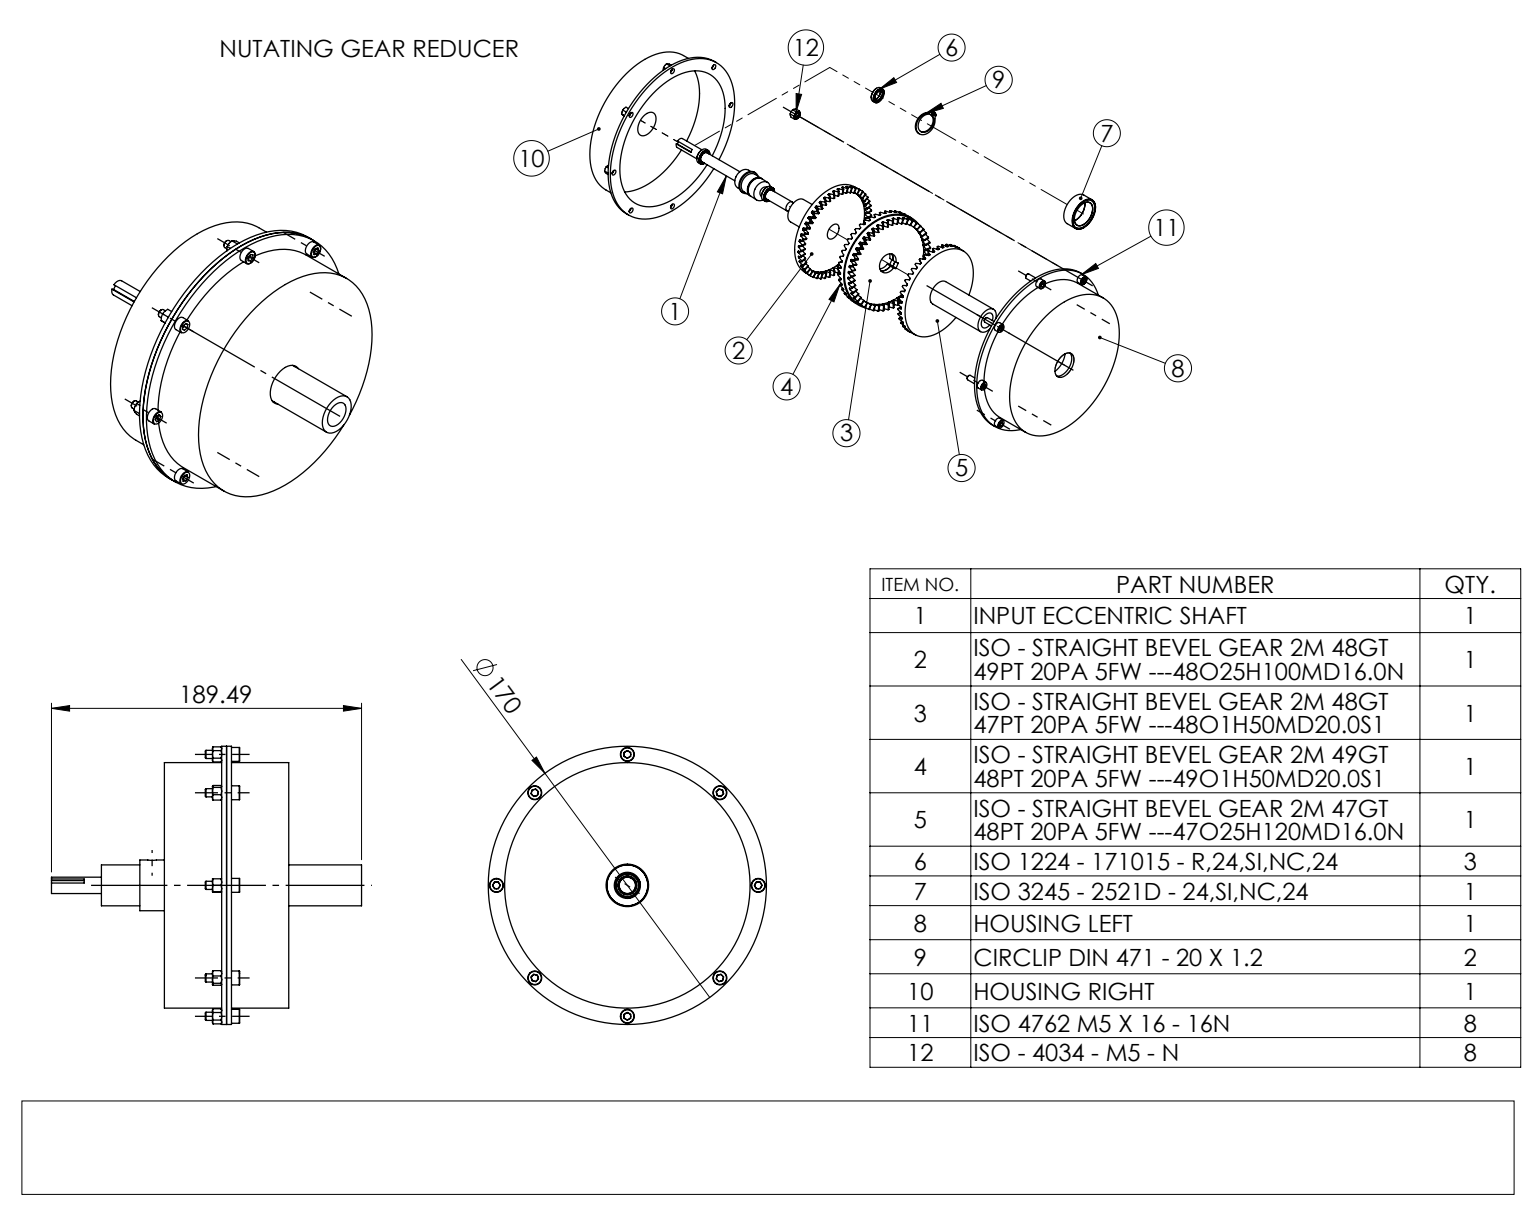
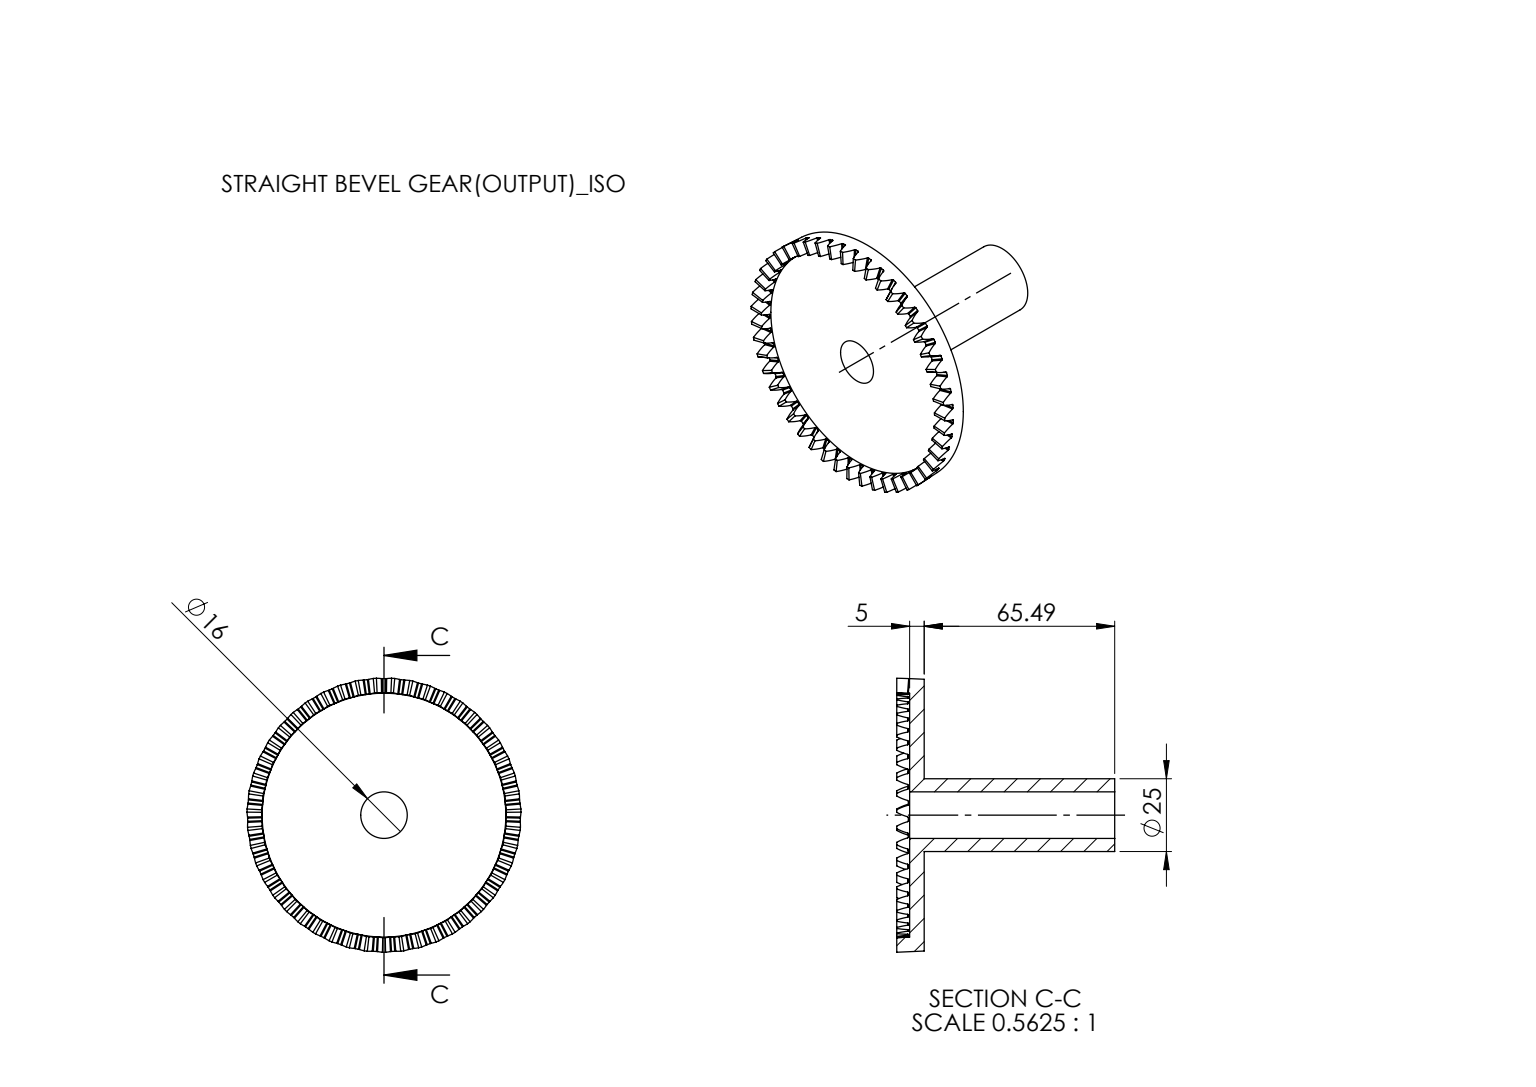
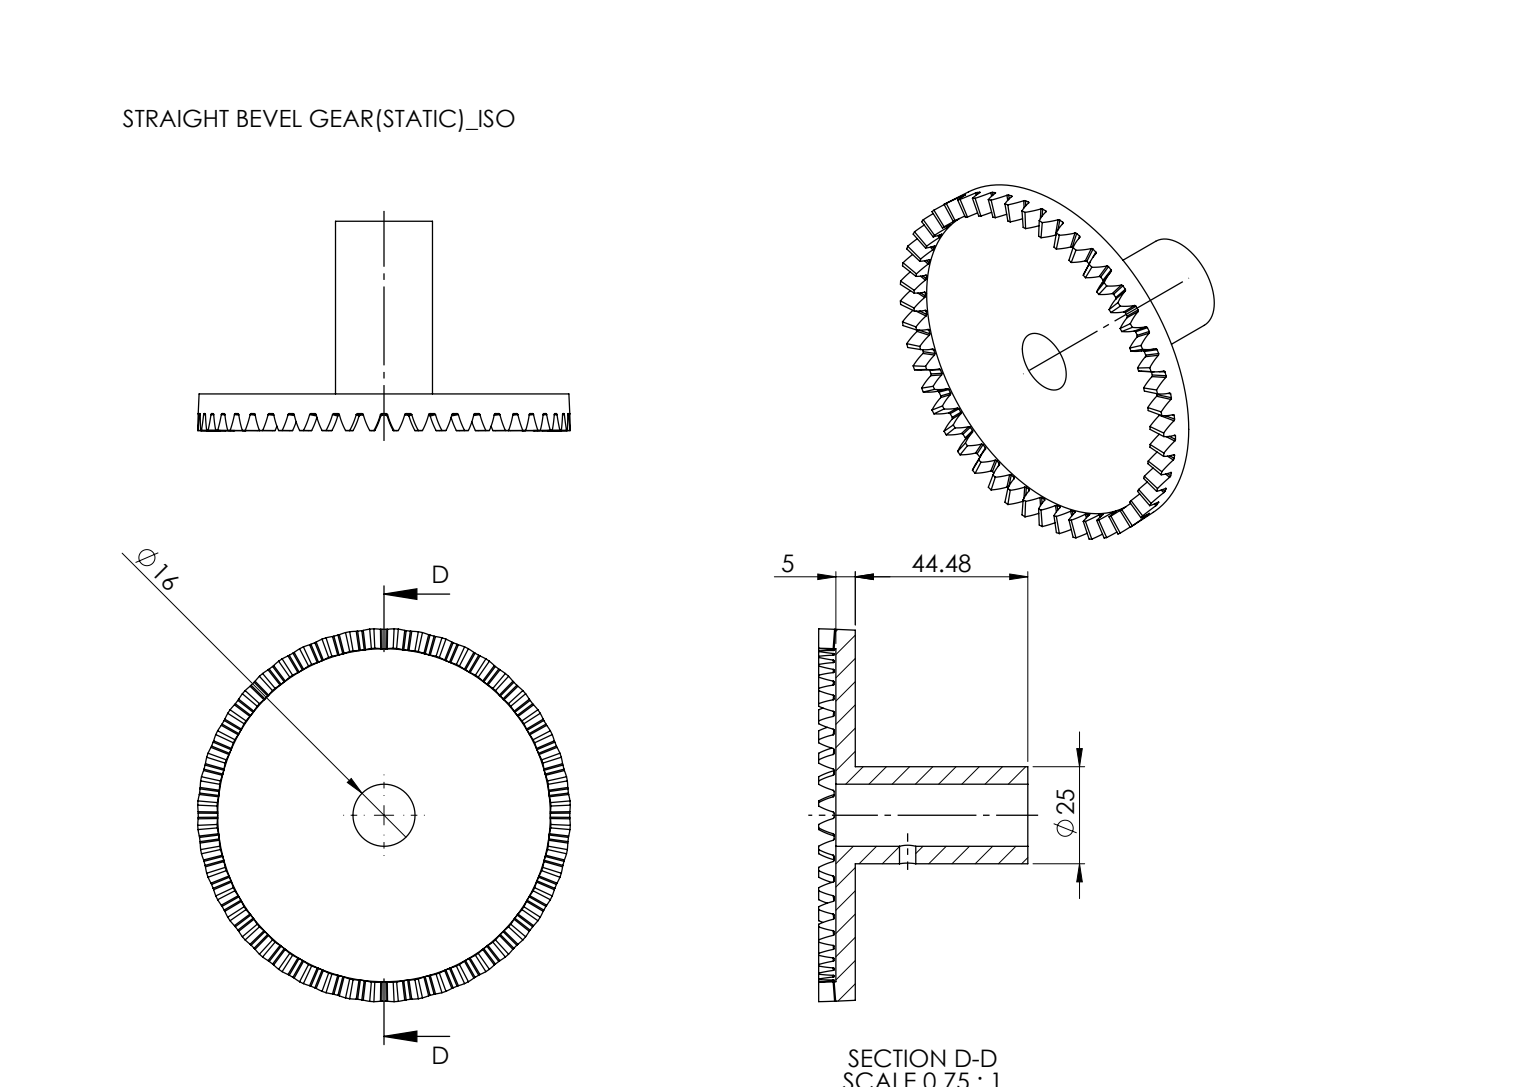
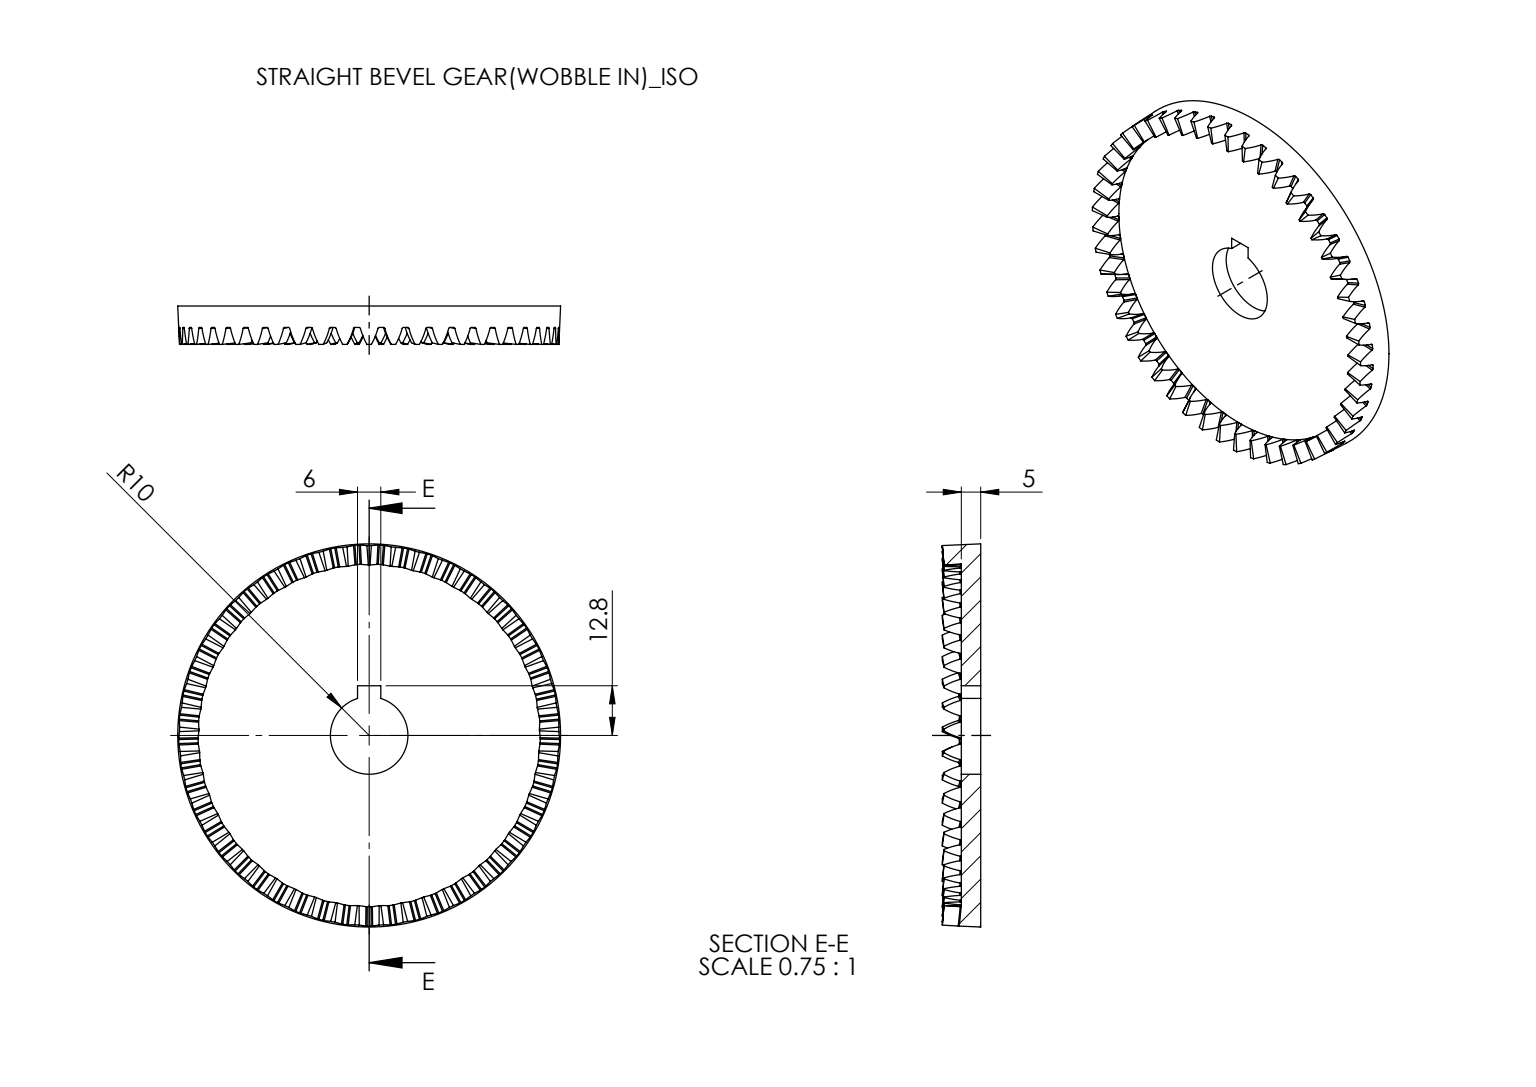
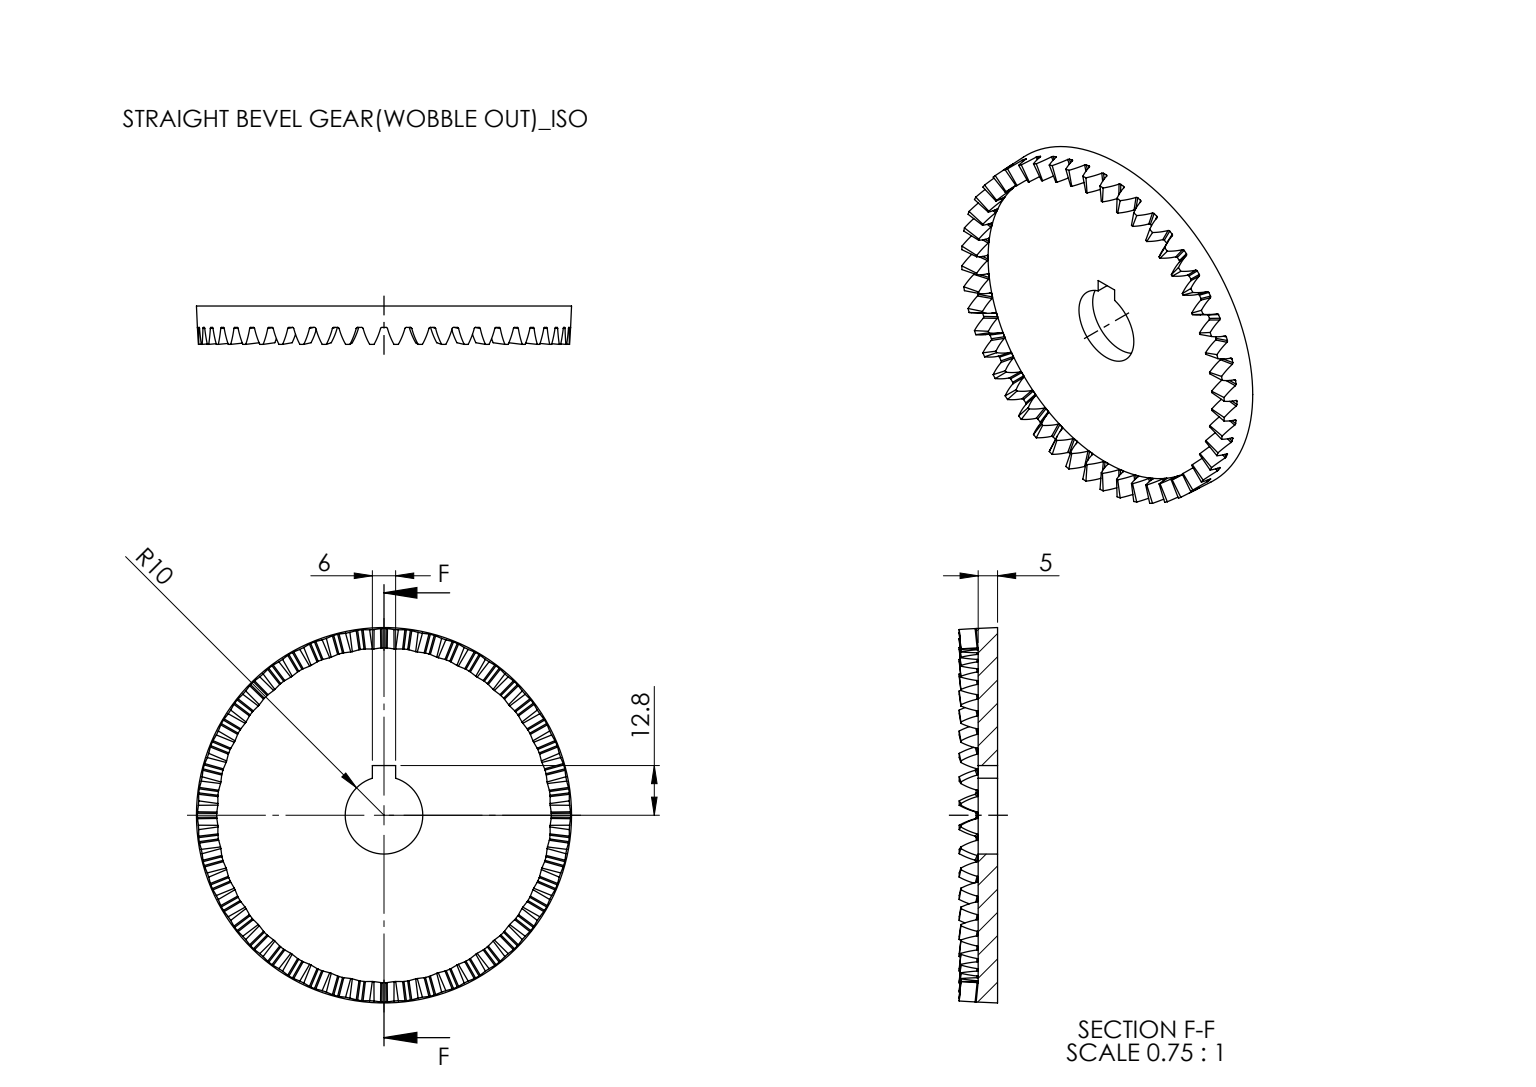
ISO-10303-21;
HEADER;
FILE_DESCRIPTION (('STEP AP214'),
    '1' );
FILE_NAME ('BR-540',
    '2026-10-08T08:02:49',
    ( '' ),
    ( '' ),
    'SwSTEP 2.0',
    'SolidWorks 2026',
    '' );
FILE_SCHEMA (( 'AUTOMOTIVE_DESIGN' ));
ENDSEC;

DATA;
#1 = CARTESIAN_POINT ( 'NONE',  ( 0.6000166863083090663, -45.71468846346234471, -17.94410043432203139 ) ) ;
#2 = ORIENTED_EDGE ( 'NONE', *, *, #40135, .F. ) ;
#3 = CARTESIAN_POINT ( 'NONE',  ( -6.017396004339686577, 14.95000090562881390, 11.47005965438143882 ) ) ;
#4 = VERTEX_POINT ( 'NONE', #15118 ) ;
#5 = FACE_OUTER_BOUND ( 'NONE', #24544, .T. ) ;
#6 = ORIENTED_EDGE ( 'NONE', *, *, #7694, .T. ) ;
#7 = CARTESIAN_POINT ( 'NONE',  ( 0.5848930533535030563, -19.57496322689467760, 42.61565319285014652 ) ) ;
#8 = CARTESIAN_POINT ( 'NONE',  ( -6.077587904424778920, 5.472951620448720078, -18.46192898789718129 ) ) ;
#9 = ORIENTED_EDGE ( 'NONE', *, *, #20619, .T. ) ;
#10 = CARTESIAN_POINT ( 'NONE',  ( 5.910764540655177868, -13.99299321836483045, 14.44636214622763681 ) ) ;
#11 = ORIENTED_EDGE ( 'NONE', *, *, #34105, .F. ) ;
#12 = CARTESIAN_POINT ( 'NONE',  ( 2.624215991343608501, -38.92973006074533515, 28.09277600149204801 ) ) ;
#13 = SHAPE_REPRESENTATION ( 'circlip for shafts normal_din_Circlip DIN 471 - 20 x 1.2', ( #14677 ), #21841 ) ;
#14 = VERTEX_POINT ( 'NONE', #34229 ) ;
#15 = CARTESIAN_POINT ( 'NONE',  ( 0.9752132459055861124, -16.63533515462550127, -39.55248938404434966 ) ) ;
#16 = CARTESIAN_POINT ( 'NONE',  ( 16.60577576646022635, -4.999999999999987566, 6.123233995736738672E-16 ) ) ;
#17 = CARTESIAN_POINT ( 'NONE',  ( 0.1152809850208375564, -22.68421566702489756, -37.84668601161344981 ) ) ;
#18 = ORIENTED_EDGE ( 'NONE', *, *, #60103, .F. ) ;
#19 = CARTESIAN_POINT ( 'NONE',  ( 0.8560838555295158248, -34.16988317699912159, -32.13708010619451727 ) ) ;
#20 = ORIENTED_EDGE ( 'NONE', *, *, #44663, .F. ) ;
#21 = ORIENTED_EDGE ( 'NONE', *, *, #24258, .F. ) ;
#22 = CIRCLE ( 'NONE', #14059, 18.99999999999999645 ) ;
#23 = CARTESIAN_POINT ( 'NONE',  ( 1.092182651088189127, 25.48667707440418440, 33.27447183874333803 ) ) ;
#24 = ADVANCED_FACE ( 'NONE', ( #21978 ), #2362, .F. ) ;
#25 = CARTESIAN_POINT ( 'NONE',  ( 5.960221823109900008, 10.26751639438343311, 17.77295928189558794 ) ) ;
#26 = ORIENTED_EDGE ( 'NONE', *, *, #59034, .F. ) ;
#27 = LINE ( 'NONE', #23853, #11554 ) ;
#28 = CARTESIAN_POINT ( 'NONE',  ( 9.999999999999994671, 54.69470952477936976, 58.44237546506825964 ) ) ;
#29 = CARTESIAN_POINT ( 'NONE',  ( 4.956653778116966613, 0.000000000000000000, 0.000000000000000000 ) ) ;
#30 = CARTESIAN_POINT ( 'NONE',  ( 0.9789233960466694473, -22.43936322751809342, -35.39508023406433068 ) ) ;
#31 = VECTOR ( 'NONE', #37686, 1000.000000000000000 ) ;
#32 = ORIENTED_EDGE ( 'NONE', *, *, #35814, .T. ) ;
#33 = CARTESIAN_POINT ( 'NONE',  ( 0.5806925824938499181, 45.08220210717423271, 12.91578164539256335 ) ) ;
#34 = DIRECTION ( 'NONE',  ( 0.09722883295013594329, -0.9880289017988295175, -0.1197724645039638103 ) ) ;
#35 = CARTESIAN_POINT ( 'NONE',  ( 5.960221823109900008, -10.25807604135609274, -17.77840967225716895 ) ) ;
#36 = DIRECTION ( 'NONE',  ( 0.000000000000000000, 0.000000000000000000, 1.000000000000000000 ) ) ;
#37 = CARTESIAN_POINT ( 'NONE',  ( 0.8560838555295223751, -26.00596412780120303, -39.03924517540328765 ) ) ;
#38 = CARTESIAN_POINT ( 'NONE',  ( 1.827326673878743257, 6.839036141888570342, -42.50320212329573621 ) ) ;
#39 = CARTESIAN_POINT ( 'NONE',  ( 0.5987334308729315158, 46.79309025446952575, 14.89864460301000015 ) ) ;
#40 = CARTESIAN_POINT ( 'NONE',  ( 0.5832655196449135770, 40.46492986189638685, -23.70284021473238667 ) ) ;
#41 = CARTESIAN_POINT ( 'NONE',  ( 0.1313383488274124655, -37.02311703718871883, 22.11173226734828745 ) ) ;
#42 = CARTESIAN_POINT ( 'NONE',  ( 0.6025881611877910160, 48.10699274197334319, 0.2181813582440121635 ) ) ;
#43 = CARTESIAN_POINT ( 'NONE',  ( -1.200000000000006617, 0.000000000000000000, 0.000000000000000000 ) ) ;
#44 = CYLINDRICAL_SURFACE ( 'NONE', #23607, 12.50000000000000000 ) ;
#45 = CARTESIAN_POINT ( 'NONE',  ( 2.528190830796654964, -23.59892530385130627, 34.71807685711083025 ) ) ;
#46 = FACE_OUTER_BOUND ( 'NONE', #12216, .T. ) ;
#47 = EDGE_CURVE ( 'NONE', #13219, #36056, #34301, .T. ) ;
#48 = CARTESIAN_POINT ( 'NONE',  ( 0.5807400328401574052, 47.89582301953903709, 0.5448834511091634747 ) ) ;
#49 = EDGE_CURVE ( 'NONE', #23782, #28115, #2220, .T. ) ;
#50 = FILL_AREA_STYLE_COLOUR ( '', #7249 ) ;
#51 = CARTESIAN_POINT ( 'NONE',  ( -6.015611763856276717, -18.68122482568281839, 2.465697960550983225 ) ) ;
#52 = ORIENTED_EDGE ( 'NONE', *, *, #55367, .T. ) ;
#53 = CARTESIAN_POINT ( 'NONE',  ( 0.5839879327111927587, 29.08515285004941120, -38.05372318152023325 ) ) ;
#54 = CARTESIAN_POINT ( 'NONE',  ( 0.5997462898726536595, 5.235280152387709940, -48.82769165002913070 ) ) ;
#55 = DIRECTION ( 'NONE',  ( -1.000000000000000000, -0.000000000000000000, -0.000000000000000000 ) ) ;
#56 = EDGE_CURVE ( 'NONE', #14922, #2416, #61883, .T. ) ;
#57 = ORIENTED_EDGE ( 'NONE', *, *, #25597, .F. ) ;
#58 = CARTESIAN_POINT ( 'NONE',  ( -6.078726893082806448, 15.42998809551244577, -11.51996131248123234 ) ) ;
#60 = VERTEX_POINT ( 'NONE', #12282 ) ;
#59 = CONICAL_SURFACE ( 'NONE', #54074, 42.92674063221959813, 1.485477209440487556 ) ;
#61 = VERTEX_POINT ( 'NONE', #2846 ) ;
#62 = B_SPLINE_CURVE_WITH_KNOTS ( 'NONE', 3,
 ( #7041, #45606, #7993, #3579, #27403, #31488 ),
 .UNSPECIFIED., .F., .F.,
 ( 4, 2, 4 ),
 ( 1.216335680627485354E-16, 0.0002448718616795927711, 0.0004897437233590629189 ),
 .UNSPECIFIED. ) ;
#63 = CARTESIAN_POINT ( 'NONE',  ( 0.9740398440564311811, -11.50548031350412970, -41.33716823241943672 ) ) ;
#64 = ORIENTED_EDGE ( 'NONE', *, *, #23685, .F. ) ;
#65 = EDGE_CURVE ( 'NONE', #40254, #5752, #47059, .T. ) ;
#66 = EDGE_LOOP ( 'NONE', ( #17110, #3171, #49258, #1993 ) ) ;
#67 = ORIENTED_EDGE ( 'NONE', *, *, #12959, .F. ) ;
#68 = FACE_OUTER_BOUND ( 'NONE', #26695, .T. ) ;
#70 = EDGE_LOOP ( 'NONE', ( #37119, #28268, #15345 ) ) ;
#69 = ADVANCED_FACE ( 'NONE', ( #31062 ), #10020, .T. ) ;
#71 = CARTESIAN_POINT ( 'NONE',  ( 0.9722240741986376555, 11.66659279944034111, -41.29187377038488194 ) ) ;
#72 = DIRECTION ( 'NONE',  ( -1.000000000000000000, 0.000000000000000000, -0.000000000000000000 ) ) ;
#73 = CARTESIAN_POINT ( 'NONE',  ( 0.1073791018717483448, -30.83464511437118816, -30.14884492832378626 ) ) ;
#74 = ORIENTED_EDGE ( 'NONE', *, *, #24741, .T. ) ;
#75 = CARTESIAN_POINT ( 'NONE',  ( 0.2285344041767094769, -7.790448184841448409, -43.42591492847049750 ) ) ;
#76 =( BOUNDED_SURFACE ( )  B_SPLINE_SURFACE ( 3, 1, ( 
 ( #47518, #33740 ),
 ( #24014, #29022 ),
 ( #42835, #9289 ),
 ( #58121, #38143 ) ),
 .UNSPECIFIED., .F., .F., .F. ) 
 B_SPLINE_SURFACE_WITH_KNOTS ( ( 4, 4 ),
 ( 2, 2 ),
 ( 0.000000000000000000, 1.000000000000000000 ),
 ( 0.000000000000000000, 1.000000000000000000 ),
 .UNSPECIFIED. ) 
 GEOMETRIC_REPRESENTATION_ITEM ( )  RATIONAL_B_SPLINE_SURFACE ( (
 ( 1.000000000000000000, 1.000000000000000000),
 ( 0.7211978278499970862, 0.9934217856018976445),
 ( 0.7211978278499970862, 0.9934217856018976445),
 ( 1.000000000000000000, 1.000000000000000000) ) ) 
 REPRESENTATION_ITEM ( '' )  SURFACE ( )  );
#77 = CARTESIAN_POINT ( 'NONE',  ( 0.9740398440564309590, -34.29238484271514409, -25.79088785829017283 ) ) ;
#78 = ORIENTED_EDGE ( 'NONE', *, *, #56716, .F. ) ;
#79 = EDGE_LOOP ( 'NONE', ( #41919, #50694, #26736, #25891 ) ) ;
#80 = DIRECTION ( 'NONE',  ( 0.07906939808003035641, -0.7873210066866034307, 0.6114520935586490458 ) ) ;
#81 = ORIENTED_EDGE ( 'NONE', *, *, #43581, .F. ) ;
#82 = CARTESIAN_POINT ( 'NONE',  ( -6.015611763856276717, 17.40650793417854203, -7.216738110653091454 ) ) ;
#83 = CARTESIAN_POINT ( 'NONE',  ( 0.7044674535452954967, 36.84332507061608908, 32.47109669462702897 ) ) ;
#84 = CARTESIAN_POINT ( 'NONE',  ( 5.981074661064941900, 2.670494474391725159, 20.35019299530689096 ) ) ;
#85 = CARTESIAN_POINT ( 'NONE',  ( 1.227938101723757836, -15.63977281655870222, 39.96870412324331312 ) ) ;
#86 = ORIENTED_EDGE ( 'NONE', *, *, #4568, .F. ) ;
#87 = DIRECTION ( 'NONE',  ( 0.09722883295013592941, 0.4536333312076272772, -0.8858687006891176052 ) ) ;
#88 = CARTESIAN_POINT ( 'NONE',  ( 1.231276596079887264, -16.87422718933211030, 38.37365278131431268 ) ) ;
#89 = CARTESIAN_POINT ( 'NONE',  ( 0.7764146366350301864, -30.95828368181982881, -35.23670167801082442 ) ) ;
#90 = EDGE_CURVE ( 'NONE', #9871, #29097, #13329, .T. ) ;
#91 = ORIENTED_EDGE ( 'NONE', *, *, #56070, .F. ) ;
#92 = CARTESIAN_POINT ( 'NONE',  ( 0.8744876279028306332, 41.62483489565916983, 26.03311679935014666 ) ) ;
#93 = CARTESIAN_POINT ( 'NONE',  ( -6.078075953587585900, 9.986729131371458124, -16.46391252114006321 ) ) ;
#94 = CARTESIAN_POINT ( 'NONE',  ( 0.6008123274975389894, -34.97209513635705491, -34.47473151356003740 ) ) ;
#95 = ORIENTED_EDGE ( 'NONE', *, *, #30971, .T. ) ;
#96 = VERTEX_POINT ( 'NONE', #35469 ) ;
#97 = CARTESIAN_POINT ( 'NONE',  ( 2.526552050251863690, 17.56110221699880825, -39.22765360404633128 ) ) ;
#98 = CARTESIAN_POINT ( 'NONE',  ( 0.1310142868023682072, 37.66054729763593656, -21.00772081177039041 ) ) ;
#99 = CARTESIAN_POINT ( 'NONE',  ( 4.553261556744875094, 35.06776520399859010, 26.45357082552112260 ) ) ;
#100 = CARTESIAN_POINT ( 'NONE',  ( 3.238018933889920792, 11.66219248059495683, 6.587925235854416250 ) ) ;
#101 = B_SPLINE_CURVE_WITH_KNOTS ( 'NONE', 3,
 ( #15435, #38953, #58005, #53923, #53312, #29209 ),
 .UNSPECIFIED., .F., .F.,
 ( 4, 2, 4 ),
 ( 0.000000000000000000, 0.0002291966416970781840, 0.0004583932833941563680 ),
 .UNSPECIFIED. ) ;
#102 = FACE_OUTER_BOUND ( 'NONE', #56108, .T. ) ;
#103 = CARTESIAN_POINT ( 'NONE',  ( 0.9758171775293917882, -42.54062484958058832, 5.606549717954040446 ) ) ;
#104 = AXIS2_PLACEMENT_3D ( 'NONE', #50216, #16097, #21404 ) ;
#105 = LINE ( 'NONE', #9217, #17995 ) ;
#106 = CARTESIAN_POINT ( 'NONE',  ( 3.270143674763207553, -9.870732238228454136, -9.482922169188068295 ) ) ;
#107 = CARTESIAN_POINT ( 'NONE',  ( 0.5782707292762442330, -44.06349990951357398, -16.06687055502457540 ) ) ;
#108 = CARTESIAN_POINT ( 'NONE',  ( 0.9787464366903551038, 41.90826471085239291, 0.1770361985267714100 ) ) ;
#109 = CARTESIAN_POINT ( 'NONE',  ( 5.959547316686252039, -5.315863417546194292, -19.82530672674360517 ) ) ;
#110 = ORIENTED_EDGE ( 'NONE', *, *, #11013, .T. ) ;
#111 = CARTESIAN_POINT ( 'NONE',  ( 0.9730545539215883499, 21.01499094264548972, 37.40983423658480689 ) ) ;
#112 = CARTESIAN_POINT ( 'NONE',  ( 0.6026112563231247332, 41.06109594249098649, 26.93561573281289512 ) ) ;
#113 = CARTESIAN_POINT ( 'NONE',  ( 0.1139756605157203062, -35.12259180221513333, 26.70877692426205030 ) ) ;
#114 = DIRECTION ( 'NONE',  ( 0.000000000000000000, 0.7071067811865540120, -0.7071067811865409114 ) ) ;
#115 = CARTESIAN_POINT ( 'NONE',  ( 4.956653778116975495, 26.26162724282373517, 40.28700667097690769 ) ) ;
#116 = CARTESIAN_POINT ( 'NONE',  ( 0.1102847568649952675, 42.76743495471822598, 5.537466591275816974 ) ) ;
#117 = LINE ( 'NONE', #14570, #16748 ) ;
#118 = CARTESIAN_POINT ( 'NONE',  ( 0.6008122571543326185, 48.11686503207880605, -9.814369564573597771 ) ) ;
#119 = CARTESIAN_POINT ( 'NONE',  ( 0.6016118706126977189, -30.88962476549868796, 38.17567467158400518 ) ) ;
#120 = EDGE_CURVE ( 'NONE', #16502, #9752, #36523, .T. ) ;
#121 = DIRECTION ( 'NONE',  ( 0.000000000000000000, 0.000000000000000000, 1.000000000000000000 ) ) ;
#123 = ORIENTED_EDGE ( 'NONE', *, *, #51983, .T. ) ;
#122 = CARTESIAN_POINT ( 'NONE',  ( 21.00000000000000355, 2.516649172247811061E-16, -2.055000000000000160 ) ) ;
#124 = ORIENTED_EDGE ( 'NONE', *, *, #27240, .T. ) ;
#125 = CARTESIAN_POINT ( 'NONE',  ( 0.1154773475650540671, -6.864599028446649598, 43.58693508638535974 ) ) ;
#126 = DIRECTION ( 'NONE',  ( 0.07906939808003035641, 0.6497517485244377333, -0.7560229464617442829 ) ) ;
#127 = CARTESIAN_POINT ( 'NONE',  ( -5.995132425357893702, -14.95525565067283047, 11.46484027925362170 ) ) ;
#128 = EDGE_CURVE ( 'NONE', #41039, #1919, #35074, .T. ) ;
#129 = VERTEX_POINT ( 'NONE', #54848 ) ;
#130 = DIRECTION ( 'NONE',  ( -1.000000000000000000, -0.000000000000000000, -0.000000000000000000 ) ) ;
#131 = CARTESIAN_POINT ( 'NONE',  ( 0.5987334308729319599, -47.34446294507543485, 13.04088704851432290 ) ) ;
#132 = CARTESIAN_POINT ( 'NONE',  ( 0.5834872094924158370, -41.36515088387901784, -24.14431479207734554 ) ) ;
#133 = B_SPLINE_CURVE_WITH_KNOTS ( 'NONE', 3,
 ( #55260, #2330, #15845, #26459 ),
 .UNSPECIFIED., .F., .F.,
 ( 4, 4 ),
 ( 0.000000000000000000, 0.004446090762761379864 ),
 .UNSPECIFIED. ) ;
#134 = EDGE_CURVE ( 'NONE', #31710, #59272, #52135, .T. ) ;
#135 = ORIENTED_EDGE ( 'NONE', *, *, #59672, .F. ) ;
#136 = ORIENTED_EDGE ( 'NONE', *, *, #11452, .T. ) ;
#137 = B_SPLINE_CURVE_WITH_KNOTS ( 'NONE', 3,
 ( #31189, #25263, #45615, #30260, #59373, #21803, #54354, #49372, #40937, #34673 ),
 .UNSPECIFIED., .F., .F.,
 ( 4, 3, 3, 4 ),
 ( 2.027574016683678720E-17, 0.0002618515315864107518, 0.0003927756766341517500, 0.0005236741812375312905 ),
 .UNSPECIFIED. ) ;
#138 = CARTESIAN_POINT ( 'NONE',  ( -6.015611763856276717, 11.46610900684744472, -14.95313250337417799 ) ) ;
#139 = CARTESIAN_POINT ( 'NONE',  ( 4.956653778116987930, -47.05699031914942054, -9.917440902361647659 ) ) ;
#140 = CARTESIAN_POINT ( 'NONE',  ( 2.648799415243708655, 41.83591888777168322, 25.57876764242928047 ) ) ;
#141 = EDGE_CURVE ( 'NONE', #1542, #34181, #7863, .T. ) ;
#142 = CARTESIAN_POINT ( 'NONE',  ( 4.958415959904820092, 24.01335991616949883, 38.55596580763011616 ) ) ;
#143 = VECTOR ( 'NONE', #45056, 1000.000000000000114 ) ;
#144 = DIRECTION ( 'NONE',  ( 0.1736481776669314969, -0.9848077530122077983, 5.551115123125780853E-17 ) ) ;
#145 = AXIS2_PLACEMENT_3D ( 'NONE', #52152, #34003, #4829 ) ;
#146 = CARTESIAN_POINT ( 'NONE',  ( 0.1152809850208375703, 33.45438703243825529, 28.77063208853051890 ) ) ;
#147 = VERTEX_POINT ( 'NONE', #41411 ) ;
#148 =( BOUNDED_SURFACE ( )  B_SPLINE_SURFACE ( 3, 1, ( 
 ( #20134, #29510 ),
 ( #43334, #14815 ),
 ( #19515, #5067 ),
 ( #19828, #43643 ) ),
 .UNSPECIFIED., .F., .F., .F. ) 
 B_SPLINE_SURFACE_WITH_KNOTS ( ( 4, 4 ),
 ( 2, 2 ),
 ( 0.000000000000000000, 1.000000000000000000 ),
 ( 0.000000000000000000, 1.000000000000000000 ),
 .UNSPECIFIED. ) 
 GEOMETRIC_REPRESENTATION_ITEM ( )  RATIONAL_B_SPLINE_SURFACE ( (
 ( 1.000000000000000000, 1.000000000000000000),
 ( 0.9953390228620291325, 0.8624445117761032620),
 ( 0.9953390228620291325, 0.8624445117761032620),
 ( 1.000000000000000000, 1.000000000000000000) ) ) 
 REPRESENTATION_ITEM ( '' )  SURFACE ( )  );
#149 = CARTESIAN_POINT ( 'NONE',  ( 0.8557997880470697982, -11.51622788066490166, 46.50333260518556244 ) ) ;
#150 = CARTESIAN_POINT ( 'NONE',  ( 2.528190830796656741, -41.94888846746666644, 1.595271919470088395 ) ) ;
#151 = ORIENTED_EDGE ( 'NONE', *, *, #60540, .T. ) ;
#152 = CARTESIAN_POINT ( 'NONE',  ( 1.227938101723756947, 42.65467462194918369, 4.762198645644581951 ) ) ;
#153 = CARTESIAN_POINT ( 'NONE',  ( 0.6064782688330876415, 5.400824873672297244, -46.58503554901177779 ) ) ;
#154 = CARTESIAN_POINT ( 'NONE',  ( 0.7056313189692692278, -13.08832644501797837, 45.03825434923295745 ) ) ;
#155 = CARTESIAN_POINT ( 'NONE',  ( 0.1156867017252034696, -40.85238086880038111, -16.67410521214435093 ) ) ;
#156 = ORIENTED_EDGE ( 'NONE', *, *, #13892, .F. ) ;
#157 = ORIENTED_EDGE ( 'NONE', *, *, #10599, .T. ) ;
#158 = CARTESIAN_POINT ( 'NONE',  ( 0.6001305935487315502, 28.87057754790937381, -38.48510059944018735 ) ) ;
#159 = CARTESIAN_POINT ( 'NONE',  ( 1.500000000000001332, 9.123618653647810742E-16, 7.400000000000022560 ) ) ;
#160 = CARTESIAN_POINT ( 'NONE',  ( 4.956445790444011124, -16.41925925744418180, -44.13554095710700409 ) ) ;
#161 = CARTESIAN_POINT ( 'NONE',  ( 0.9754292589017227177, -37.66327352597247824, -18.37948024844710559 ) ) ;
#162 = EDGE_LOOP ( 'NONE', ( #14150, #34103, #5570, #1627 ) ) ;
#163 = CARTESIAN_POINT ( 'NONE',  ( 0.6001305935487422083, -46.33281397023073112, 12.95698906763730029 ) ) ;
#164 = ORIENTED_EDGE ( 'NONE', *, *, #58852, .T. ) ;
#165 = CARTESIAN_POINT ( 'NONE',  ( 5.880360259849739535, -21.25991003419923331, -43.00389496650606702 ) ) ;
#166 = B_SPLINE_CURVE_WITH_KNOTS ( 'NONE', 3,
 ( #1737, #48445, #29959, #44100, #20871, #49069 ),
 .UNSPECIFIED., .F., .F.,
 ( 4, 2, 4 ),
 ( 1.764953265579307567E-18, 0.0002450742804987333630, 0.0004901485609974648829 ),
 .UNSPECIFIED. ) ;
#167 = ORIENTED_EDGE ( 'NONE', *, *, #37298, .F. ) ;
#168 = CARTESIAN_POINT ( 'NONE',  ( 0.5819845901640497976, -47.42480841519684986, -6.701564444318185210 ) ) ;
#169 = EDGE_CURVE ( 'NONE', #49553, #36850, #1300, .T. ) ;
#170 = CARTESIAN_POINT ( 'NONE',  ( 0.1139756605157203062, -27.19909892944385987, 34.74426912630842423 ) ) ;
#171 = CARTESIAN_POINT ( 'NONE',  ( 0.9749527285493309048, 26.34702925571547993, -33.86694354778329341 ) ) ;
#172 = B_SPLINE_CURVE_WITH_KNOTS ( 'NONE', 3,
 ( #49055, #11162, #20259, #6410, #20862, #40000, #59053, #16169, #54340, #30550, #21165, #49661, #35596, #54656, #11784, #30863, #49979, #45304, #2348 ),
 .UNSPECIFIED., .F., .F.,
 ( 4, 3, 3, 3, 3, 3, 4 ),
 ( 6.939740885162003740E-18, 0.0002732106629380659556, 0.0004098138914053819915, 0.0005464171197651502675, 0.0006830203481512588017, 0.0008196235766963637414, 0.001011968216111144630 ),
 .UNSPECIFIED. ) ;
#174 = ORIENTED_EDGE ( 'NONE', *, *, #46970, .T. ) ;
#173 = EDGE_CURVE ( 'NONE', #14818, #35927, #7295, .T. ) ;
#175 = CARTESIAN_POINT ( 'NONE',  ( 0.5837374860065644988, -18.49670552082923436, -44.18034382476643884 ) ) ;
#176 = CARTESIAN_POINT ( 'NONE',  ( 3.783278058412224976, 41.09146792477083920, -12.79810311738810569 ) ) ;
#177 = CARTESIAN_POINT ( 'NONE',  ( 0.3622758884714730732, 26.89560658783340585, 33.69533458712353280 ) ) ;
#178 = CARTESIAN_POINT ( 'NONE',  ( 0.6009452777970410997, 28.93864923253898169, -38.43042656245044242 ) ) ;
#179 = CARTESIAN_POINT ( 'NONE',  ( 0.1081432562775998252, 16.89351827868222600, -39.67792926340383985 ) ) ;
#180 = ORIENTED_EDGE ( 'NONE', *, *, #28573, .F. ) ;
#181 = EDGE_CURVE ( 'NONE', #8116, #45706, #44738, .T. ) ;
#182 = CARTESIAN_POINT ( 'NONE',  ( -6.015611763856276717, 14.95313250337430055, 11.46610900684727952 ) ) ;
#183 = CARTESIAN_POINT ( 'NONE',  ( 0.5806925824938499181, 28.25565086187788921, -37.42780459384738379 ) ) ;
#184 = ORIENTED_EDGE ( 'NONE', *, *, #61518, .T. ) ;
#185 = CARTESIAN_POINT ( 'NONE',  ( 0.7056555295713297093, 38.50897360867684682, 28.48870155114923008 ) ) ;
#186 = LINE ( 'NONE', #38450, #30341 ) ;
#187 = CARTESIAN_POINT ( 'NONE',  ( 4.975610109902397937, 39.54077024310177535, -28.79195887257430897 ) ) ;
#188 = CARTESIAN_POINT ( 'NONE',  ( 0.6845945791218034371, -45.78817307429869743, -10.19066863517858579 ) ) ;
#189 = FACE_OUTER_BOUND ( 'NONE', #26362, .T. ) ;
#190 = VECTOR ( 'NONE', #29724, 1000.000000000000114 ) ;
#191 = CARTESIAN_POINT ( 'NONE',  ( 52.60669624972128844, 15.41611702489417723, 1.616806307337775861 ) ) ;
#192 = DIRECTION ( 'NONE',  ( -1.000000000000000000, 2.773151286625958102E-17, 5.189784904172182762E-18 ) ) ;
#193 = CARTESIAN_POINT ( 'NONE',  ( 0.7242486021783862693, -29.97000013935198481, -38.89486539404931875 ) ) ;
#194 = AXIS2_PLACEMENT_3D ( 'NONE', #25352, #281, #58847 ) ;
#195 = CARTESIAN_POINT ( 'NONE',  ( 4.975801465491695552, -3.702618843597113685, -47.76942479135485087 ) ) ;
#196 = EDGE_CURVE ( 'NONE', #14140, #9995, #46409, .T. ) ;
#197 = CARTESIAN_POINT ( 'NONE',  ( 0.9772918015221170318, 28.83491956217883967, -30.41190999581177223 ) ) ;
#199 = VERTEX_POINT ( 'NONE', #3761 ) ;
#198 = FACE_OUTER_BOUND ( 'NONE', #52449, .T. ) ;
#200 = ORIENTED_EDGE ( 'NONE', *, *, #48538, .F. ) ;
#201 = CARTESIAN_POINT ( 'NONE',  ( 4.967162193818130511, -32.68434214048149045, -28.07411493385329138 ) ) ;
#202 = EDGE_CURVE ( 'NONE', #46227, #38797, #32610, .T. ) ;
#203 = CARTESIAN_POINT ( 'NONE',  ( -2.678494666091065124, -3.072372537026387018, -0.03421028094655000767 ) ) ;
#204 = CARTESIAN_POINT ( 'NONE',  ( 0.9752570700956801897, 42.57087745267997292, -5.371905812151719140 ) ) ;
#205 = CARTESIAN_POINT ( 'NONE',  ( 3.270143674763207553, 4.983712007628229301, 12.74832469035454352 ) ) ;
#206 = EDGE_CURVE ( 'NONE', #20518, #58874, #57008, .T. ) ;
#207 = ORIENTED_EDGE ( 'NONE', *, *, #11032, .T. ) ;
#208 = CARTESIAN_POINT ( 'NONE',  ( 0.2940133293162999761, -22.17757316225551278, -38.13654150825487932 ) ) ;
#209 = DIRECTION ( 'NONE',  ( -2.280301054154487250E-31, 0.000000000000000000, 1.000000000000000000 ) ) ;
#210 = DIRECTION ( 'NONE',  ( 1.000000000000000000, -0.000000000000000000, -0.000000000000000000 ) ) ;
#211 = ORIENTED_EDGE ( 'NONE', *, *, #8364, .F. ) ;
#212 = EDGE_CURVE ( 'NONE', #15210, #7786, #8757, .T. ) ;
#213 = CARTESIAN_POINT ( 'NONE',  ( 5.910764540655177868, -1.997730036635376738, -20.01275376278557161 ) ) ;
#214 = CARTESIAN_POINT ( 'NONE',  ( 0.5817216825391113844, -25.61650133936588603, -39.28141814315932123 ) ) ;
#215 = ORIENTED_EDGE ( 'NONE', *, *, #7819, .T. ) ;
#216 = CARTESIAN_POINT ( 'NONE',  ( 50.15577769773999961, 12.80000000000000071, 3.000000000000000000 ) ) ;
#217 = VERTEX_POINT ( 'NONE', #13200 ) ;
#218 = CARTESIAN_POINT ( 'NONE',  ( 0.6023143664670691511, 33.83148565876883396, 34.20175727332139815 ) ) ;
#219 = VERTEX_POINT ( 'NONE', #37023 ) ;
#220 = CARTESIAN_POINT ( 'NONE',  ( -5.995132425357893702, -16.32377331145327304, 9.414704407577744405 ) ) ;
#221 = CARTESIAN_POINT ( 'NONE',  ( 4.975610109902397937, -48.11736577406863802, 8.784561349450592971 ) ) ;
#222 = LINE ( 'NONE', #29992, #19722 ) ;
#223 = CARTESIAN_POINT ( 'NONE',  ( 0.8744876279028263033, -43.20725972823498040, 23.31271664041618052 ) ) ;
#224 = B_SPLINE_CURVE_WITH_KNOTS ( 'NONE', 3,
 ( #5732, #1055, #14880, #20192 ),
 .UNSPECIFIED., .F., .F.,
 ( 4, 4 ),
 ( 0.000000000000000000, 0.005013413432710142441 ),
 .UNSPECIFIED. ) ;
#225 = CIRCLE ( 'NONE', #35287, 43.08621763946400307 ) ;
#226 = VERTEX_POINT ( 'NONE', #61691 ) ;
#227 = CARTESIAN_POINT ( 'NONE',  ( 0.6026777506516368677, -8.009456454756694654, -48.44992257926296020 ) ) ;
#228 = ORIENTED_EDGE ( 'NONE', *, *, #20971, .T. ) ;
#229 = DIRECTION ( 'NONE',  ( -1.558861125776144859E-16, 1.000000000000000000, 0.000000000000000000 ) ) ;
#230 = VECTOR ( 'NONE', #33635, 1000.000000000000000 ) ;
#231 = ORIENTED_EDGE ( 'NONE', *, *, #52615, .T. ) ;
#232 = ORIENTED_EDGE ( 'NONE', *, *, #53084, .F. ) ;
#233 = CARTESIAN_POINT ( 'NONE',  ( 4.291220156522059348, -21.76365521422086147, 41.78196152674276931 ) ) ;
#234 = CARTESIAN_POINT ( 'NONE',  ( 0.5807400328401637335, 44.45848844984468684, -17.82553128098359352 ) ) ;
#235 = EDGE_CURVE ( 'NONE', #45826, #24987, #55024, .T. ) ;
#236 = CARTESIAN_POINT ( 'NONE',  ( 0.1095718737110178281, -16.74012863188530531, 39.74279513315646284 ) ) ;
#237 = CARTESIAN_POINT ( 'NONE',  ( 3.894904216938897878, -29.11014567165013744, -32.93514462472435866 ) ) ;
#238 = ORIENTED_EDGE ( 'NONE', *, *, #9253, .F. ) ;
#239 = CARTESIAN_POINT ( 'NONE',  ( 0.7057020205115017708, -46.04437542275037032, -13.20843872046536838 ) ) ;
#240 = ADVANCED_FACE ( 'NONE', ( #18825 ), #57227, .F. ) ;
#241 = CARTESIAN_POINT ( 'NONE',  ( 2.618530812446115519, -21.05599821100534186, -42.02822537933690938 ) ) ;
#242 = CARTESIAN_POINT ( 'NONE',  ( 0.8557997880470690211, -0.9121262075942833114, -47.89938907511595545 ) ) ;
#243 = VERTEX_POINT ( 'NONE', #51378 ) ;
#244 = B_SPLINE_CURVE_WITH_KNOTS ( 'NONE', 3,
 ( #37504, #42512, #47202, #27774, #51255, #61267 ),
 .UNSPECIFIED., .F., .F.,
 ( 4, 2, 4 ),
 ( 8.673617379884035472E-19, 0.0002291966416970798374, 0.0004583932833941588075 ),
 .UNSPECIFIED. ) ;
#245 = ADVANCED_FACE ( 'NONE', ( #8464 ), #1616, .F. ) ;
#246 = B_SPLINE_CURVE_WITH_KNOTS ( 'NONE', 3,
 ( #22467, #55345, #2101, #3338, #21239, #30943 ),
 .UNSPECIFIED., .F., .F.,
 ( 4, 2, 4 ),
 ( 3.496446946337351263E-18, 0.0002450742804987353146, 0.0004901485609974671597 ),
 .UNSPECIFIED. ) ;
#247 =( BOUNDED_SURFACE ( )  B_SPLINE_SURFACE ( 3, 1, ( 
 ( #59221, #21649 ),
 ( #26042, #59538 ),
 ( #16970, #45789 ),
 ( #49843, #50457 ) ),
 .UNSPECIFIED., .F., .F., .F. ) 
 B_SPLINE_SURFACE_WITH_KNOTS ( ( 4, 4 ),
 ( 2, 2 ),
 ( 0.000000000000000000, 1.000000000000000000 ),
 ( 0.000000000000000000, 1.000000000000000000 ),
 .UNSPECIFIED. ) 
 GEOMETRIC_REPRESENTATION_ITEM ( )  RATIONAL_B_SPLINE_SURFACE ( (
 ( 1.000000000000000000, 1.000000000000000000),
 ( 0.7269869731126817891, 0.9931720237060910339),
 ( 0.7269869731126817891, 0.9931720237060910339),
 ( 1.000000000000000000, 1.000000000000000000) ) ) 
 REPRESENTATION_ITEM ( '' )  SURFACE ( )  );
#248 = ORIENTED_EDGE ( 'NONE', *, *, #5501, .F. ) ;
#249 = CARTESIAN_POINT ( 'NONE',  ( 0.9722240741986378776, 16.95645453362518040, -39.41582013185131927 ) ) ;
#250 = FACE_OUTER_BOUND ( 'NONE', #162, .T. ) ;
#251 = B_SPLINE_CURVE_WITH_KNOTS ( 'NONE', 3,
 ( #19332, #43782, #824, #19959 ),
 .UNSPECIFIED., .F., .F.,
 ( 4, 4 ),
 ( 0.000000000000000000, 0.005013413432710153717 ),
 .UNSPECIFIED. ) ;
#252 = CARTESIAN_POINT ( 'NONE',  ( 0.9754292580325143458, 38.80678078702572265, -15.82280733156209784 ) ) ;
#253 = CARTESIAN_POINT ( 'NONE',  ( 0.8751705887134553219, -34.63284514348562482, -33.37254303619542384 ) ) ;
#254 = CARTESIAN_POINT ( 'NONE',  ( 0.9789889208857682767, 38.62063605787587051, 16.27210399817645126 ) ) ;
#255 = ORIENTED_EDGE ( 'NONE', *, *, #39405, .T. ) ;
#256 = EDGE_CURVE ( 'NONE', #600, #12966, #42031, .T. ) ;
#257 = EDGE_CURVE ( 'NONE', #37381, #21977, #57325, .T. ) ;
#258 = ORIENTED_EDGE ( 'NONE', *, *, #20245, .T. ) ;
#259 = CARTESIAN_POINT ( 'NONE',  ( 0.3676999524040323597, -7.853951980432424484, 43.40813312746703190 ) ) ;
#260 = CARTESIAN_POINT ( 'NONE',  ( 0.9769922540276056999, -41.15456160972863131, 7.914140117357955084 ) ) ;
#261 = CARTESIAN_POINT ( 'NONE',  ( -6.077587904424778920, -16.13490349385120481, -10.51003856501195877 ) ) ;
#262 = CARTESIAN_POINT ( 'NONE',  ( 0.9757402383260960210, -21.52772413548508368, 37.11731350497348103 ) ) ;
#263 = CARTESIAN_POINT ( 'NONE',  ( 0.5837157313716003770, 4.784661690600440664, -46.65130304813069273 ) ) ;
#264 =( NAMED_UNIT ( * ) PLANE_ANGLE_UNIT ( ) SI_UNIT ( $, .RADIAN. ) );
#265 = CARTESIAN_POINT ( 'NONE',  ( 4.549368137175248350, 0.000000000000000000, 0.000000000000000000 ) ) ;
#266 =( BOUNDED_SURFACE ( )  B_SPLINE_SURFACE ( 3, 1, ( 
 ( #49830, #53575 ),
 ( #35756, #6889 ),
 ( #40459, #1574 ),
 ( #29792, #1269 ) ),
 .UNSPECIFIED., .F., .F., .F. ) 
 B_SPLINE_SURFACE_WITH_KNOTS ( ( 4, 4 ),
 ( 2, 2 ),
 ( 0.000000000000000000, 1.000000000000000000 ),
 ( 0.000000000000000000, 1.000000000000000000 ),
 .UNSPECIFIED. ) 
 GEOMETRIC_REPRESENTATION_ITEM ( )  RATIONAL_B_SPLINE_SURFACE ( (
 ( 1.000000000000000000, 1.000000000000000000),
 ( 0.7269869731126821222, 0.9931720237060910339),
 ( 0.7269869731126821222, 0.9931720237060910339),
 ( 1.000000000000000000, 1.000000000000000000) ) ) 
 REPRESENTATION_ITEM ( '' )  SURFACE ( )  );
#267 = ORIENTED_EDGE ( 'NONE', *, *, #21360, .T. ) ;
#268 = CARTESIAN_POINT ( 'NONE',  ( -6.077587904424778920, -19.21689618909966413, -1.227567615774088017 ) ) ;
#269 = EDGE_CURVE ( 'NONE', #35355, #39250, #33541, .T. ) ;
#270 = CARTESIAN_POINT ( 'NONE',  ( 3.782542959838391727, 11.41479611462064980, -40.45911866388357936 ) ) ;
#271 = FACE_OUTER_BOUND ( 'NONE', #58195, .T. ) ;
#272 = CARTESIAN_POINT ( 'NONE',  ( 0.5797568599927143129, 40.66629966594037171, -23.35545718137295168 ) ) ;
#273 = FACE_OUTER_BOUND ( 'NONE', #5320, .T. ) ;
#274 = COLOUR_RGB ( '', 0.66274510, 0.83137255, 0.94901961) ;
#275 = CARTESIAN_POINT ( 'NONE',  ( 0.5850706913938534814, -47.50996714391777687, -6.071602062251110432 ) ) ;
#276 = ADVANCED_FACE ( 'NONE', ( #10344 ), #14742, .T. ) ;
#277 = EDGE_LOOP ( 'NONE', ( #3307, #822 ) ) ;
#278 = CARTESIAN_POINT ( 'NONE',  ( 1.227938101723748288, -6.439911493064859549, 42.43379953535183802 ) ) ;
#279 = CARTESIAN_POINT ( 'NONE',  ( 5.895881250540457863, 16.57931246612949394, -11.38657454016544968 ) ) ;
#280 = CARTESIAN_POINT ( 'NONE',  ( -6.077587904424778920, -12.94128980615176872, -14.25899854643104803 ) ) ;
#281 = DIRECTION ( 'NONE',  ( -1.000000000000000000, -0.000000000000000000, -0.000000000000000000 ) ) ;
#282 = DIRECTION ( 'NONE',  ( 1.000000000000000000, 0.000000000000000000, 0.000000000000000000 ) ) ;
#283 = ORIENTED_EDGE ( 'NONE', *, *, #47533, .F. ) ;
#284 = CARTESIAN_POINT ( 'NONE',  ( 4.960386119450151732, 7.741275488564681950, -43.06401187166018474 ) ) ;
#285 = CARTESIAN_POINT ( 'NONE',  ( 5.838029081930957709, 35.04472919977139611, 31.66910187339719940 ) ) ;
#286 = EDGE_CURVE ( 'NONE', #21806, #20018, #34185, .T. ) ;
#287 = CIRCLE ( 'NONE', #35352, 43.08621763946400307 ) ;
#288 = B_SPLINE_CURVE_WITH_KNOTS ( 'NONE', 3,
 ( #44380, #20544, #58724, #11151 ),
 .UNSPECIFIED., .F., .F.,
 ( 4, 4 ),
 ( 5.818439421673296370E-18, 0.004566006591234646368 ),
 .UNSPECIFIED. ) ;
#289 = FACE_OUTER_BOUND ( 'NONE', #54400, .T. ) ;
#290 = ORIENTED_EDGE ( 'NONE', *, *, #8641, .T. ) ;
#291 = DIRECTION ( 'NONE',  ( 0.000000000000000000, 0.000000000000000000, -1.000000000000000000 ) ) ;
#292 = EDGE_CURVE ( 'NONE', #49088, #39212, #16990, .T. ) ;
#293 = B_SPLINE_CURVE_WITH_KNOTS ( 'NONE', 3,
 ( #46059, #55716, #27232, #21301, #12534, #30685 ),
 .UNSPECIFIED., .F., .F.,
 ( 4, 2, 4 ),
 ( 9.842382305685178914E-18, 0.0002450742804987399766, 0.0004901485609974700871 ),
 .UNSPECIFIED. ) ;
#294 = CARTESIAN_POINT ( 'NONE',  ( 3.660176727303412036, -4.399934609596269475, -47.83637937224829528 ) ) ;
#295 = ORIENTED_EDGE ( 'NONE', *, *, #34419, .F. ) ;
#296 = B_SPLINE_CURVE_WITH_KNOTS ( 'NONE', 3,
 ( #42728, #61184, #18606, #18304, #13602, #32708 ),
 .UNSPECIFIED., .F., .F.,
 ( 4, 2, 4 ),
 ( 1.217335034318563839E-16, 0.0002448718616795921206, 0.0004897437233590624852 ),
 .UNSPECIFIED. ) ;
#297 = CARTESIAN_POINT ( 'NONE',  ( -6.078457390727109555, -6.654470124808820941, 18.06965794904637335 ) ) ;
#298 = ORIENTED_EDGE ( 'NONE', *, *, #8490, .F. ) ;
#299 = CARTESIAN_POINT ( 'NONE',  ( 4.956445790443988031, 47.01859095792194410, 2.605792484304518375 ) ) ;
#300 = ORIENTED_EDGE ( 'NONE', *, *, #3443, .F. ) ;
#301 = CARTESIAN_POINT ( 'NONE',  ( 4.962356264823601926, -41.65024625884322518, 6.040909239515423579 ) ) ;
#302 = CARTESIAN_POINT ( 'NONE',  ( -6.078075953587585900, 5.473785299353540523, -18.46165888385214870 ) ) ;
#303 = ORIENTED_EDGE ( 'NONE', *, *, #61917, .T. ) ;
#304 = FACE_OUTER_BOUND ( 'NONE', #29189, .T. ) ;
#305 = PRODUCT_DEFINITION_SHAPE ( 'NONE', 'NONE',  #61992 ) ;
#306 = ORIENTED_EDGE ( 'NONE', *, *, #19497, .F. ) ;
#307 = CARTESIAN_POINT ( 'NONE',  ( 0.2279481005628815338, -43.84759606547602573, 4.887924544401895055 ) ) ;
#308 = CARTESIAN_POINT ( 'NONE',  ( 0.5837157313716025975, 40.30294267679386877, 23.97727831037320456 ) ) ;
#309 = ORIENTED_EDGE ( 'NONE', *, *, #7412, .F. ) ;
#310 = CARTESIAN_POINT ( 'NONE',  ( 0.9730545539215883499, -16.88610103448528221, -39.44597740938079511 ) ) ;
#311 = CARTESIAN_POINT ( 'NONE',  ( 5.974727161628367256, 2.663664384318781941, -20.35137732084673345 ) ) ;
#312 = CARTESIAN_POINT ( 'NONE',  ( 0.5817217712918332229, 16.42911102810642632, 43.92401694784443578 ) ) ;
#313 = ORIENTED_EDGE ( 'NONE', *, *, #32073, .T. ) ;
#314 = ADVANCED_FACE ( 'NONE', ( #10034 ), #32031, .F. ) ;
#315 = CARTESIAN_POINT ( 'NONE',  ( 0.5837374860065646098, 44.31936661703473135, 18.16107481025614945 ) ) ;
#316 = CARTESIAN_POINT ( 'NONE',  ( 1.154321485836934169, -10.30834589251740141, 41.66001465002025128 ) ) ;
#317 = ORIENTED_EDGE ( 'NONE', *, *, #60187, .F. ) ;
#318 = CIRCLE ( 'NONE', #20387, 48.91267123290010943 ) ;
#319 = CARTESIAN_POINT ( 'NONE',  ( 0.5806925824938502512, 46.40146083665138832, -6.791670970259978013 ) ) ;
#320 = ADVANCED_FACE ( 'NONE', ( #53535 ), #44196, .F. ) ;
#321 = ORIENTED_EDGE ( 'NONE', *, *, #58759, .F. ) ;
#322 = CARTESIAN_POINT ( 'NONE',  ( 1.157643937452369043, 25.52398866004628886, 33.24948537160511108 ) ) ;
#323 = DIRECTION ( 'NONE',  ( -1.000000000000000000, -5.380183451256670742E-17, 1.298891185607911324E-16 ) ) ;
#324 = ORIENTED_EDGE ( 'NONE', *, *, #24698, .T. ) ;
#325 = CARTESIAN_POINT ( 'NONE',  ( 0.9788927965476030835, -34.63124975320486953, -23.60112609946664008 ) ) ;
#326 = CARTESIAN_POINT ( 'NONE',  ( 0.1152809850208376258, 25.42529477452768560, -36.06244123902498444 ) ) ;
#327 = CARTESIAN_POINT ( 'NONE',  ( 0.5998501479064708430, 5.759754759340140140, 47.76154736470759588 ) ) ;
#328 = CARTESIAN_POINT ( 'NONE',  ( 0.9790724872846759963, -22.51621571723094561, -35.34621959639500233 ) ) ;
#329 = EDGE_CURVE ( 'NONE', #33849, #9438, #31034, .T. ) ;
#330 = EDGE_CURVE ( 'NONE', #57580, #41543, #34967, .T. ) ;
#331 = VERTEX_POINT ( 'NONE', #19436 ) ;
#332 = CARTESIAN_POINT ( 'NONE',  ( 0.5980894510889448457, 47.60453381548683893, 6.974827154144264796 ) ) ;
#333 = EDGE_CURVE ( 'NONE', #28532, #55039, #19988, .T. ) ;
#334 = CARTESIAN_POINT ( 'NONE',  ( 0.8760168074887090262, 44.09317760313751933, -19.22870327415257563 ) ) ;
#335 = B_SPLINE_CURVE_WITH_KNOTS ( 'NONE', 3,
 ( #7423, #26237, #46002, #7741 ),
 .UNSPECIFIED., .F., .F.,
 ( 4, 4 ),
 ( 6.254634441385501517E-18, 0.004566006591234648103 ),
 .UNSPECIFIED. ) ;
#336 = MECHANICAL_DESIGN_GEOMETRIC_PRESENTATION_REPRESENTATION (  '', ( #58375 ), #3336 ) ;
#337 = CARTESIAN_POINT ( 'NONE',  ( 0.5807400328401637335, 41.75144119563886136, 23.47602859900728944 ) ) ;
#338 = CARTESIAN_POINT ( 'NONE',  ( 2.301430502907644726, 19.56449039932732603, -43.86847929982167216 ) ) ;
#339 = ADVANCED_FACE ( 'NONE', ( #24744 ), #40840, .F. ) ;
#340 = DIRECTION ( 'NONE',  ( 0.09722883295013598492, -0.9860961158916706770, -0.1347627703281412404 ) ) ;
#341 = CARTESIAN_POINT ( 'NONE',  ( 0.6001305935487315502, 6.798494447611584057, 47.62765676940946236 ) ) ;
#342 = CARTESIAN_POINT ( 'NONE',  ( 0.5797568665920704856, 46.55714410835498995, 5.626512336762159450 ) ) ;
#343 = CARTESIAN_POINT ( 'NONE',  ( -69.95594261585600293, 0.000000000000000000, -12.50000000000000000 ) ) ;
#344 = CARTESIAN_POINT ( 'NONE',  ( 0.5998501479064699549, 48.10473956285920138, -0.5236536531309904374 ) ) ;
#345 = CARTESIAN_POINT ( 'NONE',  ( 3.407937589446174087, 11.14158115674384142, -7.970324840161847391 ) ) ;
#346 = CARTESIAN_POINT ( 'NONE',  ( 0.8554163680231738898, 33.26717477998096228, -33.08323677136228724 ) ) ;
#347 = CARTESIAN_POINT ( 'NONE',  ( 0.5834584762367746036, -1.749022159738321536, 46.86338560644049522 ) ) ;
#348 = CARTESIAN_POINT ( 'NONE',  ( 0.5839254288179550612, -23.86932519546702380, -41.52446060675850248 ) ) ;
#349 = CARTESIAN_POINT ( 'NONE',  ( 0.5835871038041865466, 45.26563263149099470, -12.25793438440576821 ) ) ;
#350 = LINE ( 'NONE', #10092, #1144 ) ;
#351 = VERTEX_POINT ( 'NONE', #43564 ) ;
#352 = CARTESIAN_POINT ( 'NONE',  ( 0.5839254288179565044, 29.22920395911566160, -37.94310411505115610 ) ) ;
#353 = CARTESIAN_POINT ( 'NONE',  ( 2.879087469061463178, 18.80129513073439185, -39.78206855092381744 ) ) ;
#354 = CARTESIAN_POINT ( 'NONE',  ( 5.894904586330512508, -20.11291651039286066, -0.001227847351197789826 ) ) ;
#355 = VERTEX_POINT ( 'NONE', #58856 ) ;
#356 = CARTESIAN_POINT ( 'NONE',  ( 0.9757892942422815574, 5.651566539685822121, 42.53466646637865267 ) ) ;
#357 = DIRECTION ( 'NONE',  ( 0.07836865515943411409, 0.8593913859058514015, 0.5052769534812779906 ) ) ;
#358 = AXIS2_PLACEMENT_3D ( 'NONE', #19879, #43697, #29251 ) ;
#359 = UNCERTAINTY_MEASURE_WITH_UNIT (LENGTH_MEASURE( 1.000000000000000082E-05 ), #54349, 'distance_accuracy_value', 'NONE');
#360 = ORIENTED_EDGE ( 'NONE', *, *, #48950, .T. ) ;
#361 = ORIENTED_EDGE ( 'NONE', *, *, #7612, .T. ) ;
#362 = SHAPE_REPRESENTATION ( 'housing right', ( #14677 ), #14881 ) ;
#363 = EDGE_CURVE ( 'NONE', #33629, #19850, #31166, .T. ) ;
#364 = B_SPLINE_CURVE_WITH_KNOTS ( 'NONE', 3,
 ( #15023, #38221, #57268, #19406 ),
 .UNSPECIFIED., .F., .F.,
 ( 4, 4 ),
 ( 2.292215966409847280E-17, 0.004564976165746187711 ),
 .UNSPECIFIED. ) ;
#365 = CARTESIAN_POINT ( 'NONE',  ( 0.5997462898726536595, -31.02483596213057737, 38.06587952047342327 ) ) ;
#366 = ORIENTED_EDGE ( 'NONE', *, *, #38922, .T. ) ;
#367 = CARTESIAN_POINT ( 'NONE',  ( 5.331199999999999939, 0.000000000000000000, 12.55882000000000076 ) ) ;
#368 = ORIENTED_EDGE ( 'NONE', *, *, #18760, .F. ) ;
#369 = ORIENTED_EDGE ( 'NONE', *, *, #45796, .F. ) ;
#370 = CARTESIAN_POINT ( 'NONE',  ( 2.526464513654347765, -41.81190200959792236, -9.948146339971660979 ) ) ;
#371 = VERTEX_POINT ( 'NONE', #31845 ) ;
#372 = CARTESIAN_POINT ( 'NONE',  ( 2.618530812446111078, 9.522253559614041407, 46.03317799527443555 ) ) ;
#373 = CARTESIAN_POINT ( 'NONE',  ( 0.8760168074886960365, -28.57146030081953114, -38.69913431881812471 ) ) ;
#374 = CIRCLE ( 'NONE', #52438, 42.92674063221959813 ) ;
#375 = DIRECTION ( 'NONE',  ( -0.1024043820194934368, 0.2447326578667261276, 0.9641676559171094008 ) ) ;
#376 = VERTEX_POINT ( 'NONE', #3003 ) ;
#377 = CARTESIAN_POINT ( 'NONE',  ( 0.7044674535452954967, 27.40191655692298767, 40.75460332058619883 ) ) ;
#378 = CARTESIAN_POINT ( 'NONE',  ( 0.9783242366443567484, -39.67693573533197338, 13.49352662801158331 ) ) ;
#379 = ORIENTED_EDGE ( 'NONE', *, *, #18746, .F. ) ;
#380 = EDGE_LOOP ( 'NONE', ( #10073, #51406, #39218, #28392 ) ) ;
#381 = CARTESIAN_POINT ( 'NONE',  ( -1.399999999999998579, 9.184850993605175555E-16, 7.500000000000022204 ) ) ;
#382 = EDGE_LOOP ( 'NONE', ( #16913, #17732, #52074, #3845 ) ) ;
#383 = CARTESIAN_POINT ( 'NONE',  ( 2.706805983486680223, 34.55979480539205184, 27.24695756096361166 ) ) ;
#384 = CARTESIAN_POINT ( 'NONE',  ( -6.077587904424778920, 9.987489566522585349, 16.46347695818028001 ) ) ;
#385 = CARTESIAN_POINT ( 'NONE',  ( 4.967162193818130511, 14.26841313271336809, -40.65506779172149976 ) ) ;
#386 = CARTESIAN_POINT ( 'NONE',  ( 4.967162193818130511, 0.000000000000000000, 0.000000000000000000 ) ) ;
#387 = EDGE_CURVE ( 'NONE', #3069, #4945, #35089, .T. ) ;
#388 = ORIENTED_EDGE ( 'NONE', *, *, #42181, .T. ) ;
#389 = CARTESIAN_POINT ( 'NONE',  ( 4.549368137175248350, 0.000000000000000000, 0.000000000000000000 ) ) ;
#390 = CARTESIAN_POINT ( 'NONE',  ( 3.782625744892854414, -16.11616831265073557, 38.82663033297269806 ) ) ;
#391 = ADVANCED_FACE ( 'NONE', ( #36552 ), #45224, .F. ) ;
#392 = CARTESIAN_POINT ( 'NONE',  ( 4.967162193818132288, 19.45289607368876617, -38.44485641567052880 ) ) ;
#393 = DIRECTION ( 'NONE',  ( -1.000000000000000000, 0.000000000000000000, 0.000000000000000000 ) ) ;
#394 = EDGE_LOOP ( 'NONE', ( #29612, #23490, #21931, #13933 ) ) ;
#395 = CARTESIAN_POINT ( 'NONE',  ( 0.08486401232817714080, 0.000000000000000000, 44.12552607296456131 ) ) ;
#396 = CARTESIAN_POINT ( 'NONE',  ( 0.8744876279028306332, 33.66006955981207227, 35.74003032466684004 ) ) ;
#397 = EDGE_CURVE ( 'NONE', #43088, #32860, #59563, .T. ) ;
#398 = CARTESIAN_POINT ( 'NONE',  ( -6.072942160501519027, 11.99473239968586391, 15.06421444845188518 ) ) ;
#399 = CARTESIAN_POINT ( 'NONE',  ( 0.6016117650947691020, -35.51782622858503657, -33.91216705314681690 ) ) ;
#400 = EDGE_CURVE ( 'NONE', #39651, #55243, #39806, .T. ) ;
#401 = ORIENTED_EDGE ( 'NONE', *, *, #17470, .T. ) ;
#402 = ORIENTED_EDGE ( 'NONE', *, *, #26650, .F. ) ;
#403 = DIRECTION ( 'NONE',  ( 0.000000000000000000, 0.000000000000000000, 1.000000000000000000 ) ) ;
#404 = EDGE_CURVE ( 'NONE', #47983, #17365, #23744, .T. ) ;
#405 = CARTESIAN_POINT ( 'NONE',  ( 1.088313998177380837, -20.77783415101598763, -37.54798835078477026 ) ) ;
#406 = LINE ( 'NONE', #42444, #21829 ) ;
#407 = CIRCLE ( 'NONE', #30421, 43.92652462719577500 ) ;
#408 = CARTESIAN_POINT ( 'NONE',  ( 0.8751705887134423323, -13.30665218149394669, 46.21789262997734227 ) ) ;
#409 = CARTESIAN_POINT ( 'NONE',  ( 0.8760168074887090262, 11.58706983520326084, -46.68716261866164530 ) ) ;
#410 = LINE ( 'NONE', #3884, #31382 ) ;
#411 = DIRECTION ( 'NONE',  ( -1.000000000000000000, -0.000000000000000000, -0.000000000000000000 ) ) ;
#412 = DIRECTION ( 'NONE',  ( 0.000000000000000000, 0.000000000000000000, 1.000000000000000000 ) ) ;
#413 = CARTESIAN_POINT ( 'NONE',  ( 0.8753041380234524160, -48.57841546934886168, 7.160717726618433865 ) ) ;
#414 = B_SPLINE_CURVE_WITH_KNOTS ( 'NONE', 3,
 ( #40927, #35601, #2041, #21474, #2662, #7043 ),
 .UNSPECIFIED., .F., .F.,
 ( 4, 2, 4 ),
 ( 3.471140604459641645E-18, 0.0002291459268755710208, 0.0004582918537511385722 ),
 .UNSPECIFIED. ) ;
#415 = CONICAL_SURFACE ( 'NONE', #48459, 42.08604991992415023, 1.569615340895231137 ) ;
#416 = CARTESIAN_POINT ( 'NONE',  ( 0.1103310638050662013, 30.55179781597996680, -30.43528225250908648 ) ) ;
#417 = CARTESIAN_POINT ( 'NONE',  ( 1.000433927950263424, 3.539116715176812367, -41.75994888082603751 ) ) ;
#418 = B_SPLINE_CURVE_WITH_KNOTS ( 'NONE', 3,
 ( #44504, #16914, #36031, #25057, #6222, #26285 ),
 .UNSPECIFIED., .F., .F.,
 ( 4, 2, 4 ),
 ( 1.266823315017301927E-16, 0.0002450741128632354863, 0.0004901482257263442294 ),
 .UNSPECIFIED. ) ;
#420 = ORIENTED_EDGE ( 'NONE', *, *, #21979, .T. ) ;
#419 = EDGE_CURVE ( 'NONE', #16304, #19741, #25964, .T. ) ;
#421 = CARTESIAN_POINT ( 'NONE',  ( 5.960721111146673579, -10.26825948882938278, 17.77250458025974567 ) ) ;
#422 = CARTESIAN_POINT ( 'NONE',  ( 0.1119899015040011631, -35.69472091171160599, 25.93931778647085196 ) ) ;
#424 = EDGE_CURVE ( 'NONE', #19414, #14922, #59166, .T. ) ;
#423 = CARTESIAN_POINT ( 'NONE',  ( 0.1157991065609915299, -35.41034345021505203, 26.32584172017128310 ) ) ;
#425 = CARTESIAN_POINT ( 'NONE',  ( 5.895881250540457863, -15.78174954617507453, -12.46852288244697071 ) ) ;
#426 = VECTOR ( 'NONE', #13703, 1000.000000000000000 ) ;
#427 = CARTESIAN_POINT ( 'NONE',  ( 2.643462169533613793, -17.09809940585690313, 44.89050350746123286 ) ) ;
#428 = CARTESIAN_POINT ( 'NONE',  ( 0.6029442701453591180, 32.95047274681666494, -36.41169552382268648 ) ) ;
#429 = CARTESIAN_POINT ( 'NONE',  ( 0.6254087463353900089, 23.45485308995599993, -42.00124903776048058 ) ) ;
#430 = CONTEXT_DEPENDENT_SHAPE_REPRESENTATION ( #40883, #40299 ) ;
#431 = CARTESIAN_POINT ( 'NONE',  ( 0.1073791018717578927, 21.98088480513665388, -37.10214135362866728 ) ) ;
#432 = CARTESIAN_POINT ( 'NONE',  ( 0.8560838555295158248, -14.76796170096741534, 44.52280473286123907 ) ) ;
#433 = CARTESIAN_POINT ( 'NONE',  ( 4.958415959904820980, -16.79601473596579453, 42.20305489904562535 ) ) ;
#434 = CARTESIAN_POINT ( 'NONE',  ( 4.975610109902397937, -41.30423662854430944, -26.19941685746064053 ) ) ;
#435 = CARTESIAN_POINT ( 'NONE',  ( -6.016761891674564211, 4.880293656734964181, 18.20023637398600869 ) ) ;
#437 = VERTEX_POINT ( 'NONE', #22126 ) ;
#436 = DIRECTION ( 'NONE',  ( -1.000000000000000000, -0.000000000000000000, -0.000000000000000000 ) ) ;
#438 = EDGE_LOOP ( 'NONE', ( #51636, #8049, #36131, #12773 ) ) ;
#439 = DIRECTION ( 'NONE',  ( 0.000000000000000000, 0.000000000000000000, 1.000000000000000000 ) ) ;
#440 = FACE_OUTER_BOUND ( 'NONE', #59744, .T. ) ;
#441 = CARTESIAN_POINT ( 'NONE',  ( 0.8744876279028306332, -48.57046782678520458, 7.159588358747709158 ) ) ;
#442 = ORIENTED_EDGE ( 'NONE', *, *, #38279, .F. ) ;
#443 = CARTESIAN_POINT ( 'NONE',  ( 4.962356264823608143, 39.61238188121388504, 14.21600504921214814 ) ) ;
#444 = CARTESIAN_POINT ( 'NONE',  ( 0.6067099128993267421, 37.56352526808347392, -29.71710940500694065 ) ) ;
#445 = CARTESIAN_POINT ( 'NONE',  ( 5.860006189529234355, -15.52021937683242570, -45.66786516969946064 ) ) ;
#446 =( BOUNDED_SURFACE ( )  B_SPLINE_SURFACE ( 3, 1, ( 
 ( #42165, #8925 ),
 ( #28037, #32125 ),
 ( #2978, #56829 ),
 ( #46231, #61218 ) ),
 .UNSPECIFIED., .F., .F., .F. ) 
 B_SPLINE_SURFACE_WITH_KNOTS ( ( 4, 4 ),
 ( 2, 2 ),
 ( 0.000000000000000000, 1.000000000000000000 ),
 ( 0.000000000000000000, 1.000000000000000000 ),
 .UNSPECIFIED. ) 
 GEOMETRIC_REPRESENTATION_ITEM ( )  RATIONAL_B_SPLINE_SURFACE ( (
 ( 1.000000000000000000, 1.000000000000000000),
 ( 0.9953040768229013402, 0.8617119497784988535),
 ( 0.9953040768229013402, 0.8617119497784988535),
 ( 1.000000000000000000, 1.000000000000000000) ) ) 
 REPRESENTATION_ITEM ( '' )  SURFACE ( )  );
#447 = B_SPLINE_CURVE_WITH_KNOTS ( 'NONE', 3,
 ( #26125, #21427, #16736, #35853, #54922, #31132, #50240, #45560, #2614, #40877, #36165, #59942, #17052, #55539, #31763, #50851 ),
 .UNSPECIFIED., .F., .F.,
 ( 4, 3, 3, 3, 3, 4 ),
 ( 1.095097866269904594E-17, 0.0002724568934985561975, 0.0004086836638483808517, 0.0005449104342063608745, 0.0008173270854453682996, 0.001089761613562689442 ),
 .UNSPECIFIED. ) ;
#448 = VERTEX_POINT ( 'NONE', #17428 ) ;
#449 = AXIS2_PLACEMENT_3D ( 'NONE', #23041, #9232, #46861 ) ;
#450 = VERTEX_POINT ( 'NONE', #35397 ) ;
#451 = EDGE_CURVE ( 'NONE', #48858, #40875, #52468, .T. ) ;
#452 = CARTESIAN_POINT ( 'NONE',  ( 0.8744876279028306332, 32.34273794994798834, -36.93639603806098393 ) ) ;
#453 = CARTESIAN_POINT ( 'NONE',  ( 1.231276596079887264, 33.41651732065550817, 25.31033664684050777 ) ) ;
#454 = CARTESIAN_POINT ( 'NONE',  ( -2.569797478183790229, 14.55946937464483959, -1.464172661884012960 ) ) ;
#455 = CARTESIAN_POINT ( 'NONE',  ( 0.5824936645240066380, 17.19419371894991500, -43.63024044622647324 ) ) ;
#456 = CARTESIAN_POINT ( 'NONE',  ( 0.6254087463353900089, -17.77193046492983441, 44.70339519268186024 ) ) ;
#457 = B_SPLINE_CURVE_WITH_KNOTS ( 'NONE', 3,
 ( #61646, #61952, #57249, #33493, #52569, #5253, #28771, #46982, #61341, #18456, #47895, #37582, #56652, #54096, #25009, #25303, #35038, #58486, #25614 ),
 .UNSPECIFIED., .F., .F.,
 ( 4, 3, 3, 3, 3, 3, 4 ),
 ( 0.000000000000000000, 0.0002724573126191725029, 0.0004086839781548403999, 0.0005449106435901787757, 0.0006811373090491486390, 0.0008459866663933673144, 0.001010840725717216185 ),
 .UNSPECIFIED. ) ;
#458 = FACE_OUTER_BOUND ( 'NONE', #15532, .T. ) ;
#459 = COLOUR_RGB ( '', 0.66274510, 0.83137255, 0.94901961) ;
#460 = CARTESIAN_POINT ( 'NONE',  ( 5.960221823109900008, 2.673723662181063165, 20.35070456576735509 ) ) ;
#461 = VERTEX_POINT ( 'NONE', #18671 ) ;
#462 = VERTEX_POINT ( 'NONE', #56553 ) ;
#463 = DIRECTION ( 'NONE',  ( -1.000000000000000000, -0.000000000000000000, -0.000000000000000000 ) ) ;
#464 = CARTESIAN_POINT ( 'NONE',  ( 0.9268187852002115479, 44.04984738791743126, 1.834469408251422351 ) ) ;
#465 = VECTOR ( 'NONE', #30114, 999.9999999999998863 ) ;
#466 = ORIENTED_EDGE ( 'NONE', *, *, #12676, .F. ) ;
#467 = CARTESIAN_POINT ( 'NONE',  ( 4.975801465491695552, 15.94009207552985252, 45.18341283946464415 ) ) ;
#468 = FACE_OUTER_BOUND ( 'NONE', #1447, .T. ) ;
#469 = CARTESIAN_POINT ( 'NONE',  ( 0.6030672727741701600, 46.44558360016994669, 12.53539249098730757 ) ) ;
#470 = CARTESIAN_POINT ( 'NONE',  ( 4.549368137175248350, 0.000000000000000000, 0.000000000000000000 ) ) ;
#471 = VECTOR ( 'NONE', #9116, 1000.000000000000114 ) ;
#472 = VERTEX_POINT ( 'NONE', #13670 ) ;
#473 = VERTEX_POINT ( 'NONE', #43416 ) ;
#474 = DIRECTION ( 'NONE',  ( -1.000000000000000000, 0.000000000000000000, 0.000000000000000000 ) ) ;
#475 = CARTESIAN_POINT ( 'NONE',  ( 0.9754642270333672149, -42.51806607596984833, -5.774842730422477644 ) ) ;
#476 = CARTESIAN_POINT ( 'NONE',  ( 0.1073791018717483448, -37.58707531572191840, -21.14095454447545919 ) ) ;
#477 = CARTESIAN_POINT ( 'NONE',  ( 0.8554163680231708922, 28.56078411578483056, -37.22213163970263139 ) ) ;
#478 = VERTEX_POINT ( 'NONE', #23060 ) ;
#479 = CARTESIAN_POINT ( 'NONE',  ( 0.6027444965799114707, 4.845435411165755824, -48.86778357531332517 ) ) ;
#480 = EDGE_CURVE ( 'NONE', #24850, #5676, #46177, .T. ) ;
#481 = ORIENTED_EDGE ( 'NONE', *, *, #49627, .F. ) ;
#482 = CARTESIAN_POINT ( 'NONE',  ( 4.962356264823602814, 39.61238188121407688, -14.21600504921160812 ) ) ;
#483 = CARTESIAN_POINT ( 'NONE',  ( 0.1129192098497447394, 10.29049805561828101, 42.90754522869457332 ) ) ;
#484 = ORIENTED_EDGE ( 'NONE', *, *, #31844, .F. ) ;
#485 = CARTESIAN_POINT ( 'NONE',  ( -6.017396004339687465, -4.878103249821196030, 18.20079405513548565 ) ) ;
#486 = EDGE_CURVE ( 'NONE', #49719, #55841, #52030, .T. ) ;
#487 = CARTESIAN_POINT ( 'NONE',  ( 0.6009453534118440743, -47.75104957283902962, 5.846398087358569029 ) ) ;
#488 = CARTESIAN_POINT ( 'NONE',  ( 4.691466044806103852, -25.04870410140763326, -36.88741755356061702 ) ) ;
#489 = B_SPLINE_CURVE_WITH_KNOTS ( 'NONE', 3,
 ( #45173, #59532, #34830, #7209, #21337, #54832 ),
 .UNSPECIFIED., .F., .F.,
 ( 4, 2, 4 ),
 ( 0.000000000000000000, 0.0002291966416970804880, 0.0004583932833941609759 ),
 .UNSPECIFIED. ) ;
#490 = ORIENTED_EDGE ( 'NONE', *, *, #26338, .F. ) ;
#491 = CARTESIAN_POINT ( 'NONE',  ( 0.8753041380234524160, 49.05142151719380195, 2.257515230415333196 ) ) ;
#492 = CARTESIAN_POINT ( 'NONE',  ( 4.956445790443998689, -17.42806872899825521, 43.74700527484080936 ) ) ;
#493 = CARTESIAN_POINT ( 'NONE',  ( 0.9754292589017224957, -40.94879475388736267, 8.917604784878262691 ) ) ;
#494 = AXIS2_PLACEMENT_3D ( 'NONE', #841, #54061, #35924 ) ;
#495 = CARTESIAN_POINT ( 'NONE',  ( 0.6031357023905875581, 29.32055886552322477, -38.13964912630303417 ) ) ;
#496 = CARTESIAN_POINT ( 'NONE',  ( 0.1129192098497455998, -38.68182264534154058, 21.22895156665764915 ) ) ;
#497 = VERTEX_POINT ( 'NONE', #19290 ) ;
#498 = CARTESIAN_POINT ( 'NONE',  ( 0.5809828226811565299, -23.47450554821739743, 41.74875432577639600 ) ) ;
#499 = CARTESIAN_POINT ( 'NONE',  ( 0.9789233960466690032, 41.51700863864244440, 5.716180589452370064 ) ) ;
#500 = CARTESIAN_POINT ( 'NONE',  ( 5.894904586330512508, -15.78536547177706773, 12.46401416013601171 ) ) ;
#501 = ORIENTED_EDGE ( 'NONE', *, *, #49290, .F. ) ;
#502 = CARTESIAN_POINT ( 'NONE',  ( 5.895881250540457863, 10.82621851909522803, 16.95053610317680892 ) ) ;
#503 = LINE ( 'NONE', #38764, #11349 ) ;
#505 = EDGE_CURVE ( 'NONE', #5333, #39487, #51048, .T. ) ;
#504 = CARTESIAN_POINT ( 'NONE',  ( 4.956445790444004018, -47.08764048036452721, -0.5405220916603282744 ) ) ;
#506 = CARTESIAN_POINT ( 'NONE',  ( 5.895881250540457863, 19.71075194021738852, 4.001742065590625508 ) ) ;
#507 = CARTESIAN_POINT ( 'NONE',  ( 0.8557997880470690211, -28.43566216844996930, 38.55640757422429488 ) ) ;
#508 = LINE ( 'NONE', #20561, #47490 ) ;
#509 = SURFACE_STYLE_USAGE ( .BOTH. , #19650 ) ;
#510 = CARTESIAN_POINT ( 'NONE',  ( 4.956445790443991584, 39.12691469763999663, 26.20348443209871903 ) ) ;
#511 = DIRECTION ( 'NONE',  ( -0.07906939808003034253, -0.7447223275783662055, -0.6626738904570801392 ) ) ;
#512 = AXIS2_PLACEMENT_3D ( 'NONE', #37885, #12518, #51011 ) ;
#513 = CARTESIAN_POINT ( 'NONE',  ( 0.2885697896453121580, -26.88157175352913342, 33.71073718007492914 ) ) ;
#515 = ORIENTED_EDGE ( 'NONE', *, *, #31367, .T. ) ;
#514 = CARTESIAN_POINT ( 'NONE',  ( 5.880360259849739535, 21.17507050419515480, -43.04573319267424125 ) ) ;
#516 = VERTEX_POINT ( 'NONE', #28669 ) ;
#517 = CARTESIAN_POINT ( 'NONE',  ( 0.5980271706414711508, -47.67913160907373538, 11.77920421107846316 ) ) ;
#518 = CIRCLE ( 'NONE', #13553, 5.612499999999999822 ) ;
#519 = DIRECTION ( 'NONE',  ( -1.000000000000000000, -0.000000000000000000, -0.000000000000000000 ) ) ;
#520 = CARTESIAN_POINT ( 'NONE',  ( 0.5786265663353153954, 47.89572889566446179, -0.7221568112308096588 ) ) ;
#521 = AXIS2_PLACEMENT_3D ( 'NONE', #61352, #4959, #18467 ) ;
#522 = FACE_OUTER_BOUND ( 'NONE', #7239, .T. ) ;
#523 = CARTESIAN_POINT ( 'NONE',  ( 0.5819845901640490204, -47.54333976522121219, 5.801229454883783276 ) ) ;
#524 = CARTESIAN_POINT ( 'NONE',  ( 0.1157991065609915993, 9.897904771235362276, -42.99969589052061281 ) ) ;
#525 = ORIENTED_EDGE ( 'NONE', *, *, #29778, .F. ) ;
#526 = EDGE_CURVE ( 'NONE', #5254, #21667, #31964, .T. ) ;
#527 = CARTESIAN_POINT ( 'NONE',  ( 0.2279481005628749279, -22.21835642701406144, -38.11624489315645548 ) ) ;
#528 =( BOUNDED_SURFACE ( )  B_SPLINE_SURFACE ( 3, 1, ( 
 ( #7956, #17065 ),
 ( #3239, #18301 ),
 ( #36177, #22999 ),
 ( #13289, #2627 ) ),
 .UNSPECIFIED., .F., .F., .F. ) 
 B_SPLINE_SURFACE_WITH_KNOTS ( ( 4, 4 ),
 ( 2, 2 ),
 ( 0.000000000000000000, 1.000000000000000000 ),
 ( 0.000000000000000000, 1.000000000000000000 ),
 .UNSPECIFIED. ) 
 GEOMETRIC_REPRESENTATION_ITEM ( )  RATIONAL_B_SPLINE_SURFACE ( (
 ( 1.000000000000000000, 1.000000000000000000),
 ( 0.9953485035131437453, 0.8621029689291515030),
 ( 0.9953485035131437453, 0.8621029689291515030),
 ( 1.000000000000000000, 1.000000000000000000) ) ) 
 REPRESENTATION_ITEM ( '' )  SURFACE ( )  );
#529 = CARTESIAN_POINT ( 'NONE',  ( -6.078457390727109555, -11.01309887717693670, 15.79576412077085656 ) ) ;
#530 = CARTESIAN_POINT ( 'NONE',  ( 4.975801465491695552, 0.000000000000000000, 0.000000000000000000 ) ) ;
#531 = ORIENTED_EDGE ( 'NONE', *, *, #50574, .F. ) ;
#532 = B_SPLINE_CURVE_WITH_KNOTS ( 'NONE', 3,
 ( #47179, #28362, #4227, #47482 ),
 .UNSPECIFIED., .F., .F.,
 ( 4, 4 ),
 ( 0.000000000000000000, 0.005004948556313794893 ),
 .UNSPECIFIED. ) ;
#533 = ADVANCED_FACE ( 'NONE', ( #9251 ), #17209, .F. ) ;
#534 = DIRECTION ( 'NONE',  ( -1.000000000000000000, -0.000000000000000000, -0.000000000000000000 ) ) ;
#535 = CARTESIAN_POINT ( 'NONE',  ( 4.962356264823598373, -19.84272732133986139, 37.11471096901200895 ) ) ;
#536 = VERTEX_POINT ( 'NONE', #46883 ) ;
#537 = EDGE_CURVE ( 'NONE', #3024, #29827, #532, .T. ) ;
#538 = CARTESIAN_POINT ( 'NONE',  ( 4.549368137175248350, 40.58005590356670211, 13.99871866169379508 ) ) ;
#539 = VERTEX_POINT ( 'NONE', #4530 ) ;
#540 = CARTESIAN_POINT ( 'NONE',  ( 52.25260954720639006, 15.37154784856826772, -1.995153943981983202 ) ) ;
#541 = CARTESIAN_POINT ( 'NONE',  ( 0.3676999524040323597, -2.238562284876542741, 44.05609404179593724 ) ) ;
#542 = ORIENTED_EDGE ( 'NONE', *, *, #53181, .F. ) ;
#543 = FACE_OUTER_BOUND ( 'NONE', #2482, .T. ) ;
#544 = CARTESIAN_POINT ( 'NONE',  ( 5.895596859100789899, -4.659086063546006073, 19.56581458219818259 ) ) ;
#545 = CARTESIAN_POINT ( 'NONE',  ( 0.5997462898726536595, 22.24958391914503153, 43.77793560195857481 ) ) ;
#546 = CARTESIAN_POINT ( 'NONE',  ( 7.147292112312093160, -11.82536368408644911, -2.999999999999993339 ) ) ;
#547 = ORIENTED_EDGE ( 'NONE', *, *, #20916, .F. ) ;
#548 = CARTESIAN_POINT ( 'NONE',  ( 4.975610109902397937, 48.90928568712960356, 0.5754830253899292369 ) ) ;
#549 = ORIENTED_EDGE ( 'NONE', *, *, #18643, .T. ) ;
#550 = CARTESIAN_POINT ( 'NONE',  ( 1.000110580585049425, 40.58939401150527004, -10.43640630440781258 ) ) ;
#551 = CONICAL_SURFACE ( 'NONE', #54554, 43.08621763946400307, 1.568696531533066763 ) ;
#552 = ORIENTED_EDGE ( 'NONE', *, *, #15034, .T. ) ;
#553 = ADVANCED_FACE ( 'NONE', ( #4842 ), #51575, .F. ) ;
#554 = ORIENTED_EDGE ( 'NONE', *, *, #59411, .T. ) ;
#555 = CARTESIAN_POINT ( 'NONE',  ( 5.910764540655177868, 0.6875337509668891789, -20.10046108452351987 ) ) ;
#556 = CARTESIAN_POINT ( 'NONE',  ( 0.9772918015221170318, 35.84507786591080958, -21.71329658383247363 ) ) ;
#557 = AXIS2_PLACEMENT_3D ( 'NONE', #18443, #31926, #56946 ) ;
#558 = CARTESIAN_POINT ( 'NONE',  ( -2.739355103387248747, 13.33354922980911361, -6.712974891005759837 ) ) ;
#559 = EDGE_LOOP ( 'NONE', ( #5677, #4763, #51928, #14978 ) ) ;
#560 = FACE_OUTER_BOUND ( 'NONE', #30769, .T. ) ;
#561 = EDGE_CURVE ( 'NONE', #53916, #49170, #12131, .T. ) ;
#562 = CARTESIAN_POINT ( 'NONE',  ( 0.7057020205115049905, 11.58334423512235922, 46.47981817772228652 ) ) ;
#563 = CARTESIAN_POINT ( 'NONE',  ( -6.063463321072278589, 19.25669258467947387, 0.01559418547018328639 ) ) ;
#564 = AXIS2_PLACEMENT_3D ( 'NONE', #56138, #46464, #17637 ) ;
#565 = ORIENTED_EDGE ( 'NONE', *, *, #41540, .F. ) ;
#566 = B_SPLINE_CURVE_WITH_KNOTS ( 'NONE', 3,
 ( #25141, #5401, #33641, #24529, #7175, #53940, #58323, #5699, #11936, #43670, #15144, #53329, #10440, #48640, #24846, #43986, #39270, #15449, #31012 ),
 .UNSPECIFIED., .F., .F.,
 ( 4, 3, 3, 3, 3, 3, 4 ),
 ( 1.517943542627326963E-18, 0.0002612768053151706790, 0.0003919133833142909797, 0.0005225499612322605366, 0.0006531865391693358501, 0.0008112755173415187732, 0.0009693688056799720310 ),
 .UNSPECIFIED. ) ;
#567 = ADVANCED_FACE ( 'NONE', ( #52778 ), #57973, .F. ) ;
#568 = ORIENTED_EDGE ( 'NONE', *, *, #7137, .F. ) ;
#569 = CARTESIAN_POINT ( 'NONE',  ( 4.962356264823608143, 0.000000000000000000, 0.000000000000000000 ) ) ;
#570 = B_SPLINE_CURVE_WITH_KNOTS ( 'NONE', 3,
 ( #8385, #3987, #23127, #3374, #22510, #41628, #56005, #13125, #32224, #27508, #46636, #3679, #41946, #61013, #18121, #37242, #42257, #56310, #18429, #13424, #32531, #43726, #20817, #5753, #16120 ),
 .UNSPECIFIED., .F., .F.,
 ( 4, 3, 3, 3, 3, 3, 3, 3, 4 ),
 ( 5.553824967135426632E-18, 0.0005656085177311408327, 0.001131215744874501140, 0.001696821861372767651, 0.002262427090022497284, 0.002828031679238745058, 0.003393635864401604862, 0.003977030878808131623, 0.004561030005651157265 ),
 .UNSPECIFIED. ) ;
#571 = CARTESIAN_POINT ( 'NONE',  ( -6.078075953587585900, -18.90195907099241879, 3.675747206441630333 ) ) ;
#572 = CARTESIAN_POINT ( 'NONE',  ( 5.000000000000007994, -58.44237546506767700, -54.69470952477997372 ) ) ;
#573 = CARTESIAN_POINT ( 'NONE',  ( 0.9790850452238877288, -27.09605925476339294, -31.97093841484085885 ) ) ;
#574 = CARTESIAN_POINT ( 'NONE',  ( 0.5806925824938499181, 5.237374507879953178, -46.60249210726582447 ) ) ;
#575 = ORIENTED_EDGE ( 'NONE', *, *, #20466, .T. ) ;
#576 = ORIENTED_EDGE ( 'NONE', *, *, #47910, .T. ) ;
#577 = CARTESIAN_POINT ( 'NONE',  ( 0.6017667736363749853, 12.11362382130071502, 46.55748817282779584 ) ) ;
#579 = EDGE_CURVE ( 'NONE', #58789, #16193, #41322, .T. ) ;
#578 = CARTESIAN_POINT ( 'NONE',  ( 0.5997462898726536595, -20.35457962188166192, -44.69052157405179315 ) ) ;
#580 = CARTESIAN_POINT ( 'NONE',  ( 0.1129192098497447394, -42.55567333040724520, 11.66046547873710537 ) ) ;
#581 = CARTESIAN_POINT ( 'NONE',  ( 0.9754402186311948997, -21.29160191075025210, 37.25324696807224001 ) ) ;
#582 = CARTESIAN_POINT ( 'NONE',  ( 3.680882792899938138, 43.58303137875407174, -20.05474345988764284 ) ) ;
#583 = FILL_AREA_STYLE_COLOUR ( '', #10848 ) ;
#584 = CARTESIAN_POINT ( 'NONE',  ( 5.965394784446458765, 18.95742317323944803, -7.868087674480759297 ) ) ;
#585 = EDGE_LOOP ( 'NONE', ( #45645, #16766, #10272, #13377 ) ) ;
#586 = CARTESIAN_POINT ( 'NONE',  ( 0.6016117650947689910, 37.16599190767838223, -32.09735346976265191 ) ) ;
#587 = CARTESIAN_POINT ( 'NONE',  ( 5.901764892641288895, -22.68842833057508912, -43.39615982236257707 ) ) ;
#588 = CARTESIAN_POINT ( 'NONE',  ( 0.1129192098497447394, 30.02178898772887550, 32.33641869102754640 ) ) ;
#589 = FACE_OUTER_BOUND ( 'NONE', #57216, .T. ) ;
#590 = DIRECTION ( 'NONE',  ( -0.1011922191286467598, 0.6101824289146680069, 0.7857719377985040721 ) ) ;
#591 = CARTESIAN_POINT ( 'NONE',  ( 0.9787464366903563251, -34.65110827157835161, 23.57190464179372569 ) ) ;
#592 = CARTESIAN_POINT ( 'NONE',  ( 0.5807400328401574052, -47.55718917606839824, -5.711437504336464244 ) ) ;
#593 = VERTEX_POINT ( 'NONE', #44049 ) ;
#594 = CARTESIAN_POINT ( 'NONE',  ( 1.600000000000000089, -11.64055411052240352, -1.199999999999999956 ) ) ;
#595 = CARTESIAN_POINT ( 'NONE',  ( 0.5804410086790514622, -38.97211966759181934, 26.09010809617888427 ) ) ;
#596 = AXIS2_PLACEMENT_3D ( 'NONE', #6152, #30291, #11204 ) ;
#597 = CARTESIAN_POINT ( 'NONE',  ( 0.9268187852002115479, 24.40384675953001192, -36.71793289723704135 ) ) ;
#598 = CARTESIAN_POINT ( 'NONE',  ( 2.706805983486680223, 40.34082766586489299, 17.58959171080285699 ) ) ;
#599 = DIRECTION ( 'NONE',  ( 0.1024043820194936449, 0.01315135725335150538, 0.9946559125373961585 ) ) ;
#600 = VERTEX_POINT ( 'NONE', #1078 ) ;
#601 = EDGE_CURVE ( 'NONE', #54484, #21442, #16427, .T. ) ;
#602 = CARTESIAN_POINT ( 'NONE',  ( 0.3622758884714730732, -15.73321244754880688, 40.13994584881756111 ) ) ;
#603 = CARTESIAN_POINT ( 'NONE',  ( 0.8554163680231738898, 36.24698750680799009, 29.78861141095913112 ) ) ;
#604 = B_SPLINE_CURVE_WITH_KNOTS ( 'NONE', 3,
 ( #30557, #55279, #7044, #58741, #45007, #54663, #54345, #16471, #25555, #54046, #20559, #59060, #26479, #49364, #2663, #36214, #40928, #59992, #49668 ),
 .UNSPECIFIED., .F., .F.,
 ( 4, 3, 3, 3, 3, 3, 4 ),
 ( 1.301113191146877164E-18, 0.0002612768053151710043, 0.0003919133833142908713, 0.0005225499612322609703, 0.0006531865391693360669, 0.0008112755173415192068, 0.0009693688056799722478 ),
 .UNSPECIFIED. ) ;
#605 = EDGE_CURVE ( 'NONE', #26948, #16981, #11334, .T. ) ;
#606 = CARTESIAN_POINT ( 'NONE',  ( 4.956653778116975495, 9.917440902361160937, 47.05699031914952712 ) ) ;
#607 = ORIENTED_EDGE ( 'NONE', *, *, #39326, .T. ) ;
#608 = CARTESIAN_POINT ( 'NONE',  ( 0.7954196712028469562, -44.76287685048099263, 17.60078400783944019 ) ) ;
#609 = EDGE_CURVE ( 'NONE', #39397, #32445, #6080, .T. ) ;
#610 = CARTESIAN_POINT ( 'NONE',  ( 0.1129192098497447394, -0.9297496242502409913, 44.11448008785053077 ) ) ;
#611 = ORIENTED_EDGE ( 'NONE', *, *, #25395, .F. ) ;
#613 = AXIS2_PLACEMENT_3D ( 'NONE', #47675, #58583, #43615 ) ;
#612 = B_SPLINE_CURVE_WITH_KNOTS ( 'NONE', 3,
 ( #46317, #36930, #27494, #13113, #46024, #8082 ),
 .UNSPECIFIED., .F., .F.,
 ( 4, 2, 4 ),
 ( 8.570390151981194323E-17, 0.0002293366620881429790, 0.0004586733241762002517 ),
 .UNSPECIFIED. ) ;
#614 = CARTESIAN_POINT ( 'NONE',  ( 0.2940133293163011974, 41.60821255532008678, 14.66278273484767780 ) ) ;
#615 = EDGE_LOOP ( 'NONE', ( #60615, #22132, #37483, #15249 ) ) ;
#616 = CARTESIAN_POINT ( 'NONE',  ( 4.975610109902397937, -37.61482235126175766, 31.26618855282478648 ) ) ;
#617 = ORIENTED_EDGE ( 'NONE', *, *, #13578, .F. ) ;
#618 = DIRECTION ( 'NONE',  ( 0.000000000000000000, 0.000000000000000000, 1.000000000000000000 ) ) ;
#619 = CARTESIAN_POINT ( 'NONE',  ( 0.5807400328401574052, 41.20655774452968956, 24.41979442053183647 ) ) ;
#620 = ORIENTED_EDGE ( 'NONE', *, *, #5146, .T. ) ;
#621 = CARTESIAN_POINT ( 'NONE',  ( 0.6001305935487315502, -12.95698906763778524, -46.33281397023059611 ) ) ;
#622 = ORIENTED_EDGE ( 'NONE', *, *, #59993, .F. ) ;
#623 = CARTESIAN_POINT ( 'NONE',  ( 0.5819845079324652559, 0.4540594263153105992, 47.89381220525411464 ) ) ;
#624 =( BOUNDED_SURFACE ( )  B_SPLINE_SURFACE ( 3, 1, ( 
 ( #9004, #37856 ),
 ( #26963, #2518 ),
 ( #41390, #56916 ),
 ( #21644, #47233 ) ),
 .UNSPECIFIED., .F., .F., .F. ) 
 B_SPLINE_SURFACE_WITH_KNOTS ( ( 4, 4 ),
 ( 2, 2 ),
 ( 0.000000000000000000, 1.000000000000000000 ),
 ( 0.000000000000000000, 1.000000000000000000 ),
 .UNSPECIFIED. ) 
 GEOMETRIC_REPRESENTATION_ITEM ( )  RATIONAL_B_SPLINE_SURFACE ( (
 ( 1.000000000000000000, 1.000000000000000000),
 ( 0.9952954269826590483, 0.8620686068821307169),
 ( 0.9952954269826590483, 0.8620686068821307169),
 ( 1.000000000000000000, 1.000000000000000000) ) ) 
 REPRESENTATION_ITEM ( '' )  SURFACE ( )  );
#625 = CARTESIAN_POINT ( 'NONE',  ( 1.088313998177384834, 22.12859469727390760, -36.76812638579207260 ) ) ;
#626 = DIRECTION ( 'NONE',  ( 1.000000000000000000, 0.000000000000000000, 0.000000000000000000 ) ) ;
#627 = EDGE_CURVE ( 'NONE', #10594, #18602, #5314, .T. ) ;
#628 = EDGE_LOOP ( 'NONE', ( #53914, #15394, #25567, #1434 ) ) ;
#629 = CARTESIAN_POINT ( 'NONE',  ( 4.322998006666179727, -8.359821156456151314, -47.25487450103533860 ) ) ;
#630 = CARTESIAN_POINT ( 'NONE',  ( 0.5809828226811617480, 34.25055090842200656, -33.48000389720580472 ) ) ;
#631 = CARTESIAN_POINT ( 'NONE',  ( 0.5786265663353153954, 18.99608782658033590, 43.97352617418621890 ) ) ;
#632 = CARTESIAN_POINT ( 'NONE',  ( 0.8744876279028306332, 27.35388303025845147, -40.76904626731451486 ) ) ;
#633 = ORIENTED_EDGE ( 'NONE', *, *, #26342, .T. ) ;
#634 = EDGE_CURVE ( 'NONE', #39212, #54056, #37548, .T. ) ;
#635 = CARTESIAN_POINT ( 'NONE',  ( 0.5839254288179547281, -33.80331890503245518, -33.93171296845874707 ) ) ;
#636 = CARTESIAN_POINT ( 'NONE',  ( 3.238741278300275805, -38.98370040185414354, -18.12697907494881377 ) ) ;
#637 = ORIENTED_EDGE ( 'NONE', *, *, #3991, .T. ) ;
#638 = CARTESIAN_POINT ( 'NONE',  ( 0.8551540677456715978, -19.17641535420884580, 43.91216198251532887 ) ) ;
#639 = EDGE_CURVE ( 'NONE', #7531, #35778, #49498, .T. ) ;
#640 = ORIENTED_EDGE ( 'NONE', *, *, #39428, .T. ) ;
#641 =( BOUNDED_SURFACE ( )  B_SPLINE_SURFACE ( 3, 1, ( 
 ( #9444, #9142 ),
 ( #28248, #47991 ),
 ( #4720, #28864 ),
 ( #23866, #14478 ) ),
 .UNSPECIFIED., .F., .F., .F. ) 
 B_SPLINE_SURFACE_WITH_KNOTS ( ( 4, 4 ),
 ( 2, 2 ),
 ( 0.000000000000000000, 1.000000000000000000 ),
 ( 0.000000000000000000, 1.000000000000000000 ),
 .UNSPECIFIED. ) 
 GEOMETRIC_REPRESENTATION_ITEM ( )  RATIONAL_B_SPLINE_SURFACE ( (
 ( 1.000000000000000000, 1.000000000000000000),
 ( 0.9732289882329797637, 0.9999525324661233672),
 ( 0.9732289882329797637, 0.9999525324661233672),
 ( 1.000000000000000000, 1.000000000000000000) ) ) 
 REPRESENTATION_ITEM ( '' )  SURFACE ( )  );
#642 = CARTESIAN_POINT ( 'NONE',  ( 0.9745511491811738036, 25.84997388131858997, 34.24777528633291723 ) ) ;
#643 = CARTESIAN_POINT ( 'NONE',  ( 0.1135584504625007929, 24.88873145264492592, 36.43491592982444871 ) ) ;
#644 = ORIENTED_EDGE ( 'NONE', *, *, #34344, .F. ) ;
#645 = CARTESIAN_POINT ( 'NONE',  ( 3.270143674763207553, 9.482922169188102046, -9.870732238228422162 ) ) ;
#646 = CARTESIAN_POINT ( 'NONE',  ( 0.08486401232817714080, 0.000000000000000000, 3.000000000000000000 ) ) ;
#647 = CARTESIAN_POINT ( 'NONE',  ( 0.1129192098497447394, -22.45785791439742241, 37.98152716363431125 ) ) ;
#648 = CARTESIAN_POINT ( 'NONE',  ( 0.1073791018717578927, -40.02496097243069784, 16.05399293000745686 ) ) ;
#649 = VECTOR ( 'NONE', #57815, 1000.000000000000114 ) ;
#650 = AXIS2_PLACEMENT_3D ( 'NONE', #4623, #9354, #47896 ) ;
#651 = ORIENTED_EDGE ( 'NONE', *, *, #50283, .F. ) ;
#652 = CARTESIAN_POINT ( 'NONE',  ( 0.1135584504625008623, -41.05968028581452955, 16.15718747065669447 ) ) ;
#653 = CIRCLE ( 'NONE', #23655, 43.92652462719577500 ) ;
#654 = CARTESIAN_POINT ( 'NONE',  ( 5.917102823773431552, 5.950457534745815735, 19.21150106521946910 ) ) ;
#656 = EDGE_CURVE ( 'NONE', #2290, #7571, #45749, .T. ) ;
#655 = CARTESIAN_POINT ( 'NONE',  ( 5.860006189529234355, 26.78264244998154098, -40.11385274514653787 ) ) ;
#657 = CARTESIAN_POINT ( 'NONE',  ( 5.960221823109900008, -7.859839668735337348, 18.96108896995701798 ) ) ;
#658 = CARTESIAN_POINT ( 'NONE',  ( 0.7048096507298635682, 41.23648859290927504, -24.78213711671556396 ) ) ;
#659 = EDGE_CURVE ( 'NONE', #34606, #4050, #44974, .T. ) ;
#660 = CARTESIAN_POINT ( 'NONE',  ( 4.549368137175248350, 8.166781970325731166, -42.14271863032826104 ) ) ;
#661 = CIRCLE ( 'NONE', #21651, 48.09070567114147110 ) ;
#662 = CARTESIAN_POINT ( 'NONE',  ( -2.700785417809989042, -13.56184546075576769, -3.000000000000003997 ) ) ;
#663 = LINE ( 'NONE', #19802, #9200 ) ;
#664 = CARTESIAN_POINT ( 'NONE',  ( 0.8751705887134423323, -42.09020928323391075, 23.27176129838352736 ) ) ;
#665 = FACE_OUTER_BOUND ( 'NONE', #5662, .T. ) ;
#666 = DIRECTION ( 'NONE',  ( 1.000000000000000000, 0.000000000000000000, 0.000000000000000000 ) ) ;
#667 = CARTESIAN_POINT ( 'NONE',  ( 0.1129192098497455998, 39.54191224844618802, 19.58032082273768637 ) ) ;
#668 = CARTESIAN_POINT ( 'NONE',  ( -6.015611763856276717, 4.882992715191300626, 18.19956619163659894 ) ) ;
#669 = B_SPLINE_CURVE_WITH_KNOTS ( 'NONE', 3,
 ( #10160, #48987, #747, #24568, #6036, #20188, #4813, #39301, #58355, #34590, #53655, #52751, #10786, #33669, #29872, #25174 ),
 .UNSPECIFIED., .F., .F.,
 ( 4, 3, 3, 3, 3, 4 ),
 ( 2.221635811791082109E-17, 0.0002618515315864366642, 0.0003927756766341980997, 0.0005236998216950544205, 0.0007855159896329859956, 0.001047349442285927003 ),
 .UNSPECIFIED. ) ;
#670 = CARTESIAN_POINT ( 'NONE',  ( 0.5809828226811553087, 34.25055090842153760, 33.48000389720628789 ) ) ;
#671 = CARTESIAN_POINT ( 'NONE',  ( 0.6000166863083106206, -48.77118664543515791, 5.761495891223091803 ) ) ;
#672 = ORIENTED_EDGE ( 'NONE', *, *, #404, .F. ) ;
#673 = CARTESIAN_POINT ( 'NONE',  ( 8.000000000000007105, -56.56854249492331377, -56.56854249492430142 ) ) ;
#674 = CARTESIAN_POINT ( 'NONE',  ( 0.9790850452238870627, -1.349767895839444121, 41.88693658995079261 ) ) ;
#675 = CARTESIAN_POINT ( 'NONE',  ( -6.016761891674564211, -9.418621820384613486, 16.32039929810254009 ) ) ;
#676 = ORIENTED_EDGE ( 'NONE', *, *, #35823, .T. ) ;
#677 = EDGE_CURVE ( 'NONE', #34340, #5939, #5995, .T. ) ;
#678 = CARTESIAN_POINT ( 'NONE',  ( 0.6846871229502899947, 47.37786444808403274, -7.109010606686910982 ) ) ;
#679 = CARTESIAN_POINT ( 'NONE',  ( 5.999999999999998224, 6.934333478519240412E-15, 0.000000000000000000 ) ) ;
#680 = EDGE_CURVE ( 'NONE', #47950, #8264, #32312, .T. ) ;
#681 = ORIENTED_EDGE ( 'NONE', *, *, #11907, .F. ) ;
#682 = ORIENTED_EDGE ( 'NONE', *, *, #17053, .F. ) ;
#683 = CARTESIAN_POINT ( 'NONE',  ( 0.6846871229502932144, -13.23224427737861930, 46.04462816497483146 ) ) ;
#684 = CIRCLE ( 'NONE', #45757, 9.499999999999996447 ) ;
#685 = EDGE_CURVE ( 'NONE', #32705, #13041, #48717, .T. ) ;
#686 = ORIENTED_EDGE ( 'NONE', *, *, #27933, .T. ) ;
#687 = EDGE_CURVE ( 'NONE', #54494, #4004, #28518, .T. ) ;
#688 = CARTESIAN_POINT ( 'NONE',  ( 0.9730545539215892381, 25.71816799638828499, -34.34678117142529175 ) ) ;
#689 = AXIS2_PLACEMENT_3D ( 'NONE', #15589, #28433, #47560 ) ;
#690 = ADVANCED_FACE ( 'NONE', ( #22057 ), #36431, .F. ) ;
#691 = ORIENTED_EDGE ( 'NONE', *, *, #39031, .F. ) ;
#692 = ORIENTED_EDGE ( 'NONE', *, *, #16762, .T. ) ;
#693 = CARTESIAN_POINT ( 'NONE',  ( 0.3622758884714730732, -42.84426538328728640, -4.808133778521729518 ) ) ;
#694 = VERTEX_POINT ( 'NONE', #41182 ) ;
#695 = DIRECTION ( 'NONE',  ( -1.000000000000000000, -0.000000000000000000, -0.000000000000000000 ) ) ;
#696 = DIRECTION ( 'NONE',  ( -1.000000000000000000, -1.836909530733580185E-16, 1.836909530733574022E-16 ) ) ;
#697 = CARTESIAN_POINT ( 'NONE',  ( 0.5997462898726536595, 48.29911994996575686, -8.873930482211887849 ) ) ;
#698 = EDGE_LOOP ( 'NONE', ( #12368, #22476, #25732, #52712 ) ) ;
#699 = LINE ( 'NONE', #38957, #41739 ) ;
#700 = EDGE_CURVE ( 'NONE', #45191, #45197, #17329, .T. ) ;
#701 = CARTESIAN_POINT ( 'NONE',  ( 5.910764540655178756, -9.651974367318080894, 17.64484710281723068 ) ) ;
#702 = EDGE_LOOP ( 'NONE', ( #10491, #19240, #32643, #32157 ) ) ;
#703 = CIRCLE ( 'NONE', #14728, 15.38217999999999996 ) ;
#704 = ORIENTED_EDGE ( 'NONE', *, *, #30101, .T. ) ;
#705 = CARTESIAN_POINT ( 'NONE',  ( -6.079354080745853928, -16.13884862108074003, -10.50383360654586795 ) ) ;
#706 = CARTESIAN_POINT ( 'NONE',  ( 4.956445790444022670, -4.175462451061590308, -46.90526157542895191 ) ) ;
#707 = DIRECTION ( 'NONE',  ( 0.000000000000000000, 0.000000000000000000, 1.000000000000000000 ) ) ;
#708 = CARTESIAN_POINT ( 'NONE',  ( 4.963659409799330291, 14.83726297270336580, -42.22332985082294243 ) ) ;
#709 = CARTESIAN_POINT ( 'NONE',  ( 4.691466044806102076, 19.42108863068321511, 40.13652286047901185 ) ) ;
#710 = EDGE_LOOP ( 'NONE', ( #19478, #17460, #53566, #59552 ) ) ;
#711 = CARTESIAN_POINT ( 'NONE',  ( 0.6025881611877911270, -12.66175293297434656, 46.41131722377287616 ) ) ;
#712 = CARTESIAN_POINT ( 'NONE',  ( 2.643462169533600914, 1.382267876918459315, -48.01657676222235693 ) ) ;
#713 = CARTESIAN_POINT ( 'NONE',  ( 5.838029081930957709, -22.71741985886527715, -41.41236401256216482 ) ) ;
#714 = CARTESIAN_POINT ( 'NONE',  ( -6.078726893082806448, 9.985094725776210822, 16.46486940689163703 ) ) ;
#715 = VERTEX_POINT ( 'NONE', #55863 ) ;
#716 = CARTESIAN_POINT ( 'NONE',  ( 0.7762783648524382851, -38.54028518467400488, -28.45155609988369250 ) ) ;
#717 = CARTESIAN_POINT ( 'NONE',  ( 0.1152809850208375564, 37.10017609937931127, -23.88560687704625352 ) ) ;
#718 = LINE ( 'NONE', #58032, #49664 ) ;
#719 = CARTESIAN_POINT ( 'NONE',  ( 1.834102595619085507, -5.740732742422371082, 43.67197880148968636 ) ) ;
#720 = AXIS2_PLACEMENT_3D ( 'NONE', #46539, #27411, #3586 ) ;
#721 = ORIENTED_EDGE ( 'NONE', *, *, #32659, .F. ) ;
#722 = VERTEX_POINT ( 'NONE', #26431 ) ;
#723 = DIRECTION ( 'NONE',  ( 1.000000000000000000, 0.000000000000000000, 0.000000000000000000 ) ) ;
#724 = CARTESIAN_POINT ( 'NONE',  ( -2.569797478183783568, 2.353985772484557426, 14.44232325624827595 ) ) ;
#725 = CARTESIAN_POINT ( 'NONE',  ( 1.830465331921977024, -42.27910384509804231, -12.36339087523346336 ) ) ;
#727 = ADVANCED_FACE ( 'NONE', ( #41490 ), #47217, .F. ) ;
#726 = CARTESIAN_POINT ( 'NONE',  ( 4.834790513006555379, -47.12142688710419947, 3.487186408506746105 ) ) ;
#728 = B_SPLINE_CURVE_WITH_KNOTS ( 'NONE', 3,
 ( #16941, #36055, #21315, #30385 ),
 .UNSPECIFIED., .F., .F.,
 ( 4, 4 ),
 ( 0.000000000000000000, 0.005014147105413705591 ),
 .UNSPECIFIED. ) ;
#729 = CARTESIAN_POINT ( 'NONE',  ( 4.975801465491695552, -14.85979367497206205, 45.55012473237727733 ) ) ;
#730 = DIRECTION ( 'NONE',  ( 0.000000000000000000, 0.000000000000000000, 1.000000000000000000 ) ) ;
#731 = CARTESIAN_POINT ( 'NONE',  ( 0.5800708057587392608, 0.6275304576137059609, -47.89175345272231255 ) ) ;
#732 = EDGE_CURVE ( 'NONE', #32675, #50174, #22, .T. ) ;
#733 = CARTESIAN_POINT ( 'NONE',  ( 3.238741278300276694, 31.66556122967958231, -29.07934833201334968 ) ) ;
#734 = CARTESIAN_POINT ( 'NONE',  ( 5.894904586330512508, 12.98639672351314189, 15.35848013968732140 ) ) ;
#735 = CIRCLE ( 'NONE', #51752, 2.649999999999997691 ) ;
#736 = CARTESIAN_POINT ( 'NONE',  ( -6.015611763856276717, -13.32857883366842700, 13.31979030221794424 ) ) ;
#737 = B_SPLINE_CURVE_WITH_KNOTS ( 'NONE', 3,
 ( #57303, #14440, #48863, #33549 ),
 .UNSPECIFIED., .F., .F.,
 ( 4, 4 ),
 ( 0.000000000000000000, 0.005013413432710154584 ),
 .UNSPECIFIED. ) ;
#738 = CARTESIAN_POINT ( 'NONE',  ( 0.1119898979215350476, 39.99500470998355439, 18.63762073066790492 ) ) ;
#739 = EDGE_LOOP ( 'NONE', ( #30578, #30226 ) ) ;
#740 = AXIS2_PLACEMENT_3D ( 'NONE', #47734, #42736, #43357 ) ;
#741 = AXIS2_PLACEMENT_3D ( 'NONE', #15685, #34479, #34171 ) ;
#742 = CARTESIAN_POINT ( 'NONE',  ( 3.238741278300273585, -19.89284324544667015, -38.11287256318055228 ) ) ;
#743 = CARTESIAN_POINT ( 'NONE',  ( 0.1102144999581333162, -34.13606714958032740, -26.35238362727828232 ) ) ;
#744 = PRODUCT_DEFINITION ( 'UNKNOWN', '', #56876, #15421 ) ;
#745 = FACE_OUTER_BOUND ( 'NONE', #14666, .T. ) ;
#746 = CARTESIAN_POINT ( 'NONE',  ( 0.1129192098497455998, -27.13044910148877165, -34.79785222304216319 ) ) ;
#747 = CARTESIAN_POINT ( 'NONE',  ( 0.6017667736363749853, -24.35549005323445471, 41.48674115080360281 ) ) ;
#748 = CARTESIAN_POINT ( 'NONE',  ( 0.6016117650947691020, 32.75634116857341382, -36.58651619780874853 ) ) ;
#749 = CARTESIAN_POINT ( 'NONE',  ( -31.74999999999995737, 0.000000000000000000, 0.000000000000000000 ) ) ;
#750 = CONTEXT_DEPENDENT_SHAPE_REPRESENTATION ( #29569, #305 ) ;
#751 = FACE_OUTER_BOUND ( 'NONE', #41449, .T. ) ;
#752 = CARTESIAN_POINT ( 'NONE',  ( 0.6029443449137434907, 22.75264314188179782, -43.51846467927736484 ) ) ;
#753 =( REPRESENTATION_RELATIONSHIP ('NONE','NONE', #44881, #19619 ) REPRESENTATION_RELATIONSHIP_WITH_TRANSFORMATION ( #37456 )SHAPE_REPRESENTATION_RELATIONSHIP( ) );
#754 =( BOUNDED_SURFACE ( )  B_SPLINE_SURFACE ( 3, 1, ( 
 ( #48930, #29199 ),
 ( #58298, #43641 ),
 ( #5979, #683 ),
 ( #20739, #25738 ) ),
 .UNSPECIFIED., .F., .F., .F. ) 
 B_SPLINE_SURFACE_WITH_KNOTS ( ( 4, 4 ),
 ( 2, 2 ),
 ( 0.000000000000000000, 1.000000000000000000 ),
 ( 0.000000000000000000, 1.000000000000000000 ),
 .UNSPECIFIED. ) 
 GEOMETRIC_REPRESENTATION_ITEM ( )  RATIONAL_B_SPLINE_SURFACE ( (
 ( 1.000000000000000000, 1.000000000000000000),
 ( 0.9953390228620291325, 0.8624445117761032620),
 ( 0.9953390228620291325, 0.8624445117761032620),
 ( 1.000000000000000000, 1.000000000000000000) ) ) 
 REPRESENTATION_ITEM ( '' )  SURFACE ( )  );
#755 = CARTESIAN_POINT ( 'NONE',  ( 0.9730545539215892381, -11.59290486963536360, 41.31259007387227911 ) ) ;
#756 = CARTESIAN_POINT ( 'NONE',  ( 3.238931869106853600, -23.06038324659541772, -36.28407486357512823 ) ) ;
#757 = CARTESIAN_POINT ( 'NONE',  ( 0.8753041380234465318, -8.714053517584193997, 48.32394436680080219 ) ) ;
#759 = VERTEX_POINT ( 'NONE', #26750 ) ;
#758 = CARTESIAN_POINT ( 'NONE',  ( 0.8751705887134423323, -23.27176129838396790, -42.09020928323367627 ) ) ;
#760 = ORIENTED_EDGE ( 'NONE', *, *, #60258, .F. ) ;
#761 = DIRECTION ( 'NONE',  ( -1.000000000000000000, -0.000000000000000000, -0.000000000000000000 ) ) ;
#762 = CARTESIAN_POINT ( 'NONE',  ( 2.359973842542475886, 43.81130819181431946, -4.324947300761510682 ) ) ;
#763 = CARTESIAN_POINT ( 'NONE',  ( 0.3622758884714600280, 15.73321244754796666, 40.13994584881788086 ) ) ;
#764 = ORIENTED_EDGE ( 'NONE', *, *, #45036, .T. ) ;
#765 = CARTESIAN_POINT ( 'NONE',  ( 1.227938101723748288, 39.96870412324358313, -15.63977281655798812 ) ) ;
#766 = CARTESIAN_POINT ( 'NONE',  ( 0.5824935313925968527, -45.88237815356815474, 9.697708596715390428 ) ) ;
#767 = CARTESIAN_POINT ( 'NONE',  ( 0.5839879327111929808, -41.52454255611490197, -23.86931774877339762 ) ) ;
#768 = B_SPLINE_CURVE_WITH_KNOTS ( 'NONE', 3,
 ( #39427, #58479, #39121, #52877, #25605, #20305 ),
 .UNSPECIFIED., .F., .F.,
 ( 4, 2, 4 ),
 ( 8.652891131202922673E-17, 0.0002293366620881455539, 0.0004586733241762045886 ),
 .UNSPECIFIED. ) ;
#769 = VECTOR ( 'NONE', #19028, 1000.000000000000114 ) ;
#770 = EDGE_CURVE ( 'NONE', #27059, #18903, #60242, .T. ) ;
#771 = ORIENTED_EDGE ( 'NONE', *, *, #4210, .F. ) ;
#772 = ORIENTED_EDGE ( 'NONE', *, *, #60310, .T. ) ;
#773 = CARTESIAN_POINT ( 'NONE',  ( 5.901764892641288895, 47.37867283933450580, 12.37953260115202525 ) ) ;
#774 = EDGE_CURVE ( 'NONE', #35221, #43756, #59136, .T. ) ;
#775 = CIRCLE ( 'NONE', #19798, 5.612499999999999822 ) ;
#776 = ADVANCED_FACE ( 'NONE', ( #3231 ), #27365, .T. ) ;
#777 = CARTESIAN_POINT ( 'NONE',  ( -4.000000000000000000, -0.3902508023145539462, 2.371692252312039717E-17 ) ) ;
#778 = CARTESIAN_POINT ( 'NONE',  ( -6.079354080745853928, -12.94667982361303160, 14.25399722158711846 ) ) ;
#779 = CARTESIAN_POINT ( 'NONE',  ( 0.5806925824938499181, 46.89268439822727430, -0.5463627657667492477 ) ) ;
#780 = ADVANCED_FACE ( 'NONE', ( #41804 ), #54611, .F. ) ;
#781 = CARTESIAN_POINT ( 'NONE',  ( 0.9762797500689124330, -40.96497924994810091, -8.842808390835211085 ) ) ;
#782 = CARTESIAN_POINT ( 'NONE',  ( 0.8751705887134423323, -17.57879340691512837, -44.76769609654229498 ) ) ;
#783 = CARTESIAN_POINT ( 'NONE',  ( 0.8551540677456715978, -7.157691013574052796, -47.37911285756627677 ) ) ;
#784 = ORIENTED_EDGE ( 'NONE', *, *, #20649, .F. ) ;
#785 = ORIENTED_EDGE ( 'NONE', *, *, #4685, .F. ) ;
#786 = CARTESIAN_POINT ( 'NONE',  ( 0.1365634738349390531, 43.42681589074051374, -7.808603025828129596 ) ) ;
#787 = CARTESIAN_POINT ( 'NONE',  ( 1.227938101723748288, 42.43379953535185933, 6.439911493064710335 ) ) ;
#788 = VECTOR ( 'NONE', #13466, 1000.000000000000114 ) ;
#789 = VERTEX_POINT ( 'NONE', #46810 ) ;
#790 = LINE ( 'NONE', #58093, #17538 ) ;
#791 = CARTESIAN_POINT ( 'NONE',  ( 0.5797568665920712627, -0.9380854118316781509, 46.88651516547137987 ) ) ;
#792 = CARTESIAN_POINT ( 'NONE',  ( 5.283180000000047727, 0.000000000000000000, 15.43999999999999240 ) ) ;
#793 = CARTESIAN_POINT ( 'NONE',  ( 0.3676999524040366896, 40.09552319080398775, 18.39292264373822405 ) ) ;
#794 = B_SPLINE_CURVE_WITH_KNOTS ( 'NONE', 3,
 ( #8782, #27896, #8163, #37018, #46401, #3447 ),
 .UNSPECIFIED., .F., .F.,
 ( 4, 2, 4 ),
 ( 1.051843754078492886E-17, 0.0002448709889506574819, 0.0004897419779013044471 ),
 .UNSPECIFIED. ) ;
#795 = ORIENTED_EDGE ( 'NONE', *, *, #6044, .T. ) ;
#796 = FACE_OUTER_BOUND ( 'NONE', #9055, .T. ) ;
#797 = CARTESIAN_POINT ( 'NONE',  ( -6.016761891674564211, 17.41015286184802946, 7.207804629151374876 ) ) ;
#798 = CARTESIAN_POINT ( 'NONE',  ( 1.231276596079881047, 40.19859528295886975, 11.88905834349143653 ) ) ;
#799 = B_SPLINE_CURVE_WITH_KNOTS ( 'NONE', 3,
 ( #60694, #8701, #46635, #55683, #55382, #31593, #46951, #46327, #41627, #56004, #3986, #7773, #50681, #27507, #3073, #22200, #59050, #36206, #45602, #2653, #59358, #21785, #6716, #30545, #45301 ),
 .UNSPECIFIED., .F., .F.,
 ( 4, 3, 3, 3, 3, 3, 3, 3, 4 ),
 ( 3.469446951953613804E-18, 0.0005656085177311393148, 0.001131215744874498972, 0.001696821861372763965, 0.002262427090022496850, 0.002828031679238744624, 0.003393635864401604429, 0.003977030878808129888, 0.004561030005651157265 ),
 .UNSPECIFIED. ) ;
#800 = CARTESIAN_POINT ( 'NONE',  ( 0.5827359174754832560, 28.86822142608449226, 38.21848266111678782 ) ) ;
#801 = ORIENTED_EDGE ( 'NONE', *, *, #43455, .F. ) ;
#802 = CARTESIAN_POINT ( 'NONE',  ( 0.6021448801613057400, 4.975419407533241412, -48.85474736753931069 ) ) ;
#803 = ORIENTED_EDGE ( 'NONE', *, *, #32383, .T. ) ;
#804 = DIRECTION ( 'NONE',  ( -1.000000000000000000, 0.000000000000000000, -0.000000000000000000 ) ) ;
#805 = CARTESIAN_POINT ( 'NONE',  ( 2.624215991343608501, -43.79392271049056262, -19.66774719433024998 ) ) ;
#806 = TOROIDAL_SURFACE ( 'NONE', #38851, 7.400000000000022560, 0.09999999999999961697 ) ;
#807 = ORIENTED_EDGE ( 'NONE', *, *, #18327, .F. ) ;
#808 = CARTESIAN_POINT ( 'NONE',  ( 0.3622758884714730732, -25.58609868863794290, 34.70015533914785522 ) ) ;
#809 = CARTESIAN_POINT ( 'NONE',  ( 0.9757402383260950218, 26.18833306844200237, -33.98983788393794470 ) ) ;
#810 = FACE_OUTER_BOUND ( 'NONE', #7730, .T. ) ;
#811 = CARTESIAN_POINT ( 'NONE',  ( 0.1155031312995260795, 33.70714732405365766, -28.47402064700997926 ) ) ;
#813 = DIRECTION ( 'NONE',  ( 0.000000000000000000, 0.000000000000000000, -1.000000000000000000 ) ) ;
#812 =( GEOMETRIC_REPRESENTATION_CONTEXT ( 3 ) GLOBAL_UNCERTAINTY_ASSIGNED_CONTEXT ( ( #24190 ) ) GLOBAL_UNIT_ASSIGNED_CONTEXT ( ( #51284, #41927, #36297 ) ) REPRESENTATION_CONTEXT ( 'NONE', 'WORKASPACE' ) );
#814 = CARTESIAN_POINT ( 'NONE',  ( 0.6031356755773454870, 29.28593560184431510, -38.16621646312178484 ) ) ;
#815 = EDGE_CURVE ( 'NONE', #12977, #53425, #47107, .T. ) ;
#816 = DIRECTION ( 'NONE',  ( 0.000000000000000000, 0.7071067811865527908, -0.7071067811865421326 ) ) ;
#817 = VERTEX_POINT ( 'NONE', #56170 ) ;
#818 = CARTESIAN_POINT ( 'NONE',  ( 0.5819845901640506858, -24.34012668949516112, 41.25023214430193264 ) ) ;
#819 = MECHANICAL_DESIGN_GEOMETRIC_PRESENTATION_REPRESENTATION (  '', ( #60818 ), #10854 ) ;
#820 = CARTESIAN_POINT ( 'NONE',  ( 4.553261556744875094, 0.000000000000000000, 0.000000000000000000 ) ) ;
#821 = CARTESIAN_POINT ( 'NONE',  ( 4.553261556744875094, -15.38244134641827898, 41.14510984366961566 ) ) ;
#822 = ORIENTED_EDGE ( 'NONE', *, *, #2768, .T. ) ;
#823 = CARTESIAN_POINT ( 'NONE',  ( 0.5998501479064708430, -0.5236536531318284338, 48.10473956285918717 ) ) ;
#824 = CARTESIAN_POINT ( 'NONE',  ( 4.834790513006555379, 41.39428925248022040, 22.78381351324621917 ) ) ;
#825 = DIRECTION ( 'NONE',  ( -1.655270492344282294E-16, 1.000000000000000000, 0.000000000000000000 ) ) ;
#826 = CARTESIAN_POINT ( 'NONE',  ( 5.981074661064941900, 2.687517936919725958, 20.34795181394749619 ) ) ;
#827 = CARTESIAN_POINT ( 'NONE',  ( 0.9762797500689124330, -26.66896101499549587, -32.32787193067855469 ) ) ;
#828 = CARTESIAN_POINT ( 'NONE',  ( 0.1073791018717483448, -0.4849339620930353534, -43.12183934961191056 ) ) ;
#829 = DIRECTION ( 'NONE',  ( 7.166653630759624877E-15, -1.000000000000000000, -1.047444401652939849E-14 ) ) ;
#830 = CARTESIAN_POINT ( 'NONE',  ( 4.833616638992208614, -30.83411269743540473, -34.47248434257901550 ) ) ;
#831 =( BOUNDED_SURFACE ( )  B_SPLINE_SURFACE ( 3, 1, ( 
 ( #41675, #17861 ),
 ( #21625, #46373 ),
 ( #50730, #27252 ),
 ( #60738, #2807 ) ),
 .UNSPECIFIED., .F., .F., .F. ) 
 B_SPLINE_SURFACE_WITH_KNOTS ( ( 4, 4 ),
 ( 2, 2 ),
 ( 0.000000000000000000, 1.000000000000000000 ),
 ( 0.000000000000000000, 1.000000000000000000 ),
 .UNSPECIFIED. ) 
 GEOMETRIC_REPRESENTATION_ITEM ( )  RATIONAL_B_SPLINE_SURFACE ( (
 ( 1.000000000000000000, 1.000000000000000000),
 ( 0.9729067724841187204, 0.9999501103223794596),
 ( 0.9729067724841187204, 0.9999501103223794596),
 ( 1.000000000000000000, 1.000000000000000000) ) ) 
 REPRESENTATION_ITEM ( '' )  SURFACE ( )  );
#832 = CARTESIAN_POINT ( 'NONE',  ( 0.9789889208857702751, -6.875788487547667138, 41.34075991944121142 ) ) ;
#833 = AXIS2_PLACEMENT_3D ( 'NONE', #52167, #23673, #42803 ) ;
#834 = CARTESIAN_POINT ( 'NONE',  ( 0.9762797500689124330, 28.76866969768027715, -30.47438972336406238 ) ) ;
#836 = ORIENTED_EDGE ( 'NONE', *, *, #601, .T. ) ;
#835 = CARTESIAN_POINT ( 'NONE',  ( 4.958415959904818315, -35.95869674887519807, -27.75204644607441296 ) ) ;
#837 = ORIENTED_EDGE ( 'NONE', *, *, #10998, .T. ) ;
#838 = FACE_OUTER_BOUND ( 'NONE', #41555, .T. ) ;
#839 = VECTOR ( 'NONE', #31657, 1000.000000000000227 ) ;
#840 = FACE_OUTER_BOUND ( 'NONE', #26080, .T. ) ;
#841 = CARTESIAN_POINT ( 'NONE',  ( 0.08486401232817714080, 0.000000000000000000, 0.000000000000000000 ) ) ;
#842 = CARTESIAN_POINT ( 'NONE',  ( 4.691466044806102076, 25.04870410140789261, -36.88741755356043228 ) ) ;
#843 = CARTESIAN_POINT ( 'NONE',  ( 1.088313998177379949, 30.89087247895970734, -29.78798111128795512 ) ) ;
#844 = EDGE_CURVE ( 'NONE', #61266, #41784, #57084, .T. ) ;
#845 = ORIENTED_EDGE ( 'NONE', *, *, #3724, .T. ) ;
#846 = EDGE_CURVE ( 'NONE', #28462, #53243, #29302, .T. ) ;
#847 = CARTESIAN_POINT ( 'NONE',  ( 0.5797568665920715958, -38.30338252035704016, 27.05690662476175490 ) ) ;
#848 = CARTESIAN_POINT ( 'NONE',  ( -20.00652009675311405, -7.982586356554360663, 0.5445903824078870414 ) ) ;
#849 = CARTESIAN_POINT ( 'NONE',  ( 3.345653888883671545, -2.687187980154741140, -5.460849780464844372 ) ) ;
#850 = EDGE_LOOP ( 'NONE', ( #20238, #49927, #25803, #15835 ) ) ;
#851 = EDGE_CURVE ( 'NONE', #38431, #10608, #42121, .T. ) ;
#852 = B_SPLINE_CURVE_WITH_KNOTS ( 'NONE', 3,
 ( #40262, #11737, #26126, #30819 ),
 .UNSPECIFIED., .F., .F.,
 ( 4, 4 ),
 ( 2.204559228842524708E-17, 0.004444306975806115896 ),
 .UNSPECIFIED. ) ;
#853 = CARTESIAN_POINT ( 'NONE',  ( 0.8551540677456834771, 29.88829867897813841, 37.45266983663506721 ) ) ;
#854 = CARTESIAN_POINT ( 'NONE',  ( 0.5827359174754830340, 47.53228759166454864, -5.891371786504479680 ) ) ;
#855 = VERTEX_POINT ( 'NONE', #32699 ) ;
#856 = AXIS2_PLACEMENT_3D ( 'NONE', #6728, #16176, #30560 ) ;
#857 = CARTESIAN_POINT ( 'NONE',  ( 0.8557997880470599172, -44.60232077416698360, 17.48760788519201981 ) ) ;
#858 = ORIENTED_EDGE ( 'NONE', *, *, #44639, .F. ) ;
#859 = DIRECTION ( 'NONE',  ( -0.1024043820194934368, -0.2701391291102854253, 0.9573600124648732335 ) ) ;
#860 = EDGE_CURVE ( 'NONE', #44643, #7607, #39105, .T. ) ;
#861 = CARTESIAN_POINT ( 'NONE',  ( 0.5980894510889457338, -46.65000524237077428, -11.77356634613301445 ) ) ;
#862 = ORIENTED_EDGE ( 'NONE', *, *, #14237, .T. ) ;
#863 = CARTESIAN_POINT ( 'NONE',  ( 5.917102823773431552, 19.00193826451960888, 6.589086449814391955 ) ) ;
#864 = CARTESIAN_POINT ( 'NONE',  ( 5.894904586330512508, -4.661384928609073164, 19.56529842882492076 ) ) ;
#865 = DIRECTION ( 'NONE',  ( 0.07836865515943411409, -0.5052769534812810992, 0.8593913859058496252 ) ) ;
#866 = LINE ( 'NONE', #10586, #42418 ) ;
#867 = EDGE_CURVE ( 'NONE', #47641, #16356, #52484, .T. ) ;
#868 = VERTEX_POINT ( 'NONE', #13911 ) ;
#869 = CARTESIAN_POINT ( 'NONE',  ( 5.896782393890504181, 14.91246379622012874, 13.49609241241464375 ) ) ;
#870 = CARTESIAN_POINT ( 'NONE',  ( 0.6031356219577719280, -0.08729769678277263245, -48.10744328000515679 ) ) ;
#871 = ORIENTED_EDGE ( 'NONE', *, *, #55780, .T. ) ;
#872 = CARTESIAN_POINT ( 'NONE',  ( 3.238018933889920792, -13.17791601574921145, 2.397920317590518824 ) ) ;
#873 = VERTEX_POINT ( 'NONE', #13279 ) ;
#874 = FACE_OUTER_BOUND ( 'NONE', #59056, .T. ) ;
#875 = ORIENTED_EDGE ( 'NONE', *, *, #14039, .T. ) ;
#876 = CARTESIAN_POINT ( 'NONE',  ( 0.8560838555295223751, -46.85553835019177882, -2.220666565569921591 ) ) ;
#877 = CARTESIAN_POINT ( 'NONE',  ( 4.975610109902397937, 39.54077024310134902, 28.79195887257488451 ) ) ;
#878 = AXIS2_PLACEMENT_3D ( 'NONE', #55529, #46473, #8857 ) ;
#879 = VECTOR ( 'NONE', #23921, 1000.000000000000227 ) ;
#880 = DIRECTION ( 'NONE',  ( -0.1011922191286467598, 0.7056551247449875941, 0.7012923639317314439 ) ) ;
#881 = ORIENTED_EDGE ( 'NONE', *, *, #47421, .F. ) ;
#882 = CARTESIAN_POINT ( 'NONE',  ( 0.5836750258453345941, 6.071582023534265460, 47.50958153310754284 ) ) ;
#883 = CARTESIAN_POINT ( 'NONE',  ( 0.5838002273316434954, -6.386683873060837513, 47.46823345111867809 ) ) ;
#884 = VERTEX_POINT ( 'NONE', #47714 ) ;
#885 = VERTEX_POINT ( 'NONE', #22990 ) ;
#886 = FACE_OUTER_BOUND ( 'NONE', #43567, .T. ) ;
#887 = CARTESIAN_POINT ( 'NONE',  ( -6.078726893082806448, 7.797636468844645563, 17.60655862934219584 ) ) ;
#888 = DIRECTION ( 'NONE',  ( -1.000000000000000000, -0.000000000000000000, -0.000000000000000000 ) ) ;
#889 = EDGE_CURVE ( 'NONE', #22076, #50810, #31522, .T. ) ;
#890 = CARTESIAN_POINT ( 'NONE',  ( 0.7948878604505672518, -13.13616273002648072, 47.30898303735433075 ) ) ;
#891 = CARTESIAN_POINT ( 'NONE',  ( 0.8744876279028263033, -45.83369275826233036, 17.59609782084381280 ) ) ;
#892 = ORIENTED_EDGE ( 'NONE', *, *, #60788, .T. ) ;
#893 = CARTESIAN_POINT ( 'NONE',  ( 0.9762797500689124330, -40.96497924994810091, -8.842808390835211085 ) ) ;
#894 = CIRCLE ( 'NONE', #35930, 43.08621763946400307 ) ;
#895 = ORIENTED_EDGE ( 'NONE', *, *, #36444, .F. ) ;
#896 = CARTESIAN_POINT ( 'NONE',  ( 0.6030672727741701600, 12.36682345648116410, 46.49075153683476458 ) ) ;
#897 = DIRECTION ( 'NONE',  ( 0.000000000000000000, 0.000000000000000000, 1.000000000000000000 ) ) ;
#898 = CARTESIAN_POINT ( 'NONE',  ( 2.643462169533600914, 43.83256147628706145, 19.65219740572204543 ) ) ;
#899 = CARTESIAN_POINT ( 'NONE',  ( 5.960721111146673579, -2.685391721746187343, 20.34914600876570390 ) ) ;
#900 = CARTESIAN_POINT ( 'NONE',  ( 0.5980271706414711508, -48.61493274831085643, -6.974063142736467213 ) ) ;
#901 = CARTESIAN_POINT ( 'NONE',  ( 2.624215991343608501, 46.71702075422666667, -11.05657803850996856 ) ) ;
#902 = ORIENTED_EDGE ( 'NONE', *, *, #5659, .F. ) ;
#903 = CARTESIAN_POINT ( 'NONE',  ( 4.549368137175248350, -42.84816078363928682, 2.596185425821780246 ) ) ;
#904 = CARTESIAN_POINT ( 'NONE',  ( 3.238931869106854489, 23.06038324659516903, 36.28407486357528455 ) ) ;
#905 =( BOUNDED_SURFACE ( )  B_SPLINE_SURFACE ( 3, 1, ( 
 ( #19570, #11393 ),
 ( #26404, #54580 ),
 ( #11093, #22031 ),
 ( #30476, #49590 ) ),
 .UNSPECIFIED., .F., .F., .F. ) 
 B_SPLINE_SURFACE_WITH_KNOTS ( ( 4, 4 ),
 ( 2, 2 ),
 ( 0.000000000000000000, 1.000000000000000000 ),
 ( 0.000000000000000000, 1.000000000000000000 ),
 .UNSPECIFIED. ) 
 GEOMETRIC_REPRESENTATION_ITEM ( )  RATIONAL_B_SPLINE_SURFACE ( (
 ( 1.000000000000000000, 1.000000000000000000),
 ( 0.9953390228620291325, 0.8624445117760984880),
 ( 0.9953390228620291325, 0.8624445117760984880),
 ( 1.000000000000000000, 1.000000000000000000) ) ) 
 REPRESENTATION_ITEM ( '' )  SURFACE ( )  );
#906 = CARTESIAN_POINT ( 'NONE',  ( 0.8753041380234471980, -6.957149426673730375, -48.60798699522449340 ) ) ;
#907 = CARTESIAN_POINT ( 'NONE',  ( -6.016104459813374383, -18.20253432612970457, 4.871830707672994087 ) ) ;
#908 = CARTESIAN_POINT ( 'NONE',  ( 1.000110580585051201, -41.76694666412394241, -3.455379737181916600 ) ) ;
#909 = CARTESIAN_POINT ( 'NONE',  ( 3.407937589446174087, -5.663729899985161076, 12.47329436636627165 ) ) ;
#910 = LINE ( 'NONE', #10019, #48650 ) ;
#911 = B_SPLINE_CURVE_WITH_KNOTS ( 'NONE', 3,
 ( #35772, #40794, #49848, #40176, #59541, #54839 ),
 .UNSPECIFIED., .F., .F.,
 ( 4, 2, 4 ),
 ( 2.818925648462311528E-18, 0.0002447193893791703044, 0.0004894387787583377898 ),
 .UNSPECIFIED. ) ;
#912 = ORIENTED_EDGE ( 'NONE', *, *, #39913, .F. ) ;
#913 = ADVANCED_FACE ( 'NONE', ( #18291 ), #53578, .F. ) ;
#914 =( BOUNDED_SURFACE ( )  B_SPLINE_SURFACE ( 3, 1, ( 
 ( #11593, #53245 ),
 ( #5309, #59175 ),
 ( #30365, #48259 ),
 ( #34166, #619 ) ),
 .UNSPECIFIED., .F., .F., .F. ) 
 B_SPLINE_SURFACE_WITH_KNOTS ( ( 4, 4 ),
 ( 2, 2 ),
 ( 0.000000000000000000, 1.000000000000000000 ),
 ( 0.000000000000000000, 1.000000000000000000 ),
 .UNSPECIFIED. ) 
 GEOMETRIC_REPRESENTATION_ITEM ( )  RATIONAL_B_SPLINE_SURFACE ( (
 ( 1.000000000000000000, 1.000000000000000000),
 ( 0.9732289882329797637, 0.9999525324661233672),
 ( 0.9732289882329797637, 0.9999525324661233672),
 ( 1.000000000000000000, 1.000000000000000000) ) ) 
 REPRESENTATION_ITEM ( '' )  SURFACE ( )  );
#915 = AXIS2_PLACEMENT_3D ( 'NONE', #38595, #48285, #43928 ) ;
#916 = CARTESIAN_POINT ( 'NONE',  ( 1.830465331921977468, -40.35099765304325814, -17.66841940532562560 ) ) ;
#917 = CARTESIAN_POINT ( 'NONE',  ( 0.6026777506516367566, -47.54531535096658246, -12.28777354993009396 ) ) ;
#918 = DIRECTION ( 'NONE',  ( 0.000000000000000000, 0.000000000000000000, 1.000000000000000000 ) ) ;
#919 = FACE_OUTER_BOUND ( 'NONE', #8044, .T. ) ;
#920 = ORIENTED_EDGE ( 'NONE', *, *, #19893, .T. ) ;
#921 = ADVANCED_FACE ( 'NONE', ( #33014, #18595 ), #48023, .F. ) ;
#922 =( BOUNDED_SURFACE ( )  B_SPLINE_SURFACE ( 3, 1, ( 
 ( #61204, #61807 ),
 ( #57111, #27707 ),
 ( #4791, #22697 ),
 ( #32725, #8581 ) ),
 .UNSPECIFIED., .F., .F., .F. ) 
 B_SPLINE_SURFACE_WITH_KNOTS ( ( 4, 4 ),
 ( 2, 2 ),
 ( 0.000000000000000000, 1.000000000000000000 ),
 ( 0.000000000000000000, 1.000000000000000000 ),
 .UNSPECIFIED. ) 
 GEOMETRIC_REPRESENTATION_ITEM ( )  RATIONAL_B_SPLINE_SURFACE ( (
 ( 1.000000000000000000, 1.000000000000000000),
 ( 0.9953390228620291325, 0.8624445117761032620),
 ( 0.9953390228620291325, 0.8624445117761032620),
 ( 1.000000000000000000, 1.000000000000000000) ) ) 
 REPRESENTATION_ITEM ( '' )  SURFACE ( )  );
#923 = CARTESIAN_POINT ( 'NONE',  ( 0.5997462898726536595, 32.62638226927682439, 36.70246327105753892 ) ) ;
#924 = DIRECTION ( 'NONE',  ( -1.000000000000000000, -0.000000000000000000, -0.000000000000000000 ) ) ;
#925 = B_SPLINE_CURVE_WITH_KNOTS ( 'NONE', 3,
 ( #18539, #13233, #27317, #46445, #18240, #32336 ),
 .UNSPECIFIED., .F., .F.,
 ( 4, 2, 4 ),
 ( 3.529906531158615134E-18, 0.0002445244328975386492, 0.0004890488657950738290 ),
 .UNSPECIFIED. ) ;
#926 = ADVANCED_FACE ( 'NONE', ( #57380 ), #4353, .F. ) ;
#927 = B_SPLINE_CURVE_WITH_KNOTS ( 'NONE', 3,
 ( #45392, #7755, #22796, #26879, #21564, #16557, #54745, #41611, #26252, #36605, #11883, #30962, #40699, #59768, #12486, #35995, #31270, #7436, #26567 ),
 .UNSPECIFIED., .F., .F.,
 ( 4, 3, 3, 3, 3, 3, 4 ),
 ( 0.000000000000000000, 0.0002612768053151720343, 0.0003919133833142897328, 0.0005225499612322591272, 0.0006531865391693329227, 0.0008112755173415183395, 0.0009693688056799717057 ),
 .UNSPECIFIED. ) ;
#928 = CARTESIAN_POINT ( 'NONE',  ( 1.000110580585050091, 38.32249311736364916, 16.96478717937593572 ) ) ;
#929 = VERTEX_POINT ( 'NONE', #23904 ) ;
#930 = CARTESIAN_POINT ( 'NONE',  ( 4.834790513006555379, -32.10612123254703221, -34.66678987626880826 ) ) ;
#931 = CARTESIAN_POINT ( 'NONE',  ( 4.553261556744873317, 7.233533384970671776, 43.32684572631789166 ) ) ;
#932 = ORIENTED_EDGE ( 'NONE', *, *, #47477, .F. ) ;
#933 = CARTESIAN_POINT ( 'NONE',  ( 1.088908134280554885, -6.374115321932803724, -42.43751564162690926 ) ) ;
#934 = VECTOR ( 'NONE', #9923, 999.9999999999998863 ) ;
#935 = EDGE_LOOP ( 'NONE', ( #31985, #2475, #19862, #53772 ) ) ;
#936 = CARTESIAN_POINT ( 'NONE',  ( 4.999999999999997335, 9.184547653667864935E-16, -9.629649721936170507E-32 ) ) ;
#937 = ORIENTED_EDGE ( 'NONE', *, *, #19804, .F. ) ;
#938 = CARTESIAN_POINT ( 'NONE',  ( 0.3676999524040366896, -13.34038000160327364, -42.04741186726791113 ) ) ;
#939 = CARTESIAN_POINT ( 'NONE',  ( -2.569797478183790229, 10.65947181927839615, -10.02484965418630303 ) ) ;
#940 = VERTEX_POINT ( 'NONE', #43035 ) ;
#941 = DIRECTION ( 'NONE',  ( -1.000000000000000000, -0.000000000000000000, -0.000000000000000000 ) ) ;
#942 = EDGE_CURVE ( 'NONE', #12367, #49832, #46520, .T. ) ;
#943 = ORIENTED_EDGE ( 'NONE', *, *, #26032, .F. ) ;
#944 = CARTESIAN_POINT ( 'NONE',  ( 4.975801465491695552, 0.000000000000000000, 0.000000000000000000 ) ) ;
#945 = CARTESIAN_POINT ( 'NONE',  ( 0.9968887458511664912, 22.02152923727802403, -36.82760690604603582 ) ) ;
#946 = CARTESIAN_POINT ( 'NONE',  ( 0.5837800005270550319, 40.34941272192465078, 23.89895712447661680 ) ) ;
#947 = EDGE_LOOP ( 'NONE', ( #43971, #42340, #37157, #45668 ) ) ;
#948 = CARTESIAN_POINT ( 'NONE',  ( 0.9268187852002115479, -35.91688603071045094, -25.56817613295056191 ) ) ;
#949 = CARTESIAN_POINT ( 'NONE',  ( 0.5806925824938502512, 32.20670061096268455, -34.08739940358283604 ) ) ;
#950 = CARTESIAN_POINT ( 'NONE',  ( 0.8753041380234530822, -45.17330286263802464, 19.24866323549142066 ) ) ;
#951 = ORIENTED_EDGE ( 'NONE', *, *, #57190, .F. ) ;
#952 = CARTESIAN_POINT ( 'NONE',  ( -6.017396004339687465, 18.20079405513549631, 4.878103249821131193 ) ) ;
#953 = FACE_OUTER_BOUND ( 'NONE', #61682, .T. ) ;
#954 = ORIENTED_EDGE ( 'NONE', *, *, #11455, .T. ) ;
#955 = CARTESIAN_POINT ( 'NONE',  ( 4.962356264823609031, -20.60668162140307658, 36.69605251817252878 ) ) ;
#956 = ORIENTED_EDGE ( 'NONE', *, *, #27151, .T. ) ;
#957 = CARTESIAN_POINT ( 'NONE',  ( -5.995132425357893702, 13.33084941932907519, 13.31880955509731734 ) ) ;
#958 = DIRECTION ( 'NONE',  ( 0.000000000000000000, -0.7071067811865487940, 0.7071067811865461294 ) ) ;
#959 = ORIENTED_EDGE ( 'NONE', *, *, #22632, .F. ) ;
#960 = CARTESIAN_POINT ( 'NONE',  ( 0.9780303403264759554, -12.72545693111817400, -39.92996818542863480 ) ) ;
#961 = CARTESIAN_POINT ( 'NONE',  ( -2.601141883200665639, 8.168301201416211299, 12.49296934088654076 ) ) ;
#962 = CARTESIAN_POINT ( 'NONE',  ( 4.956653778116975495, -27.17045123668499684, 39.67974989265029961 ) ) ;
#963 = CARTESIAN_POINT ( 'NONE',  ( 0.7056759521544929692, -39.13842014767732280, 25.84439779644466384 ) ) ;
#964 = CIRCLE ( 'NONE', #42008, 7.400000000000021672 ) ;
#965 = ORIENTED_EDGE ( 'NONE', *, *, #16950, .F. ) ;
#966 = EDGE_CURVE ( 'NONE', #10647, #6988, #36109, .T. ) ;
#967 = DIRECTION ( 'NONE',  ( 1.000000000000000000, 1.836909530733573776E-16, 0.000000000000000000 ) ) ;
#968 = B_SPLINE_CURVE_WITH_KNOTS ( 'NONE', 3,
 ( #26241, #55049, #43610, #44768 ),
 .UNSPECIFIED., .F., .F.,
 ( 4, 4 ),
 ( 0.000000000000000000, 0.004445488388166993383 ),
 .UNSPECIFIED. ) ;
#969 = EDGE_CURVE ( 'NONE', #49966, #55475, #35315, .T. ) ;
#970 = FACE_BOUND ( 'NONE', #13663, .T. ) ;
#971 = CARTESIAN_POINT ( 'NONE',  ( 0.5800708057587357080, 46.09746469244102229, 13.00144577271058388 ) ) ;
#972 = CARTESIAN_POINT ( 'NONE',  ( -6.010958268070873523, 14.94067681728549779, 11.48268200989202192 ) ) ;
#973 = EDGE_CURVE ( 'NONE', #44200, #49037, #20751, .T. ) ;
#974 = CARTESIAN_POINT ( 'NONE',  ( 4.956653778116990594, -3.690426056929668075, -47.94889704119055551 ) ) ;
#975 = VECTOR ( 'NONE', #8436, 1000.000000000000227 ) ;
#976 = CARTESIAN_POINT ( 'NONE',  ( 0.8744876279028306332, 17.78802839418675674, 45.75954650373076049 ) ) ;
#977 = CARTESIAN_POINT ( 'NONE',  ( 0.8751705887134423323, -17.57879340691512837, -44.76769609654229498 ) ) ;
#978 = CARTESIAN_POINT ( 'NONE',  ( 0.09136607875274982415, 0.000000000000000000, 0.000000000000000000 ) ) ;
#979 = CARTESIAN_POINT ( 'NONE',  ( 7.000000000000016875, -56.56854249492410958, 56.56854249492351983 ) ) ;
#980 = CARTESIAN_POINT ( 'NONE',  ( 0.1145239942831223490, 39.61174555950172760, 19.43849516896738905 ) ) ;
#981 = CARTESIAN_POINT ( 'NONE',  ( 0.5806925824938494740, -1.020860314013172454, 46.88475452172951918 ) ) ;
#982 = EDGE_CURVE ( 'NONE', #10729, #25288, #1299, .T. ) ;
#983 = DIRECTION ( 'NONE',  ( -0.1011922191286467598, -0.9919158664526095404, -0.07657054699679781418 ) ) ;
#984 = ORIENTED_EDGE ( 'NONE', *, *, #31684, .F. ) ;
#985 = CARTESIAN_POINT ( 'NONE',  ( 0.5809828226811626362, 29.58751527316234231, -37.66417181417519799 ) ) ;
#986 = CARTESIAN_POINT ( 'NONE',  ( 0.5997462898726536595, -7.321308210775749004, 48.55872811583040516 ) ) ;
#987 = CARTESIAN_POINT ( 'NONE',  ( 0.3622758884714600280, 39.50828911766974016, 17.25816669465007891 ) ) ;
#988 = VERTEX_POINT ( 'NONE', #20435 ) ;
#989 = CARTESIAN_POINT ( 'NONE',  ( 0.9758171775293910111, 5.606549717954186995, 42.54062484958058121 ) ) ;
#990 = CARTESIAN_POINT ( 'NONE',  ( 3.894904216938898323, 26.94017379411146607, 34.73256927466309918 ) ) ;
#991 = EDGE_CURVE ( 'NONE', #3830, #45554, #39257, .T. ) ;
#992 =( BOUNDED_SURFACE ( )  B_SPLINE_SURFACE ( 3, 1, ( 
 ( #421, #14258 ),
 ( #33364, #13635 ),
 ( #19566, #28636 ),
 ( #23948, #56213 ) ),
 .UNSPECIFIED., .F., .F., .F. ) 
 B_SPLINE_SURFACE_WITH_KNOTS ( ( 4, 4 ),
 ( 2, 2 ),
 ( 0.000000000000000000, 1.000000000000000000 ),
 ( 0.000000000000000000, 1.000000000000000000 ),
 .UNSPECIFIED. ) 
 GEOMETRIC_REPRESENTATION_ITEM ( )  RATIONAL_B_SPLINE_SURFACE ( (
 ( 1.000000000000000000, 1.000000000000000000),
 ( 0.9953390228620291325, 0.8624445117760984880),
 ( 0.9953390228620291325, 0.8624445117760984880),
 ( 1.000000000000000000, 1.000000000000000000) ) ) 
 REPRESENTATION_ITEM ( '' )  SURFACE ( )  );
#993 = B_SPLINE_CURVE_WITH_KNOTS ( 'NONE', 3,
 ( #7007, #34629, #29915, #16436 ),
 .UNSPECIFIED., .F., .F.,
 ( 4, 4 ),
 ( 0.000000000000000000, 0.004447772540403792038 ),
 .UNSPECIFIED. ) ;
#994 = ORIENTED_EDGE ( 'NONE', *, *, #2396, .T. ) ;
#995 = VERTEX_POINT ( 'NONE', #15749 ) ;
#996 = CARTESIAN_POINT ( 'NONE',  ( 0.7044674535453004927, 21.96536420256020250, -43.92408790469978896 ) ) ;
#997 = ORIENTED_EDGE ( 'NONE', *, *, #53649, .T. ) ;
#998 =( BOUNDED_SURFACE ( )  B_SPLINE_SURFACE ( 3, 1, ( 
 ( #15677, #54781 ),
 ( #21290, #34781 ),
 ( #20676, #49790 ),
 ( #15982, #53845 ) ),
 .UNSPECIFIED., .F., .F., .F. ) 
 B_SPLINE_SURFACE_WITH_KNOTS ( ( 4, 4 ),
 ( 2, 2 ),
 ( 0.000000000000000000, 1.000000000000000000 ),
 ( 0.000000000000000000, 1.000000000000000000 ),
 .UNSPECIFIED. ) 
 GEOMETRIC_REPRESENTATION_ITEM ( )  RATIONAL_B_SPLINE_SURFACE ( (
 ( 1.000000000000000000, 1.000000000000000000),
 ( 0.7269869731126821222, 0.9931720237060910339),
 ( 0.7269869731126821222, 0.9931720237060910339),
 ( 1.000000000000000000, 1.000000000000000000) ) ) 
 REPRESENTATION_ITEM ( '' )  SURFACE ( )  );
#999 = CARTESIAN_POINT ( 'NONE',  ( 4.956445790444027111, 8.365049606152357597, -46.34181691762039179 ) ) ;
#1000 = ORIENTED_EDGE ( 'NONE', *, *, #47037, .T. ) ;
#1001 = VERTEX_POINT ( 'NONE', #34238 ) ;
#1002 = CARTESIAN_POINT ( 'NONE',  ( 0.5980271706414734822, -20.51809962909598184, -44.62125984832962899 ) ) ;
#1003 = EDGE_LOOP ( 'NONE', ( #55950, #35313, #30459, #44447 ) ) ;
#1004 = DIRECTION ( 'NONE',  ( 0.000000000000000000, 0.7071067811865500152, -0.7071067811865449082 ) ) ;
#1005 = CARTESIAN_POINT ( 'NONE',  ( 4.975801465491695552, 47.76942479135485797, -3.702618843596948039 ) ) ;
#1006 = EDGE_CURVE ( 'NONE', #14410, #28664, #11050, .T. ) ;
#1007 = CARTESIAN_POINT ( 'NONE',  ( 0.6041374136657476912, -41.74951251761557813, -23.90252055111306717 ) ) ;
#1008 = ORIENTED_EDGE ( 'NONE', *, *, #22055, .F. ) ;
#1009 = CARTESIAN_POINT ( 'NONE',  ( 4.963659409799330291, -43.79875484948454556, 9.199077662858760718 ) ) ;
#1010 = LINE ( 'NONE', #39571, #13026 ) ;
#1011 = ORIENTED_EDGE ( 'NONE', *, *, #3651, .F. ) ;
#1012 = ORIENTED_EDGE ( 'NONE', *, *, #32338, .T. ) ;
#1013 = CARTESIAN_POINT ( 'NONE',  ( 50.50000000000000000, 0.000000000000000000, -2.649999999999992806 ) ) ;
#1014 = VECTOR ( 'NONE', #19095, 1000.000000000000000 ) ;
#1015 = CARTESIAN_POINT ( 'NONE',  ( 5.895596859100789899, -7.232071727009982354, -18.76766692340500242 ) ) ;
#1016 = CARTESIAN_POINT ( 'NONE',  ( 5.958863334805807099, -14.51296551801813095, 14.51469124124454702 ) ) ;
#1017 = CARTESIAN_POINT ( 'NONE',  ( 0.1064266418746774995, 0.5615180042400674809, -43.12102053154802661 ) ) ;
#1019 = ORIENTED_EDGE ( 'NONE', *, *, #22432, .T. ) ;
#1018 = B_SPLINE_CURVE_WITH_KNOTS ( 'NONE', 3,
 ( #48990, #34593, #49286, #53658, #15796, #29258 ),
 .UNSPECIFIED., .F., .F.,
 ( 4, 2, 4 ),
 ( 8.848046324741092137E-18, 0.0002291978881530155638, 0.0004583957763060222913 ),
 .UNSPECIFIED. ) ;
#1020 = CARTESIAN_POINT ( 'NONE',  ( 0.6017667736363748743, -12.78803812527920591, 46.37677940471275662 ) ) ;
#1021 = CARTESIAN_POINT ( 'NONE',  ( -5.995132425357893702, 0.008513469642806619636, 18.84415457712583475 ) ) ;
#1022 = CARTESIAN_POINT ( 'NONE',  ( 2.282803330402978670, 45.63374208672272658, -11.13815472237010695 ) ) ;
#1023 = CARTESIAN_POINT ( 'NONE',  ( 0.6041374136657475802, 6.452348380035901165, -47.67304777898693402 ) ) ;
#1024 = ORIENTED_EDGE ( 'NONE', *, *, #19184, .T. ) ;
#1025 = CARTESIAN_POINT ( 'NONE',  ( 2.359973842542475886, -42.94220026048606087, -9.700687162299988842 ) ) ;
#1026 = CARTESIAN_POINT ( 'NONE',  ( 4.975610109902397937, 0.000000000000000000, 0.000000000000000000 ) ) ;
#1027 = CARTESIAN_POINT ( 'NONE',  ( 5.901764892641307547, -32.89013534638866787, -36.27989063291003191 ) ) ;
#1028 = DIRECTION ( 'NONE',  ( -1.000000000000000000, -0.000000000000000000, -0.000000000000000000 ) ) ;
#1029 = VERTEX_POINT ( 'NONE', #34856 ) ;
#1030 = ORIENTED_EDGE ( 'NONE', *, *, #26800, .F. ) ;
#1031 = DIRECTION ( 'NONE',  ( 0.09835009131224564660, 0.2650256080583759943, -0.9592125346408693076 ) ) ;
#1032 = DIRECTION ( 'NONE',  ( 0.07836865515943411409, -0.2503967164834464132, -0.9649662368512228472 ) ) ;
#1033 = ADVANCED_FACE ( 'NONE', ( #49241 ), #29825, .F. ) ;
#1034 = CARTESIAN_POINT ( 'NONE',  ( 3.240649175237396484, -42.05244175136726170, -12.91731629037221474 ) ) ;
#1035 = CARTESIAN_POINT ( 'NONE',  ( 3.782625744892853081, -19.24499441524892518, -37.37470125702732560 ) ) ;
#1036 = CARTESIAN_POINT ( 'NONE',  ( 0.1119898979215350893, 15.76451811348070997, 41.21214962728306119 ) ) ;
#1037 = EDGE_CURVE ( 'NONE', #437, #47724, #101, .T. ) ;
#1038 = DIRECTION ( 'NONE',  ( 0.000000000000000000, 0.000000000000000000, 1.000000000000000000 ) ) ;
#1039 = B_SPLINE_CURVE_WITH_KNOTS ( 'NONE', 3,
 ( #22633, #61430, #38919, #57348 ),
 .UNSPECIFIED., .F., .F.,
 ( 4, 4 ),
 ( 1.226634733346699349E-18, 0.004042984057420973693 ),
 .UNSPECIFIED. ) ;
#1040 = CARTESIAN_POINT ( 'NONE',  ( 5.965394784446460541, -20.35165389555760029, 2.664747781315769615 ) ) ;
#1041 = CARTESIAN_POINT ( 'NONE',  ( -6.078457390727109555, -6.654470124808557152, -18.06965794904646216 ) ) ;
#1042 = EDGE_CURVE ( 'NONE', #26356, #28755, #19522, .T. ) ;
#1043 = DIRECTION ( 'NONE',  ( 1.000000000000000000, 0.000000000000000000, 0.000000000000000000 ) ) ;
#1044 = AXIS2_PLACEMENT_3D ( 'NONE', #15501, #38707, #9874 ) ;
#1045 = EDGE_CURVE ( 'NONE', #44352, #37554, #11099, .T. ) ;
#1046 = CARTESIAN_POINT ( 'NONE',  ( 4.549368137175248350, 0.000000000000000000, 0.000000000000000000 ) ) ;
#1047 = ORIENTED_EDGE ( 'NONE', *, *, #27171, .T. ) ;
#1048 = EDGE_CURVE ( 'NONE', #8147, #48887, #3112, .T. ) ;
#1049 = CARTESIAN_POINT ( 'NONE',  ( 0.3622758884714600280, -20.83792692158946025, -37.74294673546579304 ) ) ;
#1050 = CARTESIAN_POINT ( 'NONE',  ( 4.962356264823601926, 34.44911810793277596, -24.17630781256817940 ) ) ;
#1051 = CARTESIAN_POINT ( 'NONE',  ( 0.5980894510889448457, 38.59343625445447401, -28.72954109785563404 ) ) ;
#1052 = CARTESIAN_POINT ( 'NONE',  ( 0.5998501479064708430, -47.62484632993683675, -6.798102206413969562 ) ) ;
#1053 = CARTESIAN_POINT ( 'NONE',  ( 0.5834872094924179464, -41.59216540884680313, 23.75111410077694174 ) ) ;
#1054 = CARTESIAN_POINT ( 'NONE',  ( 0.7056759521544955227, 45.45046072100352319, -11.57602908451353585 ) ) ;
#1055 = CARTESIAN_POINT ( 'NONE',  ( 4.834790513006553603, -16.75039937818133140, 44.18159641293876660 ) ) ;
#1056 = AXIS2_PLACEMENT_3D ( 'NONE', #46617, #46933, #37219 ) ;
#1057 = EDGE_CURVE ( 'NONE', #15504, #24440, #40539, .T. ) ;
#1058 = CARTESIAN_POINT ( 'NONE',  ( 4.549368137175248350, 0.000000000000000000, 0.000000000000000000 ) ) ;
#1059 = ADVANCED_FACE ( 'NONE', ( #44575 ), #1610, .T. ) ;
#1060 = CARTESIAN_POINT ( 'NONE',  ( 4.960156602257177916, 30.99165383632763238, 34.56254177294278662 ) ) ;
#1061 = CARTESIAN_POINT ( 'NONE',  ( 0.6029443199889047422, 48.20183188216083892, 9.387281025851251570 ) ) ;
#1063 = ORIENTED_EDGE ( 'NONE', *, *, #30338, .F. ) ;
#1062 = CARTESIAN_POINT ( 'NONE',  ( 0.000000000000000000, 0.000000000000000000, -5.599999999999999645 ) ) ;
#1064 = ORIENTED_EDGE ( 'NONE', *, *, #141, .F. ) ;
#1065 = CARTESIAN_POINT ( 'NONE',  ( 1.091591847532191073, 36.45402868198649315, -20.68484430226018489 ) ) ;
#1066 = CARTESIAN_POINT ( 'NONE',  ( 0.1368894036331276820, -43.83795633916983547, -5.009482002001066192 ) ) ;
#1067 = CARTESIAN_POINT ( 'NONE',  ( 0.1135584504625008068, 41.73827531235328081, 14.31322556538019164 ) ) ;
#1068 = ORIENTED_EDGE ( 'NONE', *, *, #6587, .F. ) ;
#1069 = CARTESIAN_POINT ( 'NONE',  ( 1.227938101723747621, 22.18841447410770940, -36.73927144310489012 ) ) ;
#1070 = CARTESIAN_POINT ( 'NONE',  ( 3.238931869106854933, -14.74782013370872846, 40.38337734129178358 ) ) ;
#1071 = CARTESIAN_POINT ( 'NONE',  ( 2.624215991343608501, -17.05978231157370928, -44.87417713512106587 ) ) ;
#1072 = ORIENTED_EDGE ( 'NONE', *, *, #37861, .F. ) ;
#1073 = ORIENTED_EDGE ( 'NONE', *, *, #49902, .F. ) ;
#1074 = CARTESIAN_POINT ( 'NONE',  ( 1.000433927950263646, 33.29480191618684159, 25.45338568864124795 ) ) ;
#1075 = CARTESIAN_POINT ( 'NONE',  ( 0.9730545539215883499, -39.44597740938048958, -16.88610103448599986 ) ) ;
#1076 = CARTESIAN_POINT ( 'NONE',  ( 1.227938101723748288, -25.45152231597034387, -34.55893248994532030 ) ) ;
#1077 = CARTESIAN_POINT ( 'NONE',  ( 4.962356264823608143, 0.000000000000000000, 0.000000000000000000 ) ) ;
#1078 = CARTESIAN_POINT ( 'NONE',  ( -79.49999999999975842, 4.769696007084731626, 1.500000000000002220 ) ) ;
#1079 = EDGE_CURVE ( 'NONE', #57986, #43044, #10426, .T. ) ;
#1080 = CARTESIAN_POINT ( 'NONE',  ( 0.8560838555295223751, -34.16988317699956923, 32.13708010619405542 ) ) ;
#1081 = ADVANCED_FACE ( 'NONE', ( #35168 ), #6041, .F. ) ;
#1082 = CARTESIAN_POINT ( 'NONE',  ( 0.9757402383260936896, 42.53022961222603726, 5.684842778069367775 ) ) ;
#1083 = EDGE_LOOP ( 'NONE', ( #44728, #30417, #16495, #59746 ) ) ;
#1084 = EDGE_LOOP ( 'NONE', ( #1474, #55394, #45983, #47094 ) ) ;
#1085 = CARTESIAN_POINT ( 'NONE',  ( 0.9754292589017198312, -30.68784786461271352, 28.54090854078868844 ) ) ;
#1086 = CARTESIAN_POINT ( 'NONE',  ( 0.9968887458511644928, -0.6574002966411479632, 42.90440775986216693 ) ) ;
#1087 = EDGE_LOOP ( 'NONE', ( #1602, #31859, #25371, #6168 ) ) ;
#1088 = CARTESIAN_POINT ( 'NONE',  ( 4.691466044806103852, 20.01963481131604183, 39.84135254923144487 ) ) ;
#1089 = CARTESIAN_POINT ( 'NONE',  ( 3.661933894777877896, -12.12681416997633121, -45.44855930652273912 ) ) ;
#1090 = CARTESIAN_POINT ( 'NONE',  ( 5.896782393890504181, -13.97772289704270676, -14.46199673252280249 ) ) ;
#1091 = CARTESIAN_POINT ( 'NONE',  ( 4.691466044806103852, 33.74235639413287657, 29.14742760351121831 ) ) ;
#1092 = ORIENTED_EDGE ( 'NONE', *, *, #34956, .T. ) ;
#1093 = CARTESIAN_POINT ( 'NONE',  ( 5.981074661064941900, 19.82752479807519919, 5.303881226583745168 ) ) ;
#1094 = FACE_OUTER_BOUND ( 'NONE', #30509, .T. ) ;
#1095 = CARTESIAN_POINT ( 'NONE',  ( 0.5987334363312691865, 28.58958334901124587, -39.92741702642453561 ) ) ;
#1096 = VECTOR ( 'NONE', #56830, 1000.000000000000227 ) ;
#1097 = CARTESIAN_POINT ( 'NONE',  ( 5.965394784446460541, -17.78272165951808148, 10.25014670152084229 ) ) ;
#1098 = ORIENTED_EDGE ( 'NONE', *, *, #1896, .F. ) ;
#1099 = LINE ( 'NONE', #49642, #12543 ) ;
#1100 = ORIENTED_EDGE ( 'NONE', *, *, #30334, .T. ) ;
#1101 = CARTESIAN_POINT ( 'NONE',  ( 4.322998006666165516, -22.13465289016597382, -42.57894920390120319 ) ) ;
#1102 = CARTESIAN_POINT ( 'NONE',  ( 0.5832367798473389042, 24.18350431151220192, -41.34221369670658675 ) ) ;
#1103 = ORIENTED_EDGE ( 'NONE', *, *, #51969, .F. ) ;
#1104 = CARTESIAN_POINT ( 'NONE',  ( 0.6001305935487422083, 11.94532529598378012, -46.60388846085711378 ) ) ;
#1105 = CARTESIAN_POINT ( 'NONE',  ( -6.010958268070873523, 16.32616437357112105, 9.409153349053642756 ) ) ;
#1106 = CARTESIAN_POINT ( 'NONE',  ( 4.967162193818130511, 32.10009971360111791, -28.74031574029977776 ) ) ;
#1107 = EDGE_CURVE ( 'NONE', #42042, #20290, #49545, .T. ) ;
#1108 = CARTESIAN_POINT ( 'NONE',  ( 0.1129192098497447394, -18.30288010335054949, -40.14917642626718930 ) ) ;
#1109 = CARTESIAN_POINT ( 'NONE',  ( 4.291220156522059348, 18.92432707711549256, -43.14230918696924277 ) ) ;
#1110 = CARTESIAN_POINT ( 'NONE',  ( 0.7764146366350254125, 45.46540463260674159, 11.52985061752779394 ) ) ;
#1111 = CARTESIAN_POINT ( 'NONE',  ( 0.1064266379913943877, -21.07422113734189750, 37.62465837278038094 ) ) ;
#1112 =( BOUNDED_SURFACE ( )  B_SPLINE_SURFACE ( 3, 1, ( 
 ( #25198, #24903 ),
 ( #39632, #58382 ),
 ( #35235, #54296 ),
 ( #15505, #44342 ) ),
 .UNSPECIFIED., .F., .F., .F. ) 
 B_SPLINE_SURFACE_WITH_KNOTS ( ( 4, 4 ),
 ( 2, 2 ),
 ( 0.000000000000000000, 1.000000000000000000 ),
 ( 0.000000000000000000, 1.000000000000000000 ),
 .UNSPECIFIED. ) 
 GEOMETRIC_REPRESENTATION_ITEM ( )  RATIONAL_B_SPLINE_SURFACE ( (
 ( 1.000000000000000000, 1.000000000000000000),
 ( 0.9751682680413298332, 0.9999560080971552356),
 ( 0.9751682680413298332, 0.9999560080971552356),
 ( 1.000000000000000000, 1.000000000000000000) ) ) 
 REPRESENTATION_ITEM ( '' )  SURFACE ( )  );
#1113 = FACE_OUTER_BOUND ( 'NONE', #4513, .T. ) ;
#1114 = ORIENTED_EDGE ( 'NONE', *, *, #16102, .T. ) ;
#1115 = FACE_OUTER_BOUND ( 'NONE', #7002, .T. ) ;
#1116 = EDGE_CURVE ( 'NONE', #39908, #48550, #49093, .T. ) ;
#1117 = CARTESIAN_POINT ( 'NONE',  ( 4.956653778117001252, 47.27023054223765541, -8.845409907520457082 ) ) ;
#1118 = ADVANCED_FACE ( 'NONE', ( #59873 ), #21225, .F. ) ;
#1119 = CARTESIAN_POINT ( 'NONE',  ( 3.240649175237395596, 16.89562953456788819, -40.61776237101557285 ) ) ;
#1120 = VERTEX_POINT ( 'NONE', #49868 ) ;
#1121 = EDGE_CURVE ( 'NONE', #11901, #16132, #11993, .T. ) ;
#1122 = CARTESIAN_POINT ( 'NONE',  ( 0.7056313189692690058, 16.06732225071473508, -44.06347466609102526 ) ) ;
#1123 = DIRECTION ( 'NONE',  ( 0.09835009131224550782, -0.9223318362920762681, -0.3736726418952285855 ) ) ;
#1124 = CARTESIAN_POINT ( 'NONE',  ( 0.6024113833632039894, 22.52083809065578990, 43.63890146183028662 ) ) ;
#1125 = CARTESIAN_POINT ( 'NONE',  ( 0.5804410086790514622, -45.84731009780851707, -9.876437042313495951 ) ) ;
#1126 = B_SPLINE_CURVE_WITH_KNOTS ( 'NONE', 3,
 ( #53200, #18468, #47908, #47595, #4636, #57262 ),
 .UNSPECIFIED., .F., .F.,
 ( 4, 2, 4 ),
 ( 4.878909776184769953E-19, 0.0002293801035737091010, 0.0004587602071474177140 ),
 .UNSPECIFIED. ) ;
#1127 = CARTESIAN_POINT ( 'NONE',  ( 0.6024113833632039894, -20.07675414434353200, 44.81591025660922156 ) ) ;
#1128 = CARTESIAN_POINT ( 'NONE',  ( 0.6031356219577718170, 38.11305734842063941, -29.35521383643418503 ) ) ;
#1129 = CARTESIAN_POINT ( 'NONE',  ( -1.599999999999950795, 8.286069005957492380E-13, -80.00000000000001421 ) ) ;
#1130 = CARTESIAN_POINT ( 'NONE',  ( 4.291220156522060236, -47.09990378333908723, -0.9940125280393553586 ) ) ;
#1131 = ADVANCED_FACE ( 'NONE', ( #41422 ), #10810, .F. ) ;
#1132 = CARTESIAN_POINT ( 'NONE',  ( -1.200000000000006617, 6.873330160214519262E-16, 5.612499999999999822 ) ) ;
#1133 = CARTESIAN_POINT ( 'NONE',  ( 4.956445790444002242, -36.61936279692601204, 29.60676136436992678 ) ) ;
#1135 = ORIENTED_EDGE ( 'NONE', *, *, #2307, .F. ) ;
#1134 = LINE ( 'NONE', #20271, #18358 ) ;
#1136 = ORIENTED_EDGE ( 'NONE', *, *, #51297, .F. ) ;
#1137 = FACE_OUTER_BOUND ( 'NONE', #50337, .T. ) ;
#1138 = B_SPLINE_CURVE_WITH_KNOTS ( 'NONE', 3,
 ( #1297, #39882, #370, #33930 ),
 .UNSPECIFIED., .F., .F.,
 ( 4, 4 ),
 ( 4.670885906470169154E-18, 0.004050076154993003351 ),
 .UNSPECIFIED. ) ;
#1139 = CARTESIAN_POINT ( 'NONE',  ( 0.5997462898726536595, -8.352924653000716404, 48.39194436975645175 ) ) ;
#1140 = CARTESIAN_POINT ( 'NONE',  ( 4.549368137175248350, -28.46244473166650479, -32.13400537129916046 ) ) ;
#1141 = CARTESIAN_POINT ( 'NONE',  ( 4.960386119450139297, 41.48529788082155534, 13.90706742673822838 ) ) ;
#1142 = CARTESIAN_POINT ( 'NONE',  ( 1.157644175074338921, -41.23316702885658458, 7.538448928632200285 ) ) ;
#1143 = CARTESIAN_POINT ( 'NONE',  ( 0.1158516988532803799, 9.770552602771916284, -43.02880965898619081 ) ) ;
#1144 = VECTOR ( 'NONE', #29188, 1000.000000000000000 ) ;
#1145 = ORIENTED_EDGE ( 'NONE', *, *, #12252, .T. ) ;
#1146 = VERTEX_POINT ( 'NONE', #30749 ) ;
#1147 = CARTESIAN_POINT ( 'NONE',  ( 4.549368137175248350, -28.14399996863474129, -32.41327393324131378 ) ) ;
#1148 = DIRECTION ( 'NONE',  ( 0.07906939808003035641, 0.2876259487683096583, 0.9544733332484420796 ) ) ;
#1149 = CARTESIAN_POINT ( 'NONE',  ( 0.6024113833632039894, 37.25118206351266537, 31.99830157948853326 ) ) ;
#1150 = ORIENTED_EDGE ( 'NONE', *, *, #24042, .T. ) ;
#1151 = B_SPLINE_CURVE_WITH_KNOTS ( 'NONE', 3,
 ( #11366, #25144, #44290, #30451 ),
 .UNSPECIFIED., .F., .F.,
 ( 4, 4 ),
 ( 2.100108283942811974E-17, 0.004444306975806115029 ),
 .UNSPECIFIED. ) ;
#1152 = CARTESIAN_POINT ( 'NONE',  ( 0.1103744047535531458, -0.03874731383761919473, 43.12441516302519773 ) ) ;
#1153 = CARTESIAN_POINT ( 'NONE',  ( 0.2500000000000002220, 0.000000000000000000, 0.000000000000000000 ) ) ;
#1154 = ORIENTED_EDGE ( 'NONE', *, *, #29107, .T. ) ;
#1155 = ADVANCED_FACE ( 'NONE', ( #26675 ), #57594, .F. ) ;
#1156 = CARTESIAN_POINT ( 'NONE',  ( 0.1073791018717483448, -21.14095454447585709, 37.58707531572169813 ) ) ;
#1157 = VERTEX_POINT ( 'NONE', #7237 ) ;
#1158 = CARTESIAN_POINT ( 'NONE',  ( 0.5835226383429259478, -34.65813563702828759, 31.59202603049256908 ) ) ;
#1159 = CARTESIAN_POINT ( 'NONE',  ( 0.6028618097248863439, 34.14037999462324535, 33.89350006451839192 ) ) ;
#1160 = EDGE_LOOP ( 'NONE', ( #10693, #60226, #61947, #6287 ) ) ;
#1161 = CARTESIAN_POINT ( 'NONE',  ( 2.648799415243708655, 26.90653288552096711, -40.99458441513923646 ) ) ;
#1162 = CARTESIAN_POINT ( 'NONE',  ( 0.8554163680231720024, -44.61245466728215092, -14.52357950615188642 ) ) ;
#1163 = CARTESIAN_POINT ( 'NONE',  ( 0.9769922540276050338, 40.30057869606137899, 11.49760461351358209 ) ) ;
#1164 = DIRECTION ( 'NONE',  ( 0.000000000000000000, 0.000000000000000000, -1.000000000000000000 ) ) ;
#1165 = ORIENTED_EDGE ( 'NONE', *, *, #39795, .T. ) ;
#1166 = CARTESIAN_POINT ( 'NONE',  ( -6.016761891674564211, -17.40752468084787452, 7.214149619366299504 ) ) ;
#1167 = CARTESIAN_POINT ( 'NONE',  ( 0.8551540677456739292, 44.61036085020975150, -17.49081417858739229 ) ) ;
#1169 = ORIENTED_EDGE ( 'NONE', *, *, #4409, .T. ) ;
#1168 =( BOUNDED_SURFACE ( )  B_SPLINE_SURFACE ( 3, 1, ( 
 ( #4101, #45834 ),
 ( #3800, #56425 ),
 ( #23241, #50502 ),
 ( #17312, #31716 ) ),
 .UNSPECIFIED., .F., .F., .F. ) 
 B_SPLINE_SURFACE_WITH_KNOTS ( ( 4, 4 ),
 ( 2, 2 ),
 ( 0.000000000000000000, 1.000000000000000000 ),
 ( 0.000000000000000000, 1.000000000000000000 ),
 .UNSPECIFIED. ) 
 GEOMETRIC_REPRESENTATION_ITEM ( )  RATIONAL_B_SPLINE_SURFACE ( (
 ( 1.000000000000000000, 1.000000000000000000),
 ( 0.7269869731126821222, 0.9931720237060910339),
 ( 0.7269869731126821222, 0.9931720237060910339),
 ( 1.000000000000000000, 1.000000000000000000) ) ) 
 REPRESENTATION_ITEM ( '' )  SURFACE ( )  );
#1170 = CARTESIAN_POINT ( 'NONE',  ( 4.960386119450136633, 7.741275488564100193, 43.06401187166027711 ) ) ;
#1171 = ORIENTED_EDGE ( 'NONE', *, *, #26743, .F. ) ;
#1172 = CARTESIAN_POINT ( 'NONE',  ( 0.5819845079324662551, -17.90867223323918367, 44.42187385013357925 ) ) ;
#1173 = ORIENTED_EDGE ( 'NONE', *, *, #12970, .F. ) ;
#1174 = CARTESIAN_POINT ( 'NONE',  ( 0.1064266418746779297, 41.50637583369805128, 11.70292610004339195 ) ) ;
#1175 = FACE_BOUND ( 'NONE', #17045, .T. ) ;
#1176 = CARTESIAN_POINT ( 'NONE',  ( 0.1129192098497447394, 33.91039995638862337, 28.23183597612653983 ) ) ;
#1177 = VERTEX_POINT ( 'NONE', #2229 ) ;
#1178 = CARTESIAN_POINT ( 'NONE',  ( 0.5809828226811553087, 6.791453954330313181, 47.41188724015881917 ) ) ;
#1179 = CARTESIAN_POINT ( 'NONE',  ( 3.407937589446174087, 9.356405769959053487, 10.00592723328964162 ) ) ;
#1180 = EDGE_CURVE ( 'NONE', #50113, #497, #50927, .T. ) ;
#1181 = DIRECTION ( 'NONE',  ( 1.000000000000000000, 0.000000000000000000, 0.000000000000000000 ) ) ;
#1182 = ORIENTED_EDGE ( 'NONE', *, *, #29135, .F. ) ;
#1183 = VECTOR ( 'NONE', #23803, 1000.000000000000000 ) ;
#1184 = ADVANCED_FACE ( 'NONE', ( #46119 ), #59, .F. ) ;
#1185 = ORIENTED_EDGE ( 'NONE', *, *, #43378, .T. ) ;
#1186 =( BOUNDED_SURFACE ( )  B_SPLINE_SURFACE ( 3, 1, ( 
 ( #56448, #37376 ),
 ( #13562, #37076 ),
 ( #51750, #61444 ),
 ( #18567, #16256 ) ),
 .UNSPECIFIED., .F., .F., .F. ) 
 B_SPLINE_SURFACE_WITH_KNOTS ( ( 4, 4 ),
 ( 2, 2 ),
 ( 0.000000000000000000, 1.000000000000000000 ),
 ( 0.000000000000000000, 1.000000000000000000 ),
 .UNSPECIFIED. ) 
 GEOMETRIC_REPRESENTATION_ITEM ( )  RATIONAL_B_SPLINE_SURFACE ( (
 ( 1.000000000000000000, 1.000000000000000000),
 ( 0.9953390228620291325, 0.8624445117760984880),
 ( 0.9953390228620291325, 0.8624445117760984880),
 ( 1.000000000000000000, 1.000000000000000000) ) ) 
 REPRESENTATION_ITEM ( '' )  SURFACE ( )  );
#1187 = CARTESIAN_POINT ( 'NONE',  ( 0.9784957157296363395, -31.23728338876063049, -27.93859666272861375 ) ) ;
#1188 = CARTESIAN_POINT ( 'NONE',  ( 5.960221823109900008, 19.82478916873574448, -5.317678907195231730 ) ) ;
#1189 = CARTESIAN_POINT ( 'NONE',  ( 0.7044674535452954967, -19.10600803152149751, -45.24116687167055773 ) ) ;
#1190 = DIRECTION ( 'NONE',  ( 0.09722883295013597105, -0.9646010353641062407, 0.2451354658503108463 ) ) ;
#1191 = CARTESIAN_POINT ( 'NONE',  ( 0.9787464366903556590, -26.92194882595154226, -32.11763790043268330 ) ) ;
#1192 = CARTESIAN_POINT ( 'NONE',  ( 0.8751705887134423323, -28.56654290188627243, -38.69254731947824411 ) ) ;
#1193 = ORIENTED_EDGE ( 'NONE', *, *, #12418, .F. ) ;
#1194 = EDGE_CURVE ( 'NONE', #21289, #10372, #9768, .T. ) ;
#1195 = CARTESIAN_POINT ( 'NONE',  ( 0.6845945791218023269, 28.51769667890508586, 37.24442907125723679 ) ) ;
#1196 = ADVANCED_FACE ( 'NONE', ( #40814 ), #27628, .F. ) ;
#1197 = ORIENTED_EDGE ( 'NONE', *, *, #37868, .F. ) ;
#1198 = ADVANCED_FACE ( 'NONE', ( #22914 ), #35941, .F. ) ;
#1199 = CARTESIAN_POINT ( 'NONE',  ( 0.5998501479064699549, 12.95623334615437550, 46.33007877220744319 ) ) ;
#1200 = CARTESIAN_POINT ( 'NONE',  ( 1.227938101723748288, 42.91134962331487657, 0.8460948827226649760 ) ) ;
#1201 = DIRECTION ( 'NONE',  ( 1.000000000000000000, 0.000000000000000000, 0.000000000000000000 ) ) ;
#1202 = DIRECTION ( 'NONE',  ( 0.07836865515943412797, 0.7956898808744514717, -0.6006129930017356511 ) ) ;
#1203 = CARTESIAN_POINT ( 'NONE',  ( 2.879087469061463178, 11.47169626938654474, 42.47942868596894073 ) ) ;
#1204 =( LENGTH_UNIT ( ) NAMED_UNIT ( * ) SI_UNIT ( .MILLI., .METRE. ) );
#1205 = CARTESIAN_POINT ( 'NONE',  ( 4.960386119450149955, -10.60034705332619431, 42.45078452774905742 ) ) ;
#1206 = CARTESIAN_POINT ( 'NONE',  ( -6.077587904424778920, 9.987489566522585349, 16.46347695818028001 ) ) ;
#1207 = CARTESIAN_POINT ( 'NONE',  ( 0.7948884756798509921, -47.70571120116157005, 11.61308586860173797 ) ) ;
#1209 = EDGE_CURVE ( 'NONE', #37522, #55939, #6365, .T. ) ;
#1208 = DIRECTION ( 'NONE',  ( -0.07906939808003035641, 0.8535645278111612111, -0.5149520629629237289 ) ) ;
#1210 = CARTESIAN_POINT ( 'NONE',  ( 0.3622758884714730732, 34.70015533914794759, 25.58609868863780434 ) ) ;
#1211 = ADVANCED_FACE ( 'NONE', ( #23215 ), #34056, .F. ) ;
#1212 = CARTESIAN_POINT ( 'NONE',  ( -6.016761891674564211, -18.68153697670643609, 2.462934516563739518 ) ) ;
#1213 = DIRECTION ( 'NONE',  ( 0.07836865515943411409, 0.7860872967108141207, 0.6131273243286309294 ) ) ;
#1214 = ORIENTED_EDGE ( 'NONE', *, *, #58418, .T. ) ;
#1215 = CARTESIAN_POINT ( 'NONE',  ( 3.238018933889920792, -8.435922058907767251, -10.40397574889937182 ) ) ;
#1216 = CARTESIAN_POINT ( 'NONE',  ( 5.959547316686252039, -12.49238070347965035, -16.28624005235095495 ) ) ;
#1217 = CARTESIAN_POINT ( 'NONE',  ( 0.5839879882012682932, 18.32896541547133040, -44.25011577017253472 ) ) ;
#1218 = CARTESIAN_POINT ( 'NONE',  ( 5.896782393890504181, 12.98055409426303441, 15.36331026452057813 ) ) ;
#1219 = DIRECTION ( 'NONE',  ( 0.000000000000000000, 0.000000000000000000, 1.000000000000000000 ) ) ;
#1220 = EDGE_LOOP ( 'NONE', ( #16192, #58248 ) ) ;
#1221 = CARTESIAN_POINT ( 'NONE',  ( 0.9736507210033059634, -37.38294557109051652, 21.06291100879426992 ) ) ;
#1222 = CARTESIAN_POINT ( 'NONE',  ( 0.8551540677456739292, -23.16399837394517292, -41.94570365541225954 ) ) ;
#1223 =( REPRESENTATION_RELATIONSHIP ('NONE','NONE', #44881, #53251 ) REPRESENTATION_RELATIONSHIP_WITH_TRANSFORMATION ( #59297 )SHAPE_REPRESENTATION_RELATIONSHIP( ) );
#1224 = CARTESIAN_POINT ( 'NONE',  ( -99.49999999999975842, -9.382821356248120971E-15, -1.500000000000001554 ) ) ;
#1225 = AXIS2_PLACEMENT_3D ( 'NONE', #21925, #31315, #55107 ) ;
#1226 = ORIENTED_EDGE ( 'NONE', *, *, #1888, .F. ) ;
#1227 = CARTESIAN_POINT ( 'NONE',  ( 0.1313383488274139088, -30.94058105930541558, -30.03864748494533643 ) ) ;
#1228 = EDGE_CURVE ( 'NONE', #21594, #10282, #26979, .T. ) ;
#1229 = DIRECTION ( 'NONE',  ( 0.000000000000000000, 0.000000000000000000, -1.000000000000000000 ) ) ;
#1230 = ORIENTED_EDGE ( 'NONE', *, *, #16681, .T. ) ;
#1231 = CARTESIAN_POINT ( 'NONE',  ( 4.962356264823598373, -24.61258717641114657, 34.13877780978559429 ) ) ;
#1232 = ORIENTED_EDGE ( 'NONE', *, *, #35856, .F. ) ;
#1233 = CARTESIAN_POINT ( 'NONE',  ( -6.000000000000001776, 4.730042041638951881E-15, 0.000000000000000000 ) ) ;
#1234 = ORIENTED_EDGE ( 'NONE', *, *, #11984, .F. ) ;
#1235 = CARTESIAN_POINT ( 'NONE',  ( 0.1155031312995260795, 29.78923516837971874, -32.55062365938290014 ) ) ;
#1236 = CARTESIAN_POINT ( 'NONE',  ( 0.1152339509894530906, 20.60693138425672544, 39.01662555090813811 ) ) ;
#1237 = ORIENTED_EDGE ( 'NONE', *, *, #46578, .T. ) ;
#1238 = FACE_OUTER_BOUND ( 'NONE', #25127, .T. ) ;
#1239 = ORIENTED_EDGE ( 'NONE', *, *, #35443, .F. ) ;
#1240 = CARTESIAN_POINT ( 'NONE',  ( 0.1313383488274124655, -41.48452234694106266, 11.77600546273697724 ) ) ;
#1241 = CARTESIAN_POINT ( 'NONE',  ( 0.1152339509894530906, -1.190938228105830055, 44.10809853748038023 ) ) ;
#1242 = ORIENTED_EDGE ( 'NONE', *, *, #56798, .F. ) ;
#1243 = CARTESIAN_POINT ( 'NONE',  ( -2.569797478183790229, -12.44213550320647954, -7.701637110048636714 ) ) ;
#1244 = CARTESIAN_POINT ( 'NONE',  ( 2.359973842542475886, -36.16349720208508955, -25.10652036319019587 ) ) ;
#1245 = LINE ( 'NONE', #5931, #30257 ) ;
#1246 = CARTESIAN_POINT ( 'NONE',  ( 0.5980271706414734822, -45.25597162979979515, 19.07737599053966449 ) ) ;
#1247 = VERTEX_POINT ( 'NONE', #28214 ) ;
#1248 = CARTESIAN_POINT ( 'NONE',  ( -6.016761891674564211, 18.20201388312095503, 4.873659902332430960 ) ) ;
#1249 = CARTESIAN_POINT ( 'NONE',  ( 0.8557997880470697982, -41.02602466100796619, 24.73961900479237386 ) ) ;
#1250 = ORIENTED_EDGE ( 'NONE', *, *, #39355, .F. ) ;
#1251 = CARTESIAN_POINT ( 'NONE',  ( 4.960386119450149955, -43.42409617054094895, 5.365103581847332492 ) ) ;
#1252 = ORIENTED_EDGE ( 'NONE', *, *, #33947, .F. ) ;
#1253 = CARTESIAN_POINT ( 'NONE',  ( 0.000000000000000000, 0.000000000000000000, 0.000000000000000000 ) ) ;
#1254 = CARTESIAN_POINT ( 'NONE',  ( 4.960156602257181468, 30.22163187094385961, 35.23783291257178263 ) ) ;
#1255 = EDGE_LOOP ( 'NONE', ( #52868, #40210, #7155, #49299 ) ) ;
#1256 = DIRECTION ( 'NONE',  ( -0.07836865515943411409, 0.6993330359244963601, -0.7104869166656966328 ) ) ;
#1257 = CARTESIAN_POINT ( 'NONE',  ( 4.834790513006555379, -35.67803047646649617, 30.97850032271910692 ) ) ;
#1258 = CARTESIAN_POINT ( 'NONE',  ( 43.00000000000000000, -15.49999999999999645, -2.995852231480067093E-16 ) ) ;
#1259 = CARTESIAN_POINT ( 'NONE',  ( 0.8753041380234524160, -38.81339214172321306, 30.07754840949971609 ) ) ;
#1260 = EDGE_CURVE ( 'NONE', #26356, #29096, #28406, .T. ) ;
#1261 =( BOUNDED_SURFACE ( )  B_SPLINE_SURFACE ( 3, 1, ( 
 ( #23943, #43376 ),
 ( #19562, #4803 ),
 ( #734, #10776 ),
 ( #15169, #29554 ) ),
 .UNSPECIFIED., .F., .F., .F. ) 
 B_SPLINE_SURFACE_WITH_KNOTS ( ( 4, 4 ),
 ( 2, 2 ),
 ( 0.000000000000000000, 1.000000000000000000 ),
 ( 0.000000000000000000, 1.000000000000000000 ),
 .UNSPECIFIED. ) 
 GEOMETRIC_REPRESENTATION_ITEM ( )  RATIONAL_B_SPLINE_SURFACE ( (
 ( 1.000000000000000000, 1.000000000000000000),
 ( 0.9729067724841187204, 0.9999501103223794596),
 ( 0.9729067724841187204, 0.9999501103223794596),
 ( 1.000000000000000000, 1.000000000000000000) ) ) 
 REPRESENTATION_ITEM ( '' )  SURFACE ( )  );
#1262 = ORIENTED_EDGE ( 'NONE', *, *, #48309, .T. ) ;
#1263 = DIRECTION ( 'NONE',  ( -1.000000000000000000, -0.000000000000000000, -0.000000000000000000 ) ) ;
#1264 = EDGE_CURVE ( 'NONE', #57237, #10490, #61347, .T. ) ;
#1265 = CARTESIAN_POINT ( 'NONE',  ( 0.000000000000000000, 2.357898499370431722, -2.818925648462311528E-15 ) ) ;
#1266 = B_SPLINE_CURVE_WITH_KNOTS ( 'NONE', 3,
 ( #16711, #25173, #12033, #48986, #21096, #40536 ),
 .UNSPECIFIED., .F., .F.,
 ( 4, 2, 4 ),
 ( 3.576224061345498009E-18, 0.0002445244328975361555, 0.0004890488657950687332 ),
 .UNSPECIFIED. ) ;
#1267 = AXIS2_PLACEMENT_3D ( 'NONE', #56128, #32657, #60824 ) ;
#1268 = CARTESIAN_POINT ( 'NONE',  ( 4.549368137175248350, 0.000000000000000000, 0.000000000000000000 ) ) ;
#1269 = CARTESIAN_POINT ( 'NONE',  ( 5.860006189529234355, 15.52021937683276498, 45.66786516969934695 ) ) ;
#1270 = CARTESIAN_POINT ( 'NONE',  ( 2.643462169533613793, -38.93558293168521089, -28.13401304854706808 ) ) ;
#1271 = CARTESIAN_POINT ( 'NONE',  ( 0.6846871229502932144, 41.91507847151831356, -23.20185915381512842 ) ) ;
#1272 =( BOUNDED_SURFACE ( )  B_SPLINE_SURFACE ( 3, 1, ( 
 ( #30931, #2410 ),
 ( #60340, #17453 ),
 ( #36891, #60048 ),
 ( #40361, #21532 ) ),
 .UNSPECIFIED., .F., .F., .F. ) 
 B_SPLINE_SURFACE_WITH_KNOTS ( ( 4, 4 ),
 ( 2, 2 ),
 ( 0.000000000000000000, 1.000000000000000000 ),
 ( 0.000000000000000000, 1.000000000000000000 ),
 .UNSPECIFIED. ) 
 GEOMETRIC_REPRESENTATION_ITEM ( )  RATIONAL_B_SPLINE_SURFACE ( (
 ( 1.000000000000000000, 1.000000000000000000),
 ( 0.9953040768229005630, 0.8617119497784937465),
 ( 0.9953040768229005630, 0.8617119497784937465),
 ( 1.000000000000000000, 1.000000000000000000) ) ) 
 REPRESENTATION_ITEM ( '' )  SURFACE ( )  );
#1273 = CARTESIAN_POINT ( 'NONE',  ( 0.7764146366350237471, 46.59651770594938114, 5.367030030502223603 ) ) ;
#1274 = DIRECTION ( 'NONE',  ( -1.000000000000000000, -1.836909530733573776E-16, 1.925929944387235853E-32 ) ) ;
#1275 =( BOUNDED_SURFACE ( )  B_SPLINE_SURFACE ( 3, 1, ( 
 ( #32106, #12699 ),
 ( #40598, #7649 ),
 ( #17385, #59976 ),
 ( #31475, #44989 ) ),
 .UNSPECIFIED., .F., .F., .F. ) 
 B_SPLINE_SURFACE_WITH_KNOTS ( ( 4, 4 ),
 ( 2, 2 ),
 ( 0.000000000000000000, 1.000000000000000000 ),
 ( 0.000000000000000000, 1.000000000000000000 ),
 .UNSPECIFIED. ) 
 GEOMETRIC_REPRESENTATION_ITEM ( )  RATIONAL_B_SPLINE_SURFACE ( (
 ( 1.000000000000000000, 1.000000000000000000),
 ( 0.7211978278499970862, 0.9934217856018976445),
 ( 0.7211978278499970862, 0.9934217856018976445),
 ( 1.000000000000000000, 1.000000000000000000) ) ) 
 REPRESENTATION_ITEM ( '' )  SURFACE ( )  );
#1276 = CARTESIAN_POINT ( 'NONE',  ( 4.833616638992205949, -41.67905425467720448, 20.04871863793733056 ) ) ;
#1277 = ADVANCED_FACE ( 'NONE', ( #47039 ), #22875, .F. ) ;
#1278 = DIRECTION ( 'NONE',  ( -1.000000000000000000, -0.000000000000000000, -0.000000000000000000 ) ) ;
#1279 = CARTESIAN_POINT ( 'NONE',  ( 4.962356264823609919, 39.89814050050791394, -13.39305724859256763 ) ) ;
#1280 = CARTESIAN_POINT ( 'NONE',  ( 0.5809828226811556418, 44.45562576850601744, 17.82437196699697424 ) ) ;
#1281 = VECTOR ( 'NONE', #39244, 1000.000000000000114 ) ;
#1282 = CARTESIAN_POINT ( 'NONE',  ( 4.553261556744875094, -9.994631851593741345, 42.77437199977043036 ) ) ;
#1283 = CARTESIAN_POINT ( 'NONE',  ( -2.708315649062910779, 3.532515819624157505, 14.20182604343561295 ) ) ;
#1284 = ORIENTED_EDGE ( 'NONE', *, *, #49360, .T. ) ;
#1285 = CARTESIAN_POINT ( 'NONE',  ( -4.915099999999999802, 0.000000000000000000, 3.000000000000000000 ) ) ;
#1286 = CARTESIAN_POINT ( 'NONE',  ( 3.894904216938898323, 18.33300990194901559, -39.95028260740141945 ) ) ;
#1287 = DIRECTION ( 'NONE',  ( -1.000000000000000000, -0.000000000000000000, -0.000000000000000000 ) ) ;
#1288 = ORIENTED_EDGE ( 'NONE', *, *, #26094, .T. ) ;
#1289 = CARTESIAN_POINT ( 'NONE',  ( 0.5987334363312689645, -14.55165115253731756, 46.90215725536444324 ) ) ;
#1290 = CARTESIAN_POINT ( 'NONE',  ( 0.1139756605157203340, 4.632526725434476411, 43.88046166385626634 ) ) ;
#1291 = ORIENTED_EDGE ( 'NONE', *, *, #54153, .T. ) ;
#1292 = ORIENTED_EDGE ( 'NONE', *, *, #1379, .F. ) ;
#1293 = VERTEX_POINT ( 'NONE', #57019 ) ;
#1294 = CARTESIAN_POINT ( 'NONE',  ( 0.5997462898726536595, 10.41743419021273631, 47.98988117339838055 ) ) ;
#1295 = ORIENTED_EDGE ( 'NONE', *, *, #60687, .F. ) ;
#1296 = ORIENTED_EDGE ( 'NONE', *, *, #57741, .T. ) ;
#1297 = CARTESIAN_POINT ( 'NONE',  ( 4.967162193818130511, -42.16965968614187688, -8.839793687085657936 ) ) ;
#1298 = VERTEX_POINT ( 'NONE', #17914 ) ;
#1299 = LINE ( 'NONE', #19836, #50083 ) ;
#1300 = B_SPLINE_CURVE_WITH_KNOTS ( 'NONE', 3,
 ( #26354, #60468, #2540, #21662, #30425, #40803 ),
 .UNSPECIFIED., .F., .F.,
 ( 4, 2, 4 ),
 ( 1.519276763058329222E-16, 0.0002445252820015159914, 0.0004890505640028799776 ),
 .UNSPECIFIED. ) ;
#1301 = VECTOR ( 'NONE', #57417, 1000.000000000000114 ) ;
#1302 = ADVANCED_FACE ( 'NONE', ( #22602 ), #50133, .F. ) ;
#1303 = FACE_OUTER_BOUND ( 'NONE', #57037, .T. ) ;
#1304 = EDGE_LOOP ( 'NONE', ( #45179, #2061, #25588, #25077 ) ) ;
#1305 = CARTESIAN_POINT ( 'NONE',  ( 4.967162193818130511, -42.16965968614200477, 8.839793687085075291 ) ) ;
#1306 = CARTESIAN_POINT ( 'NONE',  ( 3.238931869106854489, 41.01619136531527232, -12.88361013339121008 ) ) ;
#1307 = ORIENTED_EDGE ( 'NONE', *, *, #52182, .F. ) ;
#1308 = ADVANCED_FACE ( 'NONE', ( #34786, #1238 ), #48554, .F. ) ;
#1309 = VERTEX_POINT ( 'NONE', #38568 ) ;
#1310 = CARTESIAN_POINT ( 'NONE',  ( 0.3676999524040323597, -17.09834788623527047, -40.66444494744902727 ) ) ;
#1311 = CARTESIAN_POINT ( 'NONE',  ( 4.956445790444022670, -4.175462451061590308, -46.90526157542895191 ) ) ;
#1312 = CARTESIAN_POINT ( 'NONE',  ( 0.5806925824938499181, -14.41498975133639426, 44.62544602368059543 ) ) ;
#1313 = CARTESIAN_POINT ( 'NONE',  ( 0.5998501479064699549, 12.95623334615437550, 46.33007877220744319 ) ) ;
#1314 = CIRCLE ( 'NONE', #36387, 0.02570000000000176310 ) ;
#1315 = VERTEX_POINT ( 'NONE', #5004 ) ;
#1316 = CARTESIAN_POINT ( 'NONE',  ( 0.6017666602106489515, -12.11361215600212304, 46.55749120190025536 ) ) ;
#1317 = CARTESIAN_POINT ( 'NONE',  ( 1.227938101723756947, 41.23019537246726429, -11.92353943227906399 ) ) ;
#1318 = CARTESIAN_POINT ( 'NONE',  ( 4.956445790444041322, 46.03642002599030292, -9.908889005849065512 ) ) ;
#1319 = CARTESIAN_POINT ( 'NONE',  ( 4.834790513006553603, 7.085748555637120916, 46.71596631057383320 ) ) ;
#1320 = VERTEX_POINT ( 'NONE', #5610 ) ;
#1321 = CARTESIAN_POINT ( 'NONE',  ( 5.960221823109900008, 14.50993159119790654, 14.51763960716783508 ) ) ;
#1322 = LINE ( 'NONE', #16078, #26277 ) ;
#1323 = CARTESIAN_POINT ( 'NONE',  ( 2.185380717157383135, 8.390375351159853778, -43.22524036409571124 ) ) ;
#1324 = CARTESIAN_POINT ( 'NONE',  ( 2.299652685299201860, -29.55407244308045023, -39.12593164241979338 ) ) ;
#1325 = EDGE_CURVE ( 'NONE', #18038, #2711, #15080, .T. ) ;
#1326 = ORIENTED_EDGE ( 'NONE', *, *, #58268, .T. ) ;
#1327 = ORIENTED_EDGE ( 'NONE', *, *, #14501, .F. ) ;
#1328 = CARTESIAN_POINT ( 'NONE',  ( 0.9787284016396621267, -39.65084253017462146, -13.57006579114940870 ) ) ;
#1329 = CARTESIAN_POINT ( 'NONE',  ( -2.708315649062916552, 11.76894112707800844, 8.698422600177160291 ) ) ;
#1330 = EDGE_CURVE ( 'NONE', #4316, #49088, #60568, .T. ) ;
#1331 = CARTESIAN_POINT ( 'NONE',  ( 0.9780106845699487739, 15.35453589240238870, -38.99448004505720178 ) ) ;
#1332 = CARTESIAN_POINT ( 'NONE',  ( 1.088908134280556439, -33.56490895818185294, 26.73890361625902301 ) ) ;
#1333 = CARTESIAN_POINT ( 'NONE',  ( 0.1081432562775997974, 34.46918062033751085, -25.91533557232854790 ) ) ;
#1334 = EDGE_CURVE ( 'NONE', #1876, #16670, #3758, .T. ) ;
#1335 = CARTESIAN_POINT ( 'NONE',  ( 0.1064266418746775689, -43.12102053154801951, -0.5615180042399171567 ) ) ;
#1336 = CARTESIAN_POINT ( 'NONE',  ( 0.9788927965476035276, 9.577372930391250705, -40.79963897369664494 ) ) ;
#1337 = CARTESIAN_POINT ( 'NONE',  ( 4.967162193818130511, 32.68434214048205888, -28.07411493385260925 ) ) ;
#1338 = CARTESIAN_POINT ( 'NONE',  ( 0.5980894510889457338, 37.73932204245519273, -29.84264441023739067 ) ) ;
#1339 = CARTESIAN_POINT ( 'NONE',  ( 0.6031357023905875581, -18.36962560204189288, -44.46217339385164280 ) ) ;
#1340 = CARTESIAN_POINT ( 'NONE',  ( 5.959547316686252039, -14.51128755440531393, -14.51632612601523853 ) ) ;
#1341 = CARTESIAN_POINT ( 'NONE',  ( 0.1145239942831223490, -6.719625162407512953, -43.60954159792800056 ) ) ;
#1342 = LINE ( 'NONE', #2271, #20424 ) ;
#1343 = FACE_OUTER_BOUND ( 'NONE', #51667, .T. ) ;
#1344 = EDGE_CURVE ( 'NONE', #29077, #21542, #47180, .T. ) ;
#1345 = B_SPLINE_CURVE_WITH_KNOTS ( 'NONE', 3,
 ( #57704, #14835, #53023, #10123, #29219, #5397 ),
 .UNSPECIFIED., .F., .F.,
 ( 4, 2, 4 ),
 ( 0.000000000000000000, 0.0002291966416970784280, 0.0004583932833941568559 ),
 .UNSPECIFIED. ) ;
#1346 = CARTESIAN_POINT ( 'NONE',  ( 0.8557997880470606944, -17.48760788519184217, -44.60232077416704755 ) ) ;
#1347 = AXIS2_PLACEMENT_3D ( 'NONE', #12331, #7917, #59917 ) ;
#1348 = CARTESIAN_POINT ( 'NONE',  ( 4.967162193818130511, 35.57684288742009215, -24.30453456948074376 ) ) ;
#1349 = CARTESIAN_POINT ( 'NONE',  ( -4.915099999999998914, 9.539392014169456147, -3.000000000000000000 ) ) ;
#1350 = CARTESIAN_POINT ( 'NONE',  ( 0.2285344041767098378, 44.07067438182842523, 2.068049763982732880 ) ) ;
#1351 =( BOUNDED_SURFACE ( )  B_SPLINE_SURFACE ( 3, 1, ( 
 ( #7117, #26244 ),
 ( #58274, #10697 ),
 ( #48589, #24163 ),
 ( #38918, #337 ) ),
 .UNSPECIFIED., .F., .F., .F. ) 
 B_SPLINE_SURFACE_WITH_KNOTS ( ( 4, 4 ),
 ( 2, 2 ),
 ( 0.000000000000000000, 1.000000000000000000 ),
 ( 0.000000000000000000, 1.000000000000000000 ),
 .UNSPECIFIED. ) 
 GEOMETRIC_REPRESENTATION_ITEM ( )  RATIONAL_B_SPLINE_SURFACE ( (
 ( 1.000000000000000000, 1.000000000000000000),
 ( 0.9953390228620291325, 0.8624445117760984880),
 ( 0.9953390228620291325, 0.8624445117760984880),
 ( 1.000000000000000000, 1.000000000000000000) ) ) 
 REPRESENTATION_ITEM ( '' )  SURFACE ( )  );
#1352 = CARTESIAN_POINT ( 'NONE',  ( 0.9752570700956798566, -11.32817567195941777, 41.38610171411356475 ) ) ;
#1353 = CARTESIAN_POINT ( 'NONE',  ( 0.5988103622719989083, -47.61318311633120004, -6.880137819454693826 ) ) ;
#1354 = CARTESIAN_POINT ( 'NONE',  ( 1.157644175074339365, -27.68781125088666428, 31.47042077275824568 ) ) ;
#1356 = ORIENTED_EDGE ( 'NONE', *, *, #44945, .F. ) ;
#1355 = CARTESIAN_POINT ( 'NONE',  ( 0.09136607875274982415, 0.000000000000000000, -3.000000000000000000 ) ) ;
#1357 = VERTEX_POINT ( 'NONE', #29143 ) ;
#1358 = FACE_OUTER_BOUND ( 'NONE', #43017, .T. ) ;
#1359 = CARTESIAN_POINT ( 'NONE',  ( 1.296416391601052265, 43.89588502411658766, -3.931749232300615571 ) ) ;
#1360 = CARTESIAN_POINT ( 'NONE',  ( 0.1139756605157203201, 42.00001770421683744, 13.52603905585425714 ) ) ;
#1361 = VERTEX_POINT ( 'NONE', #29753 ) ;
#1362 = EDGE_LOOP ( 'NONE', ( #20699, #3409, #36647, #9267 ) ) ;
#1363 = LINE ( 'NONE', #40872, #18313 ) ;
#1364 = CARTESIAN_POINT ( 'NONE',  ( 4.549368137175248350, -13.99871866169391765, 40.58005590356665948 ) ) ;
#1365 = CARTESIAN_POINT ( 'NONE',  ( 2.648799415243708655, 48.37728179772441450, 8.009748382637324582 ) ) ;
#1366 = VERTEX_POINT ( 'NONE', #39498 ) ;
#1367 = ORIENTED_EDGE ( 'NONE', *, *, #20893, .F. ) ;
#1368 = FACE_OUTER_BOUND ( 'NONE', #44704, .T. ) ;
#1369 = EDGE_CURVE ( 'NONE', #23520, #22992, #25078, .T. ) ;
#1370 = CARTESIAN_POINT ( 'NONE',  ( 1.227938101723747621, 6.439911493065174852, -42.43379953535178828 ) ) ;
#1371 = CARTESIAN_POINT ( 'NONE',  ( -6.079354080745853928, -12.94495173828262047, 14.25556662296156496 ) ) ;
#1372 = CARTESIAN_POINT ( 'NONE',  ( 1.227938101723748288, 41.23019537246709376, 11.92353943227963597 ) ) ;
#1373 = EDGE_CURVE ( 'NONE', #30313, #7742, #20985, .T. ) ;
#1374 = CARTESIAN_POINT ( 'NONE',  ( 0.7954190325252775695, 19.20649988843056732, 44.09776758977478295 ) ) ;
#1375 = ADVANCED_FACE ( 'NONE', ( #304 ), #29263, .F. ) ;
#1376 = CARTESIAN_POINT ( 'NONE',  ( 0.5980271706414711508, -13.30134363210393644, -47.27709276618382006 ) ) ;
#1377 = CARTESIAN_POINT ( 'NONE',  ( -6.016104459813371719, -7.206059014950207064, 17.41090761020834066 ) ) ;
#1378 = EDGE_LOOP ( 'NONE', ( #17663, #16734, #24499, #56689 ) ) ;
#1379 = EDGE_CURVE ( 'NONE', #46207, #45900, #10564, .T. ) ;
#1380 = B_SPLINE_CURVE_WITH_KNOTS ( 'NONE', 3,
 ( #57058, #23875, #33291, #47371, #13877, #28257 ),
 .UNSPECIFIED., .F., .F.,
 ( 4, 2, 4 ),
 ( 0.000000000000000000, 0.0002291966416970781298, 0.0004583932833941562596 ),
 .UNSPECIFIED. ) ;
#1381 = EDGE_LOOP ( 'NONE', ( #46301, #55090, #25849, #33963 ) ) ;
#1382 = CARTESIAN_POINT ( 'NONE',  ( 4.962356264823603702, 37.36413190407388640, -19.36897635181878030 ) ) ;
#1383 = CARTESIAN_POINT ( 'NONE',  ( -5.995132425357893702, -9.414704407577689338, -16.32377331145330501 ) ) ;
#1384 = ORIENTED_EDGE ( 'NONE', *, *, #50407, .F. ) ;
#1385 = CARTESIAN_POINT ( 'NONE',  ( 4.960156602257185909, -30.99165383632742277, -34.56254177294303531 ) ) ;
#1386 = CARTESIAN_POINT ( 'NONE',  ( 0.6008123274975393224, -8.267100005214324199, 48.40671036811161088 ) ) ;
#1387 = DIRECTION ( 'NONE',  ( 0.000000000000000000, 0.000000000000000000, 1.000000000000000000 ) ) ;
#1388 = CARTESIAN_POINT ( 'NONE',  ( 0.6845945791218023269, -8.654967045697796735, -46.10312425586610630 ) ) ;
#1389 = VECTOR ( 'NONE', #52131, 1000.000000000000114 ) ;
#1390 = ORIENTED_EDGE ( 'NONE', *, *, #12134, .F. ) ;
#1391 = CARTESIAN_POINT ( 'NONE',  ( 0.5817217712918331118, -14.32834839058178389, 44.65348123502227651 ) ) ;
#1392 = DIRECTION ( 'NONE',  ( 0.000000000000000000, 0.000000000000000000, 1.000000000000000000 ) ) ;
#1393 = CARTESIAN_POINT ( 'NONE',  ( 4.958415959904820092, 43.07243048339554292, -14.42115411732696195 ) ) ;
#1394 = CARTESIAN_POINT ( 'NONE',  ( 4.963659409799330291, 13.93274247732021287, 42.53037318521000287 ) ) ;
#1395 = VERTEX_POINT ( 'NONE', #57936 ) ;
#1396 = DIRECTION ( 'NONE',  ( 1.000000000000000000, 1.836909530733573776E-16, 0.000000000000000000 ) ) ;
#1397 = CARTESIAN_POINT ( 'NONE',  ( 5.896782393890504181, 10.81700609697900894, -16.95636948099241792 ) ) ;
#1398 = VERTEX_POINT ( 'NONE', #34168 ) ;
#1399 = FACE_BOUND ( 'NONE', #17286, .T. ) ;
#1400 = CARTESIAN_POINT ( 'NONE',  ( 0.1154773475650540393, 9.993826709811125752, 42.97751805002688741 ) ) ;
#1401 = EDGE_CURVE ( 'NONE', #59975, #52610, #57565, .T. ) ;
#1402 = ORIENTED_EDGE ( 'NONE', *, *, #22563, .F. ) ;
#1403 = CARTESIAN_POINT ( 'NONE',  ( 1.231276596079887264, -13.22565419921979313, -39.77887431816952102 ) ) ;
#1404 = EDGE_CURVE ( 'NONE', #41574, #37380, #46122, .T. ) ;
#1405 = CARTESIAN_POINT ( 'NONE',  ( 0.6027935024548037868, -47.71838037711337677, 6.106197519200678769 ) ) ;
#1406 = CARTESIAN_POINT ( 'NONE',  ( 0.1129192098497455998, -42.55567333040708888, -11.66046547873770756 ) ) ;
#1407 = MECHANICAL_DESIGN_GEOMETRIC_PRESENTATION_REPRESENTATION (  '', ( #54392 ), #17442 ) ;
#1408 = EDGE_CURVE ( 'NONE', #2552, #57258, #32199, .T. ) ;
#1409 = CARTESIAN_POINT ( 'NONE',  ( -6.072942160501519027, -19.21577577016805094, -1.248248308487848401 ) ) ;
#1410 = CARTESIAN_POINT ( 'NONE',  ( 4.956653778116966613, 0.000000000000000000, 0.000000000000000000 ) ) ;
#1411 = CARTESIAN_POINT ( 'NONE',  ( 1.296416391601052265, 21.36356421792644511, 38.54744476593347002 ) ) ;
#1412 = CARTESIAN_POINT ( 'NONE',  ( 0.5809828226811553087, 46.11980934799357357, -12.92184523170154620 ) ) ;
#1413 = CARTESIAN_POINT ( 'NONE',  ( 3.238741278300274917, -9.350673766180513269, -41.96285461600078293 ) ) ;
#1414 = VERTEX_POINT ( 'NONE', #55901 ) ;
#1415 = CARTESIAN_POINT ( 'NONE',  ( 0.9754642270333692133, 39.70914670678655511, -16.25787253057890425 ) ) ;
#1416 = CARTESIAN_POINT ( 'NONE',  ( 0.9775691876210979014, 41.48266884170315194, 5.960024728101428693 ) ) ;
#1417 = CARTESIAN_POINT ( 'NONE',  ( 0.7948884756798506590, 33.64624544102139225, -35.75791957486759998 ) ) ;
#1418 = EDGE_LOOP ( 'NONE', ( #55748, #32684, #10445, #30814 ) ) ;
#1419 = CARTESIAN_POINT ( 'NONE',  ( 0.8551540677456739292, 34.52115452272974494, -33.23105123575864894 ) ) ;
#1420 = CARTESIAN_POINT ( 'NONE',  ( 0.6000166863083106206, 37.05402083933981316, -32.23077754796219807 ) ) ;
#1421 = CARTESIAN_POINT ( 'NONE',  ( 0.5987334308729317378, 48.96426922180645391, -3.750099484572206432 ) ) ;
#1422 = CARTESIAN_POINT ( 'NONE',  ( 0.5980271706414734822, 5.412294693954527780, 48.81348490926923489 ) ) ;
#1423 = EDGE_CURVE ( 'NONE', #16132, #8543, #39641, .T. ) ;
#1424 = LINE ( 'NONE', #15869, #46163 ) ;
#1425 = CARTESIAN_POINT ( 'NONE',  ( 0.9730545539215883499, 41.31259007387247095, -11.59290486963463351 ) ) ;
#1426 = CARTESIAN_POINT ( 'NONE',  ( 0.000000000000000000, 0.000000000000000000, 0.000000000000000000 ) ) ;
#1427 = CARTESIAN_POINT ( 'NONE',  ( 4.691466044806103852, -29.64918311951105778, -33.30232861642423359 ) ) ;
#1428 = ADVANCED_FACE ( 'NONE', ( #13320 ), #35699, .F. ) ;
#1429 = VECTOR ( 'NONE', #5050, 1000.000000000000114 ) ;
#1430 = DIRECTION ( 'NONE',  ( 0.000000000000000000, 0.000000000000000000, -1.000000000000000000 ) ) ;
#1431 = CARTESIAN_POINT ( 'NONE',  ( 0.1064266418746773746, -6.185136754498649303, 42.67882141624135528 ) ) ;
#1433 = EDGE_LOOP ( 'NONE', ( #37109, #26749, #12228, #28663 ) ) ;
#1432 = CARTESIAN_POINT ( 'NONE',  ( 0.8560838555295223751, -29.58154842764516701, 36.40473632241573654 ) ) ;
#1434 = ORIENTED_EDGE ( 'NONE', *, *, #19326, .F. ) ;
#1435 = CARTESIAN_POINT ( 'NONE',  ( 4.694002226626921015, -4.034398983147713835, 45.40934261020424856 ) ) ;
#1436 = CARTESIAN_POINT ( 'NONE',  ( 5.959547316686252039, -16.28624005235090877, -12.49238070347970364 ) ) ;
#1437 = B_SPLINE_CURVE_WITH_KNOTS ( 'NONE', 3,
 ( #47295, #47008, #4042, #17876 ),
 .UNSPECIFIED., .F., .F.,
 ( 4, 4 ),
 ( 0.000000000000000000, 0.005013413432710148512 ),
 .UNSPECIFIED. ) ;
#1438 = CARTESIAN_POINT ( 'NONE',  ( 4.956445790443988919, 44.65954324082213134, 14.93530206124989945 ) ) ;
#1439 = CARTESIAN_POINT ( 'NONE',  ( 2.526464513654346433, -42.43615126908562729, 6.809833384818880120 ) ) ;
#1440 = CARTESIAN_POINT ( 'NONE',  ( 0.8557997880470606944, -11.51622788066425684, -46.50333260518571876 ) ) ;
#1441 = EDGE_LOOP ( 'NONE', ( #60485, #13982, #14945, #61799 ) ) ;
#1442 = ORIENTED_EDGE ( 'NONE', *, *, #24398, .F. ) ;
#1443 = CARTESIAN_POINT ( 'NONE',  ( 3.782625744892851749, 30.43998245888566245, 28.99388852840778341 ) ) ;
#1445 = CARTESIAN_POINT ( 'NONE',  ( -2.500000000000000444, 3.061616997868384127E-16, 3.469446951953614189E-15 ) ) ;
#1444 = AXIS2_PLACEMENT_3D ( 'NONE', #21886, #41315, #26887 ) ;
#1446 = CARTESIAN_POINT ( 'NONE',  ( 0.5997462898726536595, 37.72933316221968170, 31.43324751403423534 ) ) ;
#1447 = EDGE_LOOP ( 'NONE', ( #2708, #42694, #34709, #41037 ) ) ;
#1448 = EDGE_CURVE ( 'NONE', #42568, #34245, #40424, .T. ) ;
#1449 = AXIS2_PLACEMENT_3D ( 'NONE', #48895, #15398, #34502 ) ;
#1450 = EDGE_CURVE ( 'NONE', #1988, #10608, #40149, .T. ) ;
#1451 = B_SPLINE_CURVE_WITH_KNOTS ( 'NONE', 3,
 ( #29436, #58233, #61695, #38560, #48254, #29136 ),
 .UNSPECIFIED., .F., .F.,
 ( 4, 2, 4 ),
 ( 1.870559545977334001E-17, 0.0002293319059085109570, 0.0004586638118170032114 ),
 .UNSPECIFIED. ) ;
#1452 = CARTESIAN_POINT ( 'NONE',  ( 0.1073791018717483448, 37.10214135362888754, -21.98088480513627729 ) ) ;
#1453 = CARTESIAN_POINT ( 'NONE',  ( 4.303969348037258058, 48.06163817123226067, -2.158280495710381608 ) ) ;
#1454 = EDGE_LOOP ( 'NONE', ( #41993, #42412, #46073, #34853 ) ) ;
#1455 = CARTESIAN_POINT ( 'NONE',  ( 0.5809828226811548646, -46.40184912890831015, -11.86925843957216742 ) ) ;
#1456 = ORIENTED_EDGE ( 'NONE', *, *, #1817, .F. ) ;
#1457 = EDGE_CURVE ( 'NONE', #27177, #27976, #6745, .T. ) ;
#1458 = EDGE_CURVE ( 'NONE', #22677, #21051, #43417, .T. ) ;
#1459 = CARTESIAN_POINT ( 'NONE',  ( 0.9762797500689124330, 4.697980241569248427, -41.64437257103928403 ) ) ;
#1460 = DIRECTION ( 'NONE',  ( -0.1736481776669314137, 0.9848077530122079093, -5.551115123125779004E-17 ) ) ;
#1461 = EDGE_LOOP ( 'NONE', ( #5875, #47255, #11594, #58640 ) ) ;
#1462 = CARTESIAN_POINT ( 'NONE',  ( 0.8554163680231816613, 40.82560365045065254, 23.11872746688558067 ) ) ;
#1463 = ADVANCED_FACE ( 'NONE', ( #56515 ), #12099, .F. ) ;
#1464 = CARTESIAN_POINT ( 'NONE',  ( 4.303969348037258058, -27.54579249306236832, 39.44373910178601506 ) ) ;
#1465 = CARTESIAN_POINT ( 'NONE',  ( -2.678494666091065124, -3.072372537026387018, -5.565789719053451101 ) ) ;
#1466 = VERTEX_POINT ( 'NONE', #41840 ) ;
#1467 = DIRECTION ( 'NONE',  ( -0.1024043820194934507, -0.01315135725336535714, 0.9946559125373960475 ) ) ;
#1468 = DIRECTION ( 'NONE',  ( 1.000000000000000000, 0.000000000000000000, 0.000000000000000000 ) ) ;
#1469 = ORIENTED_EDGE ( 'NONE', *, *, #537, .F. ) ;
#1470 = CARTESIAN_POINT ( 'NONE',  ( 0.3622758884714730732, -34.70015533914812522, -25.58609868863756276 ) ) ;
#1471 = VECTOR ( 'NONE', #19350, 1000.000000000000114 ) ;
#1472 = EDGE_CURVE ( 'NONE', #22620, #59460, #15009, .T. ) ;
#1473 =( BOUNDED_SURFACE ( )  B_SPLINE_SURFACE ( 3, 1, ( 
 ( #21443, #31457 ),
 ( #50556, #7633 ),
 ( #26758, #50866 ),
 ( #12997, #22682 ) ),
 .UNSPECIFIED., .F., .F., .F. ) 
 B_SPLINE_SURFACE_WITH_KNOTS ( ( 4, 4 ),
 ( 2, 2 ),
 ( 0.000000000000000000, 1.000000000000000000 ),
 ( 0.000000000000000000, 1.000000000000000000 ),
 .UNSPECIFIED. ) 
 GEOMETRIC_REPRESENTATION_ITEM ( )  RATIONAL_B_SPLINE_SURFACE ( (
 ( 1.000000000000000000, 1.000000000000000000),
 ( 0.9953390228620291325, 0.8624445117760984880),
 ( 0.9953390228620291325, 0.8624445117760984880),
 ( 1.000000000000000000, 1.000000000000000000) ) ) 
 REPRESENTATION_ITEM ( '' )  SURFACE ( )  );
#1474 = ORIENTED_EDGE ( 'NONE', *, *, #15088, .T. ) ;
#1475 = CARTESIAN_POINT ( 'NONE',  ( 0.9968887458511658251, -36.82760690604611398, -22.02152923727788902 ) ) ;
#1476 = VERTEX_POINT ( 'NONE', #3264 ) ;
#1477 = CARTESIAN_POINT ( 'NONE',  ( 3.407937589446178528, -11.14158115674367799, -7.970324840162072988 ) ) ;
#1478 = CARTESIAN_POINT ( 'NONE',  ( 0.6016118706126978299, -30.34494265132144619, -38.61004416304056974 ) ) ;
#1479 = CARTESIAN_POINT ( 'NONE',  ( -4.000000000000000000, -2.309401076758531346, -0.3572655899081733644 ) ) ;
#1480 = ORIENTED_EDGE ( 'NONE', *, *, #24999, .F. ) ;
#1481 = CARTESIAN_POINT ( 'NONE',  ( 0.6041374136657475802, -18.57118264377566774, 44.37863742124635991 ) ) ;
#1482 = CARTESIAN_POINT ( 'NONE',  ( 3.238018933889920792, 5.069615556373155307, 12.39784217024205759 ) ) ;
#1483 = B_SPLINE_CURVE_WITH_KNOTS ( 'NONE', 3,
 ( #61942, #14069, #14371, #9651 ),
 .UNSPECIFIED., .F., .F.,
 ( 4, 4 ),
 ( 1.551583845779545699E-17, 0.005004741218457429280 ),
 .UNSPECIFIED. ) ;
#1484 = FACE_OUTER_BOUND ( 'NONE', #30690, .T. ) ;
#1485 = ORIENTED_EDGE ( 'NONE', *, *, #15585, .F. ) ;
#1486 = EDGE_LOOP ( 'NONE', ( #50446, #50345, #15384, #23586 ) ) ;
#1487 = CARTESIAN_POINT ( 'NONE',  ( 0.5819845901640493535, 17.90867915372053432, 44.42187107932949885 ) ) ;
#1488 = CARTESIAN_POINT ( 'NONE',  ( 1.154321713695928286, -42.90848032340444718, -0.8253077511131137189 ) ) ;
#1489 = CARTESIAN_POINT ( 'NONE',  ( 4.963659409799332067, 29.86601237216454052, -33.33129552235055115 ) ) ;
#1490 = CARTESIAN_POINT ( 'NONE',  ( 0.1073791018717578927, 30.14884492832347718, 30.83464511437148659 ) ) ;
#1491 = CARTESIAN_POINT ( 'NONE',  ( 0.9789233960466698914, -26.95685022293044142, -32.08839280629113944 ) ) ;
#1493 = VECTOR ( 'NONE', #30697, 1000.000000000000114 ) ;
#1492 = CARTESIAN_POINT ( 'NONE',  ( 2.643462169533600914, 4.896978544601506833, 47.78621045426877600 ) ) ;
#1494 = VERTEX_POINT ( 'NONE', #60587 ) ;
#1495 = DIRECTION ( 'NONE',  ( -0.1736481776669314137, 0.9848077530122077983, -5.551115123125779004E-17 ) ) ;
#1496 = ORIENTED_EDGE ( 'NONE', *, *, #49753, .T. ) ;
#1497 = VECTOR ( 'NONE', #54986, 1000.000000000000000 ) ;
#1498 = CARTESIAN_POINT ( 'NONE',  ( 0.2285344041767113921, -38.80901244121420035, -20.98479744084123766 ) ) ;
#1499 = FACE_OUTER_BOUND ( 'NONE', #22375, .T. ) ;
#1500 = CIRCLE ( 'NONE', #4484, 42.08604991992415023 ) ;
#1501 = CARTESIAN_POINT ( 'NONE',  ( 4.975610109902397937, 47.16372689271670993, -12.96272628450527264 ) ) ;
#1502 = CARTESIAN_POINT ( 'NONE',  ( 0.8557997880470599172, -47.60865952217002928, 5.347802024197076065 ) ) ;
#1503 = CARTESIAN_POINT ( 'NONE',  ( 3.390910168358336474, 11.69695288386326837, 42.39432072537923801 ) ) ;
#1504 = CARTESIAN_POINT ( 'NONE',  ( 5.895881250540457863, -13.98558879082075634, -14.45444526027788434 ) ) ;
#1505 = ADVANCED_FACE ( 'NONE', ( #36831 ), #7660, .F. ) ;
#1506 = CARTESIAN_POINT ( 'NONE',  ( 0.6008123274975391004, 37.67355407045358362, -31.50012499751496264 ) ) ;
#1507 = CARTESIAN_POINT ( 'NONE',  ( 0.8744876279028263033, 11.79038800009220722, -47.65854384249244191 ) ) ;
#1508 = B_SPLINE_CURVE_WITH_KNOTS ( 'NONE', 3,
 ( #20044, #10634, #5889, #33522 ),
 .UNSPECIFIED., .F., .F.,
 ( 4, 4 ),
 ( 0.000000000000000000, 0.004442905043737215703 ),
 .UNSPECIFIED. ) ;
#1509 = CARTESIAN_POINT ( 'NONE',  ( 0.8744876279028306332, -29.90976330662902427, 38.93271258621624042 ) ) ;
#1510 = CARTESIAN_POINT ( 'NONE',  ( -2.708315649062910779, -9.116606751444415124, 11.44805714186556322 ) ) ;
#1511 = CARTESIAN_POINT ( 'NONE',  ( 0.2285344041767106982, -17.16127025498933634, 40.64470412649936293 ) ) ;
#1512 = CARTESIAN_POINT ( 'NONE',  ( -6.001507490154110336, -18.19774963328911710, 4.892199142591239891 ) ) ;
#1513 = FACE_OUTER_BOUND ( 'NONE', #8620, .T. ) ;
#1514 = LINE ( 'NONE', #25648, #36695 ) ;
#1515 = ORIENTED_EDGE ( 'NONE', *, *, #29580, .T. ) ;
#1516 = DIRECTION ( 'NONE',  ( 0.000000000000000000, 0.000000000000000000, 1.000000000000000000 ) ) ;
#1517 = CARTESIAN_POINT ( 'NONE',  ( -6.063463321072276813, 5.464110623310199699, -18.46520911269890064 ) ) ;
#1518 = CARTESIAN_POINT ( 'NONE',  ( 5.965394784446460541, 20.35165389555757898, -2.664747781315902841 ) ) ;
#1519 = CARTESIAN_POINT ( 'NONE',  ( 1.227938101723748288, -33.52879263017845091, -26.79402671879361364 ) ) ;
#1520 = CARTESIAN_POINT ( 'NONE',  ( 5.896278296736517710, -17.30792457686182573, 10.24513184180886682 ) ) ;
#1521 = ORIENTED_EDGE ( 'NONE', *, *, #31367, .F. ) ;
#1522 = CARTESIAN_POINT ( 'NONE',  ( 5.965394784446460541, 16.29267539192343150, -12.48356622107660030 ) ) ;
#1523 = CARTESIAN_POINT ( 'NONE',  ( 0.9758171775293911221, 16.41489794146178838, -39.64453667157730621 ) ) ;
#1524 = ADVANCED_FACE ( 'NONE', ( #28629 ), #5280, .F. ) ;
#1525 =( BOUNDED_SURFACE ( )  B_SPLINE_SURFACE ( 3, 1, ( 
 ( #60113, #36961 ),
 ( #55099, #54787 ),
 ( #22532, #12223 ),
 ( #13144, #41351 ) ),
 .UNSPECIFIED., .F., .F., .F. ) 
 B_SPLINE_SURFACE_WITH_KNOTS ( ( 4, 4 ),
 ( 2, 2 ),
 ( 0.000000000000000000, 1.000000000000000000 ),
 ( 0.000000000000000000, 1.000000000000000000 ),
 .UNSPECIFIED. ) 
 GEOMETRIC_REPRESENTATION_ITEM ( )  RATIONAL_B_SPLINE_SURFACE ( (
 ( 1.000000000000000000, 1.000000000000000000),
 ( 0.7211978278499968642, 0.9934217856018975334),
 ( 0.7211978278499968642, 0.9934217856018975334),
 ( 1.000000000000000000, 1.000000000000000000) ) ) 
 REPRESENTATION_ITEM ( '' )  SURFACE ( )  );
#1526 = CARTESIAN_POINT ( 'NONE',  ( 0.6008122571543326185, -13.55447923524773302, 47.19990088047383381 ) ) ;
#1527 = VERTEX_POINT ( 'NONE', #10151 ) ;
#1528 = CARTESIAN_POINT ( 'NONE',  ( 0.5549461598389365813, -44.09588694354911098, 0.8777528858055476668 ) ) ;
#1529 = AXIS2_PLACEMENT_3D ( 'NONE', #38802, #53468, #57859 ) ;
#1530 = EDGE_CURVE ( 'NONE', #7607, #11343, #58340, .T. ) ;
#1531 = CARTESIAN_POINT ( 'NONE',  ( 4.962356264823608143, -36.43094049105388166, 21.07183363638861096 ) ) ;
#1532 = VERTEX_POINT ( 'NONE', #14253 ) ;
#1533 = ADVANCED_FACE ( 'NONE', ( #29246 ), #1261, .F. ) ;
#1534 = CARTESIAN_POINT ( 'NONE',  ( 5.860006189529246790, -3.137522369585184823, -48.13093674595588567 ) ) ;
#1535 = VECTOR ( 'NONE', #49234, 1000.000000000000000 ) ;
#1536 = ORIENTED_EDGE ( 'NONE', *, *, #14661, .T. ) ;
#1537 = FACE_OUTER_BOUND ( 'NONE', #43813, .T. ) ;
#1538 = EDGE_CURVE ( 'NONE', #30127, #16034, #13558, .T. ) ;
#1539 = ORIENTED_EDGE ( 'NONE', *, *, #10760, .T. ) ;
#1540 = CARTESIAN_POINT ( 'NONE',  ( 0.1156495703730067853, 29.56366858242225604, -32.75564765318752336 ) ) ;
#1541 = LINE ( 'NONE', #49478, #29332 ) ;
#1542 = VERTEX_POINT ( 'NONE', #53049 ) ;
#1543 = CIRCLE ( 'NONE', #53547, 43.92652462719577500 ) ;
#1544 = ORIENTED_EDGE ( 'NONE', *, *, #24999, .T. ) ;
#1545 = CARTESIAN_POINT ( 'NONE',  ( 0.9788927965476030835, 20.01615798422175985, -36.81969625326166096 ) ) ;
#1546 = CARTESIAN_POINT ( 'NONE',  ( -6.078726893082806448, 17.85000270430361269, -7.222980321520601876 ) ) ;
#1547 =( BOUNDED_SURFACE ( )  B_SPLINE_SURFACE ( 3, 1, ( 
 ( #61067, #18804 ),
 ( #3740, #18180 ),
 ( #37928, #3133 ),
 ( #55750, #22261 ) ),
 .UNSPECIFIED., .F., .F., .F. ) 
 B_SPLINE_SURFACE_WITH_KNOTS ( ( 4, 4 ),
 ( 2, 2 ),
 ( 0.000000000000000000, 1.000000000000000000 ),
 ( 0.000000000000000000, 1.000000000000000000 ),
 .UNSPECIFIED. ) 
 GEOMETRIC_REPRESENTATION_ITEM ( )  RATIONAL_B_SPLINE_SURFACE ( (
 ( 1.000000000000000000, 1.000000000000000000),
 ( 0.7282232189291693025, 0.9929344683865674037),
 ( 0.7282232189291693025, 0.9929344683865674037),
 ( 1.000000000000000000, 1.000000000000000000) ) ) 
 REPRESENTATION_ITEM ( '' )  SURFACE ( )  );
#1548 = VERTEX_POINT ( 'NONE', #58345 ) ;
#1549 = ORIENTED_EDGE ( 'NONE', *, *, #2878, .F. ) ;
#1550 = CARTESIAN_POINT ( 'NONE',  ( 5.895596859100789899, 3.341829471546786667, 19.83331437242874884 ) ) ;
#1551 = DIRECTION ( 'NONE',  ( 1.000000000000000000, 0.000000000000000000, 0.000000000000000000 ) ) ;
#1552 = EDGE_CURVE ( 'NONE', #1853, #34885, #5718, .T. ) ;
#1553 = CARTESIAN_POINT ( 'NONE',  ( 0.8560838555295223751, -39.18289055412714106, -25.78902716088815694 ) ) ;
#1554 = CARTESIAN_POINT ( 'NONE',  ( 0.1365634738349403299, -6.412693133886302022, -43.65478194188872862 ) ) ;
#1555 = ORIENTED_EDGE ( 'NONE', *, *, #11372, .T. ) ;
#1556 = FACE_OUTER_BOUND ( 'NONE', #17373, .T. ) ;
#1557 = ADVANCED_FACE ( 'NONE', ( #14864 ), #21059, .F. ) ;
#1558 = CARTESIAN_POINT ( 'NONE',  ( 0.5839879882012667389, -44.25009266679219877, 18.32902119196551638 ) ) ;
#1559 = ORIENTED_EDGE ( 'NONE', *, *, #8314, .T. ) ;
#1560 = CARTESIAN_POINT ( 'NONE',  ( 0.8560838555295223751, 46.60258007729417784, 5.345312359546021241 ) ) ;
#1561 = B_SPLINE_CURVE_WITH_KNOTS ( 'NONE', 3,
 ( #26472, #16166, #21162, #39996, #40921, #59985, #44997, #44682, #12097, #26164, #35277, #2032, #40606, #54337, #16462, #34974, #45922, #30860, #11461 ),
 .UNSPECIFIED., .F., .F.,
 ( 4, 3, 3, 3, 3, 3, 4 ),
 ( 1.144439277862597989E-16, 0.0002618519381806243447, 0.0003927759815485966800, 0.0005237000248299447311, 0.0006546240681324983672, 0.0007855481115631302155, 0.0009699050456655107250 ),
 .UNSPECIFIED. ) ;
#1562 = ORIENTED_EDGE ( 'NONE', *, *, #45647, .T. ) ;
#1563 = CARTESIAN_POINT ( 'NONE',  ( -1.399999999999998579, 0.000000000000000000, 0.000000000000000000 ) ) ;
#1564 = CARTESIAN_POINT ( 'NONE',  ( 0.9730545539215883499, -42.90536227157002003, 0.5054011016611185125 ) ) ;
#1565 = EDGE_LOOP ( 'NONE', ( #14507, #60385, #31317, #56504 ) ) ;
#1566 = CARTESIAN_POINT ( 'NONE',  ( -2.739355103387248747, 14.24824591804147289, 4.453656386614430751 ) ) ;
#1567 = LINE ( 'NONE', #59511, #60713 ) ;
#1568 = CARTESIAN_POINT ( 'NONE',  ( 52.88125656235560967, 12.44562621623030374, 1.175754242111713532 ) ) ;
#1569 = CARTESIAN_POINT ( 'NONE',  ( 0.6253024248130448770, 49.04477337953059646, -2.460575454669923445 ) ) ;
#1570 = ORIENTED_EDGE ( 'NONE', *, *, #59670, .T. ) ;
#1571 = DIRECTION ( 'NONE',  ( -1.000000000000000000, -0.000000000000000000, -0.000000000000000000 ) ) ;
#1572 = CARTESIAN_POINT ( 'NONE',  ( 0.1073791018717578927, 42.81622261970994003, -5.147744207006430983 ) ) ;
#1573 = CARTESIAN_POINT ( 'NONE',  ( 0.9780106845699501061, 41.57531628521707745, -5.274876514156579432 ) ) ;
#1574 = CARTESIAN_POINT ( 'NONE',  ( 4.303969348037246512, 16.39840148505092543, 45.22910199346979709 ) ) ;
#1575 = B_SPLINE_CURVE_WITH_KNOTS ( 'NONE', 3,
 ( #38696, #9539, #61528, #5438, #43710, #19895 ),
 .UNSPECIFIED., .F., .F.,
 ( 4, 2, 4 ),
 ( 6.619851161367215630E-18, 0.0002291472222819954021, 0.0004582944445639841905 ),
 .UNSPECIFIED. ) ;
#1576 = ADVANCED_FACE ( 'NONE', ( #43068 ), #18483, .F. ) ;
#1577 = CARTESIAN_POINT ( 'NONE',  ( 4.962356264823603702, 17.31942680647464528, -38.35717733303005161 ) ) ;
#1578 = DIRECTION ( 'NONE',  ( 0.000000000000000000, 0.000000000000000000, 1.000000000000000000 ) ) ;
#1579 = CIRCLE ( 'NONE', #17620, 47.91270532121795611 ) ;
#1580 = CARTESIAN_POINT ( 'NONE',  ( 2.526464513654346433, 15.32058692775046005, -40.15570173027678180 ) ) ;
#1581 = CARTESIAN_POINT ( 'NONE',  ( 5.896782393890504181, -17.30187591025968530, 10.25529994022543079 ) ) ;
#1582 = CARTESIAN_POINT ( 'NONE',  ( 0.8751705887134553219, 47.55935879196470495, -7.160166390003808168 ) ) ;
#1583 = TOROIDAL_SURFACE ( 'NONE', #25619, 7.400000000000021672, 0.1000000000000001582 ) ;
#1584 = CARTESIAN_POINT ( 'NONE',  ( 0.6846871229502899947, 46.49193983736591917, 11.56285438919648811 ) ) ;
#1585 = CARTESIAN_POINT ( 'NONE',  ( 5.959828726073459926, 12.49879082830546473, 16.28130559351268758 ) ) ;
#1586 = CARTESIAN_POINT ( 'NONE',  ( 0.8753041380234465318, -45.17330286263774752, -19.24866323549208147 ) ) ;
#1587 = CARTESIAN_POINT ( 'NONE',  ( 0.6021448801613057400, -45.61590711508016938, 18.18598792189538926 ) ) ;
#1588 = CONICAL_SURFACE ( 'NONE', #36650, 4.000000000000000000, 1.047197551196595855 ) ;
#1589 = ORIENTED_EDGE ( 'NONE', *, *, #61644, .F. ) ;
#1590 = DIRECTION ( 'NONE',  ( 0.09722883295013594329, -0.1662994675516162035, 0.9812701162958157308 ) ) ;
#1591 = CARTESIAN_POINT ( 'NONE',  ( 3.407937589446178528, -9.356405769959122765, 10.00592723328957767 ) ) ;
#1592 = CARTESIAN_POINT ( 'NONE',  ( 0.5804410086790514622, 46.89585601637879364, 0.5463884574786330717 ) ) ;
#1593 = ORIENTED_EDGE ( 'NONE', *, *, #60869, .F. ) ;
#1594 = CARTESIAN_POINT ( 'NONE',  ( 0.1129192098497447394, 37.24220309526806005, 23.66368729500878842 ) ) ;
#1595 = CARTESIAN_POINT ( 'NONE',  ( 0.8554163680231708922, 36.24698750680798298, 29.78861141095913467 ) ) ;
#1596 = FACE_BOUND ( 'NONE', #57316, .T. ) ;
#1597 = PRODUCT_DEFINITION_CONTEXT ( 'detailed design', #21992, 'design' ) ;
#1598 = ORIENTED_EDGE ( 'NONE', *, *, #47462, .F. ) ;
#1599 = ORIENTED_EDGE ( 'NONE', *, *, #18489, .T. ) ;
#1600 = CARTESIAN_POINT ( 'NONE',  ( -6.077587904424778920, -8.912150607695380700, 17.06955163264944630 ) ) ;
#1601 = ADVANCED_FACE ( 'NONE', ( #24869 ), #22507, .F. ) ;
#1602 = ORIENTED_EDGE ( 'NONE', *, *, #33800, .T. ) ;
#1603 = CARTESIAN_POINT ( 'NONE',  ( 0.6021447746440204973, 11.18199449963166003, 47.81740413383703014 ) ) ;
#1604 = B_SPLINE_CURVE_WITH_KNOTS ( 'NONE', 3,
 ( #31589, #41620, #36311, #41025, #3672, #17496 ),
 .UNSPECIFIED., .F., .F.,
 ( 4, 2, 4 ),
 ( 1.519728548185745998E-16, 0.0002445252820015222798, 0.0004890505640028926628 ),
 .UNSPECIFIED. ) ;
#1605 = ORIENTED_EDGE ( 'NONE', *, *, #37368, .F. ) ;
#1606 = ADVANCED_FACE ( 'NONE', ( #35512 ), #26517, .F. ) ;
#1607 = ORIENTED_EDGE ( 'NONE', *, *, #26595, .F. ) ;
#1608 = CARTESIAN_POINT ( 'NONE',  ( 0.5987334363312689645, -48.77819064245283442, 5.678998513875774812 ) ) ;
#1609 = VERTEX_POINT ( 'NONE', #54571 ) ;
#1610 = CYLINDRICAL_SURFACE ( 'NONE', #37094, 11.40403086437694569 ) ;
#1611 = CARTESIAN_POINT ( 'NONE',  ( 2.528100132419515589, -37.99744774289700899, -17.84510419296803718 ) ) ;
#1612 = ORIENTED_EDGE ( 'NONE', *, *, #11387, .T. ) ;
#1613 = CARTESIAN_POINT ( 'NONE',  ( 1.227938101723748288, -26.79402671879349640, 33.52879263017854328 ) ) ;
#1614 = CARTESIAN_POINT ( 'NONE',  ( -2.000000000000022649, -3.464101615137742396, 0.000000000000000000 ) ) ;
#1615 = VECTOR ( 'NONE', #23772, 1000.000000000000000 ) ;
#1616 =( BOUNDED_SURFACE ( )  B_SPLINE_SURFACE ( 3, 1, ( 
 ( #42949, #36707 ),
 ( #55774, #12899 ),
 ( #31999, #51076 ),
 ( #3455, #22593 ) ),
 .UNSPECIFIED., .F., .F., .F. ) 
 B_SPLINE_SURFACE_WITH_KNOTS ( ( 4, 4 ),
 ( 2, 2 ),
 ( 0.000000000000000000, 1.000000000000000000 ),
 ( 0.000000000000000000, 1.000000000000000000 ),
 .UNSPECIFIED. ) 
 GEOMETRIC_REPRESENTATION_ITEM ( )  RATIONAL_B_SPLINE_SURFACE ( (
 ( 1.000000000000000000, 1.000000000000000000),
 ( 0.9754377213608244057, 0.9999580625633939235),
 ( 0.9754377213608244057, 0.9999580625633939235),
 ( 1.000000000000000000, 1.000000000000000000) ) ) 
 REPRESENTATION_ITEM ( '' )  SURFACE ( )  );
#1617 = ORIENTED_EDGE ( 'NONE', *, *, #32269, .T. ) ;
#1618 = CARTESIAN_POINT ( 'NONE',  ( 0.6023143664670691511, -18.65155446683280260, 44.34466302085792222 ) ) ;
#1619 = EDGE_CURVE ( 'NONE', #27238, #20167, #55359, .T. ) ;
#1620 = VECTOR ( 'NONE', #38965, 1000.000000000000114 ) ;
#1621 = CARTESIAN_POINT ( 'NONE',  ( 0.9754292580325141238, -37.13786007973355652, -19.41923828583751899 ) ) ;
#1622 = DIRECTION ( 'NONE',  ( 0.07906939808003035641, -0.9968364091521051407, -0.008074879317899854095 ) ) ;
#1623 = AXIS2_PLACEMENT_3D ( 'NONE', #6015, #6949, #58966 ) ;
#1624 = CARTESIAN_POINT ( 'NONE',  ( 0.7245667037590776127, 13.24050682223029618, 46.24390958543281727 ) ) ;
#1625 = ORIENTED_EDGE ( 'NONE', *, *, #59196, .T. ) ;
#1626 = EDGE_CURVE ( 'NONE', #20568, #57911, #59595, .T. ) ;
#1627 = ORIENTED_EDGE ( 'NONE', *, *, #680, .F. ) ;
#1628 = CARTESIAN_POINT ( 'NONE',  ( 2.282803330402965791, -46.76237730313502539, -4.447131256914662600 ) ) ;
#1629 = LINE ( 'NONE', #10754, #47485 ) ;
#1630 = CARTESIAN_POINT ( 'NONE',  ( -2.739355103387248747, 12.36564479942413897, -8.362917890634330220 ) ) ;
#1631 = ORIENTED_EDGE ( 'NONE', *, *, #9264, .F. ) ;
#1632 = CARTESIAN_POINT ( 'NONE',  ( 3.050102900204245682, -42.97776842906123562, -9.398758962546484241 ) ) ;
#1633 = CARTESIAN_POINT ( 'NONE',  ( 0.2224561200757622370, 42.64482917976808807, 6.380320192202126428 ) ) ;
#1634 = CARTESIAN_POINT ( 'NONE',  ( 0.9754292589017217185, 41.45298143524652090, -6.162612840702018424 ) ) ;
#1635 = CARTESIAN_POINT ( 'NONE',  ( 0.6027935024548037868, -41.57475399306903796, -24.20473723001681776 ) ) ;
#1636 = VECTOR ( 'NONE', #1213, 1000.000000000000114 ) ;
#1637 = ORIENTED_EDGE ( 'NONE', *, *, #43667, .F. ) ;
#1638 = VERTEX_POINT ( 'NONE', #35205 ) ;
#1639 = FACE_OUTER_BOUND ( 'NONE', #16266, .T. ) ;
#1640 = CARTESIAN_POINT ( 'NONE',  ( 4.553261556744875094, 42.43205150231973732, 11.36048287389764688 ) ) ;
#1641 =( BOUNDED_SURFACE ( )  B_SPLINE_SURFACE ( 3, 1, ( 
 ( #48627, #48328 ),
 ( #38336, #33017 ),
 ( #34241, #14827 ),
 ( #14522, #61781 ) ),
 .UNSPECIFIED., .F., .F., .F. ) 
 B_SPLINE_SURFACE_WITH_KNOTS ( ( 4, 4 ),
 ( 2, 2 ),
 ( 0.000000000000000000, 1.000000000000000000 ),
 ( 0.000000000000000000, 1.000000000000000000 ),
 .UNSPECIFIED. ) 
 GEOMETRIC_REPRESENTATION_ITEM ( )  RATIONAL_B_SPLINE_SURFACE ( (
 ( 1.000000000000000000, 1.000000000000000000),
 ( 0.7269869731126817891, 0.9931720237060910339),
 ( 0.7269869731126817891, 0.9931720237060910339),
 ( 1.000000000000000000, 1.000000000000000000) ) ) 
 REPRESENTATION_ITEM ( '' )  SURFACE ( )  );
#1642 = CARTESIAN_POINT ( 'NONE',  ( 0.1092355843206037486, -39.95589129953380336, 16.22491322981557005 ) ) ;
#1643 = CARTESIAN_POINT ( 'NONE',  ( 1.231276596079887264, -18.40965318903149495, -37.66113965983570466 ) ) ;
#1644 = CARTESIAN_POINT ( 'NONE',  ( 0.1102144999581333162, 34.28951223307529972, -26.15241010112988818 ) ) ;
#1645 = CARTESIAN_POINT ( 'NONE',  ( 0.7044674535452954967, 16.16814117525538563, 46.37234017976575018 ) ) ;
#1646 = EDGE_CURVE ( 'NONE', #14994, #48858, #28079, .T. ) ;
#1647 = CARTESIAN_POINT ( 'NONE',  ( 5.958863334805807099, 18.96276366205782438, 7.855954700275686875 ) ) ;
#1648 = DIRECTION ( 'NONE',  ( 0.000000000000000000, 0.000000000000000000, -1.000000000000000000 ) ) ;
#1649 = CARTESIAN_POINT ( 'NONE',  ( 0.6009452777970412107, -5.846392105360883384, 47.75105029762382003 ) ) ;
#1650 = CARTESIAN_POINT ( 'NONE',  ( 0.1129192098497455998, -6.563350895508677674, -43.63340707310831590 ) ) ;
#1651 = CARTESIAN_POINT ( 'NONE',  ( 4.833616638992205949, 43.93936707042099954, -14.43699082351666085 ) ) ;
#1652 = CARTESIAN_POINT ( 'NONE',  ( 0.8554163680231708922, -34.17638377241205916, -32.14312158693720534 ) ) ;
#1653 = CARTESIAN_POINT ( 'NONE',  ( 2.185380717157383135, 41.31325970390012969, -15.23267460774046178 ) ) ;
#1654 = DIRECTION ( 'NONE',  ( -1.000000000000000000, -3.673819061467147552E-16, 1.925929944387235306E-32 ) ) ;
#1655 = CARTESIAN_POINT ( 'NONE',  ( 3.238018933889920792, 6.676852487597082053, -11.61150865419828193 ) ) ;
#1656 = CARTESIAN_POINT ( 'NONE',  ( 0.9747592971366236814, -25.86343094887205751, 34.23774590565627562 ) ) ;
#1657 = CARTESIAN_POINT ( 'NONE',  ( 0.8753041380234465318, 11.79227530596935303, -47.66634631457717575 ) ) ;
#1658 = AXIS2_PLACEMENT_3D ( 'NONE', #1806, #16240, #49131 ) ;
#1659 = DIRECTION ( 'NONE',  ( -0.07439287786467650709, 0.9665813013808178811, 0.2453289374370170028 ) ) ;
#1660 = CARTESIAN_POINT ( 'NONE',  ( 0.6008123274975389894, 48.11686618743674870, 9.814363935516372095 ) ) ;
#1662 = ORIENTED_EDGE ( 'NONE', *, *, #36726, .T. ) ;
#1661 = CARTESIAN_POINT ( 'NONE',  ( 0.8557997880470690211, 41.02602466100812961, -24.73961900479208609 ) ) ;
#1663 = ORIENTED_EDGE ( 'NONE', *, *, #37491, .T. ) ;
#1664 = AXIS2_PLACEMENT_3D ( 'NONE', #21306, #16611, #35733 ) ;
#1665 = CARTESIAN_POINT ( 'NONE',  ( 0.1103744047535531458, -43.12441516302519773, -0.03874731383716748662 ) ) ;
#1666 = CARTESIAN_POINT ( 'NONE',  ( 3.376099380956842921, -9.627698927086855818, 9.328225822815269908 ) ) ;
#1667 = AXIS2_PLACEMENT_3D ( 'NONE', #61773, #37718, #61468 ) ;
#1668 = CARTESIAN_POINT ( 'NONE',  ( 0.8744876279028263033, -34.64280934553510605, -34.78829991575325664 ) ) ;
#1669 = ORIENTED_EDGE ( 'NONE', *, *, #1457, .T. ) ;
#1670 = ORIENTED_EDGE ( 'NONE', *, *, #57983, .T. ) ;
#1671 = CARTESIAN_POINT ( 'NONE',  ( 0.1103878639767399278, -11.11454059769229374, 41.66755962011260550 ) ) ;
#1672 = CARTESIAN_POINT ( 'NONE',  ( 4.962356264823608143, 0.000000000000000000, 0.000000000000000000 ) ) ;
#1673 = B_SPLINE_CURVE_WITH_KNOTS ( 'NONE', 3,
 ( #4355, #42621, #18816, #61683, #37943, #56999 ),
 .UNSPECIFIED., .F., .F.,
 ( 4, 2, 4 ),
 ( 9.140795285775094282E-18, 0.0002291978881530184911, 0.0004583957763060278749 ),
 .UNSPECIFIED. ) ;
#1674 = ORIENTED_EDGE ( 'NONE', *, *, #61049, .F. ) ;
#1675 = ORIENTED_EDGE ( 'NONE', *, *, #39734, .T. ) ;
#1676 = CARTESIAN_POINT ( 'NONE',  ( 0.8554163680231708922, -44.61245466728234987, 14.52357950615124160 ) ) ;
#1677 = EDGE_CURVE ( 'NONE', #17303, #60647, #12024, .T. ) ;
#1678 = VECTOR ( 'NONE', #9467, 1000.000000000000000 ) ;
#1679 = CARTESIAN_POINT ( 'NONE',  ( 5.959547316686252039, -12.49238070347988483, 16.28624005235077732 ) ) ;
#1680 = CARTESIAN_POINT ( 'NONE',  ( -6.078457390727109555, -18.27366031693668091, 6.071890122418351687 ) ) ;
#1681 = CARTESIAN_POINT ( 'NONE',  ( 4.553261556744875094, -9.994631851593741345, 42.77437199977043036 ) ) ;
#1682 = ADVANCED_FACE ( 'NONE', ( #45529 ), #50483, .F. ) ;
#1683 = ORIENTED_EDGE ( 'NONE', *, *, #28104, .F. ) ;
#1684 = CARTESIAN_POINT ( 'NONE',  ( 3.660087539127331535, 4.399983418616820074, -47.83637163185228758 ) ) ;
#1685 = B_SPLINE_CURVE_WITH_KNOTS ( 'NONE', 3,
 ( #43605, #24155, #52346, #38592 ),
 .UNSPECIFIED., .F., .F.,
 ( 4, 4 ),
 ( 0.000000000000000000, 0.004447772540403801579 ),
 .UNSPECIFIED. ) ;
#1686 = CARTESIAN_POINT ( 'NONE',  ( 4.549368137175248350, 0.000000000000000000, 0.000000000000000000 ) ) ;
#1687 = EDGE_CURVE ( 'NONE', #7406, #7463, #48599, .T. ) ;
#1688 = DIRECTION ( 'NONE',  ( 0.000000000000000000, 0.000000000000000000, -1.000000000000000000 ) ) ;
#1689 = ORIENTED_EDGE ( 'NONE', *, *, #18590, .F. ) ;
#1690 = ORIENTED_EDGE ( 'NONE', *, *, #41870, .F. ) ;
#1691 = CARTESIAN_POINT ( 'NONE',  ( 4.691466044806102076, 2.583163953527854773, 44.51344083442440080 ) ) ;
#1692 = CARTESIAN_POINT ( 'NONE',  ( 0.1129192098497455998, -40.71518461128082578, -17.00663193740825463 ) ) ;
#1693 = EDGE_LOOP ( 'NONE', ( #9790, #42814, #6756, #22247 ) ) ;
#1694 = CARTESIAN_POINT ( 'NONE',  ( 0.5834872094924179464, 44.33648115256923461, -18.11905305011470091 ) ) ;
#1695 = CARTESIAN_POINT ( 'NONE',  ( 0.6026777506516367566, -7.665548088515766523, 48.50552301686759904 ) ) ;
#1696 = CARTESIAN_POINT ( 'NONE',  ( 0.5848930533535030563, 27.67115520191724443, 37.86264983039310295 ) ) ;
#1697 = CARTESIAN_POINT ( 'NONE',  ( 0.8557997880470697982, -17.48760788519248521, 44.60232077416680596 ) ) ;
#1698 = EDGE_CURVE ( 'NONE', #24833, #50125, #35120, .T. ) ;
#1699 = ORIENTED_EDGE ( 'NONE', *, *, #39716, .F. ) ;
#1700 = FACE_OUTER_BOUND ( 'NONE', #27596, .T. ) ;
#1701 = DIRECTION ( 'NONE',  ( -1.000000000000000000, 0.000000000000000000, 0.000000000000000000 ) ) ;
#1702 = DIRECTION ( 'NONE',  ( 0.1736481776669314969, -0.9848077530122077983, 5.551115123125780853E-17 ) ) ;
#1703 = VERTEX_POINT ( 'NONE', #13245 ) ;
#1704 = CARTESIAN_POINT ( 'NONE',  ( 5.958863334805807099, -10.26176968287957258, 17.77634700750911279 ) ) ;
#1705 = VECTOR ( 'NONE', #52626, 1000.000000000000114 ) ;
#1706 = CARTESIAN_POINT ( 'NONE',  ( -6.072942160501519915, 18.63017572808491806, 4.870391630012528950 ) ) ;
#1707 = ORIENTED_EDGE ( 'NONE', *, *, #59461, .F. ) ;
#1708 = CARTESIAN_POINT ( 'NONE',  ( 0.7762777257811939169, 33.23866587527477634, 34.49689427664277730 ) ) ;
#1709 = CARTESIAN_POINT ( 'NONE',  ( 1.830465331921977246, 41.40011171874475338, 15.04682044665391949 ) ) ;
#1710 = CIRCLE ( 'NONE', #42763, 43.08621763946400307 ) ;
#1711 = ORIENTED_EDGE ( 'NONE', *, *, #11636, .F. ) ;
#1712 = CARTESIAN_POINT ( 'NONE',  ( -6.016761891674565099, -4.880293656735092078, 18.20023637398597671 ) ) ;
#1713 = VECTOR ( 'NONE', #21673, 1000.000000000000114 ) ;
#1714 = CARTESIAN_POINT ( 'NONE',  ( 0.8760168074886960365, -41.20610493656892714, -24.81951362746063339 ) ) ;
#1715 = CARTESIAN_POINT ( 'NONE',  ( 4.214292481396495482, -11.25702090725073035, -1.199999999999999956 ) ) ;
#1716 = CARTESIAN_POINT ( 'NONE',  ( 2.648799415243708655, 49.00436887187488111, 1.757638972832060720 ) ) ;
#1717 =( BOUNDED_SURFACE ( )  B_SPLINE_SURFACE ( 3, 1, ( 
 ( #12022, #22322 ),
 ( #21701, #45843 ),
 ( #17626, #36751 ),
 ( #17318, #56124 ) ),
 .UNSPECIFIED., .F., .F., .F. ) 
 B_SPLINE_SURFACE_WITH_KNOTS ( ( 4, 4 ),
 ( 2, 2 ),
 ( 0.000000000000000000, 1.000000000000000000 ),
 ( 0.000000000000000000, 1.000000000000000000 ),
 .UNSPECIFIED. ) 
 GEOMETRIC_REPRESENTATION_ITEM ( )  RATIONAL_B_SPLINE_SURFACE ( (
 ( 1.000000000000000000, 1.000000000000000000),
 ( 0.9751682680413298332, 0.9999560080971552356),
 ( 0.9751682680413298332, 0.9999560080971552356),
 ( 1.000000000000000000, 1.000000000000000000) ) ) 
 REPRESENTATION_ITEM ( '' )  SURFACE ( )  );
#1718 = CARTESIAN_POINT ( 'NONE',  ( 3.727782113643637096, 22.20616388426432408, 37.94290528479822910 ) ) ;
#1719 = CARTESIAN_POINT ( 'NONE',  ( 4.553261556744875094, -43.85016385001095784, 2.588956575693979190 ) ) ;
#1720 = CARTESIAN_POINT ( 'NONE',  ( 4.322998006666165516, 8.359821156456478164, -47.25487450103527465 ) ) ;
#1721 = CARTESIAN_POINT ( 'NONE',  ( 2.301430502907645170, -40.93949994354167643, -25.12309903330006122 ) ) ;
#1722 = LINE ( 'NONE', #34653, #61604 ) ;
#1723 = CARTESIAN_POINT ( 'NONE',  ( 0.9790850452238877288, 41.54146669795389357, 5.535690999864669060 ) ) ;
#1724 = CARTESIAN_POINT ( 'NONE',  ( 0.5837800304671217910, 27.85439319122116686, -37.72757760747899169 ) ) ;
#1725 = VERTEX_POINT ( 'NONE', #38529 ) ;
#1726 = B_SPLINE_CURVE_WITH_KNOTS ( 'NONE', 3,
 ( #60754, #24102, #23798, #18803 ),
 .UNSPECIFIED., .F., .F.,
 ( 4, 4 ),
 ( 0.000000000000000000, 0.004444103432399266161 ),
 .UNSPECIFIED. ) ;
#1727 = EDGE_CURVE ( 'NONE', #60037, #54442, #34421, .T. ) ;
#1728 = CARTESIAN_POINT ( 'NONE',  ( 1.231276596079881047, -31.65135013586901991, 27.48579279545509380 ) ) ;
#1729 = CARTESIAN_POINT ( 'NONE',  ( 4.975801465491695552, 0.000000000000000000, 0.000000000000000000 ) ) ;
#1730 = CARTESIAN_POINT ( 'NONE',  ( 4.960386119450149955, -43.75174247978070952, -0.4706321868421235455 ) ) ;
#1731 = CARTESIAN_POINT ( 'NONE',  ( 0.5998501479064699549, 33.64490850298844293, -34.38546660123262200 ) ) ;
#1733 = B_SPLINE_CURVE_WITH_KNOTS ( 'NONE', 3,
 ( #46527, #3576, #60281, #51817, #22708, #12711 ),
 .UNSPECIFIED., .F., .F.,
 ( 4, 2, 4 ),
 ( 1.226145898665688582E-16, 0.0002448718616795922832, 0.0004897437233590619431 ),
 .UNSPECIFIED. ) ;
#1732 = CARTESIAN_POINT ( 'NONE',  ( 1.088908134280558881, 41.24246781061832934, -11.85879120571462764 ) ) ;
#1734 = EDGE_CURVE ( 'NONE', #12769, #55806, #53791, .T. ) ;
#1735 = DIRECTION ( 'NONE',  ( 6.853073559125475997E-15, 0.7071067811865487940, -0.7071067811865463515 ) ) ;
#1736 = FACE_OUTER_BOUND ( 'NONE', #26676, .T. ) ;
#1737 = CARTESIAN_POINT ( 'NONE',  ( 0.5998501479064699549, 46.60114184914301205, 11.94461217097485672 ) ) ;
#1738 = B_SPLINE_CURVE_WITH_KNOTS ( 'NONE', 3,
 ( #27448, #51242, #55946, #37816, #3015, #3930, #12763, #3315, #4239, #3619, #51548, #23374, #36563, #47193, #60633, #13064, #13996, #37183, #61561 ),
 .UNSPECIFIED., .F., .F.,
 ( 4, 3, 3, 3, 3, 3, 4 ),
 ( 8.674294979774126656E-18, 0.0002732106629380585830, 0.0004098138914053739684, 0.0005464171197651428950, 0.0006830203481512547902, 0.0008196235766963618982, 0.001011968216111142028 ),
 .UNSPECIFIED. ) ;
#1739 = EDGE_CURVE ( 'NONE', #28202, #37486, #8089, .T. ) ;
#1740 = VECTOR ( 'NONE', #39786, 1000.000000000000114 ) ;
#1741 = CARTESIAN_POINT ( 'NONE',  ( 5.895596859100789899, 8.469463536102802337, 18.24270732712424348 ) ) ;
#1742 = B_SPLINE_CURVE_WITH_KNOTS ( 'NONE', 3,
 ( #25440, #1621, #19845, #39266, #54236, #58953 ),
 .UNSPECIFIED., .F., .F.,
 ( 4, 2, 4 ),
 ( 0.000000000000000000, 0.0002291459268755689067, 0.0004582918537511378133 ),
 .UNSPECIFIED. ) ;
#1744 = VERTEX_POINT ( 'NONE', #56130 ) ;
#1743 = CARTESIAN_POINT ( 'NONE',  ( 0.7948878604505665857, 48.35174766440331240, 8.532710301907952655 ) ) ;
#1745 = ORIENTED_EDGE ( 'NONE', *, *, #28623, .F. ) ;
#1746 = CARTESIAN_POINT ( 'NONE',  ( 0.000000000000000000, 0.000000000000000000, 0.000000000000000000 ) ) ;
#1747 = FACE_BOUND ( 'NONE', #39086, .T. ) ;
#1748 = CARTESIAN_POINT ( 'NONE',  ( 0.1073791018717578927, 16.05399293000759542, 40.02496097243063389 ) ) ;
#1749 = VERTEX_POINT ( 'NONE', #51119 ) ;
#1750 = CARTESIAN_POINT ( 'NONE',  ( -2.739355103387247858, -7.962282735395077360, 12.62733624295506196 ) ) ;
#1751 = CARTESIAN_POINT ( 'NONE',  ( 0.7056759521544992975, 31.99426006192621230, 34.29454989071619764 ) ) ;
#1752 = CARTESIAN_POINT ( 'NONE',  ( 5.440000000000000391, 6.831466544798160849E-15, 0.000000000000000000 ) ) ;
#1753 = ORIENTED_EDGE ( 'NONE', *, *, #1423, .T. ) ;
#1754 = ORIENTED_EDGE ( 'NONE', *, *, #40398, .F. ) ;
#1755 = CARTESIAN_POINT ( 'NONE',  ( -6.016489644550736315, 7.215050741358040476, 17.40716454747931152 ) ) ;
#1756 = ADVANCED_FACE ( 'NONE', ( #46456 ), #56058, .F. ) ;
#1757 = CIRCLE ( 'NONE', #29764, 2.649999999999999467 ) ;
#1758 = CARTESIAN_POINT ( 'NONE',  ( 0.1081432562775998252, -10.75186376283313372, -41.76274004527628847 ) ) ;
#1759 = AXIS2_PLACEMENT_3D ( 'NONE', #7101, #2724, #17772 ) ;
#1760 = CARTESIAN_POINT ( 'NONE',  ( 0.6026112563231247332, 37.27953482426413245, 31.96525110476507692 ) ) ;
#1761 = EDGE_CURVE ( 'NONE', #41223, #46515, #2321, .T. ) ;
#1762 = ORIENTED_EDGE ( 'NONE', *, *, #37756, .F. ) ;
#1763 = B_SPLINE_CURVE_WITH_KNOTS ( 'NONE', 3,
 ( #15361, #294, #47944, #4993 ),
 .UNSPECIFIED., .F., .F.,
 ( 4, 4 ),
 ( 0.000000000000000000, 0.004446090762761373792 ),
 .UNSPECIFIED. ) ;
#1764 = CARTESIAN_POINT ( 'NONE',  ( 0.9754292589017198312, -27.49953653147686694, -31.62440445999337157 ) ) ;
#1765 = EDGE_CURVE ( 'NONE', #58463, #53012, #24756, .T. ) ;
#1766 = CARTESIAN_POINT ( 'NONE',  ( 5.974727161628369032, -20.52494643607030156, -0.01551142186642303668 ) ) ;
#1767 = ORIENTED_EDGE ( 'NONE', *, *, #22018, .T. ) ;
#1768 = CARTESIAN_POINT ( 'NONE',  ( 0.9747592971366243475, 41.36145845824422906, -11.41797089479089777 ) ) ;
#1769 = ORIENTED_EDGE ( 'NONE', *, *, #21092, .F. ) ;
#1770 = CARTESIAN_POINT ( 'NONE',  ( 0.1064266418746775411, -37.06314021531093772, -22.04679912212815296 ) ) ;
#1771 = CARTESIAN_POINT ( 'NONE',  ( 5.959547316686252039, -0.003562808153049117858, 20.52562247508876681 ) ) ;
#1772 = EDGE_LOOP ( 'NONE', ( #39252, #3865, #33031, #3390 ) ) ;
#1773 = DIRECTION ( 'NONE',  ( -1.000000000000000000, -1.836909530733573776E-16, 1.925929944387235853E-32 ) ) ;
#1774 = CARTESIAN_POINT ( 'NONE',  ( 0.5837800304671211249, -19.78143393310113396, 42.51978602638839533 ) ) ;
#1775 = DIRECTION ( 'NONE',  ( -0.9848077530122080203, -0.1736481776669315524, 2.220446049250313574E-16 ) ) ;
#1776 = CARTESIAN_POINT ( 'NONE',  ( 0.5832366564991504632, -37.83193087518330344, 29.37287047358866943 ) ) ;
#1777 = EDGE_CURVE ( 'NONE', #18401, #35559, #18782, .T. ) ;
#1778 = AXIS2_PLACEMENT_3D ( 'NONE', #20254, #15546, #816 ) ;
#1779 = ORIENTED_EDGE ( 'NONE', *, *, #16286, .T. ) ;
#1780 = CARTESIAN_POINT ( 'NONE',  ( 4.975801465491695552, 8.787181743660156030, -47.10002938642133330 ) ) ;
#1781 = CARTESIAN_POINT ( 'NONE',  ( 0.1140933569871963732, 39.91767626351668241, -18.80236878175147552 ) ) ;
#1782 = ORIENTED_EDGE ( 'NONE', *, *, #33899, .T. ) ;
#1783 = CARTESIAN_POINT ( 'NONE',  ( 0.5782707292762423457, 17.53027906811894709, 43.50201914281093707 ) ) ;
#1784 = B_SPLINE_CURVE_WITH_KNOTS ( 'NONE', 3,
 ( #42064, #61118, #47351, #56421, #42363, #61418, #18535, #37663, #13856, #32960, #52032, #9128, #28234, #36356, #46671, #32258 ),
 .UNSPECIFIED., .F., .F.,
 ( 4, 3, 3, 3, 3, 4 ),
 ( 2.194378057379452319E-17, 0.0002612764279487688802, 0.0003919131003184762093, 0.0005225497727000617864, 0.0007837925190632418848, 0.001045051706266715867 ),
 .UNSPECIFIED. ) ;
#1785 = EDGE_LOOP ( 'NONE', ( #26681, #47476, #7372, #29705, #50543, #46251, #13058, #12859, #29736, #56103, #18679, #28008, #61702, #49743, #44732, #23947, #15196, #56585, #20948, #52576, #29452, #10800, #50944, #42394, #56388, #23385, #32255, #16806, #15974, #42474, #50312, #5372, #4211, #57015, #23899, #59809, #29466, #7475, #15123, #54708, #28044, #50173, #11499, #49177, #34038, #61806, #8966, #55785, #44452, #1663, #17622, #35156, #54989, #24121, #24307, #4162, #20569, #14889, #57043, #3331, #57616, #35531, #26298, #29303, #25707, #36346, #49300, #21530, #36266, #19152, #40250, #8168, #52254, #31456, #56784, #1931, #44120, #997, #21672, #6018, #26943, #44572, #56485, #35657, #549, #27307, #24367, #50334, #56178, #44440, #28787, #6665, #43977, #19200, #16507, #47349, #36235, #24202, #16452, #4637, #35491, #55842, #44419, #60106, #13297, #27706, #15673, #19034, #36330, #7473, #45729, #53037, #32997, #53919, #4135, #17910, #8468, #3749, #1390, #30361, #48511, #58408, #17856, #61697, #27558, #35075, #19751, #17247, #45447, #58598, #30229, #24688, #22220, #20828, #28767, #12825, #33469, #18448, #45654, #640, #55681, #17785, #36157, #30142, #56925, #42819, #13909, #16379 ) ) ;
#1786 = FACE_OUTER_BOUND ( 'NONE', #6546, .T. ) ;
#1787 = AXIS2_PLACEMENT_3D ( 'NONE', #1410, #52817, #24318 ) ;
#1788 = VERTEX_POINT ( 'NONE', #17629 ) ;
#1789 = CARTESIAN_POINT ( 'NONE',  ( 3.783198216974392292, -41.09147814699331036, -12.79806054635177226 ) ) ;
#1790 = FACE_OUTER_BOUND ( 'NONE', #6223, .T. ) ;
#1791 = CARTESIAN_POINT ( 'NONE',  ( 0.5980271706414711508, -42.44486003424485432, -24.70795619866254711 ) ) ;
#1792 = ORIENTED_EDGE ( 'NONE', *, *, #61263, .F. ) ;
#1793 = CARTESIAN_POINT ( 'NONE',  ( 0.1152339509894530906, 43.35263776105328759, 8.215320420661617717 ) ) ;
#1794 = CARTESIAN_POINT ( 'NONE',  ( -4.473699999999999122, 0.000000000000000000, -47.67072199303260049 ) ) ;
#1795 = DIRECTION ( 'NONE',  ( 1.000000000000000000, 0.000000000000000000, 0.000000000000000000 ) ) ;
#1796 = ORIENTED_EDGE ( 'NONE', *, *, #1228, .T. ) ;
#1797 = B_SPLINE_CURVE_WITH_KNOTS ( 'NONE', 3,
 ( #16475, #31496, #50903, #12111 ),
 .UNSPECIFIED., .F., .F.,
 ( 4, 4 ),
 ( 2.093184199687144787E-17, 0.004559932413162186803 ),
 .UNSPECIFIED. ) ;
#1798 = ORIENTED_EDGE ( 'NONE', *, *, #49935, .T. ) ;
#1799 = CARTESIAN_POINT ( 'NONE',  ( 0.5827357941260193908, 18.66407988912490978, 44.10984861950464619 ) ) ;
#1800 = CARTESIAN_POINT ( 'NONE',  ( 1.112077966505211624, 30.40372978055294695, 31.91619558405531976 ) ) ;
#1801 = CARTESIAN_POINT ( 'NONE',  ( 4.553261556744873317, -33.59363643963353496, -28.30206982864260112 ) ) ;
#1802 = CARTESIAN_POINT ( 'NONE',  ( 0.1092565886968784733, 26.00565248013053221, -34.40108480122224677 ) ) ;
#1803 = DIRECTION ( 'NONE',  ( -0.000000000000000000, -0.000000000000000000, -1.000000000000000000 ) ) ;
#1804 = CARTESIAN_POINT ( 'NONE',  ( -5.995132425357893702, -2.468096378287997439, -18.68182899165013922 ) ) ;
#1805 = ORIENTED_EDGE ( 'NONE', *, *, #29261, .T. ) ;
#1806 = CARTESIAN_POINT ( 'NONE',  ( 5.000000000000007994, -56.56854249492410958, 56.56854249492351983 ) ) ;
#1807 = VECTOR ( 'NONE', #52222, 999.9999999999998863 ) ;
#1808 = CARTESIAN_POINT ( 'NONE',  ( 2.618530812446115519, -15.26631161697991601, -44.45971793445684028 ) ) ;
#1809 = VERTEX_POINT ( 'NONE', #60827 ) ;
#1810 = VECTOR ( 'NONE', #7131, 1000.000000000000000 ) ;
#1811 = EDGE_CURVE ( 'NONE', #50189, #49082, #41196, .T. ) ;
#1812 = CARTESIAN_POINT ( 'NONE',  ( 0.8760168074886965917, -28.57146030081952759, -38.69913431881813182 ) ) ;
#1813 = CARTESIAN_POINT ( 'NONE',  ( 0.6029443199889047422, -19.87788362468473835, -44.90442499863340231 ) ) ;
#1814 = CARTESIAN_POINT ( 'NONE',  ( 0.1155031312995260795, -42.72350491080801760, 11.02922303101952117 ) ) ;
#1815 = CARTESIAN_POINT ( 'NONE',  ( 4.549368137175248350, -19.17571786012296187, -38.40568845698270195 ) ) ;
#1816 = FACE_OUTER_BOUND ( 'NONE', #9677, .T. ) ;
#1817 = EDGE_CURVE ( 'NONE', #33784, #61780, #18663, .T. ) ;
#1818 = FILL_AREA_STYLE_COLOUR ( '', #25853 ) ;
#1819 = LINE ( 'NONE', #59139, #34862 ) ;
#1820 = CARTESIAN_POINT ( 'NONE',  ( 0.1156867017252034419, 20.51982528184129606, -39.06250859427608191 ) ) ;
#1821 = CARTESIAN_POINT ( 'NONE',  ( 0.8557997880470697982, -5.347802024197571669, 47.60865952216997243 ) ) ;
#1822 = EDGE_CURVE ( 'NONE', #46926, #29080, #14228, .T. ) ;
#1823 = CARTESIAN_POINT ( 'NONE',  ( 0.1152809850208375425, 29.50062020599969514, 32.81247765639037084 ) ) ;
#1824 = EDGE_CURVE ( 'NONE', #18698, #37177, #3642, .T. ) ;
#1825 = DIRECTION ( 'NONE',  ( -0.000000000000000000, 0.8660254037844392627, 0.4999999999999990008 ) ) ;
#1826 = AXIS2_PLACEMENT_3D ( 'NONE', #39226, #20107, #30097 ) ;
#1827 = EDGE_CURVE ( 'NONE', #40810, #10512, #4408, .T. ) ;
#1828 = CARTESIAN_POINT ( 'NONE',  ( 0.1073791018717483448, 0.4849339620927342054, 43.12183934961191767 ) ) ;
#1829 = DIRECTION ( 'NONE',  ( 0.07439287786467665975, -0.9868880006907391200, -0.1432402660415254547 ) ) ;
#1830 = CARTESIAN_POINT ( 'NONE',  ( 0.6253024248130502061, 27.52858932731207631, 40.66473898927478814 ) ) ;
#1831 = CARTESIAN_POINT ( 'NONE',  ( 5.958863334805807099, -20.52565293643016275, 0.001220270596100524923 ) ) ;
#1832 = CARTESIAN_POINT ( 'NONE',  ( 1.157643937452368821, 38.90537125510820715, 15.60046031682893286 ) ) ;
#1833 = EDGE_CURVE ( 'NONE', #42044, #1398, #55236, .T. ) ;
#1834 = VERTEX_POINT ( 'NONE', #25330 ) ;
#1835 = CARTESIAN_POINT ( 'NONE',  ( -1.500000000000001332, 0.000000000000000000, 0.000000000000000000 ) ) ;
#1836 = ADVANCED_FACE ( 'NONE', ( #1816 ), #16105, .F. ) ;
#1837 = CARTESIAN_POINT ( 'NONE',  ( 0.6067375320500729696, 5.548194933740165702, 47.57460111700603278 ) ) ;
#1838 = CARTESIAN_POINT ( 'NONE',  ( 0.9756950546413936110, -26.19769393035348060, -33.98259063592748674 ) ) ;
#1839 = CARTESIAN_POINT ( 'NONE',  ( 5.894904586330512508, -13.98146465072135847, 14.45849432971053794 ) ) ;
#1840 = CARTESIAN_POINT ( 'NONE',  ( 0.5326698147273788431, 0.000000000000000000, 0.000000000000000000 ) ) ;
#1841 = ORIENTED_EDGE ( 'NONE', *, *, #58152, .F. ) ;
#1842 = CARTESIAN_POINT ( 'NONE',  ( 4.553261556744875094, -14.95853073564453339, -41.30111286702108941 ) ) ;
#1843 = CARTESIAN_POINT ( 'NONE',  ( 2.624215991343608501, -22.77108897942107291, -42.26352390376119672 ) ) ;
#1844 = CARTESIAN_POINT ( 'NONE',  ( 0.5263152470540364281, 5.264429658279185424E-15, 42.88844316795388778 ) ) ;
#1845 = ORIENTED_EDGE ( 'NONE', *, *, #29444, .T. ) ;
#1846 = CARTESIAN_POINT ( 'NONE',  ( 1.834102595619085507, -44.02840226159792536, 1.302896445847945950 ) ) ;
#1847 = CARTESIAN_POINT ( 'NONE',  ( 4.335381028904201628, 39.85754067141741785, 28.48040202122594167 ) ) ;
#1848 = VERTEX_POINT ( 'NONE', #5579 ) ;
#1849 = VECTOR ( 'NONE', #56074, 1000.000000000000000 ) ;
#1850 = CARTESIAN_POINT ( 'NONE',  ( 1.000110580585052311, -26.55225625611131690, -32.42522429346786339 ) ) ;
#1851 = ORIENTED_EDGE ( 'NONE', *, *, #6408, .T. ) ;
#1852 = CARTESIAN_POINT ( 'NONE',  ( 0.6039202388192952409, -35.39742030260028827, 34.03801329058516245 ) ) ;
#1853 = VERTEX_POINT ( 'NONE', #10010 ) ;
#1854 = CARTESIAN_POINT ( 'NONE',  ( 0.9740398440564310700, 21.81228698783141695, 36.95080095316281898 ) ) ;
#1855 = CARTESIAN_POINT ( 'NONE',  ( 0.5998501479064699549, 41.39809967730487017, -24.50586714782561160 ) ) ;
#1856 = ORIENTED_EDGE ( 'NONE', *, *, #3295, .F. ) ;
#1857 = ADVANCED_FACE ( 'NONE', ( #25637 ), #54862, .F. ) ;
#1858 = VERTEX_POINT ( 'NONE', #34439 ) ;
#1859 = CARTESIAN_POINT ( 'NONE',  ( 5.896782393890504181, 16.58545041924856278, 11.37756218478545911 ) ) ;
#1860 = CARTESIAN_POINT ( 'NONE',  ( 0.8557997880470690211, -24.73961900479222820, -41.02602466100805145 ) ) ;
#1861 = EDGE_CURVE ( 'NONE', #7602, #58429, #54453, .T. ) ;
#1862 = B_SPLINE_CURVE_WITH_KNOTS ( 'NONE', 3,
 ( #11174, #53140, #835, #10247 ),
 .UNSPECIFIED., .F., .F.,
 ( 4, 4 ),
 ( 0.000000000000000000, 0.005004948556313794025 ),
 .UNSPECIFIED. ) ;
#1863 = ORIENTED_EDGE ( 'NONE', *, *, #30854, .T. ) ;
#1864 = ORIENTED_EDGE ( 'NONE', *, *, #11045, .T. ) ;
#1865 = CARTESIAN_POINT ( 'NONE',  ( 0.1100053167205931187, 5.806749312984545774, 42.73174076921946352 ) ) ;
#1866 = CARTESIAN_POINT ( 'NONE',  ( -2.569797478183783568, 13.34095667500604776, -6.011723966604011871 ) ) ;
#1867 = CARTESIAN_POINT ( 'NONE',  ( 0.5839254288179547281, 33.93171296845886076, -33.80331890503232728 ) ) ;
#1868 = CARTESIAN_POINT ( 'NONE',  ( 0.5806925824938499181, -34.41156632303712826, -31.86010774524751454 ) ) ;
#1869 = CARTESIAN_POINT ( 'NONE',  ( 5.960721111146673579, -7.860635756377761574, -18.96073515164545498 ) ) ;
#1870 = ORIENTED_EDGE ( 'NONE', *, *, #54295, .T. ) ;
#1871 = PRODUCT_RELATED_PRODUCT_CATEGORY ( 'part', '', ( #3775 ) ) ;
#1872 = DIRECTION ( 'NONE',  ( 0.000000000000000000, 0.000000000000000000, -1.000000000000000000 ) ) ;
#1873 = CARTESIAN_POINT ( 'NONE',  ( -90.00000000000000000, 0.000000000000000000, 0.000000000000000000 ) ) ;
#1874 = VERTEX_POINT ( 'NONE', #54743 ) ;
#1875 = CARTESIAN_POINT ( 'NONE',  ( 0.8744876279028306332, -34.64280934553560343, 34.78829991575276637 ) ) ;
#1876 = VERTEX_POINT ( 'NONE', #55361 ) ;
#1877 = AXIS2_PLACEMENT_3D ( 'NONE', #61296, #18414, #23723 ) ;
#1878 = DIRECTION ( 'NONE',  ( 0.09722883295013597105, 0.9927043560032283720, 0.07130649069594115208 ) ) ;
#1879 = CARTESIAN_POINT ( 'NONE',  ( 3.783198216974389627, 20.00646744835666269, 38.10565824507906996 ) ) ;
#1880 = ORIENTED_EDGE ( 'NONE', *, *, #27271, .F. ) ;
#1881 = CARTESIAN_POINT ( 'NONE',  ( 0.9790724872846777727, -12.37788730724380315, -40.03901991546029393 ) ) ;
#1882 = CARTESIAN_POINT ( 'NONE',  ( 4.962356264823608143, -36.43094049105388166, 21.07183363638861096 ) ) ;
#1883 = CARTESIAN_POINT ( 'NONE',  ( 52.61790645059762284, 12.39576633866792044, -1.629651744153580939 ) ) ;
#1884 = CARTESIAN_POINT ( 'NONE',  ( 0.8744876279028306332, 48.35212675551500183, 8.510105087371359289 ) ) ;
#1885 = EDGE_LOOP ( 'NONE', ( #25728, #31435 ) ) ;
#1886 = LINE ( 'NONE', #50135, #48953 ) ;
#1887 = VERTEX_POINT ( 'NONE', #36294 ) ;
#1888 = EDGE_CURVE ( 'NONE', #41892, #30382, #23864, .T. ) ;
#1889 = CARTESIAN_POINT ( 'NONE',  ( 4.967162193818129623, -32.10009971360051395, -28.74031574030045633 ) ) ;
#1890 = LINE ( 'NONE', #20401, #30786 ) ;
#1891 = B_SPLINE_CURVE_WITH_KNOTS ( 'NONE', 3,
 ( #12129, #50311, #49694, #21502 ),
 .UNSPECIFIED., .F., .F.,
 ( 4, 4 ),
 ( 7.589415207398532001E-19, 0.004446298630425063285 ),
 .UNSPECIFIED. ) ;
#1892 = ADVANCED_FACE ( 'NONE', ( #45389 ), #39356, .F. ) ;
#1893 = CARTESIAN_POINT ( 'NONE',  ( 4.956445790443991584, 29.98832127573247774, 36.30755619981999871 ) ) ;
#1894 = CARTESIAN_POINT ( 'NONE',  ( 4.956445790443998689, -16.41925925744477510, 44.13554095710679093 ) ) ;
#1895 = CARTESIAN_POINT ( 'NONE',  ( 5.960721111146673579, -17.77250458025999080, 10.26825948882894934 ) ) ;
#1896 = EDGE_CURVE ( 'NONE', #12539, #40478, #35684, .T. ) ;
#1897 = VECTOR ( 'NONE', #41450, 1000.000000000000114 ) ;
#1898 = EDGE_CURVE ( 'NONE', #54850, #49335, #4039, .T. ) ;
#1899 = CARTESIAN_POINT ( 'NONE',  ( 0.9752570700956795235, 37.27462300504105741, -21.25416333281058101 ) ) ;
#1900 = CARTESIAN_POINT ( 'NONE',  ( 5.901463166500146684, -17.29756286482734495, 10.26217273670555130 ) ) ;
#1901 = FACE_OUTER_BOUND ( 'NONE', #41118, .T. ) ;
#1902 = B_SPLINE_CURVE_WITH_KNOTS ( 'NONE', 3,
 ( #49260, #6014, #26387, #54557 ),
 .UNSPECIFIED., .F., .F.,
 ( 4, 4 ),
 ( 8.673617379884035472E-19, 0.004446298630425045070 ),
 .UNSPECIFIED. ) ;
#1903 = CARTESIAN_POINT ( 'NONE',  ( 0.2111111111111110827, -9.497654031326126400, 0.000000000000000000 ) ) ;
#1904 = CARTESIAN_POINT ( 'NONE',  ( 4.967162193818130511, -18.65818244221228284, -38.83676580803786749 ) ) ;
#1905 =( BOUNDED_SURFACE ( )  B_SPLINE_SURFACE ( 3, 1, ( 
 ( #18082, #61273 ),
 ( #3640, #8981 ),
 ( #14012, #28390 ),
 ( #9586, #42828 ) ),
 .UNSPECIFIED., .F., .F., .F. ) 
 B_SPLINE_SURFACE_WITH_KNOTS ( ( 4, 4 ),
 ( 2, 2 ),
 ( 0.000000000000000000, 1.000000000000000000 ),
 ( 0.000000000000000000, 1.000000000000000000 ),
 .UNSPECIFIED. ) 
 GEOMETRIC_REPRESENTATION_ITEM ( )  RATIONAL_B_SPLINE_SURFACE ( (
 ( 1.000000000000000000, 1.000000000000000000),
 ( 0.9953485035131437453, 0.8621029689291515030),
 ( 0.9953485035131437453, 0.8621029689291515030),
 ( 1.000000000000000000, 1.000000000000000000) ) ) 
 REPRESENTATION_ITEM ( '' )  SURFACE ( )  );
#1906 = CARTESIAN_POINT ( 'NONE',  ( 0.5326698147273788431, 0.000000000000000000, 0.000000000000000000 ) ) ;
#1907 = CARTESIAN_POINT ( 'NONE',  ( 0.1158516988532803660, 37.00677167196558059, 24.03000227323755666 ) ) ;
#1908 = VERTEX_POINT ( 'NONE', #50366 ) ;
#1909 = AXIS2_PLACEMENT_3D ( 'NONE', #23583, #13584, #8547 ) ;
#1910 = CARTESIAN_POINT ( 'NONE',  ( 1.834102595619085507, -2.713406789205373038, -43.96402129530440561 ) ) ;
#1911 = CARTESIAN_POINT ( 'NONE',  ( 0.9762797500689124330, 20.58271139965489738, 36.50584578699993443 ) ) ;
#1912 = CARTESIAN_POINT ( 'NONE',  ( 2.706805983486680223, -42.11943299225157489, 12.75654646567733153 ) ) ;
#1913 = EDGE_CURVE ( 'NONE', #1320, #26290, #14898, .T. ) ;
#1914 = ORIENTED_EDGE ( 'NONE', *, *, #48852, .T. ) ;
#1915 = CARTESIAN_POINT ( 'NONE',  ( 0.5980271706414734822, 48.33586592461342235, 8.700190122029439976 ) ) ;
#1916 = CARTESIAN_POINT ( 'NONE',  ( 0.7242486021783884897, 44.58864233489314444, -20.56366789035821441 ) ) ;
#1917 = CARTESIAN_POINT ( 'NONE',  ( 0.6031356219577718170, -12.53544563195267436, -46.44562759437249611 ) ) ;
#1918 =( BOUNDED_SURFACE ( )  B_SPLINE_SURFACE ( 3, 1, ( 
 ( #47050, #32950 ),
 ( #13846, #23522 ),
 ( #5323, #42971 ),
 ( #61714, #23225 ) ),
 .UNSPECIFIED., .F., .F., .F. ) 
 B_SPLINE_SURFACE_WITH_KNOTS ( ( 4, 4 ),
 ( 2, 2 ),
 ( 0.000000000000000000, 1.000000000000000000 ),
 ( 0.000000000000000000, 1.000000000000000000 ),
 .UNSPECIFIED. ) 
 GEOMETRIC_REPRESENTATION_ITEM ( )  RATIONAL_B_SPLINE_SURFACE ( (
 ( 1.000000000000000000, 1.000000000000000000),
 ( 0.9729067724841187204, 0.9999501103223794596),
 ( 0.9729067724841187204, 0.9999501103223794596),
 ( 1.000000000000000000, 1.000000000000000000) ) ) 
 REPRESENTATION_ITEM ( '' )  SURFACE ( )  );
#1919 = VERTEX_POINT ( 'NONE', #59766 ) ;
#1920 = CARTESIAN_POINT ( 'NONE',  ( 0.2940133293163006978, 3.434477758206464948, 43.98232499659869177 ) ) ;
#1921 = CARTESIAN_POINT ( 'NONE',  ( 50.15577769773999961, 1.224646799147353256E-15, -10.00000000000000000 ) ) ;
#1922 = ORIENTED_EDGE ( 'NONE', *, *, #59059, .F. ) ;
#1923 = CARTESIAN_POINT ( 'NONE',  ( 1.231276596079887931, 41.42457922925077440, -6.425029704024191268 ) ) ;
#1924 = ORIENTED_EDGE ( 'NONE', *, *, #2309, .F. ) ;
#1925 = ORIENTED_EDGE ( 'NONE', *, *, #58983, .T. ) ;
#1926 = CARTESIAN_POINT ( 'NONE',  ( 0.9757892942422831117, -5.549787678908672639, 42.54806590760152574 ) ) ;
#1927 = ORIENTED_EDGE ( 'NONE', *, *, #21557, .T. ) ;
#1928 = CARTESIAN_POINT ( 'NONE',  ( 5.959547316686252039, -2.682663672454773440, -20.34955788964375856 ) ) ;
#1929 = B_SPLINE_CURVE_WITH_KNOTS ( 'NONE', 3,
 ( #55493, #21071, #12621, #6621 ),
 .UNSPECIFIED., .F., .F.,
 ( 4, 4 ),
 ( 0.000000000000000000, 0.004446090762761219402 ),
 .UNSPECIFIED. ) ;
#1930 = CARTESIAN_POINT ( 'NONE',  ( 3.782625744892855302, -38.26642674074366823, -17.40455941959752195 ) ) ;
#1931 = ORIENTED_EDGE ( 'NONE', *, *, #45023, .T. ) ;
#1932 = CARTESIAN_POINT ( 'NONE',  ( 1.231276596079887264, -21.83837404314831332, 35.78214904347716185 ) ) ;
#1933 = AXIS2_PLACEMENT_3D ( 'NONE', #51157, #46486, #60861 ) ;
#1934 = EDGE_CURVE ( 'NONE', #16409, #27021, #41097, .T. ) ;
#1935 = CARTESIAN_POINT ( 'NONE',  ( 3.783198216974390515, 41.98529422752528006, -9.462293521184431455 ) ) ;
#1936 = EDGE_LOOP ( 'NONE', ( #501, #5562, #42226, #18781, #54727 ) ) ;
#1937 = CARTESIAN_POINT ( 'NONE',  ( 0.1154773475650540254, 43.27575480954529752, -8.611194789937002270 ) ) ;
#1938 = VECTOR ( 'NONE', #21205, 1000.000000000000000 ) ;
#1939 = CARTESIAN_POINT ( 'NONE',  ( 49.80403646751975799, 12.23154873426529399, 2.580195994037977059 ) ) ;
#1940 = CARTESIAN_POINT ( 'NONE',  ( 4.549368137175248350, 42.82045902618772715, -3.018832571116098151 ) ) ;
#1941 = CARTESIAN_POINT ( 'NONE',  ( 0.9769922540276061440, 35.83105161777989878, 21.73631282094816797 ) ) ;
#1942 = VERTEX_POINT ( 'NONE', #41308 ) ;
#1943 = ORIENTED_EDGE ( 'NONE', *, *, #27256, .F. ) ;
#1944 = CARTESIAN_POINT ( 'NONE',  ( 0.1100053167205930632, 41.70112744323654397, 10.98799238780965659 ) ) ;
#1945 = CYLINDRICAL_SURFACE ( 'NONE', #29493, 5.000000000000000000 ) ;
#1946 = CARTESIAN_POINT ( 'NONE',  ( 0.2224561200757602386, -41.84032767736809433, 10.42482236669231099 ) ) ;
#1947 = VERTEX_POINT ( 'NONE', #27183 ) ;
#1948 = CARTESIAN_POINT ( 'NONE',  ( 2.533389852662419894, -42.95075564070678098, -9.627207363816017605 ) ) ;
#1949 = CARTESIAN_POINT ( 'NONE',  ( 4.967162193818132288, -24.30453456948087521, -35.57684288742000689 ) ) ;
#1950 = DIRECTION ( 'NONE',  ( -0.1024043820194934507, 0.7126273545981537394, -0.6940285268068185909 ) ) ;
#1951 = CARTESIAN_POINT ( 'NONE',  ( 0.6030672727741701600, -41.61859040196966930, -24.12926094633971275 ) ) ;
#1952 = VECTOR ( 'NONE', #27873, 1000.000000000000000 ) ;
#1953 = ORIENTED_EDGE ( 'NONE', *, *, #41986, .T. ) ;
#1954 = VERTEX_POINT ( 'NONE', #16877 ) ;
#1955 = CARTESIAN_POINT ( 'NONE',  ( 0.1064266418746774023, 15.98292515284405191, 40.05351192729366261 ) ) ;
#1956 = CARTESIAN_POINT ( 'NONE',  ( 0.1092355843206037486, 34.02913268098554056, 26.49036028133793508 ) ) ;
#1957 = CARTESIAN_POINT ( 'NONE',  ( -6.016104459813374383, 7.206059014950080943, 17.41090761020838329 ) ) ;
#1958 = CARTESIAN_POINT ( 'NONE',  ( 0.8753041380234465318, 49.05142151719384458, -2.257515230414630203 ) ) ;
#1959 = CARTESIAN_POINT ( 'NONE',  ( 0.1095718737110178004, 34.36877422440999652, -26.04820588677157289 ) ) ;
#1960 = EDGE_CURVE ( 'NONE', #36040, #30530, #35993, .T. ) ;
#1961 = CARTESIAN_POINT ( 'NONE',  ( 2.706805983486679779, -41.38491211916735324, -14.96880630539891399 ) ) ;
#1962 = CARTESIAN_POINT ( 'NONE',  ( 4.960156602257182357, 2.524999074837563917, 46.35381625054454702 ) ) ;
#1963 = ADVANCED_FACE ( 'NONE', ( #21874 ), #26877, .T. ) ;
#1964 = CARTESIAN_POINT ( 'NONE',  ( 4.691466044806102076, -19.42108863068351354, -40.13652286047886264 ) ) ;
#1965 = CARTESIAN_POINT ( 'NONE',  ( 0.6028618097248862329, -6.106174977919399005, 47.71844004092977087 ) ) ;
#1966 = EDGE_CURVE ( 'NONE', #5597, #24375, #43297, .T. ) ;
#1967 = LINE ( 'NONE', #58661, #24922 ) ;
#1968 = CARTESIAN_POINT ( 'NONE',  ( 4.691466044806102076, 42.32811009116555567, -14.01607102724497977 ) ) ;
#1969 = LINE ( 'NONE', #17635, #39073 ) ;
#1970 = CARTESIAN_POINT ( 'NONE',  ( 0.5549461598389364703, 41.57286777559680502, -14.72801277768148509 ) ) ;
#1971 = CARTESIAN_POINT ( 'NONE',  ( 0.5998501479064699549, -47.76154736470754614, -5.759754759340617092 ) ) ;
#1972 = FACE_OUTER_BOUND ( 'NONE', #29277, .T. ) ;
#1973 = CONTEXT_DEPENDENT_SHAPE_REPRESENTATION ( #45597, #25369 ) ;
#1974 = CARTESIAN_POINT ( 'NONE',  ( -6.057079549204054558, -17.34624894862984235, -8.362946760077846875 ) ) ;
#1975 = CARTESIAN_POINT ( 'NONE',  ( 0.3622758884714730732, 43.10531414739106282, -0.8252992914323589169 ) ) ;
#1976 = FACE_OUTER_BOUND ( 'NONE', #25358, .T. ) ;
#1977 = CARTESIAN_POINT ( 'NONE',  ( 0.5997462898726536595, 48.97040376101519144, -3.667585803694250135 ) ) ;
#1979 = ORIENTED_EDGE ( 'NONE', *, *, #19274, .T. ) ;
#1978 = CARTESIAN_POINT ( 'NONE',  ( -6.017396004339687465, -18.68211039806565310, 2.458362590802723791 ) ) ;
#1980 = VERTEX_POINT ( 'NONE', #40386 ) ;
#1981 = ADVANCED_FACE ( 'NONE', ( #3055 ), #20489, .F. ) ;
#1982 = VECTOR ( 'NONE', #50943, 1000.000000000000000 ) ;
#1983 = FACE_BOUND ( 'NONE', #59580, .T. ) ;
#1984 = CARTESIAN_POINT ( 'NONE',  ( 0.9268187852002115479, 3.245393988162387000, -43.96841765142595904 ) ) ;
#1985 = CARTESIAN_POINT ( 'NONE',  ( -6.016104459813371719, 18.68271063303494728, 2.454244026261157341 ) ) ;
#1986 = VERTEX_POINT ( 'NONE', #16555 ) ;
#1987 = EDGE_CURVE ( 'NONE', #50136, #9272, #47848, .T. ) ;
#1988 = VERTEX_POINT ( 'NONE', #18412 ) ;
#1989 = CARTESIAN_POINT ( 'NONE',  ( 1.000433927950261870, -23.10322705937726795, -34.96654940218871843 ) ) ;
#1990 = CARTESIAN_POINT ( 'NONE',  ( 0.7048096507298635682, -28.61383451045728066, 38.67623024743999594 ) ) ;
#1991 = CARTESIAN_POINT ( 'NONE',  ( -6.063463321072278589, -18.89860197674386200, -3.696389563355431562 ) ) ;
#1992 = ORIENTED_EDGE ( 'NONE', *, *, #10301, .F. ) ;
#1993 = ORIENTED_EDGE ( 'NONE', *, *, #31136, .F. ) ;
#1994 = CARTESIAN_POINT ( 'NONE',  ( 0.5804410086790514622, -44.48029469925801038, 14.86685021524586325 ) ) ;
#1995 = CARTESIAN_POINT ( 'NONE',  ( 1.157643937452369931, 36.47889976118223387, 20.64684350714105321 ) ) ;
#1996 = CARTESIAN_POINT ( 'NONE',  ( -6.016489644550737204, 2.455165042129735298, 18.68257207665197228 ) ) ;
#1997 = VERTEX_POINT ( 'NONE', #61599 ) ;
#1998 = CARTESIAN_POINT ( 'NONE',  ( 0.2940133293163009753, -2.218054141563334802, 44.06042198394310816 ) ) ;
#1999 = CARTESIAN_POINT ( 'NONE',  ( 0.5806925824938499181, -29.85799195566266917, -36.16244846134105018 ) ) ;
#2000 = EDGE_CURVE ( 'NONE', #19675, #29055, #27635, .T. ) ;
#2001 = LINE ( 'NONE', #21129, #4931 ) ;
#2002 = VERTEX_POINT ( 'NONE', #3970 ) ;
#2003 = VERTEX_POINT ( 'NONE', #47530 ) ;
#2004 = CARTESIAN_POINT ( 'NONE',  ( 0.5806925824938499181, 27.37593026015182218, 38.07598724570208049 ) ) ;
#2005 = CARTESIAN_POINT ( 'NONE',  ( 0.8760168074887090262, -23.27577685234627580, 42.09738177923914293 ) ) ;
#2006 = VERTEX_POINT ( 'NONE', #47225 ) ;
#2007 = CARTESIAN_POINT ( 'NONE',  ( 0.6029442701453591180, -7.751548539172897989, 48.49184179223475155 ) ) ;
#2008 = CARTESIAN_POINT ( 'NONE',  ( 0.5987334363312688534, -8.434467551029658949, 48.37791503984752239 ) ) ;
#2009 = B_SPLINE_CURVE_WITH_KNOTS ( 'NONE', 3,
 ( #59423, #21848, #12458, #50044, #16854, #22158, #21227, #31871, #60051, #40672, #8048, #17156, #26852, #36269, #13080, #36894, #41281, #60341, #46287 ),
 .UNSPECIFIED., .F., .F.,
 ( 4, 3, 3, 3, 3, 3, 4 ),
 ( 1.138109825968292890E-16, 0.0002618519381806228810, 0.0003927759815485970052, 0.0005237000248299436469, 0.0006546240681325004272, 0.0007855481115631334681, 0.0009699050456655086650 ),
 .UNSPECIFIED. ) ;
#2010 = ORIENTED_EDGE ( 'NONE', *, *, #41099, .T. ) ;
#2011 = CARTESIAN_POINT ( 'NONE',  ( 0.000000000000000000, 0.000000000000000000, 0.000000000000000000 ) ) ;
#2012 = CARTESIAN_POINT ( 'NONE',  ( 0.6024113833632039894, -35.42741226244881858, 34.00647481711914111 ) ) ;
#2013 =( BOUNDED_SURFACE ( )  B_SPLINE_SURFACE ( 3, 1, ( 
 ( #46893, #3929 ),
 ( #36562, #18375 ),
 ( #60325, #31533 ),
 ( #32787, #51864 ) ),
 .UNSPECIFIED., .F., .F., .F. ) 
 B_SPLINE_SURFACE_WITH_KNOTS ( ( 4, 4 ),
 ( 2, 2 ),
 ( 0.000000000000000000, 1.000000000000000000 ),
 ( 0.000000000000000000, 1.000000000000000000 ),
 .UNSPECIFIED. ) 
 GEOMETRIC_REPRESENTATION_ITEM ( )  RATIONAL_B_SPLINE_SURFACE ( (
 ( 1.000000000000000000, 1.000000000000000000),
 ( 0.9953485035131437453, 0.8621029689291515030),
 ( 0.9953485035131437453, 0.8621029689291515030),
 ( 1.000000000000000000, 1.000000000000000000) ) ) 
 REPRESENTATION_ITEM ( '' )  SURFACE ( )  );
#2014 = LINE ( 'NONE', #30525, #29451 ) ;
#2015 = VERTEX_POINT ( 'NONE', #27486 ) ;
#2016 = DIRECTION ( 'NONE',  ( 0.1024043820194936449, 0.9946559125373961585, -0.01315135725335497656 ) ) ;
#2017 = CARTESIAN_POINT ( 'NONE',  ( 0.8744876279028263033, 23.49358985382666631, -43.10917867646825385 ) ) ;
#2018 = ORIENTED_EDGE ( 'NONE', *, *, #8269, .F. ) ;
#2019 = CARTESIAN_POINT ( 'NONE',  ( 4.956445790443996025, 14.46717203539371610, 44.81337951368942640 ) ) ;
#2020 = CARTESIAN_POINT ( 'NONE',  ( 0.1073791018717483448, 30.14884492832389284, -30.83464511437107447 ) ) ;
#2021 = AXIS2_PLACEMENT_3D ( 'NONE', #34926, #30197, #50237 ) ;
#2022 = B_SPLINE_CURVE_WITH_KNOTS ( 'NONE', 3,
 ( #39689, #29330, #48441, #25252 ),
 .UNSPECIFIED., .F., .F.,
 ( 4, 4 ),
 ( 0.000000000000000000, 0.004444878191957668707 ),
 .UNSPECIFIED. ) ;
#2023 = ORIENTED_EDGE ( 'NONE', *, *, #47307, .T. ) ;
#2024 = CYLINDRICAL_SURFACE ( 'NONE', #46927, 2.649999999999992806 ) ;
#2025 = CARTESIAN_POINT ( 'NONE',  ( 0.1073791018717483448, -42.68962945260958008, 6.109314776651994627 ) ) ;
#2026 = B_SPLINE_CURVE_WITH_KNOTS ( 'NONE', 3,
 ( #32104, #37127, #27388, #55888 ),
 .UNSPECIFIED., .F., .F.,
 ( 4, 4 ),
 ( 4.336808689942017736E-19, 0.004048833967417082152 ),
 .UNSPECIFIED. ) ;
#2027 = CARTESIAN_POINT ( 'NONE',  ( 0.1073791018717483448, 25.86618856530710531, -34.50606437925521419 ) ) ;
#2028 = DIRECTION ( 'NONE',  ( -1.000000000000000000, -0.000000000000000000, -0.000000000000000000 ) ) ;
#2029 = CARTESIAN_POINT ( 'NONE',  ( 2.706805983486680223, 21.80916877957961475, 38.22481223581831244 ) ) ;
#2030 = FACE_OUTER_BOUND ( 'NONE', #31689, .T. ) ;
#2031 = DIRECTION ( 'NONE',  ( 1.000000000000000000, -0.000000000000000000, -0.000000000000000000 ) ) ;
#2032 = CARTESIAN_POINT ( 'NONE',  ( 0.1102144999581332746, -41.62223437741661769, -11.28312052188132952 ) ) ;
#2034 = ADVANCED_FACE ( 'NONE', ( #24026, #4272 ), #4895, .F. ) ;
#2033 = CARTESIAN_POINT ( 'NONE',  ( -6.063463321072278589, -19.21812676738395353, 1.218218384457574688 ) ) ;
#2035 = CARTESIAN_POINT ( 'NONE',  ( 3.660087539127320877, 8.130906407640051015, 47.34518630204115652 ) ) ;
#2036 = CARTESIAN_POINT ( 'NONE',  ( 0.3676999524040323597, 16.00695768809450215, -41.10629986868669761 ) ) ;
#2037 = ORIENTED_EDGE ( 'NONE', *, *, #46922, .T. ) ;
#2038 = ADVANCED_FACE ( 'NONE', ( #56602 ), #56882, .F. ) ;
#2039 = CARTESIAN_POINT ( 'NONE',  ( 5.960721111146673579, -14.50930005615026808, 14.51823969584074625 ) ) ;
#2040 = CARTESIAN_POINT ( 'NONE',  ( 4.553261556744875094, -3.993093339916522488, -43.74465420371214464 ) ) ;
#2041 = CARTESIAN_POINT ( 'NONE',  ( 1.000110580585051867, -34.92014527540499813, 23.17328066365460870 ) ) ;
#2042 = CARTESIAN_POINT ( 'NONE',  ( 4.962356264823608143, 0.000000000000000000, 0.000000000000000000 ) ) ;
#2043 = CARTESIAN_POINT ( 'NONE',  ( -6.079354080745853928, 18.62591919961132447, 4.885497847478016631 ) ) ;
#2044 = CARTESIAN_POINT ( 'NONE',  ( 0.9790724872846771065, -31.10874810710284422, 28.08168444360627092 ) ) ;
#2045 = DIRECTION ( 'NONE',  ( -1.000000000000000000, 0.000000000000000000, -6.982962677686266711E-15 ) ) ;
#2046 = CARTESIAN_POINT ( 'NONE',  ( 0.6031356219577718170, -44.41207482560220399, 18.49057407199378034 ) ) ;
#2047 = CARTESIAN_POINT ( 'NONE',  ( 0.6029303876144825880, 41.72757124235822346, -23.94027529185509451 ) ) ;
#2048 = CARTESIAN_POINT ( 'NONE',  ( 0.7245667037590721726, -29.92941129926923693, -37.65687897229916103 ) ) ;
#2050 = ORIENTED_EDGE ( 'NONE', *, *, #33871, .F. ) ;
#2049 = CARTESIAN_POINT ( 'NONE',  ( 1.231276596079881047, 41.91134057782998212, 0.8463462572780127147 ) ) ;
#2051 = VERTEX_POINT ( 'NONE', #42236 ) ;
#2052 = CARTESIAN_POINT ( 'NONE',  ( 1.154321485836933725, 42.43366804742927911, -6.418927614505664181 ) ) ;
#2053 = CARTESIAN_POINT ( 'NONE',  ( 0.08486401232817714080, 0.000000000000000000, 44.12552607296456131 ) ) ;
#2054 = CARTESIAN_POINT ( 'NONE',  ( 4.967162193818130511, 0.000000000000000000, 0.000000000000000000 ) ) ;
#2055 = ADVANCED_FACE ( 'NONE', ( #22792 ), #5640, .F. ) ;
#2056 = EDGE_LOOP ( 'NONE', ( #10118, #29574, #481, #3544 ) ) ;
#2057 = LINE ( 'NONE', #45626, #49516 ) ;
#2058 = CARTESIAN_POINT ( 'NONE',  ( 4.291220156522059348, -36.34793638197146493, 29.97026056072670741 ) ) ;
#2059 = CARTESIAN_POINT ( 'NONE',  ( 0.1104177457020373010, 41.65375561851285369, -11.16615714989265484 ) ) ;
#2060 = ORIENTED_EDGE ( 'NONE', *, *, #3949, .T. ) ;
#2061 = ORIENTED_EDGE ( 'NONE', *, *, #8099, .F. ) ;
#2062 = DIRECTION ( 'NONE',  ( -1.000000000000000000, 0.000000000000000000, 0.000000000000000000 ) ) ;
#2063 = CARTESIAN_POINT ( 'NONE',  ( 0.1104177457020373426, -11.16615714989280050, -41.65375561851281816 ) ) ;
#2064 = CARTESIAN_POINT ( 'NONE',  ( 0.6029442701453591180, 37.44910241782426397, 31.76649104414250147 ) ) ;
#2065 = ORIENTED_EDGE ( 'NONE', *, *, #35663, .F. ) ;
#2066 = VERTEX_POINT ( 'NONE', #14033 ) ;
#2067 = CARTESIAN_POINT ( 'NONE',  ( 0.5786265663353196143, -0.7221568112309819654, 47.89572889566445468 ) ) ;
#2068 = ORIENTED_EDGE ( 'NONE', *, *, #57480, .F. ) ;
#2069 = AXIS2_PLACEMENT_3D ( 'NONE', #36760, #8523, #46159 ) ;
#2070 = LINE ( 'NONE', #31847, #33940 ) ;
#2071 = CARTESIAN_POINT ( 'NONE',  ( 0.9740398440564312921, 41.33716823241947935, -11.50548031350398759 ) ) ;
#2072 = ORIENTED_EDGE ( 'NONE', *, *, #52458, .F. ) ;
#2073 = CARTESIAN_POINT ( 'NONE',  ( -1.500000000000001332, 0.000000000000000000, 0.000000000000000000 ) ) ;
#2074 = CARTESIAN_POINT ( 'NONE',  ( -6.079354080745853928, 15.43131048252518944, -11.51814273396845323 ) ) ;
#2075 = VERTEX_POINT ( 'NONE', #52208 ) ;
#2076 = CARTESIAN_POINT ( 'NONE',  ( 0.8751705887134423323, 23.27176129838367302, 42.09020928323383259 ) ) ;
#2077 = CARTESIAN_POINT ( 'NONE',  ( 0.8551540677456834771, -28.44084013485144879, 38.56334384152421535 ) ) ;
#2078 = CARTESIAN_POINT ( 'NONE',  ( -5.283180000000052168, 0.000000000000000000, 15.43999999999999240 ) ) ;
#2079 = CARTESIAN_POINT ( 'NONE',  ( 2.643462169533613793, -19.65219740572159424, -43.83256147628726040 ) ) ;
#2080 = ADVANCED_FACE ( 'NONE', ( #4580 ), #61294, .F. ) ;
#2081 = VERTEX_POINT ( 'NONE', #13101 ) ;
#2082 = EDGE_CURVE ( 'NONE', #39212, #3487, #48118, .T. ) ;
#2083 = DIRECTION ( 'NONE',  ( 0.09722883295013594329, 0.8382159563662527901, 0.5366009360187167232 ) ) ;
#2084 = CARTESIAN_POINT ( 'NONE',  ( 0.6025881611877910160, 44.52856035602907525, -18.20817581200370228 ) ) ;
#2085 = ORIENTED_EDGE ( 'NONE', *, *, #15130, .F. ) ;
#2086 = CARTESIAN_POINT ( 'NONE',  ( 0.2224561200757619595, -31.02237548791974220, 29.94832483817983970 ) ) ;
#2087 =( BOUNDED_SURFACE ( )  B_SPLINE_SURFACE ( 3, 1, ( 
 ( #48643, #44593 ),
 ( #39275, #10756 ),
 ( #5094, #29846 ),
 ( #714, #19855 ) ),
 .UNSPECIFIED., .F., .F., .F. ) 
 B_SPLINE_SURFACE_WITH_KNOTS ( ( 4, 4 ),
 ( 2, 2 ),
 ( 0.000000000000000000, 1.000000000000000000 ),
 ( 0.000000000000000000, 1.000000000000000000 ),
 .UNSPECIFIED. ) 
 GEOMETRIC_REPRESENTATION_ITEM ( )  RATIONAL_B_SPLINE_SURFACE ( (
 ( 1.000000000000000000, 1.000000000000000000),
 ( 0.9754377213608244057, 0.9999580625633939235),
 ( 0.9754377213608244057, 0.9999580625633939235),
 ( 1.000000000000000000, 1.000000000000000000) ) ) 
 REPRESENTATION_ITEM ( '' )  SURFACE ( )  );
#2088 = ORIENTED_EDGE ( 'NONE', *, *, #55043, .T. ) ;
#2089 = CARTESIAN_POINT ( 'NONE',  ( 0.5839880159502364165, -18.37091806000265493, 44.23273844814454492 ) ) ;
#2090 = ADVANCED_FACE ( 'NONE', ( #32828 ), #4079, .T. ) ;
#2091 = VERTEX_POINT ( 'NONE', #51585 ) ;
#2092 = CARTESIAN_POINT ( 'NONE',  ( 4.962356264823602814, 42.01891079680549979, 2.376285612557970772 ) ) ;
#2093 = CARTESIAN_POINT ( 'NONE',  ( 0.9785694773339239649, 24.67983040667081340, 33.87095181438870384 ) ) ;
#2094 = CARTESIAN_POINT ( 'NONE',  ( -2.601141883200665639, 5.573165628699342733, -13.84684990690925943 ) ) ;
#2095 = EDGE_LOOP ( 'NONE', ( #22526, #10405, #52719, #3876 ) ) ;
#2096 = CARTESIAN_POINT ( 'NONE',  ( 0.5839879882012675161, 6.251708210202064464, 47.48620708510744493 ) ) ;
#2097 = DIRECTION ( 'NONE',  ( -1.000000000000000000, -0.000000000000000000, -0.000000000000000000 ) ) ;
#2098 = CARTESIAN_POINT ( 'NONE',  ( 0.1129192098497447394, 14.78321943369649283, -41.57412910645673776 ) ) ;
#2099 = EDGE_LOOP ( 'NONE', ( #27603, #15245, #51859, #2349 ) ) ;
#2100 = EDGE_LOOP ( 'NONE', ( #50022, #60282, #17987, #56722 ) ) ;
#2101 = CARTESIAN_POINT ( 'NONE',  ( 0.6254087463353908971, -37.74264085326077378, 29.82831063981268116 ) ) ;
#2102 = CARTESIAN_POINT ( 'NONE',  ( 1.296416391601052487, 30.44260198708226639, 31.86777931284597187 ) ) ;
#2103 = CARTESIAN_POINT ( 'NONE',  ( 4.833616638992205949, 25.31740731790842602, 38.70560126501871423 ) ) ;
#2104 = CARTESIAN_POINT ( 'NONE',  ( 1.154321485836933725, -0.8253076867715974929, -42.90848031452337352 ) ) ;
#2105 = CARTESIAN_POINT ( 'NONE',  ( 0.5834584762367737154, -30.13807749983152817, -35.92954597023653918 ) ) ;
#2106 = CARTESIAN_POINT ( 'NONE',  ( 0.7044674535453004927, 40.69315356317313359, -27.49308960256953682 ) ) ;
#2107 = ORIENTED_EDGE ( 'NONE', *, *, #50234, .F. ) ;
#2108 = EDGE_CURVE ( 'NONE', #12977, #14660, #15667, .T. ) ;
#2109 = CARTESIAN_POINT ( 'NONE',  ( -4.214292481396491930, -11.25702090725073035, -1.199999999999999956 ) ) ;
#2110 = CARTESIAN_POINT ( 'NONE',  ( 4.956445790444004018, -45.55738122058073003, 11.91902120403828036 ) ) ;
#2111 = ORIENTED_EDGE ( 'NONE', *, *, #18060, .T. ) ;
#2112 = EDGE_CURVE ( 'NONE', #22007, #56473, #2202, .T. ) ;
#2113 = DIRECTION ( 'NONE',  ( -1.000000000000000000, -1.836909530733573776E-16, 1.925929944387235853E-32 ) ) ;
#2114 = CARTESIAN_POINT ( 'NONE',  ( 0.6016117650947691020, 44.39439963300118563, 20.99257810441308081 ) ) ;
#2115 = CARTESIAN_POINT ( 'NONE',  ( 0.5824935313925952984, 45.32465144643322930, 12.03802925371000399 ) ) ;
#2116 = B_SPLINE_CURVE_WITH_KNOTS ( 'NONE', 3,
 ( #48192, #38193, #37570, #47264, #18145, #4008, #23147, #33174, #56332, #52559, #52248, #9037, #9345, #9653, #32870, #4940, #33797, #9976, #32555 ),
 .UNSPECIFIED., .F., .F.,
 ( 4, 3, 3, 3, 3, 3, 4 ),
 ( 9.541595121948225732E-18, 0.0002732106629380623777, 0.0004098138914053767873, 0.0005464171197651445213, 0.0006830203481512576091, 0.0008196235766963660182, 0.001011968216111140077 ),
 .UNSPECIFIED. ) ;
#2117 = CARTESIAN_POINT ( 'NONE',  ( 5.901764892641307547, 13.89173340560966352, 46.95754689533032433 ) ) ;
#2118 = CARTESIAN_POINT ( 'NONE',  ( 0.6254087463353916743, -47.60024110474256531, 6.960754339421005632 ) ) ;
#2119 = ADVANCED_FACE ( 'NONE', ( #39080 ), #28893, .F. ) ;
#2120 = FACE_OUTER_BOUND ( 'NONE', #57558, .T. ) ;
#2121 = CONICAL_SURFACE ( 'NONE', #54163, 42.08604991992415023, 1.569615340895231137 ) ;
#2122 = VECTOR ( 'NONE', #21712, 1000.000000000000000 ) ;
#2123 = CARTESIAN_POINT ( 'NONE',  ( -6.016761891674564211, -18.84319130225482297, 0.003433883959717882409 ) ) ;
#2124 = LINE ( 'NONE', #39775, #58597 ) ;
#2125 = CARTESIAN_POINT ( 'NONE',  ( 0.8751705887134423323, -44.76769609654249393, 17.57879340691464165 ) ) ;
#2126 = CARTESIAN_POINT ( 'NONE',  ( -4.000000000000000000, 2.309401076758496263, -0.3572655899081631503 ) ) ;
#2127 = CARTESIAN_POINT ( 'NONE',  ( 0.9789889208857696090, 9.808795407786901066, 40.74460001878221505 ) ) ;
#2128 = EDGE_CURVE ( 'NONE', #48540, #52878, #3114, .T. ) ;
#2129 = CARTESIAN_POINT ( 'NONE',  ( 3.782625744892851749, 13.48684605329171049, -39.81636708226672283 ) ) ;
#2130 = CARTESIAN_POINT ( 'NONE',  ( -3.282060897439244229, -10.26526840094481052, -2.999999999999990674 ) ) ;
#2131 = EDGE_LOOP ( 'NONE', ( #49457, #40864, #51409, #49024 ) ) ;
#2132 = LINE ( 'NONE', #15659, #58862 ) ;
#2133 = CARTESIAN_POINT ( 'NONE',  ( 0.9758171775293911221, -39.64453667157735595, -16.41489794146167114 ) ) ;
#2134 = CARTESIAN_POINT ( 'NONE',  ( 3.678748215320120529, -21.50126778036843334, -44.00350324845027927 ) ) ;
#2135 = CARTESIAN_POINT ( 'NONE',  ( 4.975610109902397937, -5.269241389991576874, 48.62802178077752302 ) ) ;
#2136 = ORIENTED_EDGE ( 'NONE', *, *, #9331, .F. ) ;
#2137 = B_SPLINE_CURVE_WITH_KNOTS ( 'NONE', 3,
 ( #57787, #10203, #29299, #48410 ),
 .UNSPECIFIED., .F., .F.,
 ( 4, 4 ),
 ( 2.380737581782212780E-07, 0.002336974151641539946 ),
 .UNSPECIFIED. ) ;
#2138 = CARTESIAN_POINT ( 'NONE',  ( 2.624215991343620935, -47.98682984381861871, 1.411420423865310747 ) ) ;
#2139 = CARTESIAN_POINT ( 'NONE',  ( 0.6016118706126978299, 28.38023484439529298, -40.07634370749035213 ) ) ;
#2140 = CARTESIAN_POINT ( 'NONE',  ( 3.270143674763207553, 11.02405647745181305, -8.113405361969396878 ) ) ;
#2141 = ORIENTED_EDGE ( 'NONE', *, *, #14391, .T. ) ;
#2142 = CARTESIAN_POINT ( 'NONE',  ( 1.827119703190777544, 17.60659059422121686, 39.28489939038895074 ) ) ;
#2143 = VERTEX_POINT ( 'NONE', #827 ) ;
#2144 = EDGE_CURVE ( 'NONE', #40793, #41494, #47846, .T. ) ;
#2145 = CARTESIAN_POINT ( 'NONE',  ( 4.975610109902397937, 34.73360008816180056, -34.43873447229760387 ) ) ;
#2146 = CARTESIAN_POINT ( 'NONE',  ( 5.895596859100789899, 20.06773179721813349, 1.346968346847024822 ) ) ;
#2147 = EDGE_LOOP ( 'NONE', ( #59872, #5116, #9175, #58869 ) ) ;
#2148 = CARTESIAN_POINT ( 'NONE',  ( 4.303969348037246512, -30.97035057417686232, 36.81598326424538925 ) ) ;
#2149 = ORIENTED_EDGE ( 'NONE', *, *, #43157, .T. ) ;
#2150 = CARTESIAN_POINT ( 'NONE',  ( 1.231276596079887931, -35.03243822710496858, -23.02183839058345072 ) ) ;
#2151 = CARTESIAN_POINT ( 'NONE',  ( 0.1158516988532803660, 20.45274844683495985, 39.09766284323509922 ) ) ;
#2152 = ADVANCED_FACE ( 'NONE', ( #10864 ), #14113, .F. ) ;
#2153 = ORIENTED_EDGE ( 'NONE', *, *, #33275, .F. ) ;
#2154 = B_SPLINE_CURVE_WITH_KNOTS ( 'NONE', 3,
 ( #7739, #39367, #9594, #4881, #19636, #5188 ),
 .UNSPECIFIED., .F., .F.,
 ( 4, 2, 4 ),
 ( 0.004120275011746849653, 0.005288420935197133549, 0.006456566858647416578 ),
 .UNSPECIFIED. ) ;
#2155 = VECTOR ( 'NONE', #44445, 1000.000000000000114 ) ;
#2156 = ORIENTED_EDGE ( 'NONE', *, *, #11387, .F. ) ;
#2157 = EDGE_CURVE ( 'NONE', #55402, #25319, #24135, .T. ) ;
#2158 = LINE ( 'NONE', #58242, #51760 ) ;
#2159 = CARTESIAN_POINT ( 'NONE',  ( 0.1156867017252034557, -1.539136465540023035, 44.09732266493773523 ) ) ;
#2160 = AXIS2_PLACEMENT_3D ( 'NONE', #3680, #4593, #22815 ) ;
#2161 = B_SPLINE_CURVE_WITH_KNOTS ( 'NONE', 3,
 ( #10477, #34596, #53661, #10791 ),
 .UNSPECIFIED., .F., .F.,
 ( 4, 4 ),
 ( 1.440969542111313559E-17, 0.004042984057420977162 ),
 .UNSPECIFIED. ) ;
#2162 = ORIENTED_EDGE ( 'NONE', *, *, #27048, .T. ) ;
#2163 = EDGE_CURVE ( 'NONE', #6622, #2619, #47074, .T. ) ;
#2164 =( BOUNDED_SURFACE ( )  B_SPLINE_SURFACE ( 3, 1, ( 
 ( #12359, #31446 ),
 ( #50542, #7621 ),
 ( #45881, #2929 ),
 ( #12984, #47399 ) ),
 .UNSPECIFIED., .F., .F., .F. ) 
 B_SPLINE_SURFACE_WITH_KNOTS ( ( 4, 4 ),
 ( 2, 2 ),
 ( 0.000000000000000000, 1.000000000000000000 ),
 ( 0.000000000000000000, 1.000000000000000000 ),
 .UNSPECIFIED. ) 
 GEOMETRIC_REPRESENTATION_ITEM ( )  RATIONAL_B_SPLINE_SURFACE ( (
 ( 1.000000000000000000, 1.000000000000000000),
 ( 0.7282232189291693025, 0.9929344683865674037),
 ( 0.7282232189291693025, 0.9929344683865674037),
 ( 1.000000000000000000, 1.000000000000000000) ) ) 
 REPRESENTATION_ITEM ( '' )  SURFACE ( )  );
#2165 = ORIENTED_EDGE ( 'NONE', *, *, #31844, .T. ) ;
#2166 = CARTESIAN_POINT ( 'NONE',  ( 4.956445790443988031, 0.000000000000000000, 0.000000000000000000 ) ) ;
#2168 = EDGE_CURVE ( 'NONE', #59631, #48937, #1424, .T. ) ;
#2167 = CARTESIAN_POINT ( 'NONE',  ( -6.078075953587585900, -17.35139778253845932, 8.350099953848184597 ) ) ;
#2169 = CARTESIAN_POINT ( 'NONE',  ( 0.6026112563231247332, -25.30784345655240486, -42.08389305283965598 ) ) ;
#2170 = CARTESIAN_POINT ( 'NONE',  ( 0.5832655196449135770, 32.76499612651431192, -33.55130715490577131 ) ) ;
#2171 = FACE_OUTER_BOUND ( 'NONE', #44128, .T. ) ;
#2172 = ORIENTED_EDGE ( 'NONE', *, *, #37571, .T. ) ;
#2173 = CARTESIAN_POINT ( 'NONE',  ( 5.860006189529234355, -47.30296539008831047, 9.426589201135334051 ) ) ;
#2174 = CARTESIAN_POINT ( 'NONE',  ( -6.072942160501519027, 16.78547611690390440, -9.436734277167554197 ) ) ;
#2175 = VERTEX_POINT ( 'NONE', #39691 ) ;
#2176 = ORIENTED_EDGE ( 'NONE', *, *, #54993, .F. ) ;
#2177 = CARTESIAN_POINT ( 'NONE',  ( 2.643462169533600914, -32.97543604874651635, -34.93025802711714789 ) ) ;
#2178 = CARTESIAN_POINT ( 'NONE',  ( 0.5980271706414711508, -35.76345691233170498, 33.66042769367994936 ) ) ;
#2179 = CARTESIAN_POINT ( 'NONE',  ( 0.8557997880470697982, 17.48760788519276943, -44.60232077416669227 ) ) ;
#2180 = ORIENTED_EDGE ( 'NONE', *, *, #12497, .T. ) ;
#2181 = CARTESIAN_POINT ( 'NONE',  ( 3.238931869106853600, -29.07925862215153501, 31.66562935062887263 ) ) ;
#2182 = DIRECTION ( 'NONE',  ( -1.000000000000000000, -0.000000000000000000, -0.000000000000000000 ) ) ;
#2183 = CARTESIAN_POINT ( 'NONE',  ( 51.83055647397077337, 12.28729589684768264, 2.298227778111301856 ) ) ;
#2184 = CARTESIAN_POINT ( 'NONE',  ( 0.6027935024548037868, -29.14731236071041920, -38.27223087442838079 ) ) ;
#2185 = EDGE_CURVE ( 'NONE', #36718, #55958, #58742, .T. ) ;
#2186 = ORIENTED_EDGE ( 'NONE', *, *, #37368, .T. ) ;
#2187 = CARTESIAN_POINT ( 'NONE',  ( -6.001507490154111224, 13.33564355450126904, -13.31361390284146218 ) ) ;
#2188 = VERTEX_POINT ( 'NONE', #44695 ) ;
#2189 = DIRECTION ( 'NONE',  ( -1.000000000000000000, -0.000000000000000000, -0.000000000000000000 ) ) ;
#2190 = CARTESIAN_POINT ( 'NONE',  ( 0.8557997880470690211, -33.22501220301925429, 34.51495345639537504 ) ) ;
#2191 = ADVANCED_FACE ( 'NONE', ( #38768 ), #11718, .F. ) ;
#2192 = CARTESIAN_POINT ( 'NONE',  ( 0.7056759521545007408, 17.64077833824084607, -43.45747080466188805 ) ) ;
#2193 = ORIENTED_EDGE ( 'NONE', *, *, #58111, .F. ) ;
#2194 = DIRECTION ( 'NONE',  ( -1.000000000000000000, -0.000000000000000000, -0.000000000000000000 ) ) ;
#2195 = CARTESIAN_POINT ( 'NONE',  ( 5.860006189529246790, 36.27483683749480292, -31.78942168514526401 ) ) ;
#2196 = CARTESIAN_POINT ( 'NONE',  ( 0.1140933569871965397, -35.58732562960275914, 26.08624550633002315 ) ) ;
#2197 = CARTESIAN_POINT ( 'NONE',  ( 0.9754642270333682141, 37.24735125696685856, -21.30186789325715679 ) ) ;
#2198 = CARTESIAN_POINT ( 'NONE',  ( 5.895596859100789899, 19.71057157537860149, -4.002693016503341639 ) ) ;
#2199 = CARTESIAN_POINT ( 'NONE',  ( -2.708315649062910779, 12.54007339125004883, 7.544341609840020446 ) ) ;
#2200 = ADVANCED_FACE ( 'NONE', ( #26480 ), #20861, .F. ) ;
#2201 = CARTESIAN_POINT ( 'NONE',  ( 0.1135584504625008900, -43.70468290122602895, -6.070646146707417756 ) ) ;
#2202 = B_SPLINE_CURVE_WITH_KNOTS ( 'NONE', 3,
 ( #33752, #5506, #10545, #43465, #1127, #19963, #53132, #29640, #34988, #20265, #11168, #29037, #34666, #49063, #25254, #5808 ),
 .UNSPECIFIED., .F., .F.,
 ( 4, 3, 3, 3, 3, 4 ),
 ( 2.194378057379452319E-17, 0.0002612764279487765238, 0.0003919131003184808172, 0.0005225497727000681832, 0.0007837925190632486069, 0.001045051706266716300 ),
 .UNSPECIFIED. ) ;
#2203 = CIRCLE ( 'NONE', #18248, 6.866799999999992465 ) ;
#2204 = CARTESIAN_POINT ( 'NONE',  ( 0.6064515330803585957, -7.098679639542389452, 46.35669405180046709 ) ) ;
#2205 = CIRCLE ( 'NONE', #37265, 43.92652462719577500 ) ;
#2206 = ADVANCED_FACE ( 'NONE', ( #20868 ), #39724, .F. ) ;
#2207 = CARTESIAN_POINT ( 'NONE',  ( 0.1073791018717578927, 33.91564619577771111, 26.63563652260178927 ) ) ;
#2208 = CARTESIAN_POINT ( 'NONE',  ( 0.1157506346131639274, 37.03045437084058733, 23.99345971076133566 ) ) ;
#2209 = VERTEX_POINT ( 'NONE', #7997 ) ;
#2210 = CARTESIAN_POINT ( 'NONE',  ( -2.739355103387247858, -2.641750642666087945, 14.69247155835226870 ) ) ;
#2211 = CARTESIAN_POINT ( 'NONE',  ( 0.5832367798473397924, 46.19266341874894977, 12.65931911325620263 ) ) ;
#2212 = DIRECTION ( 'NONE',  ( -1.000000000000000000, -0.000000000000000000, -0.000000000000000000 ) ) ;
#2213 = ORIENTED_EDGE ( 'NONE', *, *, #10690, .F. ) ;
#2214 = CARTESIAN_POINT ( 'NONE',  ( 4.975801465491695552, 8.787181743660156030, -47.10002938642133330 ) ) ;
#2215 = CARTESIAN_POINT ( 'NONE',  ( 1.154321485836933725, -4.782433484301485294, 42.64911658695774577 ) ) ;
#2216 = B_SPLINE_CURVE_WITH_KNOTS ( 'NONE', 3,
 ( #11329, #16334, #49530, #6585 ),
 .UNSPECIFIED., .F., .F.,
 ( 4, 4 ),
 ( 0.000000000000000000, 0.004444103432399266161 ),
 .UNSPECIFIED. ) ;
#2217 = DIRECTION ( 'NONE',  ( 1.000000000000000000, 0.000000000000000000, 0.000000000000000000 ) ) ;
#2218 = B_SPLINE_CURVE_WITH_KNOTS ( 'NONE', 3,
 ( #61618, #20213, #3990, #29589 ),
 .UNSPECIFIED., .F., .F.,
 ( 4, 4 ),
 ( 0.000000000000000000, 0.005014147105413705591 ),
 .UNSPECIFIED. ) ;
#2219 = ORIENTED_EDGE ( 'NONE', *, *, #2595, .F. ) ;
#2220 = LINE ( 'NONE', #7539, #50037 ) ;
#2221 = CARTESIAN_POINT ( 'NONE',  ( -6.016761891674565099, -13.32172022638582121, -13.32657647165369141 ) ) ;
#2222 = VERTEX_POINT ( 'NONE', #50589 ) ;
#2223 = CARTESIAN_POINT ( 'NONE',  ( 0.6024113833632039894, 10.71508360385645631, 47.92419902787352015 ) ) ;
#2224 = ORIENTED_EDGE ( 'NONE', *, *, #627, .F. ) ;
#2225 = EDGE_LOOP ( 'NONE', ( #39572, #53306, #36706, #33179 ) ) ;
#2226 = CARTESIAN_POINT ( 'NONE',  ( 0.9756354156337463390, -5.729847988735645714, 42.52418499698892873 ) ) ;
#2227 = EDGE_CURVE ( 'NONE', #41115, #11845, #26858, .T. ) ;
#2228 = VERTEX_POINT ( 'NONE', #27108 ) ;
#2229 = CARTESIAN_POINT ( 'NONE',  ( -1.500000000000001332, 0.000000000000000000, -6.728125000000022560 ) ) ;
#2230 = PRODUCT_DEFINITION_SHAPE ( 'NONE', 'NONE',  #12658 ) ;
#2231 = B_SPLINE_CURVE_WITH_KNOTS ( 'NONE', 3,
 ( #2235, #20754, #44274, #6605, #5685, #58947 ),
 .UNSPECIFIED., .F., .F.,
 ( 4, 2, 4 ),
 ( 2.504504451673693158E-17, 0.0002293755540694321588, 0.0004587511081388392724 ),
 .UNSPECIFIED. ) ;
#2232 = CARTESIAN_POINT ( 'NONE',  ( 2.301430502907646947, 43.86847929982158689, 19.56449039932746459 ) ) ;
#2233 = ORIENTED_EDGE ( 'NONE', *, *, #57194, .T. ) ;
#2234 = ADVANCED_FACE ( 'NONE', ( #31183 ), #32945, .F. ) ;
#2235 = CARTESIAN_POINT ( 'NONE',  ( 0.1129192098497455998, 37.24220309526837980, -23.66368729500826618 ) ) ;
#2236 = CARTESIAN_POINT ( 'NONE',  ( 0.8554163680231720024, 46.36773742900852113, -7.158100224664473821 ) ) ;
#2237 = ADVANCED_FACE ( 'NONE', ( #40615 ), #35322, .F. ) ;
#2238 = ORIENTED_EDGE ( 'NONE', *, *, #32665, .T. ) ;
#2239 = EDGE_CURVE ( 'NONE', #28569, #2327, #55116, .T. ) ;
#2240 = CARTESIAN_POINT ( 'NONE',  ( 0.6017667736363750963, -18.73201910948690596, 44.31084570541168688 ) ) ;
#2241 = CARTESIAN_POINT ( 'NONE',  ( 5.960221823109900008, -19.82761049839338696, -5.307149561568015095 ) ) ;
#2242 = CARTESIAN_POINT ( 'NONE',  ( 0.1129192098497447394, 4.719118110134695954, 43.87119455916095490 ) ) ;
#2243 = FACE_OUTER_BOUND ( 'NONE', #31690, .T. ) ;
#2245 = EDGE_CURVE ( 'NONE', #24034, #37726, #33639, .T. ) ;
#2244 = EDGE_LOOP ( 'NONE', ( #57865, #19145, #28472, #20033 ) ) ;
#2246 = ORIENTED_EDGE ( 'NONE', *, *, #15858, .T. ) ;
#2247 = CIRCLE ( 'NONE', #57236, 48.91267123290010943 ) ;
#2248 = CARTESIAN_POINT ( 'NONE',  ( 0.5809828226811617480, -37.66417181417530458, -29.58751527316218954 ) ) ;
#2249 = AXIS2_PLACEMENT_3D ( 'NONE', #25761, #35180, #20447 ) ;
#2250 = FACE_OUTER_BOUND ( 'NONE', #32718, .T. ) ;
#2251 = EDGE_CURVE ( 'NONE', #24292, #47165, #45934, .T. ) ;
#2252 = CARTESIAN_POINT ( 'NONE',  ( 3.559346040607745287, 13.24178938536624450, -41.92952772707547382 ) ) ;
#2253 = ORIENTED_EDGE ( 'NONE', *, *, #27298, .T. ) ;
#2254 = CARTESIAN_POINT ( 'NONE',  ( 0.5819845079324655890, -46.37938935563221321, -11.95724301473555684 ) ) ;
#2255 = CARTESIAN_POINT ( 'NONE',  ( 5.838029081930957709, 7.836690858011984950, -46.57951625498993309 ) ) ;
#2256 = CARTESIAN_POINT ( 'NONE',  ( 1.000433927950264756, 41.44279064093520049, -6.238091177953354993 ) ) ;
#2257 = CARTESIAN_POINT ( 'NONE',  ( 0.5800708057587390387, 29.65250565429499474, -37.61306623599811161 ) ) ;
#2258 = ORIENTED_EDGE ( 'NONE', *, *, #41131, .F. ) ;
#2259 = ORIENTED_EDGE ( 'NONE', *, *, #36823, .F. ) ;
#2260 = CARTESIAN_POINT ( 'NONE',  ( -31.75000000000000000, 0.000000000000000000, 0.000000000000000000 ) ) ;
#2261 = CARTESIAN_POINT ( 'NONE',  ( 0.9754402186311968981, -16.24692483025446066, 39.71365199966008674 ) ) ;
#2262 = B_SPLINE_CURVE_WITH_KNOTS ( 'NONE', 3,
 ( #36958, #16595, #45731, #2781, #45125, #54784, #35722, #56023, #7159, #21913, #11919, #50703, #30675, #50104, #55401, #2474, #41646, #36035, #41348 ),
 .UNSPECIFIED., .F., .F.,
 ( 4, 3, 3, 3, 3, 3, 4 ),
 ( 1.138109825968292890E-16, 0.0002618519381806232063, 0.0003927759815485936442, 0.0005237000248299411532, 0.0006546240681324906694, 0.0007855481115631298902, 0.0009699050456655105082 ),
 .UNSPECIFIED. ) ;
#2263 = CARTESIAN_POINT ( 'NONE',  ( 0.6252788684277227338, -49.10165704764342820, 0.6867360113443859992 ) ) ;
#2264 =( BOUNDED_SURFACE ( )  B_SPLINE_SURFACE ( 3, 1, ( 
 ( #50633, #49720 ),
 ( #17448, #26844 ),
 ( #50036, #40356 ),
 ( #11846, #11518 ) ),
 .UNSPECIFIED., .F., .F., .F. ) 
 B_SPLINE_SURFACE_WITH_KNOTS ( ( 4, 4 ),
 ( 2, 2 ),
 ( 0.000000000000000000, 1.000000000000000000 ),
 ( 0.000000000000000000, 1.000000000000000000 ),
 .UNSPECIFIED. ) 
 GEOMETRIC_REPRESENTATION_ITEM ( )  RATIONAL_B_SPLINE_SURFACE ( (
 ( 1.000000000000000000, 1.000000000000000000),
 ( 0.9754377213608244057, 0.9999580625633939235),
 ( 0.9754377213608244057, 0.9999580625633939235),
 ( 1.000000000000000000, 1.000000000000000000) ) ) 
 REPRESENTATION_ITEM ( '' )  SURFACE ( )  );
#2265 = VECTOR ( 'NONE', #24584, 1000.000000000000000 ) ;
#2266 = CARTESIAN_POINT ( 'NONE',  ( 3.727782113643637096, -14.54354975905613045, -41.48810596197220946 ) ) ;
#2267 = CARTESIAN_POINT ( 'NONE',  ( 3.782625744892853525, 21.69837273921715948, 36.00581514929220361 ) ) ;
#2268 = CARTESIAN_POINT ( 'NONE',  ( 0.8744876279028306332, 44.61213666265828692, 20.49651952824657286 ) ) ;
#2269 = CARTESIAN_POINT ( 'NONE',  ( 5.974727161628369032, -2.694421823323069454, 20.34732802718242795 ) ) ;
#2270 = CARTESIAN_POINT ( 'NONE',  ( 3.680882792899938138, 8.091276083384761009, 47.28852514876959390 ) ) ;
#2271 = CARTESIAN_POINT ( 'NONE',  ( -49.49999999999975842, -5.000000000000000000, 6.123233995736873765E-16 ) ) ;
#2272 = CARTESIAN_POINT ( 'NONE',  ( -2.569797478183783568, -12.89088113963431326, -6.924386868080802060 ) ) ;
#2273 = DIRECTION ( 'NONE',  ( 0.07906939808003035641, -0.3507354328807343324, -0.9331305837926573421 ) ) ;
#2275 = B_SPLINE_CURVE_WITH_KNOTS ( 'NONE', 3,
 ( #21622, #11296, #59508, #45450 ),
 .UNSPECIFIED., .F., .F.,
 ( 4, 4 ),
 ( 1.409462824231155764E-18, 0.004446298630425050274 ),
 .UNSPECIFIED. ) ;
#2274 = CARTESIAN_POINT ( 'NONE',  ( 0.8744876279028306332, 44.61213666265828692, 20.49651952824657286 ) ) ;
#2276 = CARTESIAN_POINT ( 'NONE',  ( 4.956653778116992370, 14.93973939759951541, -45.71126949320233734 ) ) ;
#2277 = CARTESIAN_POINT ( 'NONE',  ( 5.958863334805807099, -2.677925489610788023, 20.35021240744029924 ) ) ;
#2278 =( BOUNDED_SURFACE ( )  B_SPLINE_SURFACE ( 3, 1, ( 
 ( #43301, #18874 ),
 ( #43613, #38297 ),
 ( #52975, #10078 ),
 ( #19796, #33283 ) ),
 .UNSPECIFIED., .F., .F., .F. ) 
 B_SPLINE_SURFACE_WITH_KNOTS ( ( 4, 4 ),
 ( 2, 2 ),
 ( 0.000000000000000000, 1.000000000000000000 ),
 ( 0.000000000000000000, 1.000000000000000000 ),
 .UNSPECIFIED. ) 
 GEOMETRIC_REPRESENTATION_ITEM ( )  RATIONAL_B_SPLINE_SURFACE ( (
 ( 1.000000000000000000, 1.000000000000000000),
 ( 0.9754377213608244057, 0.9999580625633939235),
 ( 0.9754377213608244057, 0.9999580625633939235),
 ( 1.000000000000000000, 1.000000000000000000) ) ) 
 REPRESENTATION_ITEM ( '' )  SURFACE ( )  );
#2279 = EDGE_CURVE ( 'NONE', #31934, #58618, #41850, .T. ) ;
#2280 = LINE ( 'NONE', #2906, #49470 ) ;
#2281 = CARTESIAN_POINT ( 'NONE',  ( 4.962356264823608143, 0.000000000000000000, 0.000000000000000000 ) ) ;
#2282 = CARTESIAN_POINT ( 'NONE',  ( 0.3676999524040323597, 29.04098611012938136, 33.20499524279608750 ) ) ;
#2283 = B_SPLINE_CURVE_WITH_KNOTS ( 'NONE', 3,
 ( #4332, #23466, #42597, #18788 ),
 .UNSPECIFIED., .F., .F.,
 ( 4, 4 ),
 ( 0.000000000000000000, 0.005013413432710145910 ),
 .UNSPECIFIED. ) ;
#2285 = ORIENTED_EDGE ( 'NONE', *, *, #13474, .F. ) ;
#2284 = CARTESIAN_POINT ( 'NONE',  ( 4.967162193818130511, 0.000000000000000000, 0.000000000000000000 ) ) ;
#2286 = ORIENTED_EDGE ( 'NONE', *, *, #16129, .F. ) ;
#2287 = FACE_OUTER_BOUND ( 'NONE', #21187, .T. ) ;
#2288 = CARTESIAN_POINT ( 'NONE',  ( 0.1310142868023675411, 30.94009702668472883, -30.03916697317183804 ) ) ;
#2289 = CARTESIAN_POINT ( 'NONE',  ( 4.967162193818130511, -43.02067033766017801, -2.375726030843023029 ) ) ;
#2290 = VERTEX_POINT ( 'NONE', #13330 ) ;
#2291 = PRODUCT_DEFINITION ( 'UNKNOWN', '', #46903, #3527 ) ;
#2292 = ORIENTED_EDGE ( 'NONE', *, *, #4943, .T. ) ;
#2293 = CARTESIAN_POINT ( 'NONE',  ( 4.226256110419178924, -29.84627472560808314, 32.24945170062143518 ) ) ;
#2294 = CARTESIAN_POINT ( 'NONE',  ( 0.6031356755773454870, 6.279306815850185686, 47.69587413076375526 ) ) ;
#2295 = AXIS2_PLACEMENT_3D ( 'NONE', #33150, #28123, #47242 ) ;
#2296 = UNCERTAINTY_MEASURE_WITH_UNIT (LENGTH_MEASURE( 1.000000000000000082E-05 ), #22184, 'distance_accuracy_value', 'NONE');
#2297 = ORIENTED_EDGE ( 'NONE', *, *, #20089, .T. ) ;
#2298 = ORIENTED_EDGE ( 'NONE', *, *, #43067, .F. ) ;
#2299 = DIRECTION ( 'NONE',  ( 0.000000000000000000, 0.000000000000000000, 1.000000000000000000 ) ) ;
#2300 = CARTESIAN_POINT ( 'NONE',  ( 0.5850706913938533704, 44.18063951072221585, 18.49682194437980698 ) ) ;
#2301 = DIRECTION ( 'NONE',  ( 0.000000000000000000, 0.000000000000000000, 1.000000000000000000 ) ) ;
#2302 = EDGE_LOOP ( 'NONE', ( #58956, #27585, #54804, #32628 ) ) ;
#2303 = CARTESIAN_POINT ( 'NONE',  ( 4.691466044806102076, -29.64918311951151964, 33.30232861642381437 ) ) ;
#2304 = CIRCLE ( 'NONE', #10339, 10.00000000000000000 ) ;
#2305 = B_SPLINE_CURVE_WITH_KNOTS ( 'NONE', 3,
 ( #38814, #5246, #550, #6160, #24377, #25297 ),
 .UNSPECIFIED., .F., .F.,
 ( 4, 2, 4 ),
 ( 0.000000000000000000, 0.0002291459268755701264, 0.0004582918537511402528 ),
 .UNSPECIFIED. ) ;
#2306 = CARTESIAN_POINT ( 'NONE',  ( -6.079354080745853928, -16.13757513887051687, 10.50579001719862404 ) ) ;
#2307 = EDGE_CURVE ( 'NONE', #26672, #35006, #12672, .T. ) ;
#2308 = CARTESIAN_POINT ( 'NONE',  ( 0.7954190325252773475, -24.79809930825956599, -41.21355377862690261 ) ) ;
#2309 = EDGE_CURVE ( 'NONE', #32300, #52379, #27136, .T. ) ;
#2310 = VERTEX_POINT ( 'NONE', #13639 ) ;
#2311 = ORIENTED_EDGE ( 'NONE', *, *, #38579, .F. ) ;
#2312 = EDGE_CURVE ( 'NONE', #38360, #25968, #28337, .T. ) ;
#2313 = CARTESIAN_POINT ( 'NONE',  ( 0.8554163680231720024, -20.57434774096662977, -42.16517150618031451 ) ) ;
#2314 = CARTESIAN_POINT ( 'NONE',  ( -6.001507490154111224, -9.408444979392205809, -16.32705935667517139 ) ) ;
#2315 = ORIENTED_EDGE ( 'NONE', *, *, #59385, .F. ) ;
#2316 = CARTESIAN_POINT ( 'NONE',  ( 0.6021447746440204973, -48.67017425780974094, 6.538751930064458762 ) ) ;
#2317 = CARTESIAN_POINT ( 'NONE',  ( 2.282803330402968456, -12.65678521539727619, -45.23607736606130914 ) ) ;
#2318 = EDGE_CURVE ( 'NONE', #7116, #10837, #26074, .T. ) ;
#2319 = CARTESIAN_POINT ( 'NONE',  ( 0.5804410086790514622, 27.37779091616948079, 38.07855586029891271 ) ) ;
#2320 = CARTESIAN_POINT ( 'NONE',  ( 4.390527457369401532, -43.82188413991281095, -3.134933341664180695 ) ) ;
#2321 = B_SPLINE_CURVE_WITH_KNOTS ( 'NONE', 3,
 ( #57578, #22634, #46153, #3200 ),
 .UNSPECIFIED., .F., .F.,
 ( 4, 4 ),
 ( 0.000000000000000000, 0.002122961284640939757 ),
 .UNSPECIFIED. ) ;
#2322 = ORIENTED_EDGE ( 'NONE', *, *, #27876, .F. ) ;
#2323 = CARTESIAN_POINT ( 'NONE',  ( 0.9752570700956788574, -30.17732761204920422, -30.50353876750662963 ) ) ;
#2324 = CARTESIAN_POINT ( 'NONE',  ( 0.000000000000000000, 0.000000000000000000, -5.600000000000000533 ) ) ;
#2325 = CARTESIAN_POINT ( 'NONE',  ( 0.1149546198390366952, -31.50544959404307122, -30.89260770638230014 ) ) ;
#2326 = CARTESIAN_POINT ( 'NONE',  ( 0.9756354156337447847, -21.34128958497355555, -37.22481466014919960 ) ) ;
#2327 = VERTEX_POINT ( 'NONE', #23037 ) ;
#2328 = CARTESIAN_POINT ( 'NONE',  ( -31.75000000000000000, -15.14599999999999369, 1.854850041988580438E-15 ) ) ;
#2329 = CARTESIAN_POINT ( 'NONE',  ( 4.549368137175248350, 42.84816078363926550, 2.596185425822091553 ) ) ;
#2330 = CARTESIAN_POINT ( 'NONE',  ( 3.660176727303413813, 30.71420464230624603, -36.93665184075187113 ) ) ;
#2331 = CARTESIAN_POINT ( 'NONE',  ( 0.6001305935487315502, 11.94532529598378190, -46.60388846085711378 ) ) ;
#2332 = EDGE_CURVE ( 'NONE', #34292, #14733, #50816, .T. ) ;
#2333 = B_SPLINE_CURVE_WITH_KNOTS ( 'NONE', 3,
 ( #12190, #49758, #26884, #50074 ),
 .UNSPECIFIED., .F., .F.,
 ( 4, 4 ),
 ( 8.673617379884034509E-19, 0.004050076154992999881 ),
 .UNSPECIFIED. ) ;
#2334 = ORIENTED_EDGE ( 'NONE', *, *, #1448, .T. ) ;
#2335 = PLANE ( 'NONE',  #54882 ) ;
#2336 = DIRECTION ( 'NONE',  ( -1.000000000000000000, 0.000000000000000000, 0.000000000000000000 ) ) ;
#2337 = EDGE_CURVE ( 'NONE', #18623, #39044, #19433, .T. ) ;
#2338 = CARTESIAN_POINT ( 'NONE',  ( 0.1313383488274157129, 25.74310646082151877, -34.59671037481849254 ) ) ;
#2339 = AXIS2_PLACEMENT_3D ( 'NONE', #28791, #14100, #43223 ) ;
#2340 = LINE ( 'NONE', #46219, #9470 ) ;
#2341 = B_SPLINE_CURVE_WITH_KNOTS ( 'NONE', 3,
 ( #43722, #48694, #19282, #53676, #132, #34609, #24586, #10803, #5142, #39021, #767, #29892, #6059, #42786, #38399, #58076 ),
 .UNSPECIFIED., .F., .F.,
 ( 4, 3, 3, 3, 3, 4 ),
 ( 1.250973872328959164E-17, 0.0002724568934985599380, 0.0004086836638483908805, 0.0005449104342063664039, 0.0008173270854453730701, 0.001089761613562692045 ),
 .UNSPECIFIED. ) ;
#2342 = CARTESIAN_POINT ( 'NONE',  ( 1.830465331921977246, -36.02667829546079759, 25.34668630953094492 ) ) ;
#2343 = CARTESIAN_POINT ( 'NONE',  ( 0.9754402186311964540, 42.90805920318125999, -0.1875553420613088607 ) ) ;
#2344 = CARTESIAN_POINT ( 'NONE',  ( 0.9754642270333678811, -5.426415525315535504, -42.56393738774956859 ) ) ;
#2345 = CARTESIAN_POINT ( 'NONE',  ( 0.8751705887134423323, -41.19904111682490822, -24.81530984069193480 ) ) ;
#2346 = CARTESIAN_POINT ( 'NONE',  ( 3.270143674763207553, 13.28976595685398188, -3.277085381512974571 ) ) ;
#2347 = CARTESIAN_POINT ( 'NONE',  ( 0.6001305935487422083, -5.760103278697706664, -47.76436356026965768 ) ) ;
#2348 = CARTESIAN_POINT ( 'NONE',  ( 0.9762797500689124330, 14.58899758184639595, 39.28722355604407568 ) ) ;
#2349 = ORIENTED_EDGE ( 'NONE', *, *, #42345, .F. ) ;
#2350 = CARTESIAN_POINT ( 'NONE',  ( 0.6846871229502899947, -41.91507847151781618, -23.20185915381600950 ) ) ;
#2351 = CARTESIAN_POINT ( 'NONE',  ( 0.9722240741986378776, -16.95645453362492105, 39.41582013185140454 ) ) ;
#2352 = CARTESIAN_POINT ( 'NONE',  ( 4.694002226626920127, -40.92287315640982115, 20.08987864748135976 ) ) ;
#2353 = CARTESIAN_POINT ( 'NONE',  ( 0.5832655196449136881, -34.62741248031726116, -31.62558280714044301 ) ) ;
#2354 = AXIS2_PLACEMENT_3D ( 'NONE', #34177, #30686, #30071 ) ;
#2355 = CARTESIAN_POINT ( 'NONE',  ( 5.959547316686252039, 19.82530672674354832, 5.315863417546399461 ) ) ;
#2356 = B_SPLINE_CURVE_WITH_KNOTS ( 'NONE', 3,
 ( #3846, #57377, #47402, #56472, #33315, #52698, #42118, #52083, #47105, #61171, #18288, #9176, #37399, #4152, #18592, #43344 ),
 .UNSPECIFIED., .F., .F.,
 ( 4, 3, 3, 3, 3, 4 ),
 ( 1.040890552917501732E-17, 0.0002724568934985589080, 0.0004086836638483807974, 0.0005449104342063607661, 0.0008173270854453691669, 0.001089761613562693346 ),
 .UNSPECIFIED. ) ;
#2357 = CARTESIAN_POINT ( 'NONE',  ( 0.6254087463353934506, 17.77193046492952533, -44.70339519268195971 ) ) ;
#2358 = PRODUCT_CONTEXT ( 'NONE', #36374, 'mechanical' ) ;
#2359 = CARTESIAN_POINT ( 'NONE',  ( 2.299746137290200387, 23.81427056122728914, 42.86212611762045555 ) ) ;
#2360 = EDGE_CURVE ( 'NONE', #6447, #24288, #28038, .T. ) ;
#2361 = CARTESIAN_POINT ( 'NONE',  ( 0.9787464366903563251, -7.145144750301928305, 41.29504691107269565 ) ) ;
#2362 =( BOUNDED_SURFACE ( )  B_SPLINE_SURFACE ( 3, 1, ( 
 ( #16343, #50171 ),
 ( #31681, #31370 ),
 ( #25737, #11338 ),
 ( #45802, #6916 ) ),
 .UNSPECIFIED., .F., .F., .F. ) 
 B_SPLINE_SURFACE_WITH_KNOTS ( ( 4, 4 ),
 ( 2, 2 ),
 ( 0.000000000000000000, 1.000000000000000000 ),
 ( 0.000000000000000000, 1.000000000000000000 ),
 .UNSPECIFIED. ) 
 GEOMETRIC_REPRESENTATION_ITEM ( )  RATIONAL_B_SPLINE_SURFACE ( (
 ( 1.000000000000000000, 1.000000000000000000),
 ( 0.7269869731126821222, 0.9931720237060910339),
 ( 0.7269869731126821222, 0.9931720237060910339),
 ( 1.000000000000000000, 1.000000000000000000) ) ) 
 REPRESENTATION_ITEM ( '' )  SURFACE ( )  );
#2363 = CARTESIAN_POINT ( 'NONE',  ( 5.895596859100789899, 8.462961974658517406, 18.24572437114984780 ) ) ;
#2365 = VERTEX_POINT ( 'NONE', #42769 ) ;
#2364 = FACE_OUTER_BOUND ( 'NONE', #59481, .T. ) ;
#2366 = ORIENTED_EDGE ( 'NONE', *, *, #45718, .F. ) ;
#2367 = CARTESIAN_POINT ( 'NONE',  ( -6.063463321072276813, 0.6016212027212631819, -19.24729862624639054 ) ) ;
#2368 = CARTESIAN_POINT ( 'NONE',  ( 5.960721111146673579, 17.77250458025977764, 10.26825948882932060 ) ) ;
#2369 = FACE_OUTER_BOUND ( 'NONE', #43922, .T. ) ;
#2370 = VERTEX_POINT ( 'NONE', #61825 ) ;
#2371 = CARTESIAN_POINT ( 'NONE',  ( 0.5997462898726536595, -47.36625756029525292, -12.96106765957508244 ) ) ;
#2372 = CARTESIAN_POINT ( 'NONE',  ( 0.8551540677456715978, 44.61036085020950992, 17.49081417858803178 ) ) ;
#2373 = CYLINDRICAL_SURFACE ( 'NONE', #28066, 7.500000000000022204 ) ;
#2374 = ORIENTED_EDGE ( 'NONE', *, *, #58896, .F. ) ;
#2375 = EDGE_LOOP ( 'NONE', ( #14900, #3773, #35253, #48613 ) ) ;
#2376 = CARTESIAN_POINT ( 'NONE',  ( 5.200000000000002842, 0.000000000000000000, 0.000000000000000000 ) ) ;
#2377 = CARTESIAN_POINT ( 'NONE',  ( 0.1103878639767399417, -39.86034920885575872, -16.45816205842750080 ) ) ;
#2378 = CARTESIAN_POINT ( 'NONE',  ( 0.6016118706126977189, 37.16599942407935231, 32.09734477481374881 ) ) ;
#2379 = ORIENTED_EDGE ( 'NONE', *, *, #48886, .T. ) ;
#2380 = AXIS2_PLACEMENT_3D ( 'NONE', #47153, #47762, #5118 ) ;
#2381 = VERTEX_POINT ( 'NONE', #18962 ) ;
#2382 = CARTESIAN_POINT ( 'NONE',  ( -6.078457390727109555, 9.978433202401499003, -16.46892169702434572 ) ) ;
#2383 = DIRECTION ( 'NONE',  ( -1.000000000000000000, -1.836970198721027715E-16, 2.218671295934095703E-31 ) ) ;
#2384 = VERTEX_POINT ( 'NONE', #38082 ) ;
#2385 = SHAPE_REPRESENTATION ( 'straight bevel gear(wobble in)_iso_ISO - Straight bevel gear 2M 49GT 48PT 20PA 5FW ---49O1H50MD20.0S1', ( #14677 ), #61711 ) ;
#2386 = CARTESIAN_POINT ( 'NONE',  ( 0.2940135542859035889, 29.05872894121237238, -33.19383709384268855 ) ) ;
#2387 = CARTESIAN_POINT ( 'NONE',  ( 4.549368137175248350, 0.000000000000000000, 0.000000000000000000 ) ) ;
#2388 = ADVANCED_FACE ( 'NONE', ( #57131 ), #18118, .F. ) ;
#2389 = ORIENTED_EDGE ( 'NONE', *, *, #45161, .F. ) ;
#2390 = CARTESIAN_POINT ( 'NONE',  ( -5.995132425357893702, 18.68182899165011435, 2.468096378288185733 ) ) ;
#2391 = LINE ( 'NONE', #21516, #32558 ) ;
#2392 = B_SPLINE_CURVE_WITH_KNOTS ( 'NONE', 3,
 ( #32218, #26574, #61004, #55996 ),
 .UNSPECIFIED., .F., .F.,
 ( 4, 4 ),
 ( 0.000000000000000000, 0.004444103432399267029 ),
 .UNSPECIFIED. ) ;
#2393 = ORIENTED_EDGE ( 'NONE', *, *, #22307, .F. ) ;
#2394 = CARTESIAN_POINT ( 'NONE',  ( 4.291220156522060236, 41.58924158504501634, 22.12970812474624438 ) ) ;
#2395 = CARTESIAN_POINT ( 'NONE',  ( 5.860006189529246790, -26.81109398084734963, 40.09484204000590779 ) ) ;
#2396 = EDGE_CURVE ( 'NONE', #31646, #45810, #15179, .T. ) ;
#2397 = CARTESIAN_POINT ( 'NONE',  ( 0.9730545539215883499, 42.60426903087360984, -5.099196237954451760 ) ) ;
#2398 = CARTESIAN_POINT ( 'NONE',  ( 2.299746137290200387, -42.07681931141168974, 25.17583393496532551 ) ) ;
#2399 = CIRCLE ( 'NONE', #34448, 47.91270532121795611 ) ;
#2400 = ORIENTED_EDGE ( 'NONE', *, *, #28056, .F. ) ;
#2401 = B_SPLINE_CURVE_WITH_KNOTS ( 'NONE', 3,
 ( #28633, #29248, #28030, #61819, #738, #47446 ),
 .UNSPECIFIED., .F., .F.,
 ( 4, 2, 4 ),
 ( 1.029992063861229212E-18, 0.0002293801035737083962, 0.0004587602071474157625 ),
 .UNSPECIFIED. ) ;
#2402 = FACE_OUTER_BOUND ( 'NONE', #50002, .T. ) ;
#2403 = CARTESIAN_POINT ( 'NONE',  ( 0.5998501479064708430, 44.64337787626247689, -17.92509395669061689 ) ) ;
#2404 = EDGE_LOOP ( 'NONE', ( #1064, #11527, #13683, #18976 ) ) ;
#2405 = CARTESIAN_POINT ( 'NONE',  ( 0.3622758884714600280, -31.06363466427748321, 29.89648521331577058 ) ) ;
#2406 = VERTEX_POINT ( 'NONE', #24878 ) ;
#2407 = CARTESIAN_POINT ( 'NONE',  ( 0.9787284016396627928, 4.381134602593736993, 41.67903140096688475 ) ) ;
#2408 = VERTEX_POINT ( 'NONE', #1346 ) ;
#2409 = CARTESIAN_POINT ( 'NONE',  ( 5.960221823109900008, -0.005450390361865286269, 20.52559243573973546 ) ) ;
#2410 = CARTESIAN_POINT ( 'NONE',  ( 0.8760168074887076939, -17.58183840866429293, 44.77533136581851636 ) ) ;
#2411 = CARTESIAN_POINT ( 'NONE',  ( 0.1149546198390366675, -43.79613980524445793, 5.370726504180043825 ) ) ;
#2412 = ORIENTED_EDGE ( 'NONE', *, *, #45028, .F. ) ;
#2413 = CARTESIAN_POINT ( 'NONE',  ( 0.1139756605157202646, -27.82078886304557130, -34.24848794812498198 ) ) ;
#2414 = EDGE_CURVE ( 'NONE', #29913, #31002, #13896, .T. ) ;
#2415 = CARTESIAN_POINT ( 'NONE',  ( 0.5804410086790514622, 17.36461428077124935, 43.56592731407690877 ) ) ;
#2416 = VERTEX_POINT ( 'NONE', #20482 ) ;
#2417 = EDGE_LOOP ( 'NONE', ( #36052, #5937, #36617, #30490 ) ) ;
#2418 = CARTESIAN_POINT ( 'NONE',  ( 3.238018933889920792, -2.498552698661987925, 13.15920692061880537 ) ) ;
#2419 = CARTESIAN_POINT ( 'NONE',  ( 0.5807400328401637335, -46.40483864045154405, 11.87003418057225979 ) ) ;
#2420 = LINE ( 'NONE', #16864, #49805 ) ;
#2421 = CARTESIAN_POINT ( 'NONE',  ( 0.1084644655670282259, 25.93599432281498096, -34.45367667780541154 ) ) ;
#2422 = CARTESIAN_POINT ( 'NONE',  ( -0.6554360035617894376, 4.240386000424038571, -0.1586754815284913411 ) ) ;
#2423 = CARTESIAN_POINT ( 'NONE',  ( 0.1365634738349400801, 33.18118851476105391, 29.08386749335686261 ) ) ;
#2424 = ORIENTED_EDGE ( 'NONE', *, *, #32462, .F. ) ;
#2425 = CARTESIAN_POINT ( 'NONE',  ( 5.960721111146673579, -2.672857320903164524, -20.35079619394245043 ) ) ;
#2426 = CARTESIAN_POINT ( 'NONE',  ( 4.833616638992208614, -20.04871863793836084, 41.67905425467671421 ) ) ;
#2427 = EDGE_LOOP ( 'NONE', ( #4011, #46448, #1469, #5991 ) ) ;
#2428 = CARTESIAN_POINT ( 'NONE',  ( 0.7044674535453004927, -43.19749584530687514, -23.36191506502847304 ) ) ;
#2429 = CARTESIAN_POINT ( 'NONE',  ( 0.5817216825391099411, 37.08439865257854962, 28.70509238417621845 ) ) ;
#2430 = CARTESIAN_POINT ( 'NONE',  ( 0.5782707292762442330, 3.973746573563663009, 46.73270473529977664 ) ) ;
#2431 = CARTESIAN_POINT ( 'NONE',  ( 0.1135584504625008206, -42.78871615279810214, 10.77394181024413378 ) ) ;
#2432 = CARTESIAN_POINT ( 'NONE',  ( 2.624215991343608501, 43.79392271049069763, 19.66774719432994090 ) ) ;
#2433 = CARTESIAN_POINT ( 'NONE',  ( 4.834790513006553603, 33.61992680604592465, 33.20075093247886144 ) ) ;
#2434 = CARTESIAN_POINT ( 'NONE',  ( -48.95476116535499500, 9.797174393178825657E-16, -8.000000000000000000 ) ) ;
#2435 =( NAMED_UNIT ( * ) PLANE_ANGLE_UNIT ( ) SI_UNIT ( $, .RADIAN. ) );
#2436 = CARTESIAN_POINT ( 'NONE',  ( 0.6031356755773454870, 38.16621646312168536, 29.28593560184445010 ) ) ;
#2437 = ADVANCED_FACE ( 'NONE', ( #14568 ), #49139, .F. ) ;
#2438 = CARTESIAN_POINT ( 'NONE',  ( 0.9757787079277452369, -39.65734351318510420, 16.38386580718278296 ) ) ;
#2439 = CARTESIAN_POINT ( 'NONE',  ( 2.618530812446111078, -18.50060774051875967, -43.21405214082170687 ) ) ;
#2440 = AXIS2_PLACEMENT_3D ( 'NONE', #41505, #59968, #8898 ) ;
#2441 = FACE_OUTER_BOUND ( 'NONE', #14027, .T. ) ;
#2442 = FACE_OUTER_BOUND ( 'NONE', #54471, .T. ) ;
#2443 = LINE ( 'NONE', #46626, #14497 ) ;
#2444 = DIRECTION ( 'NONE',  ( -1.000000000000000000, -0.000000000000000000, -0.000000000000000000 ) ) ;
#2445 = CARTESIAN_POINT ( 'NONE',  ( 4.553261556744875094, 17.57396821678876364, 40.25785894628445760 ) ) ;
#2446 = CONICAL_SURFACE ( 'NONE', #51447, 42.92674063221959813, 1.485477209440487556 ) ;
#2447 = CARTESIAN_POINT ( 'NONE',  ( 0.5987334363312687424, 40.82324421486000432, 27.29515778019931460 ) ) ;
#2448 = LINE ( 'NONE', #11569, #8667 ) ;
#2449 = ADVANCED_FACE ( 'NONE', ( #19265 ), #26897, .F. ) ;
#2450 = VERTEX_POINT ( 'NONE', #48674 ) ;
#2451 = EDGE_CURVE ( 'NONE', #41641, #27695, #17883, .T. ) ;
#2452 = CARTESIAN_POINT ( 'NONE',  ( 0.1073791018717578927, 11.62916352156150346, -41.52698815987157133 ) ) ;
#2453 = CARTESIAN_POINT ( 'NONE',  ( 0.5809828226811617480, 5.711058609465307967, 47.55412398569209387 ) ) ;
#2454 = CARTESIAN_POINT ( 'NONE',  ( 0.1158516988532803244, -38.47034482238524333, -21.60959805455839700 ) ) ;
#2455 = CARTESIAN_POINT ( 'NONE',  ( 0.8753041380234524160, 32.34805756193409110, -36.94240787824717387 ) ) ;
#2456 = CARTESIAN_POINT ( 'NONE',  ( 0.1084644655670282953, -41.55047717876512792, 11.54510651093188933 ) ) ;
#2457 = ORIENTED_EDGE ( 'NONE', *, *, #42273, .T. ) ;
#2458 = CARTESIAN_POINT ( 'NONE',  ( 4.967162193818130511, -42.96271701169388280, 3.259922920617591924 ) ) ;
#2459 = CARTESIAN_POINT ( 'NONE',  ( 0.6846871229502932144, -34.48177377577859914, 33.25969555998731408 ) ) ;
#2460 = CARTESIAN_POINT ( 'NONE',  ( 0.8557997880470599172, 13.27832040216703469, -46.03118133706011861 ) ) ;
#2461 =( BOUNDED_SURFACE ( )  B_SPLINE_SURFACE ( 3, 1, ( 
 ( #37914, #28466 ),
 ( #9057, #41990 ),
 ( #47593, #47283 ),
 ( #46993, #4634 ) ),
 .UNSPECIFIED., .F., .F., .F. ) 
 B_SPLINE_SURFACE_WITH_KNOTS ( ( 4, 4 ),
 ( 2, 2 ),
 ( 0.000000000000000000, 1.000000000000000000 ),
 ( 0.000000000000000000, 1.000000000000000000 ),
 .UNSPECIFIED. ) 
 GEOMETRIC_REPRESENTATION_ITEM ( )  RATIONAL_B_SPLINE_SURFACE ( (
 ( 1.000000000000000000, 1.000000000000000000),
 ( 0.7211978278499968642, 0.9934217856018975334),
 ( 0.7211978278499968642, 0.9934217856018975334),
 ( 1.000000000000000000, 1.000000000000000000) ) ) 
 REPRESENTATION_ITEM ( '' )  SURFACE ( )  );
#2462 = VERTEX_POINT ( 'NONE', #44018 ) ;
#2463 = CIRCLE ( 'NONE', #33486, 10.00000000000000711 ) ;
#2464 = DIRECTION ( 'NONE',  ( 0.07439287786467667363, -0.5100024374914997605, 0.8569499480574931383 ) ) ;
#2465 = EDGE_CURVE ( 'NONE', #56737, #40264, #39611, .T. ) ;
#2466 = EDGE_LOOP ( 'NONE', ( #42337, #3518, #28965, #17680 ) ) ;
#2467 = DIRECTION ( 'NONE',  ( 0.9848077530122080203, 0.1736481776669315524, -2.220446049250313574E-16 ) ) ;
#2468 = CARTESIAN_POINT ( 'NONE',  ( 0.6017666602106490625, -29.00829887116099570, 38.37783452831155984 ) ) ;
#2469 = VERTEX_POINT ( 'NONE', #1052 ) ;
#2470 = CARTESIAN_POINT ( 'NONE',  ( 0.8753041380234524160, -26.21158409634513475, -41.52217705074249210 ) ) ;
#2472 = ORIENTED_EDGE ( 'NONE', *, *, #49512, .F. ) ;
#2471 = EDGE_CURVE ( 'NONE', #25842, #9574, #669, .T. ) ;
#2473 = CARTESIAN_POINT ( 'NONE',  ( 1.231276596079881935, 35.62927148397020005, 22.08691432816306133 ) ) ;
#2474 = CARTESIAN_POINT ( 'NONE',  ( 0.1092355843206037486, -26.01340835034388732, -34.39511076960595659 ) ) ;
#2475 = ORIENTED_EDGE ( 'NONE', *, *, #49175, .F. ) ;
#2476 = CARTESIAN_POINT ( 'NONE',  ( 4.291220156522059348, 20.72764654175944443, 42.30548033228772908 ) ) ;
#2477 = EDGE_CURVE ( 'NONE', #4518, #45517, #28308, .T. ) ;
#2478 = VERTEX_POINT ( 'NONE', #57430 ) ;
#2479 = FACE_OUTER_BOUND ( 'NONE', #13500, .T. ) ;
#2480 = AXIS2_PLACEMENT_3D ( 'NONE', #61725, #13854, #43598 ) ;
#2481 = ORIENTED_EDGE ( 'NONE', *, *, #42602, .F. ) ;
#2482 = EDGE_LOOP ( 'NONE', ( #60136, #24303, #6387, #24058 ) ) ;
#2483 = FACE_OUTER_BOUND ( 'NONE', #47134, .T. ) ;
#2484 = CARTESIAN_POINT ( 'NONE',  ( 0.5809828226811617480, 44.03860873105695362, 18.83114015454715684 ) ) ;
#2485 = FACE_OUTER_BOUND ( 'NONE', #29596, .T. ) ;
#2486 = CONICAL_SURFACE ( 'NONE', #19503, 42.08604991992415023, 1.569615340895231137 ) ;
#2487 = CARTESIAN_POINT ( 'NONE',  ( 0.1102144999581332746, -16.61938362665576108, 39.79340763430480621 ) ) ;
#2488 = DIRECTION ( 'NONE',  ( -1.000000000000000000, -3.673819061467147552E-16, 1.925929944387235306E-32 ) ) ;
#2489 = ORIENTED_EDGE ( 'NONE', *, *, #15281, .F. ) ;
#2490 = CARTESIAN_POINT ( 'NONE',  ( 0.9756354156337453398, 10.97961179198200021, 41.47994205070116891 ) ) ;
#2491 = CARTESIAN_POINT ( 'NONE',  ( 0.8751705887134553219, 7.160166390003662507, 47.55935879196473337 ) ) ;
#2492 = ADVANCED_FACE ( 'NONE', ( #38687 ), #905, .F. ) ;
#2493 = DIRECTION ( 'NONE',  ( 4.437342591868191405E-31, -1.000000000000000000, -4.551914400963141816E-15 ) ) ;
#2494 = CIRCLE ( 'NONE', #56508, 2.099999999999999645 ) ;
#2495 = ORIENTED_EDGE ( 'NONE', *, *, #56606, .F. ) ;
#2496 = EDGE_LOOP ( 'NONE', ( #25039, #40521, #14637, #42290 ) ) ;
#2497 = CARTESIAN_POINT ( 'NONE',  ( 0.9757402383260938006, 34.09320464257847050, -26.05362288587330966 ) ) ;
#2498 = CARTESIAN_POINT ( 'NONE',  ( -5.995132425357893702, 2.451215106828613433, -18.68405145320021532 ) ) ;
#2499 = CARTESIAN_POINT ( 'NONE',  ( 4.999999999999986677, 56.56854249492450037, -56.56854249492312192 ) ) ;
#2500 = VERTEX_POINT ( 'NONE', #35213 ) ;
#2501 = CARTESIAN_POINT ( 'NONE',  ( 0.3622758884714730732, -29.89648521331652731, 31.06363466427676201 ) ) ;
#2502 = CARTESIAN_POINT ( 'NONE',  ( -6.016761891674564211, -16.31696541414278911, 9.424569481870193499 ) ) ;
#2503 = CARTESIAN_POINT ( 'NONE',  ( 0.6031357023905875581, -29.25135304925253976, -38.19275261685265122 ) ) ;
#2504 = ORIENTED_EDGE ( 'NONE', *, *, #25635, .F. ) ;
#2505 = CARTESIAN_POINT ( 'NONE',  ( 3.238018933889920792, -13.34321331060666083, 1.168824587054079878 ) ) ;
#2506 = ORIENTED_EDGE ( 'NONE', *, *, #36413, .F. ) ;
#2507 = CARTESIAN_POINT ( 'NONE',  ( 0.5850706913938534814, -33.73916126769474744, 33.99603398296579115 ) ) ;
#2508 = CARTESIAN_POINT ( 'NONE',  ( 5.895881250540457863, 5.963300346357645942, 19.20850672455908992 ) ) ;
#2509 = CARTESIAN_POINT ( 'NONE',  ( 5.860006189529246790, -36.25227510158441646, -31.81514841426795570 ) ) ;
#2510 = FILL_AREA_STYLE ('',( #39850 ) ) ;
#2511 = ORIENTED_EDGE ( 'NONE', *, *, #55388, .F. ) ;
#2512 = CARTESIAN_POINT ( 'NONE',  ( 0.9754642270333673260, 21.60621846558691672, -37.07163437210427048 ) ) ;
#2513 = CARTESIAN_POINT ( 'NONE',  ( 0.8753041380234471980, -0.6841799139044226763, -49.09857661601188994 ) ) ;
#2514 = CARTESIAN_POINT ( 'NONE',  ( 5.000000000000010658, -72.00000000000002842, 8.817456953860946444E-15 ) ) ;
#2515 = CARTESIAN_POINT ( 'NONE',  ( 0.5980271706414711508, 4.018631420204758165, 48.94792992916254093 ) ) ;
#2516 = B_SPLINE_CURVE_WITH_KNOTS ( 'NONE', 3,
 ( #58510, #30959, #44473, #1502 ),
 .UNSPECIFIED., .F., .F.,
 ( 4, 4 ),
 ( 0.000000000000000000, 0.004446090762761369455 ),
 .UNSPECIFIED. ) ;
#2517 = CARTESIAN_POINT ( 'NONE',  ( 0.09136607875274982415, 5.281323502666703820E-15, -43.12527911185304674 ) ) ;
#2518 = CARTESIAN_POINT ( 'NONE',  ( 0.6845945791218023269, 43.51705215793850812, 17.51207275559363907 ) ) ;
#2519 = EDGE_CURVE ( 'NONE', #14527, #30513, #42153, .T. ) ;
#2520 = DIRECTION ( 'NONE',  ( 0.000000000000000000, 0.000000000000000000, -1.000000000000000000 ) ) ;
#2521 = CARTESIAN_POINT ( 'NONE',  ( 0.8753041380234524160, 5.600023814135298927, 48.78296896616787848 ) ) ;
#2522 = CARTESIAN_POINT ( 'NONE',  ( 4.962356264823608143, 34.44911810793244200, 24.17630781256866612 ) ) ;
#2523 = B_SPLINE_CURVE_WITH_KNOTS ( 'NONE', 3,
 ( #18871, #42373, #23545, #47072 ),
 .UNSPECIFIED., .F., .F.,
 ( 4, 4 ),
 ( 2.168404344971008868E-19, 0.004041751736740997747 ),
 .UNSPECIFIED. ) ;
#2524 = EDGE_CURVE ( 'NONE', #40320, #18600, #32098, .T. ) ;
#2525 = B_SPLINE_CURVE_WITH_KNOTS ( 'NONE', 3,
 ( #45898, #28000, #55877, #41193, #42428, #23005 ),
 .UNSPECIFIED., .F., .F.,
 ( 4, 2, 4 ),
 ( 0.000000000000000000, 0.0002447195606305742582, 0.0004894391212611485164 ),
 .UNSPECIFIED. ) ;
#2526 = AXIS2_PLACEMENT_3D ( 'NONE', #21208, #54697, #59096 ) ;
#2527 = EDGE_CURVE ( 'NONE', #51919, #39239, #6636, .T. ) ;
#2528 = FACE_OUTER_BOUND ( 'NONE', #34304, .T. ) ;
#2529 = DIRECTION ( 'NONE',  ( 1.000000000000000000, 0.000000000000000000, 0.000000000000000000 ) ) ;
#2530 = ORIENTED_EDGE ( 'NONE', *, *, #23555, .T. ) ;
#2531 = CARTESIAN_POINT ( 'NONE',  ( 3.390910168358336918, -3.377210997459680453, -43.84850718567593475 ) ) ;
#2532 = CIRCLE ( 'NONE', #47582, 43.08621763946400307 ) ;
#2533 = CARTESIAN_POINT ( 'NONE',  ( 0.8557997880470599172, 44.60232077416710439, -17.48760788519168941 ) ) ;
#2534 = EDGE_LOOP ( 'NONE', ( #50849, #28925, #12291, #26740 ) ) ;
#2535 = CARTESIAN_POINT ( 'NONE',  ( 5.965394784446458765, 5.326334832595374991, 19.82223131420056106 ) ) ;
#2536 = VECTOR ( 'NONE', #27315, 1000.000000000000114 ) ;
#2537 = CARTESIAN_POINT ( 'NONE',  ( 0.3622758884714730732, -39.50828911767010965, 17.25816669464924047 ) ) ;
#2538 = CARTESIAN_POINT ( 'NONE',  ( 0.5797568665920715958, -14.49376217790061183, -44.59995702388432193 ) ) ;
#2539 = ORIENTED_EDGE ( 'NONE', *, *, #5894, .F. ) ;
#2540 = CARTESIAN_POINT ( 'NONE',  ( 0.7057020205115013267, -33.27137945725694124, -34.46103118762825801 ) ) ;
#2541 = DIRECTION ( 'NONE',  ( 1.000000000000000000, 0.000000000000000000, 0.000000000000000000 ) ) ;
#2542 = ADVANCED_FACE ( 'NONE', ( #49283 ), #52494, .F. ) ;
#2544 = ORIENTED_EDGE ( 'NONE', *, *, #32151, .T. ) ;
#2543 =( BOUNDED_SURFACE ( )  B_SPLINE_SURFACE ( 3, 1, ( 
 ( #21050, #54221 ),
 ( #11342, #40489 ),
 ( #13509, #56394 ),
 ( #45806, #42036 ) ),
 .UNSPECIFIED., .F., .F., .F. ) 
 B_SPLINE_SURFACE_WITH_KNOTS ( ( 4, 4 ),
 ( 2, 2 ),
 ( 0.000000000000000000, 1.000000000000000000 ),
 ( 0.000000000000000000, 1.000000000000000000 ),
 .UNSPECIFIED. ) 
 GEOMETRIC_REPRESENTATION_ITEM ( )  RATIONAL_B_SPLINE_SURFACE ( (
 ( 1.000000000000000000, 1.000000000000000000),
 ( 0.7223157951917480446, 0.9931996967497186413),
 ( 0.7223157951917480446, 0.9931996967497186413),
 ( 1.000000000000000000, 1.000000000000000000) ) ) 
 REPRESENTATION_ITEM ( '' )  SURFACE ( )  );
#2545 = CARTESIAN_POINT ( 'NONE',  ( 0.5807400328401637335, -29.58941477092991335, -37.66660715020896077 ) ) ;
#2547 = VERTEX_POINT ( 'NONE', #20794 ) ;
#2546 = EDGE_CURVE ( 'NONE', #35321, #42399, #32154, .T. ) ;
#2548 = ORIENTED_EDGE ( 'NONE', *, *, #11307, .T. ) ;
#2549 = CARTESIAN_POINT ( 'NONE',  ( 0.1140933569871963871, 44.00767033400067874, 3.205448776352883833 ) ) ;
#2550 = ORIENTED_EDGE ( 'NONE', *, *, #51977, .F. ) ;
#2551 = DIRECTION ( 'NONE',  ( 0.000000000000000000, 0.000000000000000000, -1.000000000000000000 ) ) ;
#2552 = VERTEX_POINT ( 'NONE', #35523 ) ;
#2553 = CARTESIAN_POINT ( 'NONE',  ( 0.6000166863083106206, -43.04473087057989744, -23.64264422580097502 ) ) ;
#2554 = EDGE_CURVE ( 'NONE', #61929, #715, #58988, .T. ) ;
#2555 = CARTESIAN_POINT ( 'NONE',  ( 0.5987334308729320709, 40.82324396785260490, -27.29515815141791535 ) ) ;
#2556 = ORIENTED_EDGE ( 'NONE', *, *, #40784, .F. ) ;
#2557 = DIRECTION ( 'NONE',  ( 0.000000000000000000, -1.000000000000000000, 0.000000000000000000 ) ) ;
#2558 = CARTESIAN_POINT ( 'NONE',  ( 50.50000000000000000, 12.21587082446438011, -2.649999999999992806 ) ) ;
#2559 = CARTESIAN_POINT ( 'NONE',  ( 0.5824935313925951874, -44.41938431943384558, -15.03849971693567511 ) ) ;
#2560 = CARTESIAN_POINT ( 'NONE',  ( 0.5830082357119561465, -30.48544060673254918, 35.63523461339518406 ) ) ;
#2561 = ORIENTED_EDGE ( 'NONE', *, *, #37649, .F. ) ;
#2562 = CARTESIAN_POINT ( 'NONE',  ( 0.5834872094924180574, 44.16273175734639977, 18.53852119651579855 ) ) ;
#2563 = EDGE_CURVE ( 'NONE', #14707, #41543, #59604, .T. ) ;
#2564 = VERTEX_POINT ( 'NONE', #2591 ) ;
#2565 = CARTESIAN_POINT ( 'NONE',  ( 0.1087620492084204749, 41.55994353650425666, 11.51076657762349598 ) ) ;
#2566 = CARTESIAN_POINT ( 'NONE',  ( 0.9747592971366227932, 26.37717450293426680, 33.84353661172414007 ) ) ;
#2567 = DIRECTION ( 'NONE',  ( 0.09835009131224567436, -0.7091251765524118067, 0.6981896185982600089 ) ) ;
#2568 = ORIENTED_EDGE ( 'NONE', *, *, #11533, .F. ) ;
#2569 = CARTESIAN_POINT ( 'NONE',  ( 0.5839879327111929808, -46.28746210677702067, -12.30864801674759512 ) ) ;
#2570 = CARTESIAN_POINT ( 'NONE',  ( -6.078726893082806448, 9.979253153318998315, -16.46841060244408794 ) ) ;
#2571 = CARTESIAN_POINT ( 'NONE',  ( 7.000000000000006217, 8.392413579938656024E-13, -80.00000000000001421 ) ) ;
#2572 = CARTESIAN_POINT ( 'NONE',  ( 0.8557997880470606944, 29.88293891557523807, -37.44587306708065455 ) ) ;
#2574 = VERTEX_POINT ( 'NONE', #3205 ) ;
#2573 = AXIS2_PLACEMENT_3D ( 'NONE', #29978, #31216, #50314 ) ;
#2575 = B_SPLINE_CURVE_WITH_KNOTS ( 'NONE', 3,
 ( #11598, #35727, #21604, #54790, #11925, #20748, #48320, #5380, #24506, #29822, #58616, #10735, #53606, #38950, #25748, #48938, #5986, #25126, #30432 ),
 .UNSPECIFIED., .F., .F.,
 ( 4, 3, 3, 3, 3, 3, 4 ),
 ( 1.161276725443423652E-16, 0.0002618519381806236400, 0.0003927759815485981978, 0.0005237000248299445142, 0.0006546240681324981504, 0.0007855481115631340102, 0.0009699050456655115924 ),
 .UNSPECIFIED. ) ;
#2576 = ORIENTED_EDGE ( 'NONE', *, *, #23148, .T. ) ;
#2577 = CARTESIAN_POINT ( 'NONE',  ( 0.9762797500689124330, -39.42083772998312696, -14.22400568939859866 ) ) ;
#2578 = CARTESIAN_POINT ( 'NONE',  ( 3.559346040607745287, 42.33240525468902149, 11.89107845801906649 ) ) ;
#2579 = CARTESIAN_POINT ( 'NONE',  ( 3.238741278300274029, 12.88350628398740483, -41.01623499586001742 ) ) ;
#2580 = CIRCLE ( 'NONE', #7582, 15.14599999999999369 ) ;
#2581 = CARTESIAN_POINT ( 'NONE',  ( 0.6027935024548038978, 6.452291758824724610, -47.67281620606625836 ) ) ;
#2582 = CARTESIAN_POINT ( 'NONE',  ( 0.7413678028165008316, -13.43842184872795897, -41.99874890976961694 ) ) ;
#2583 = CARTESIAN_POINT ( 'NONE',  ( 0.8554163680231708922, -30.98316862405949124, 35.23136010892730496 ) ) ;
#2584 = CARTESIAN_POINT ( 'NONE',  ( 0.2230388203127609270, -6.380812898001274824, -42.64472907182728534 ) ) ;
#2585 = AXIS2_PLACEMENT_3D ( 'NONE', #44389, #54037, #49354 ) ;
#2586 = CARTESIAN_POINT ( 'NONE',  ( -69.95594261585600293, 1.530808498934191521E-15, 12.50000000000000000 ) ) ;
#2587 = CARTESIAN_POINT ( 'NONE',  ( 3.376099380956838925, -0.9076095657324720900, 13.37477583020582905 ) ) ;
#2588 = CARTESIAN_POINT ( 'NONE',  ( 0.5809828226811617480, -41.74875432577665890, 23.47450554821694979 ) ) ;
#2589 = EDGE_CURVE ( 'NONE', #19228, #15999, #14131, .T. ) ;
#2590 = CARTESIAN_POINT ( 'NONE',  ( 0.6254087463353908971, 5.596276562478328387, -47.77987801197956230 ) ) ;
#2591 = CARTESIAN_POINT ( 'NONE',  ( 1.231276596079887264, 3.353048872156665805, -41.78556968953512296 ) ) ;
#2592 = CARTESIAN_POINT ( 'NONE',  ( 0.5824936645240075261, -13.54584401086361112, -44.89708552983879741 ) ) ;
#2593 = DIRECTION ( 'NONE',  ( 0.000000000000000000, 0.000000000000000000, 1.000000000000000000 ) ) ;
#2595 = EDGE_CURVE ( 'NONE', #5803, #59492, #29106, .T. ) ;
#2594 = CARTESIAN_POINT ( 'NONE',  ( -6.072942160501519027, -17.34299816270043593, -8.368068894170846761 ) ) ;
#2596 = CARTESIAN_POINT ( 'NONE',  ( 0.1064266379913940824, 43.12102052820963394, -0.5615183164813251082 ) ) ;
#2597 = EDGE_CURVE ( 'NONE', #18903, #13003, #27644, .T. ) ;
#2598 = CARTESIAN_POINT ( 'NONE',  ( 3.238018933889920792, 13.30865154331497280, -1.512377752505324358 ) ) ;
#2599 = DIRECTION ( 'NONE',  ( -0.07439287786467652097, 0.9161872986448755807, -0.3937848822959269524 ) ) ;
#2600 = ADVANCED_FACE ( 'NONE', ( #32052 ), #9690, .F. ) ;
#2601 = ORIENTED_EDGE ( 'NONE', *, *, #17120, .T. ) ;
#2602 = ORIENTED_EDGE ( 'NONE', *, *, #43973, .F. ) ;
#2603 = LINE ( 'NONE', #59305, #48905 ) ;
#2604 = CARTESIAN_POINT ( 'NONE',  ( 0.3676999524040366896, 3.413584541509296688, -43.98065510995495941 ) ) ;
#2605 = EDGE_CURVE ( 'NONE', #49867, #47520, #25311, .T. ) ;
#2606 = CYLINDRICAL_SURFACE ( 'NONE', #2774, 1.000000000000000888 ) ;
#2607 = ORIENTED_EDGE ( 'NONE', *, *, #38979, .F. ) ;
#2608 = ORIENTED_EDGE ( 'NONE', *, *, #42852, .T. ) ;
#2609 = CARTESIAN_POINT ( 'NONE',  ( 0.5997462898726536595, 37.05192695178169515, -32.22896739432000146 ) ) ;
#2610 = CARTESIAN_POINT ( 'NONE',  ( 0.1101816497532063233, -37.27878591512690321, 21.67974746580484435 ) ) ;
#2611 = ORIENTED_EDGE ( 'NONE', *, *, #3313, .T. ) ;
#2612 = ORIENTED_EDGE ( 'NONE', *, *, #6390, .F. ) ;
#2613 = EDGE_CURVE ( 'NONE', #25770, #53648, #44757, .T. ) ;
#2614 = CARTESIAN_POINT ( 'NONE',  ( 0.5839880159502327528, 47.89596769806549048, 0.04537901683497938543 ) ) ;
#2615 = CARTESIAN_POINT ( 'NONE',  ( -31.75000000000000000, 15.43999999999999240, 0.000000000000000000 ) ) ;
#2616 = CONICAL_SURFACE ( 'NONE', #14638, 42.08604991992415023, 1.569615340895231137 ) ;
#2617 = CARTESIAN_POINT ( 'NONE',  ( -6.015611763856276717, 2.453375430804066504, 18.68284711750059301 ) ) ;
#2618 = AXIS2_PLACEMENT_3D ( 'NONE', #47580, #3399, #13150 ) ;
#2619 = VERTEX_POINT ( 'NONE', #18259 ) ;
#2620 = CARTESIAN_POINT ( 'NONE',  ( 0.8760168074886965917, 7.161346975773705381, -47.56749362999706676 ) ) ;
#2621 = CARTESIAN_POINT ( 'NONE',  ( 4.553261556744875094, 0.000000000000000000, 0.000000000000000000 ) ) ;
#2622 = CARTESIAN_POINT ( 'NONE',  ( 0.1155031312995260795, 15.39696621848024272, -41.35063559123108945 ) ) ;
#2623 = EDGE_LOOP ( 'NONE', ( #54315, #25988, #22454, #19690 ) ) ;
#2624 = AXIS2_PLACEMENT_3D ( 'NONE', #35525, #55211, #22033 ) ;
#2625 = EDGE_LOOP ( 'NONE', ( #36396, #26501, #31258, #19273 ) ) ;
#2626 = DIRECTION ( 'NONE',  ( 0.09835009131224567436, -0.2500873580884643288, -0.9632152266566414989 ) ) ;
#2627 = CARTESIAN_POINT ( 'NONE',  ( 0.6000166863083090663, -1.051715750664325322, 49.09905676984292455 ) ) ;
#2628 = EDGE_LOOP ( 'NONE', ( #18829, #12248, #48276, #60391 ) ) ;
#2629 = CARTESIAN_POINT ( 'NONE',  ( 0.5997462898726536595, -48.76843890605309184, 5.761162800240605897 ) ) ;
#2630 = DIRECTION ( 'NONE',  ( 0.000000000000000000, 0.000000000000000000, 1.000000000000000000 ) ) ;
#2631 = CARTESIAN_POINT ( 'NONE',  ( 0.6000166863083090663, -39.04292238714170793, 29.79049669240313847 ) ) ;
#2632 = CARTESIAN_POINT ( 'NONE',  ( 0.6067099128993224122, -17.67241243535514883, 44.51753430581932491 ) ) ;
#2633 = EDGE_CURVE ( 'NONE', #49170, #14203, #6085, .T. ) ;
#2634 = VERTEX_POINT ( 'NONE', #22644 ) ;
#2635 = LINE ( 'NONE', #17074, #47894 ) ;
#2636 = CARTESIAN_POINT ( 'NONE',  ( 0.6009452777970409887, 18.81240106508465004, 44.27681866781112063 ) ) ;
#2637 =( BOUNDED_SURFACE ( )  B_SPLINE_SURFACE ( 3, 1, ( 
 ( #2825, #31351 ),
 ( #49837, #26335 ),
 ( #16964, #54505 ),
 ( #7517, #11633 ) ),
 .UNSPECIFIED., .F., .F., .F. ) 
 B_SPLINE_SURFACE_WITH_KNOTS ( ( 4, 4 ),
 ( 2, 2 ),
 ( 0.000000000000000000, 1.000000000000000000 ),
 ( 0.000000000000000000, 1.000000000000000000 ),
 .UNSPECIFIED. ) 
 GEOMETRIC_REPRESENTATION_ITEM ( )  RATIONAL_B_SPLINE_SURFACE ( (
 ( 1.000000000000000000, 1.000000000000000000),
 ( 0.9732289882329797637, 0.9999525324661233672),
 ( 0.9732289882329797637, 0.9999525324661233672),
 ( 1.000000000000000000, 1.000000000000000000) ) ) 
 REPRESENTATION_ITEM ( '' )  SURFACE ( )  );
#2638 = CARTESIAN_POINT ( 'NONE',  ( 7.147292112312088719, -11.82536368408648286, 3.000000000000017764 ) ) ;
#2639 = EDGE_CURVE ( 'NONE', #50100, #8159, #22332, .T. ) ;
#2640 = B_SPLINE_CURVE_WITH_KNOTS ( 'NONE', 3,
 ( #17185, #41314, #60370, #55675 ),
 .UNSPECIFIED., .F., .F.,
 ( 4, 4 ),
 ( 2.170598744017606518E-17, 0.004559932413162186803 ),
 .UNSPECIFIED. ) ;
#2641 = EDGE_LOOP ( 'NONE', ( #28229, #27216, #27458, #6927 ) ) ;
#2642 = DIRECTION ( 'NONE',  ( -1.000000000000000000, -0.000000000000000000, -0.000000000000000000 ) ) ;
#2643 = CARTESIAN_POINT ( 'NONE',  ( 0.1313383488274121880, -4.995828979989775043, 42.83318330237614902 ) ) ;
#2644 = FACE_OUTER_BOUND ( 'NONE', #50040, .T. ) ;
#2645 = ORIENTED_EDGE ( 'NONE', *, *, #58120, .F. ) ;
#2646 = CARTESIAN_POINT ( 'NONE',  ( 1.000433927950264534, -13.04434877168812790, -39.82792541390282537 ) ) ;
#2647 = DIRECTION ( 'NONE',  ( 1.000000000000000000, 0.000000000000000000, 0.000000000000000000 ) ) ;
#2648 = CARTESIAN_POINT ( 'NONE',  ( -6.078075953587585900, 0.6118799989804611927, -19.24631853404654791 ) ) ;
#2649 = CARTESIAN_POINT ( 'NONE',  ( -2.601141883200662974, -4.674544242619348644, -14.17547401652526418 ) ) ;
#2650 =( BOUNDED_SURFACE ( )  B_SPLINE_SURFACE ( 3, 1, ( 
 ( #55883, #50566 ),
 ( #51180, #3869 ),
 ( #32717, #22378 ),
 ( #27080, #22691 ) ),
 .UNSPECIFIED., .F., .F., .F. ) 
 B_SPLINE_SURFACE_WITH_KNOTS ( ( 4, 4 ),
 ( 2, 2 ),
 ( 0.000000000000000000, 1.000000000000000000 ),
 ( 0.000000000000000000, 1.000000000000000000 ),
 .UNSPECIFIED. ) 
 GEOMETRIC_REPRESENTATION_ITEM ( )  RATIONAL_B_SPLINE_SURFACE ( (
 ( 1.000000000000000000, 1.000000000000000000),
 ( 0.9952954269826590483, 0.8620686068821339365),
 ( 0.9952954269826590483, 0.8620686068821339365),
 ( 1.000000000000000000, 1.000000000000000000) ) ) 
 REPRESENTATION_ITEM ( '' )  SURFACE ( )  );
#2651 = CARTESIAN_POINT ( 'NONE',  ( 0.5832366564991520175, 46.19265750221185840, -12.65934068133935853 ) ) ;
#2652 = CARTESIAN_POINT ( 'NONE',  ( 0.7056555295713293763, -47.59410019435325268, -5.417452459790225383 ) ) ;
#2653 = CARTESIAN_POINT ( 'NONE',  ( 1.296416391601053153, -32.42183002721205298, -29.85183933634123576 ) ) ;
#2654 = CIRCLE ( 'NONE', #53704, 0.05882000000000109363 ) ;
#2655 = CARTESIAN_POINT ( 'NONE',  ( 0.6008123274975391004, 41.39240128969535704, -26.42392224162195902 ) ) ;
#2656 = CARTESIAN_POINT ( 'NONE',  ( 5.959547316686252039, 10.26589671991338548, 17.77392908783937386 ) ) ;
#2657 = ORIENTED_EDGE ( 'NONE', *, *, #41689, .F. ) ;
#2658 = STYLED_ITEM ( 'NONE', ( #18504 ), #30252 ) ;
#2659 = AXIS2_PLACEMENT_3D ( 'NONE', #51775, #8874, #36245 ) ;
#2660 = CARTESIAN_POINT ( 'NONE',  ( -16.58656855106744032, -12.39978673513562946, -1.582714324450230192 ) ) ;
#2661 = CARTESIAN_POINT ( 'NONE',  ( 7.999999999999981348, 85.00000000000001421, 1.040949779275250495E-14 ) ) ;
#2662 = CARTESIAN_POINT ( 'NONE',  ( 1.157644175074339588, -35.01838093932130391, 23.03725834095192937 ) ) ;
#2663 = CARTESIAN_POINT ( 'NONE',  ( 0.1149546198390366814, 44.05025956747236648, -2.553663458940844677 ) ) ;
#2664 = CARTESIAN_POINT ( 'NONE',  ( 0.6039202388192952409, -47.45712035475593638, -12.62479467093234575 ) ) ;
#2665 = FACE_OUTER_BOUND ( 'NONE', #47818, .T. ) ;
#2666 = APPLICATION_PROTOCOL_DEFINITION ( 'draft international standard', 'automotive_design', 1998, #36374 ) ;
#2668 = ADVANCED_FACE ( 'NONE', ( #8218 ), #60908, .F. ) ;
#2667 = CARTESIAN_POINT ( 'NONE',  ( 0.6009452777970414328, -44.27681866781119169, 18.81240106508449372 ) ) ;
#2669 = CARTESIAN_POINT ( 'NONE',  ( 4.553261556744875094, 35.33793455049291765, -26.09156851415253087 ) ) ;
#2670 = EDGE_CURVE ( 'NONE', #45306, #44423, #29090, .T. ) ;
#2671 = CIRCLE ( 'NONE', #37728, 2.500000000000000444 ) ;
#2672 = CARTESIAN_POINT ( 'NONE',  ( 4.975801465491694664, 42.71626295676232843, 21.70134120755216145 ) ) ;
#2673 = EDGE_CURVE ( 'NONE', #25113, #55855, #10086, .T. ) ;
#2675 = ORIENTED_EDGE ( 'NONE', *, *, #8604, .T. ) ;
#2674 = LINE ( 'NONE', #26806, #53327 ) ;
#2676 = ORIENTED_EDGE ( 'NONE', *, *, #53167, .T. ) ;
#2677 = CARTESIAN_POINT ( 'NONE',  ( 5.974727161628369032, 17.78288073588502982, -10.24903993264990376 ) ) ;
#2678 = CARTESIAN_POINT ( 'NONE',  ( 0.5837799406558227266, -7.710363279387344448, 46.25790578568249600 ) ) ;
#2679 = EDGE_CURVE ( 'NONE', #32472, #35664, #39232, .T. ) ;
#2680 = CARTESIAN_POINT ( 'NONE',  ( 1.227938101723748288, -0.8460948827228147451, 42.91134962331487657 ) ) ;
#2681 = ORIENTED_EDGE ( 'NONE', *, *, #38988, .T. ) ;
#2682 = CARTESIAN_POINT ( 'NONE',  ( 0.1073791018717578927, 37.58707531572206051, -21.14095454447521405 ) ) ;
#2683 = CARTESIAN_POINT ( 'NONE',  ( 0.5839879327111928697, -47.47435452316579330, 6.341736898931764621 ) ) ;
#2684 = DIRECTION ( 'NONE',  ( -1.000000000000000000, -0.000000000000000000, -0.000000000000000000 ) ) ;
#2685 = VECTOR ( 'NONE', #12874, 1000.000000000000114 ) ;
#2686 = ORIENTED_EDGE ( 'NONE', *, *, #19180, .F. ) ;
#2687 = ORIENTED_EDGE ( 'NONE', *, *, #14205, .T. ) ;
#2688 = CARTESIAN_POINT ( 'NONE',  ( 4.960386119450147291, 32.13287905145141821, -29.69704612477700678 ) ) ;
#2689 = CARTESIAN_POINT ( 'NONE',  ( 0.1104177457020373287, -39.84367193872667201, -16.49849172082149451 ) ) ;
#2690 = DIRECTION ( 'NONE',  ( 0.000000000000000000, 0.000000000000000000, 1.000000000000000000 ) ) ;
#2691 = VERTEX_POINT ( 'NONE', #5356 ) ;
#2692 = CARTESIAN_POINT ( 'NONE',  ( 0.6029442701453591180, 49.01209361462912995, 3.059396128177434449 ) ) ;
#2693 = CARTESIAN_POINT ( 'NONE',  ( 0.7246131072078549895, 0.8205838906003107835, -48.09507913767662757 ) ) ;
#2694 = ORIENTED_EDGE ( 'NONE', *, *, #40398, .T. ) ;
#2695 = CARTESIAN_POINT ( 'NONE',  ( 4.967162193818130511, -28.74031574029989855, -32.10009971360102554 ) ) ;
#2696 = CARTESIAN_POINT ( 'NONE',  ( 0.5809828226811553087, -44.03860873105708151, 18.83114015454682999 ) ) ;
#2697 = VECTOR ( 'NONE', #4936, 1000.000000000000000 ) ;
#2698 = ORIENTED_EDGE ( 'NONE', *, *, #34693, .T. ) ;
#2699 = CARTESIAN_POINT ( 'NONE',  ( 4.956445790444027999, 24.88142650099568698, -39.98065363916886383 ) ) ;
#2700 = CARTESIAN_POINT ( 'NONE',  ( 0.6000166863083106206, -39.04292238714170793, 29.79049669240313847 ) ) ;
#2701 = CONICAL_SURFACE ( 'NONE', #48729, 42.92674063221959813, 1.485477209440487556 ) ;
#2702 = VERTEX_POINT ( 'NONE', #57355 ) ;
#2703 = AXIS2_PLACEMENT_3D ( 'NONE', #8726, #28143, #42892 ) ;
#2704 = CARTESIAN_POINT ( 'NONE',  ( -4.923482091946712380, -0.9563062221994939049, 3.000000000000061284 ) ) ;
#2705 = CARTESIAN_POINT ( 'NONE',  ( 0.5806925824938499181, 46.89268439822727430, 0.5463627657667635695 ) ) ;
#2706 = CARTESIAN_POINT ( 'NONE',  ( 2.526464513654349098, 25.19161096467279037, -34.82216969498438885 ) ) ;
#2707 = CARTESIAN_POINT ( 'NONE',  ( 0.8551540677456834771, 43.91216198251566993, -19.17641535420805354 ) ) ;
#2708 = ORIENTED_EDGE ( 'NONE', *, *, #9982, .T. ) ;
#2709 = CARTESIAN_POINT ( 'NONE',  ( 0.5782707292762423457, 36.35509350284772268, -29.63179930592838218 ) ) ;
#2710 = CARTESIAN_POINT ( 'NONE',  ( 0.1152339509894530906, 39.65706410057246245, -19.34579947632894914 ) ) ;
#2711 = VERTEX_POINT ( 'NONE', #24485 ) ;
#2712 = CARTESIAN_POINT ( 'NONE',  ( 0.2885700199627515561, 42.84523253167937185, 4.828949117911921718 ) ) ;
#2713 = EDGE_CURVE ( 'NONE', #23990, #45978, #57117, .T. ) ;
#2714 = B_SPLINE_CURVE_WITH_KNOTS ( 'NONE', 3,
 ( #14902, #34009, #48394, #47671 ),
 .UNSPECIFIED., .F., .F.,
 ( 4, 4 ),
 ( 8.009840277583554626E-17, 0.005004741218457497802 ),
 .UNSPECIFIED. ) ;
#2715 = EDGE_LOOP ( 'NONE', ( #53068, #64, #38704, #39941 ) ) ;
#2716 = DIRECTION ( 'NONE',  ( 0.000000000000000000, 0.000000000000000000, 1.000000000000000000 ) ) ;
#2717 = ORIENTED_EDGE ( 'NONE', *, *, #55538, .T. ) ;
#2718 = CARTESIAN_POINT ( 'NONE',  ( 0.7242486021783828276, 10.12618746694265326, 48.04655856310944984 ) ) ;
#2720 = CIRCLE ( 'NONE', #37781, 2.649999999999999467 ) ;
#2719 = CARTESIAN_POINT ( 'NONE',  ( 0.5998501479064699549, 44.24259072156085182, -18.89267974119621485 ) ) ;
#2721 = CARTESIAN_POINT ( 'NONE',  ( 4.967162193818130511, 43.02067033766018511, 2.375726030842731706 ) ) ;
#2722 = ORIENTED_EDGE ( 'NONE', *, *, #60540, .F. ) ;
#2723 = CARTESIAN_POINT ( 'NONE',  ( 0.7048096507298635682, -44.11842270945987821, 19.18768066167044140 ) ) ;
#2724 = DIRECTION ( 'NONE',  ( 1.000000000000000000, 0.000000000000000000, 0.000000000000000000 ) ) ;
#2725 = VERTEX_POINT ( 'NONE', #10707 ) ;
#2726 = VERTEX_POINT ( 'NONE', #20113 ) ;
#2727 = CARTESIAN_POINT ( 'NONE',  ( 4.549368137175248350, 0.000000000000000000, 0.000000000000000000 ) ) ;
#2728 = CARTESIAN_POINT ( 'NONE',  ( 0.7057020205115018818, -7.085441699093939505, 47.37450661940665952 ) ) ;
#2729 = CARTESIAN_POINT ( 'NONE',  ( 0.9790724872846762183, 38.59896336290614727, -16.32345665876211527 ) ) ;
#2730 = CARTESIAN_POINT ( 'NONE',  ( 0.1073791018717578927, -5.147744207006579309, -42.81622261970993293 ) ) ;
#2731 = LINE ( 'NONE', #21549, #50799 ) ;
#2732 = ORIENTED_EDGE ( 'NONE', *, *, #44512, .T. ) ;
#2733 = AXIS2_PLACEMENT_3D ( 'NONE', #54755, #9771, #40098 ) ;
#2734 = CARTESIAN_POINT ( 'NONE',  ( 4.291220156522060236, -46.81214323738926453, 5.292659334195587206 ) ) ;
#2735 = DIRECTION ( 'NONE',  ( 0.000000000000000000, 0.000000000000000000, -1.000000000000000000 ) ) ;
#2736 = ORIENTED_EDGE ( 'NONE', *, *, #34296, .T. ) ;
#2737 = CARTESIAN_POINT ( 'NONE',  ( 2.624215991343620935, -46.71702075422643929, -11.05657803851094201 ) ) ;
#2738 = DIRECTION ( 'NONE',  ( -1.000000000000000000, -0.000000000000000000, -0.000000000000000000 ) ) ;
#2739 = LINE ( 'NONE', #12480, #41873 ) ;
#2740 = CARTESIAN_POINT ( 'NONE',  ( 0.1129192098497455998, -42.80154921430131054, 10.72283417016679508 ) ) ;
#2741 = CARTESIAN_POINT ( 'NONE',  ( 0.5809828226811617480, -46.40184912890847357, 11.86925843957150128 ) ) ;
#2742 = CARTESIAN_POINT ( 'NONE',  ( 4.962356264823608143, 41.32726869310149453, -7.955655864260332777 ) ) ;
#2743 = CARTESIAN_POINT ( 'NONE',  ( 2.618530812446115519, 3.301668998266477306, -46.89163860459650124 ) ) ;
#2744 = SHAPE_REPRESENTATION_RELATIONSHIP ( 'NONE' , 'NONE' ,  #362, #34065 ) ;
#2746 = EDGE_CURVE ( 'NONE', #32390, #56965, #43941, .T. ) ;
#2745 = CARTESIAN_POINT ( 'NONE',  ( 0.6017667736363750963, 37.95278695280770620, 29.56223180955344532 ) ) ;
#2747 = CARTESIAN_POINT ( 'NONE',  ( 0.5850706913938534814, -33.99603398296567036, -33.73916126769486823 ) ) ;
#2748 = CARTESIAN_POINT ( 'NONE',  ( 5.000000000000007994, -54.69470952477976056, 58.44237546506787595 ) ) ;
#2749 = EDGE_CURVE ( 'NONE', #46714, #25119, #18114, .T. ) ;
#2750 = CARTESIAN_POINT ( 'NONE',  ( 0.1313383488274123545, -40.08066228784256424, -15.91164383651733161 ) ) ;
#2751 = CARTESIAN_POINT ( 'NONE',  ( -6.001507490154110336, -17.40350523682700157, 7.225628667346519762 ) ) ;
#2752 = CONICAL_SURFACE ( 'NONE', #47803, 43.92652462719577500, 1.486293639869522343 ) ;
#2753 = CIRCLE ( 'NONE', #37812, 2.649999999999985700 ) ;
#2754 = CARTESIAN_POINT ( 'NONE',  ( 5.895596859100789899, 17.95274561709302930, 9.067916410093047830 ) ) ;
#2755 = EDGE_CURVE ( 'NONE', #14506, #56562, #60466, .T. ) ;
#2756 = CARTESIAN_POINT ( 'NONE',  ( 2.009741617377216460, 16.48880107124495709, 40.83654633849385363 ) ) ;
#2757 = CARTESIAN_POINT ( 'NONE',  ( 0.9762797500689124330, -7.469026406145721886, -41.23758515880873432 ) ) ;
#2758 = CARTESIAN_POINT ( 'NONE',  ( 3.678834586032787346, -33.87007428955444510, -35.37556271281655285 ) ) ;
#2759 = APPLICATION_CONTEXT ( 'automotive_design' ) ;
#2760 =( BOUNDED_SURFACE ( )  B_SPLINE_SURFACE ( 3, 1, ( 
 ( #34936, #53998 ),
 ( #11425, #25507 ),
 ( #6999, #30209 ),
 ( #6682, #35554 ) ),
 .UNSPECIFIED., .F., .F., .F. ) 
 B_SPLINE_SURFACE_WITH_KNOTS ( ( 4, 4 ),
 ( 2, 2 ),
 ( 0.000000000000000000, 1.000000000000000000 ),
 ( 0.000000000000000000, 1.000000000000000000 ),
 .UNSPECIFIED. ) 
 GEOMETRIC_REPRESENTATION_ITEM ( )  RATIONAL_B_SPLINE_SURFACE ( (
 ( 1.000000000000000000, 1.000000000000000000),
 ( 0.9953040768229005630, 0.8617119497784937465),
 ( 0.9953040768229005630, 0.8617119497784937465),
 ( 1.000000000000000000, 1.000000000000000000) ) ) 
 REPRESENTATION_ITEM ( '' )  SURFACE ( )  );
#2761 = ORIENTED_EDGE ( 'NONE', *, *, #43531, .T. ) ;
#2762 = CARTESIAN_POINT ( 'NONE',  ( 0.5809828226811553087, 11.86925843957232729, -46.40184912890826752 ) ) ;
#2763 = EDGE_CURVE ( 'NONE', #19329, #57918, #30119, .T. ) ;
#2764 = CARTESIAN_POINT ( 'NONE',  ( 0.1095718737110178559, 37.21776476380626519, 21.78439022773168787 ) ) ;
#2765 = CARTESIAN_POINT ( 'NONE',  ( 5.981074661064941900, 20.35019299530688386, -2.670494474391787332 ) ) ;
#2766 = CARTESIAN_POINT ( 'NONE',  ( 4.960386119450146403, 38.83699438620099897, -20.15252668323582697 ) ) ;
#2767 = ORIENTED_EDGE ( 'NONE', *, *, #56931, .F. ) ;
#2768 = EDGE_CURVE ( 'NONE', #61018, #60897, #54119, .T. ) ;
#2769 = FACE_OUTER_BOUND ( 'NONE', #21973, .T. ) ;
#2770 = CYLINDRICAL_SURFACE ( 'NONE', #48946, 2.649999999999992806 ) ;
#2771 = CARTESIAN_POINT ( 'NONE',  ( 0.2279481005628808121, 43.97337838321706727, 3.584059240488700393 ) ) ;
#2772 = ORIENTED_EDGE ( 'NONE', *, *, #49016, .T. ) ;
#2773 = CARTESIAN_POINT ( 'NONE',  ( 5.901764892641288895, 39.27045567455304820, 29.25444886769604480 ) ) ;
#2774 = AXIS2_PLACEMENT_3D ( 'NONE', #40253, #59307, #16414 ) ;
#2775 = EDGE_LOOP ( 'NONE', ( #35597, #49308, #3343, #42126 ) ) ;
#2776 = CARTESIAN_POINT ( 'NONE',  ( 0.6028618097248862329, -29.14732267129602050, 38.27229381545001985 ) ) ;
#2777 = EDGE_LOOP ( 'NONE', ( #9549, #39429, #651, #25838 ) ) ;
#2778 = DIRECTION ( 'NONE',  ( -1.000000000000000000, -1.836909530733573776E-16, 1.103352205049209901E-32 ) ) ;
#2779 = VERTEX_POINT ( 'NONE', #47998 ) ;
#2780 = CARTESIAN_POINT ( 'NONE',  ( 0.1073791018717483448, -33.91564619577824402, 26.63563652260111070 ) ) ;
#2781 = CARTESIAN_POINT ( 'NONE',  ( 0.1097557419366048670, -26.42915440612308231, -34.07666148910637105 ) ) ;
#2782 = B_SPLINE_CURVE_WITH_KNOTS ( 'NONE', 3,
 ( #46593, #12160, #3637, #22770, #41904, #31241 ),
 .UNSPECIFIED., .F., .F.,
 ( 4, 2, 4 ),
 ( 0.000000000000000000, 0.0002447195606305748545, 0.0004894391212611497090 ),
 .UNSPECIFIED. ) ;
#2783 = ORIENTED_EDGE ( 'NONE', *, *, #26117, .F. ) ;
#2784 = B_SPLINE_CURVE_WITH_KNOTS ( 'NONE', 3,
 ( #52700, #37401, #19521, #9178 ),
 .UNSPECIFIED., .F., .F.,
 ( 4, 4 ),
 ( 1.301042606982605321E-18, 0.004048833967417090826 ),
 .UNSPECIFIED. ) ;
#2785 = ORIENTED_EDGE ( 'NONE', *, *, #7532, .T. ) ;
#2786 = CARTESIAN_POINT ( 'NONE',  ( 0.5782707292762423457, -38.25309408463888161, 27.13737545635878590 ) ) ;
#2787 = EDGE_CURVE ( 'NONE', #58874, #34772, #33539, .T. ) ;
#2788 = ORIENTED_EDGE ( 'NONE', *, *, #57317, .F. ) ;
#2789 = ORIENTED_EDGE ( 'NONE', *, *, #10264, .F. ) ;
#2790 = FACE_OUTER_BOUND ( 'NONE', #6094, .T. ) ;
#2791 = DIRECTION ( 'NONE',  ( 0.000000000000000000, 0.4999999999999992784, -0.8660254037844389297 ) ) ;
#2792 = CARTESIAN_POINT ( 'NONE',  ( 0.6021447746440204973, -25.67999315004615823, -41.85784383962067778 ) ) ;
#2793 = VECTOR ( 'NONE', #3966, 1000.000000000000000 ) ;
#2794 = CARTESIAN_POINT ( 'NONE',  ( 4.960156602257181468, 38.88108289790859828, 25.36362146861398159 ) ) ;
#2795 = ORIENTED_EDGE ( 'NONE', *, *, #50137, .F. ) ;
#2796 = CARTESIAN_POINT ( 'NONE',  ( 0.7413678028165009426, 5.162182772362567285, 43.79312686706632718 ) ) ;
#2797 = CARTESIAN_POINT ( 'NONE',  ( 5.838029081930955932, -43.47829931555671834, -18.45812955799640420 ) ) ;
#2798 = CARTESIAN_POINT ( 'NONE',  ( 0.5838002273316426072, -44.30203797796952614, 18.20308624554815680 ) ) ;
#2799 = B_SPLINE_CURVE_WITH_KNOTS ( 'NONE', 3,
 ( #26999, #22926, #2865, #26375 ),
 .UNSPECIFIED., .F., .F.,
 ( 4, 4 ),
 ( 0.000000000000000000, 0.005014147105413707325 ),
 .UNSPECIFIED. ) ;
#2800 = ORIENTED_EDGE ( 'NONE', *, *, #15957, .F. ) ;
#2801 = VERTEX_POINT ( 'NONE', #53586 ) ;
#2802 = CARTESIAN_POINT ( 'NONE',  ( 0.1073791018717483448, -30.14884492832410601, 30.83464511437086841 ) ) ;
#2803 = CARTESIAN_POINT ( 'NONE',  ( 0.3622758884714600280, -22.26738722580193652, 36.91764744403282350 ) ) ;
#2804 = CARTESIAN_POINT ( 'NONE',  ( 0.8551540677456739292, -41.94570365541218848, 23.16399837394531858 ) ) ;
#2805 = ORIENTED_EDGE ( 'NONE', *, *, #14358, .T. ) ;
#2806 = CARTESIAN_POINT ( 'NONE',  ( 0.1103878639767399555, -42.76182653383953891, -5.580746265796884487 ) ) ;
#2807 = CARTESIAN_POINT ( 'NONE',  ( 0.5804410086790514622, 4.150428748651751043, 46.71502748642842562 ) ) ;
#2808 = VECTOR ( 'NONE', #7267, 1000.000000000000341 ) ;
#2809 = VERTEX_POINT ( 'NONE', #57660 ) ;
#2810 = CARTESIAN_POINT ( 'NONE',  ( 0.6001305935487315502, 38.48510059944008077, 28.87057754790950881 ) ) ;
#2811 = ORIENTED_EDGE ( 'NONE', *, *, #52900, .T. ) ;
#2812 = CARTESIAN_POINT ( 'NONE',  ( 0.2940133293163009753, 39.39157466687257170, 19.86314161562180303 ) ) ;
#2813 = CARTESIAN_POINT ( 'NONE',  ( 5.896782393890504181, 5.965008392936887560, 19.20793486427431418 ) ) ;
#2814 = CARTESIAN_POINT ( 'NONE',  ( 0.6846871229502932144, -41.91507847151813593, 23.20185915381541619 ) ) ;
#2815 = SURFACE_STYLE_USAGE ( .BOTH. , #26634 ) ;
#2816 = SURFACE_STYLE_FILL_AREA ( #25400 ) ;
#2817 = MECHANICAL_DESIGN_GEOMETRIC_PRESENTATION_REPRESENTATION (  '', ( #48840 ), #50847 ) ;
#2818 = ORIENTED_EDGE ( 'NONE', *, *, #27002, .T. ) ;
#2819 = CARTESIAN_POINT ( 'NONE',  ( 5.896782393890504181, 19.00205529748295774, -6.591508275759957236 ) ) ;
#2820 = CARTESIAN_POINT ( 'NONE',  ( 4.967162193818130511, 0.000000000000000000, 0.000000000000000000 ) ) ;
#2821 = EDGE_CURVE ( 'NONE', #57549, #39665, #59140, .T. ) ;
#2822 = AXIS2_PLACEMENT_3D ( 'NONE', #46688, #22564, #41688 ) ;
#2823 = DIRECTION ( 'NONE',  ( 0.000000000000000000, 0.000000000000000000, -1.000000000000000000 ) ) ;
#2824 = CARTESIAN_POINT ( 'NONE',  ( 0.1104177457020373565, 21.55798761925387907, -37.34931850022147870 ) ) ;
#2825 = CARTESIAN_POINT ( 'NONE',  ( 5.959547316686252039, -5.315863417546468739, 19.82530672674353056 ) ) ;
#2826 = EDGE_CURVE ( 'NONE', #29313, #2228, #35102, .T. ) ;
#2827 = CARTESIAN_POINT ( 'NONE',  ( 0.5824935313925948543, 32.86262163222748711, 33.45573607785207315 ) ) ;
#2828 = CARTESIAN_POINT ( 'NONE',  ( 0.8551540677456715978, -44.61036085020962361, 17.49081417858771559 ) ) ;
#2829 = CARTESIAN_POINT ( 'NONE',  ( 0.6008122571543325074, -49.10565090547250833, 0.4354303792607690515 ) ) ;
#2830 = CARTESIAN_POINT ( 'NONE',  ( 0.6001305935487315502, 28.87057754790885866, 38.48510059944057815 ) ) ;
#2831 = ADVANCED_FACE ( 'NONE', ( #16323 ), #24501, .F. ) ;
#2832 =( BOUNDED_SURFACE ( )  B_SPLINE_SURFACE ( 3, 1, ( 
 ( #14884, #39304 ),
 ( #10475, #10166 ),
 ( #29570, #48678 ),
 ( #44023, #58362 ) ),
 .UNSPECIFIED., .F., .F., .F. ) 
 B_SPLINE_SURFACE_WITH_KNOTS ( ( 4, 4 ),
 ( 2, 2 ),
 ( 0.000000000000000000, 1.000000000000000000 ),
 ( 0.000000000000000000, 1.000000000000000000 ),
 .UNSPECIFIED. ) 
 GEOMETRIC_REPRESENTATION_ITEM ( )  RATIONAL_B_SPLINE_SURFACE ( (
 ( 1.000000000000000000, 1.000000000000000000),
 ( 0.9953390228620291325, 0.8624445117761032620),
 ( 0.9953390228620291325, 0.8624445117761032620),
 ( 1.000000000000000000, 1.000000000000000000) ) ) 
 REPRESENTATION_ITEM ( '' )  SURFACE ( )  );
#2833 = CARTESIAN_POINT ( 'NONE',  ( 0.1064266418746771803, 33.86837517279509768, 26.69589626339724120 ) ) ;
#2834 = CARTESIAN_POINT ( 'NONE',  ( -6.072942160501519027, -16.14637491494731947, 10.49279464179969246 ) ) ;
#2835 = B_SPLINE_CURVE_WITH_KNOTS ( 'NONE', 3,
 ( #22043, #60850, #23886, #9466, #23570, #52068 ),
 .UNSPECIFIED., .F., .F.,
 ( 4, 2, 4 ),
 ( 1.233001025668604810E-16, 0.0002448718616795908195, 0.0004897437233590583652 ),
 .UNSPECIFIED. ) ;
#2836 = VECTOR ( 'NONE', #3766, 1000.000000000000000 ) ;
#2837 = ORIENTED_EDGE ( 'NONE', *, *, #52913, .F. ) ;
#2838 = CARTESIAN_POINT ( 'NONE',  ( -4.915099999999998914, 9.539392014169456147, 3.000000000000000000 ) ) ;
#2839 = CARTESIAN_POINT ( 'NONE',  ( -6.016104459813374383, 18.68271063303497925, -2.454244026260903766 ) ) ;
#2840 = CARTESIAN_POINT ( 'NONE',  ( 1.834102595619085507, -42.25796167961109973, 12.42829109500596729 ) ) ;
#2841 = ORIENTED_EDGE ( 'NONE', *, *, #2144, .F. ) ;
#2842 = ADVANCED_FACE ( 'NONE', ( #45174 ), #45784, .F. ) ;
#2843 = CARTESIAN_POINT ( 'NONE',  ( 0.6029442701453591180, 44.20645327330244356, -21.38538552735501597 ) ) ;
#2844 = CARTESIAN_POINT ( 'NONE',  ( 3.238741278300274029, -42.82436441900176760, 3.793425828151925305 ) ) ;
#2845 = ORIENTED_EDGE ( 'NONE', *, *, #22515, .F. ) ;
#2846 = CARTESIAN_POINT ( 'NONE',  ( 0.5806925824938502512, 40.06810415365508504, -24.36738377166110325 ) ) ;
#2847 = CARTESIAN_POINT ( 'NONE',  ( 0.9752132459055862235, -41.50604997043404154, -10.88033124649664352 ) ) ;
#2848 = DIRECTION ( 'NONE',  ( 0.000000000000000000, 0.000000000000000000, 1.000000000000000000 ) ) ;
#2849 = ORIENTED_EDGE ( 'NONE', *, *, #33530, .F. ) ;
#2850 = CARTESIAN_POINT ( 'NONE',  ( 5.895596859100789899, -2.009647457887034694, 20.01223376606159121 ) ) ;
#2851 = AXIS2_PLACEMENT_3D ( 'NONE', #1046, #53963, #58982 ) ;
#2852 = VERTEX_POINT ( 'NONE', #26339 ) ;
#2853 = ORIENTED_EDGE ( 'NONE', *, *, #55652, .F. ) ;
#2854 = CARTESIAN_POINT ( 'NONE',  ( 0.1156867017252034557, 44.02533442314084056, 2.951734440256478909 ) ) ;
#2855 = VERTEX_POINT ( 'NONE', #1903 ) ;
#2856 = CARTESIAN_POINT ( 'NONE',  ( -6.072942160501519027, -8.919639966878298409, 17.06587780192650072 ) ) ;
#2857 = B_SPLINE_CURVE_WITH_KNOTS ( 'NONE', 3,
 ( #31874, #50959, #7732, #60054, #36272, #40676 ),
 .UNSPECIFIED., .F., .F.,
 ( 4, 2, 4 ),
 ( 5.966068130930023556E-18, 0.0002291472222819933963, 0.0004582944445639808295 ),
 .UNSPECIFIED. ) ;
#2858 = VERTEX_POINT ( 'NONE', #49840 ) ;
#2859 = CARTESIAN_POINT ( 'NONE',  ( 2.618530812446115519, 18.20180174657032879, 43.34075682745686464 ) ) ;
#2860 = PRODUCT_DEFINITION_FORMATION_WITH_SPECIFIED_SOURCE ( 'ANY', '', #16779, .NOT_KNOWN. ) ;
#2861 = CARTESIAN_POINT ( 'NONE',  ( 2.079412931998606329, -0.01372856698588024484, 44.03669822926320165 ) ) ;
#2862 = EDGE_LOOP ( 'NONE', ( #18275, #8560, #55564, #25530 ) ) ;
#2863 = CARTESIAN_POINT ( 'NONE',  ( 0.1149546198390367369, 14.98162911076433090, 41.50298006421608932 ) ) ;
#2864 = FACE_OUTER_BOUND ( 'NONE', #2427, .T. ) ;
#2865 = CARTESIAN_POINT ( 'NONE',  ( 4.833616638992208614, 46.11947910922909699, -3.476827473557382753 ) ) ;
#2866 = CARTESIAN_POINT ( 'NONE',  ( -6.078075953587585900, 3.078503442539340273, 19.00836633699512390 ) ) ;
#2867 = ORIENTED_EDGE ( 'NONE', *, *, #42320, .T. ) ;
#2868 = ADVANCED_FACE ( 'NONE', ( #45471 ), #58897, .F. ) ;
#2869 = CARTESIAN_POINT ( 'NONE',  ( 0.5839254288179547281, 44.21529885210830457, 18.41284501069694102 ) ) ;
#2870 = ORIENTED_EDGE ( 'NONE', *, *, #7147, .F. ) ;
#2871 = CARTESIAN_POINT ( 'NONE',  ( 0.7764139734771235979, -30.95828352313330711, 35.23670177823344574 ) ) ;
#2872 = ADVANCED_FACE ( 'NONE', ( #31044 ), #41733, .F. ) ;
#2873 = CARTESIAN_POINT ( 'NONE',  ( 0.7764146366350271888, -25.98546534488490778, -39.04863716544984698 ) ) ;
#2874 = CARTESIAN_POINT ( 'NONE',  ( 3.238741278300273141, 18.12697907494894878, -38.98370040185407959 ) ) ;
#2875 = EDGE_LOOP ( 'NONE', ( #61577, #34846, #28820, #58367 ) ) ;
#2876 = CARTESIAN_POINT ( 'NONE',  ( 0.5809828226811548646, -46.40184912890831015, -11.86925843957216742 ) ) ;
#2877 = CARTESIAN_POINT ( 'NONE',  ( 0.7048096507298579061, 11.63498350884271737, 46.68221792389243063 ) ) ;
#2878 = EDGE_CURVE ( 'NONE', #38025, #24504, #50156, .T. ) ;
#2879 = CARTESIAN_POINT ( 'NONE',  ( 0.9268187852002115479, 8.841305801404754305, -43.19242577853983533 ) ) ;
#2880 = SURFACE_STYLE_FILL_AREA ( #45835 ) ;
#2881 = AXIS2_PLACEMENT_3D ( 'NONE', #43874, #48844, #15347 ) ;
#2882 = AXIS2_PLACEMENT_3D ( 'NONE', #4169, #27696, #46826 ) ;
#2883 = ORIENTED_EDGE ( 'NONE', *, *, #21075, .T. ) ;
#2884 = ORIENTED_EDGE ( 'NONE', *, *, #27440, .T. ) ;
#2885 = CARTESIAN_POINT ( 'NONE',  ( 0.9787464366903567692, -39.53137008141080599, -13.91419319892470341 ) ) ;
#2886 = CARTESIAN_POINT ( 'NONE',  ( 4.060580049360325461, 42.38076202783113899, 11.63351642022113630 ) ) ;
#2887 = FACE_OUTER_BOUND ( 'NONE', #44367, .T. ) ;
#2888 = DIRECTION ( 'NONE',  ( -0.07836865515943411409, 0.5052769534812689978, 0.8593913859058567306 ) ) ;
#2889 = CARTESIAN_POINT ( 'NONE',  ( 0.5837799406558222826, 4.603457743365774846, -46.66960173798624822 ) ) ;
#2890 = CIRCLE ( 'NONE', #23925, 43.08621763946400307 ) ;
#2891 = CARTESIAN_POINT ( 'NONE',  ( 5.895881250540457863, 12.98195518060028419, -15.36217827318725071 ) ) ;
#2892 = EDGE_CURVE ( 'NONE', #53425, #45127, #11924, .T. ) ;
#2893 = CARTESIAN_POINT ( 'NONE',  ( 2.526552050251864134, -42.43615142762120485, -6.809858322089482385 ) ) ;
#2894 = CARTESIAN_POINT ( 'NONE',  ( 5.917102823773431552, -15.78915961314075034, 12.45761440896719385 ) ) ;
#2895 = CARTESIAN_POINT ( 'NONE',  ( -6.077587904424778920, 19.09718056542704900, 2.468545289316316893 ) ) ;
#2896 = ADVANCED_FACE ( 'NONE', ( #59533 ), #30910, .F. ) ;
#2897 = CARTESIAN_POINT ( 'NONE',  ( 0.3622758884714600280, -15.73321244754826509, -40.13994584881776007 ) ) ;
#2898 = CARTESIAN_POINT ( 'NONE',  ( 0.6000166863083090663, -20.35571918921453261, 44.69304395538859609 ) ) ;
#2899 = CARTESIAN_POINT ( 'NONE',  ( 5.896782393890504181, 14.92098591823879872, -13.48666994130618235 ) ) ;
#2900 = B_SPLINE_CURVE_WITH_KNOTS ( 'NONE', 3,
 ( #9818, #44284, #1020, #57399, #711, #28922, #5091, #43356, #48958, #48041, #6007, #24218, #38348, #1316, #34557, #53624 ),
 .UNSPECIFIED., .F., .F.,
 ( 4, 3, 3, 3, 3, 4 ),
 ( 2.030557555191247372E-17, 0.0002618515315864420852, 0.0003927756766342001596, 0.0005236998216950581068, 0.0007855159896329935850, 0.001047349442285931556 ),
 .UNSPECIFIED. ) ;
#2901 = CARTESIAN_POINT ( 'NONE',  ( 0.6025881611877910160, -33.86250327239872604, -34.17105830828403157 ) ) ;
#2902 = CARTESIAN_POINT ( 'NONE',  ( 4.549368137175248350, -2.596185425822241211, 42.84816078363925840 ) ) ;
#2903 = CARTESIAN_POINT ( 'NONE',  ( 0.6031357023905875581, -6.236038527293725764, -47.70157053127527291 ) ) ;
#2904 = B_SPLINE_CURVE_WITH_KNOTS ( 'NONE', 3,
 ( #43423, #47801, #52786, #23369 ),
 .UNSPECIFIED., .F., .F.,
 ( 4, 4 ),
 ( 9.309503074677274191E-17, 0.005004948556313900711 ),
 .UNSPECIFIED. ) ;
#2905 = EDGE_CURVE ( 'NONE', #61046, #46997, #36148, .T. ) ;
#2906 = CARTESIAN_POINT ( 'NONE',  ( 3.376099380956838925, -13.22083125066029474, 2.217657474370499759 ) ) ;
#2908 =( BOUNDED_SURFACE ( )  B_SPLINE_SURFACE ( 3, 1, ( 
 ( #3386, #22522 ),
 ( #41640, #56017 ),
 ( #13135, #861 ),
 ( #48473, #57540 ) ),
 .UNSPECIFIED., .F., .F., .F. ) 
 B_SPLINE_SURFACE_WITH_KNOTS ( ( 4, 4 ),
 ( 2, 2 ),
 ( 0.000000000000000000, 1.000000000000000000 ),
 ( 0.000000000000000000, 1.000000000000000000 ),
 .UNSPECIFIED. ) 
 GEOMETRIC_REPRESENTATION_ITEM ( )  RATIONAL_B_SPLINE_SURFACE ( (
 ( 1.000000000000000000, 1.000000000000000000),
 ( 0.9953040768229005630, 0.8617119497784937465),
 ( 0.9953040768229005630, 0.8617119497784937465),
 ( 1.000000000000000000, 1.000000000000000000) ) ) 
 REPRESENTATION_ITEM ( '' )  SURFACE ( )  );
#2907 = DIRECTION ( 'NONE',  ( -1.000000000000000000, -0.000000000000000000, -0.000000000000000000 ) ) ;
#2909 = CARTESIAN_POINT ( 'NONE',  ( 0.6029303876144825880, 46.50193792184025199, -12.32464004947830993 ) ) ;
#2911 = VERTEX_POINT ( 'NONE', #30407 ) ;
#2910 = CARTESIAN_POINT ( 'NONE',  ( 0.5804410086790514622, -41.60900809504509823, -21.63816760268458950 ) ) ;
#2912 = ORIENTED_EDGE ( 'NONE', *, *, #61029, .T. ) ;
#2913 = CARTESIAN_POINT ( 'NONE',  ( 0.6008122571543326185, 16.55073813642506764, -46.23448515561519656 ) ) ;
#2914 = CARTESIAN_POINT ( 'NONE',  ( 4.956653778116975495, -14.93973939759918323, 45.71126949320244393 ) ) ;
#2915 = CARTESIAN_POINT ( 'NONE',  ( -6.015611763856276717, -13.31979030221789984, -13.32857883366847318 ) ) ;
#2916 = ORIENTED_EDGE ( 'NONE', *, *, #24565, .T. ) ;
#2917 = EDGE_CURVE ( 'NONE', #47400, #1357, #48167, .T. ) ;
#2918 = ORIENTED_EDGE ( 'NONE', *, *, #34519, .T. ) ;
#2919 = DIRECTION ( 'NONE',  ( 1.000000000000000000, 0.000000000000000000, 0.000000000000000000 ) ) ;
#2920 = CARTESIAN_POINT ( 'NONE',  ( 0.9730545539215883499, 5.099196237955498923, -42.60426903087348194 ) ) ;
#2921 = B_SPLINE_CURVE_WITH_KNOTS ( 'NONE', 3,
 ( #37702, #56766, #19207, #47388 ),
 .UNSPECIFIED., .F., .F.,
 ( 4, 4 ),
 ( 0.000000000000000000, 0.005013413432710141573 ),
 .UNSPECIFIED. ) ;
#2922 = VECTOR ( 'NONE', #27208, 1000.000000000000114 ) ;
#2923 = ORIENTED_EDGE ( 'NONE', *, *, #6537, .F. ) ;
#2924 = ORIENTED_EDGE ( 'NONE', *, *, #38011, .T. ) ;
#2925 = CARTESIAN_POINT ( 'NONE',  ( 0.8751705887134423323, -11.58504748649167837, -46.67919521768883584 ) ) ;
#2926 =( BOUNDED_SURFACE ( )  B_SPLINE_SURFACE ( 3, 1, ( 
 ( #16153, #22383 ),
 ( #35579, #27086 ),
 ( #7647, #36196 ),
 ( #35267, #26775 ) ),
 .UNSPECIFIED., .F., .F., .F. ) 
 B_SPLINE_SURFACE_WITH_KNOTS ( ( 4, 4 ),
 ( 2, 2 ),
 ( 0.000000000000000000, 1.000000000000000000 ),
 ( 0.000000000000000000, 1.000000000000000000 ),
 .UNSPECIFIED. ) 
 GEOMETRIC_REPRESENTATION_ITEM ( )  RATIONAL_B_SPLINE_SURFACE ( (
 ( 1.000000000000000000, 1.000000000000000000),
 ( 0.7282232189291694135, 0.9929344683865672927),
 ( 0.7282232189291694135, 0.9929344683865672927),
 ( 1.000000000000000000, 1.000000000000000000) ) ) 
 REPRESENTATION_ITEM ( '' )  SURFACE ( )  );
#2927 = CONICAL_SURFACE ( 'NONE', #59943, 42.92674063221959813, 1.485477209440487556 ) ;
#2928 = DIRECTION ( 'NONE',  ( -0.07439287786467650709, 0.7991213610169827231, 0.5965490341031292054 ) ) ;
#2929 = CARTESIAN_POINT ( 'NONE',  ( 2.618530812446115519, 26.73752065161077951, -38.66305443964414224 ) ) ;
#2930 =( BOUNDED_SURFACE ( )  B_SPLINE_SURFACE ( 3, 1, ( 
 ( #53638, #48659 ),
 ( #44607, #48973 ),
 ( #11078, #16701 ),
 ( #15777, #1958 ) ),
 .UNSPECIFIED., .F., .F., .F. ) 
 B_SPLINE_SURFACE_WITH_KNOTS ( ( 4, 4 ),
 ( 2, 2 ),
 ( 0.000000000000000000, 1.000000000000000000 ),
 ( 0.000000000000000000, 1.000000000000000000 ),
 .UNSPECIFIED. ) 
 GEOMETRIC_REPRESENTATION_ITEM ( )  RATIONAL_B_SPLINE_SURFACE ( (
 ( 1.000000000000000000, 1.000000000000000000),
 ( 0.9953485035131437453, 0.8621029689291523912),
 ( 0.9953485035131437453, 0.8621029689291523912),
 ( 1.000000000000000000, 1.000000000000000000) ) ) 
 REPRESENTATION_ITEM ( '' )  SURFACE ( )  );
#2931 = EDGE_LOOP ( 'NONE', ( #46632, #22151, #51467, #15535 ) ) ;
#2932 = B_SPLINE_CURVE_WITH_KNOTS ( 'NONE', 3,
 ( #43118, #34948, #54012, #49028, #30218, #11135, #52793, #19301, #34025, #29605, #15523, #155, #29918, #6079, #20226, #33715, #25218, #38733, #48716 ),
 .UNSPECIFIED., .F., .F.,
 ( 4, 3, 3, 3, 3, 3, 4 ),
 ( 0.000000000000000000, 0.0002612768053151700827, 0.0003919133833142882692, 0.0005225499612322571756, 0.0006531865391693363922, 0.0008112755173415194237, 0.0009693688056799737657 ),
 .UNSPECIFIED. ) ;
#2933 = CARTESIAN_POINT ( 'NONE',  ( 4.833616638992205949, -30.83411269743588434, 34.47248434257857497 ) ) ;
#2934 = CARTESIAN_POINT ( 'NONE',  ( 0.8753041380234530822, -42.34096624980190171, 24.86726573039578980 ) ) ;
#2935 = CARTESIAN_POINT ( 'NONE',  ( 0.6031356755773454870, -48.10744332413212021, 2.564066922309144806E-05 ) ) ;
#2936 = ORIENTED_EDGE ( 'NONE', *, *, #59282, .T. ) ;
#2937 = ORIENTED_EDGE ( 'NONE', *, *, #56558, .F. ) ;
#2938 = CARTESIAN_POINT ( 'NONE',  ( 0.9972139404380323535, -29.87264297738548180, 30.80335716430307613 ) ) ;
#2939 = CIRCLE ( 'NONE', #47947, 72.00000000000002842 ) ;
#2940 = ORIENTED_EDGE ( 'NONE', *, *, #1538, .T. ) ;
#2941 = CARTESIAN_POINT ( 'NONE',  ( 0.6041374136657476912, -12.28249295042078160, 46.51335992032597488 ) ) ;
#2942 = LINE ( 'NONE', #22070, #32648 ) ;
#2943 = CARTESIAN_POINT ( 'NONE',  ( 5.895596859100789899, -2.016778947468235828, 20.01151633159107845 ) ) ;
#2944 = CARTESIAN_POINT ( 'NONE',  ( 0.8557997880470697982, 47.60865952216998664, 5.347802024197403803 ) ) ;
#2945 = EDGE_CURVE ( 'NONE', #3160, #38104, #19341, .T. ) ;
#2946 = ORIENTED_EDGE ( 'NONE', *, *, #1448, .F. ) ;
#2947 = CARTESIAN_POINT ( 'NONE',  ( -2.739355103387248747, 5.401627249124187458, 13.91653656670854744 ) ) ;
#2948 = DIRECTION ( 'NONE',  ( 2.280301054154487250E-31, 0.000000000000000000, -1.000000000000000000 ) ) ;
#2949 = ADVANCED_FACE ( 'NONE', ( #31980 ), #37710, .F. ) ;
#2950 = CARTESIAN_POINT ( 'NONE',  ( 0.1081432562775998252, 40.00205417854812140, -16.11101151263784459 ) ) ;
#2951 = ORIENTED_EDGE ( 'NONE', *, *, #35118, .F. ) ;
#2952 = CARTESIAN_POINT ( 'NONE',  ( 0.1087620492084205442, 42.80136086877933366, -5.269740196867475746 ) ) ;
#2953 = CARTESIAN_POINT ( 'NONE',  ( 1.154321713695926288, -26.77578845938205276, 33.53917066545415082 ) ) ;
#2954 = EDGE_CURVE ( 'NONE', #50432, #31086, #17901, .T. ) ;
#2955 = CARTESIAN_POINT ( 'NONE',  ( 0.7245667037590756143, 48.09508190954920082, -0.8205429720399597393 ) ) ;
#2956 = CARTESIAN_POINT ( 'NONE',  ( 0.6064782688330891958, -41.53115349968965830, -21.78296892996878498 ) ) ;
#2958 = EDGE_CURVE ( 'NONE', #14741, #10982, #9670, .T. ) ;
#2957 = B_SPLINE_CURVE_WITH_KNOTS ( 'NONE', 3,
 ( #35288, #39692, #54348, #30559 ),
 .UNSPECIFIED., .F., .F.,
 ( 4, 4 ),
 ( 0.000000000000000000, 0.004442905043737217438 ),
 .UNSPECIFIED. ) ;
#2959 = ORIENTED_EDGE ( 'NONE', *, *, #19256, .F. ) ;
#2960 = DIRECTION ( 'NONE',  ( -1.000000000000000000, -1.836909530733580185E-16, 1.836909530733574022E-16 ) ) ;
#2961 = EDGE_CURVE ( 'NONE', #31462, #32300, #59698, .T. ) ;
#2962 = CARTESIAN_POINT ( 'NONE',  ( -2.569797478183790229, 6.924386868080667945, 12.89088113963438431 ) ) ;
#2963 = CARTESIAN_POINT ( 'NONE',  ( 1.092182651088184242, 40.62377872806010970, 10.31841975769022035 ) ) ;
#2964 = CARTESIAN_POINT ( 'NONE',  ( 0.9730545539215883499, -15.95224156741799426, -39.83279466599056917 ) ) ;
#2965 = CARTESIAN_POINT ( 'NONE',  ( 0.5832655196449142432, -46.80593288449814793, 2.905138513940911160 ) ) ;
#2966 = EDGE_CURVE ( 'NONE', #53003, #59514, #17570, .T. ) ;
#2967 = CARTESIAN_POINT ( 'NONE',  ( 0.5786265663353153954, 11.69877690266720371, -46.45062944555881757 ) ) ;
#2968 = CARTESIAN_POINT ( 'NONE',  ( -6.072942160501519027, -18.27069728648816849, -6.081593784077838905 ) ) ;
#2969 = CARTESIAN_POINT ( 'NONE',  ( 0.5980271706414734822, 48.96187791475881568, -3.844964746511586373 ) ) ;
#2970 = EDGE_CURVE ( 'NONE', #7798, #11211, #32285, .T. ) ;
#2971 = DIRECTION ( 'NONE',  ( -1.000000000000000000, -0.000000000000000000, -0.000000000000000000 ) ) ;
#2972 = CARTESIAN_POINT ( 'NONE',  ( 4.967162193818130511, 0.000000000000000000, 0.000000000000000000 ) ) ;
#2973 = ORIENTED_EDGE ( 'NONE', *, *, #18346, .T. ) ;
#2974 = VECTOR ( 'NONE', #15899, 1000.000000000000000 ) ;
#2975 = CARTESIAN_POINT ( 'NONE',  ( -6.077587904424778920, 15.42837212129410673, 11.52221137980054699 ) ) ;
#2976 = CARTESIAN_POINT ( 'NONE',  ( 0.9754292580325131246, -18.16743313816920491, 37.76601435251217964 ) ) ;
#2977 = CARTESIAN_POINT ( 'NONE',  ( 0.6067099128993239665, -0.7089426894587230743, -47.89177823194874861 ) ) ;
#2978 = CARTESIAN_POINT ( 'NONE',  ( -6.016104459813371719, 14.95258000663132236, 11.46679299034585675 ) ) ;
#2979 = CARTESIAN_POINT ( 'NONE',  ( 2.643462169533613793, 1.382267876917792737, 48.01657676222237825 ) ) ;
#2980 = CARTESIAN_POINT ( 'NONE',  ( 5.896782393890504181, 19.70854070425246363, 4.012419492879101490 ) ) ;
#2981 = CARTESIAN_POINT ( 'NONE',  ( 0.6029303876144825880, -44.49541906039141281, 18.28892193312784542 ) ) ;
#2982 = CARTESIAN_POINT ( 'NONE',  ( 1.296416391601052487, 36.31792729719459345, -24.96628788810715704 ) ) ;
#2983 = CARTESIAN_POINT ( 'NONE',  ( 1.231276596079887264, -41.76121777166943616, 3.643825084340432952 ) ) ;
#2985 = ORIENTED_EDGE ( 'NONE', *, *, #29421, .F. ) ;
#2984 = CARTESIAN_POINT ( 'NONE',  ( 1.231276596079881047, -13.22565419922034557, 39.77887431816932917 ) ) ;
#2986 = ORIENTED_EDGE ( 'NONE', *, *, #38914, .F. ) ;
#2987 = CIRCLE ( 'NONE', #34010, 42.92674063221959813 ) ;
#2988 = CARTESIAN_POINT ( 'NONE',  ( 4.956653778116982600, -47.05699031914957686, 9.917440902360995736 ) ) ;
#2989 = CARTESIAN_POINT ( 'NONE',  ( 0.8560838555295158248, 46.89922841446242074, 0.9138972643637033322 ) ) ;
#2990 = CARTESIAN_POINT ( 'NONE',  ( 4.967162193818130511, -2.375726030842872927, 43.02067033766017801 ) ) ;
#2991 = ADVANCED_FACE ( 'NONE', ( #46390 ), #23123, .F. ) ;
#2992 = VERTEX_POINT ( 'NONE', #51676 ) ;
#2993 = CARTESIAN_POINT ( 'NONE',  ( 0.7242486021783833827, -47.28179493328054406, -13.24550226534200981 ) ) ;
#2994 = CARTESIAN_POINT ( 'NONE',  ( 0.5800708119828342779, -23.40241990038066078, 41.78924007434317645 ) ) ;
#2995 = CARTESIAN_POINT ( 'NONE',  ( 0.1084644655670283647, 41.55047717876504976, -11.54510651093217710 ) ) ;
#2997 = EDGE_CURVE ( 'NONE', #39074, #29160, #8897, .T. ) ;
#2996 = ORIENTED_EDGE ( 'NONE', *, *, #58617, .T. ) ;
#2998 = EDGE_LOOP ( 'NONE', ( #11330, #45882, #7990, #51314 ) ) ;
#2999 = FACE_OUTER_BOUND ( 'NONE', #60876, .T. ) ;
#3000 = DIRECTION ( 'NONE',  ( 0.000000000000000000, 0.000000000000000000, 1.000000000000000000 ) ) ;
#3001 = CARTESIAN_POINT ( 'NONE',  ( 0.9762797500689124330, 32.57381952463267538, -26.36799322592379369 ) ) ;
#3002 = ORIENTED_EDGE ( 'NONE', *, *, #44980, .F. ) ;
#3003 = CARTESIAN_POINT ( 'NONE',  ( 2.500000000000000000, 1.178949249685212974, -2.042000000000001148 ) ) ;
#3004 = B_SPLINE_CURVE_WITH_KNOTS ( 'NONE', 3,
 ( #53832, #24736, #39170, #43877 ),
 .UNSPECIFIED., .F., .F.,
 ( 4, 4 ),
 ( 6.505213034913026604E-19, 0.004048833967417084755 ),
 .UNSPECIFIED. ) ;
#3005 = CARTESIAN_POINT ( 'NONE',  ( 1.227938101723748288, -6.439911493064859549, 42.43379953535183802 ) ) ;
#3006 =( BOUNDED_SURFACE ( )  B_SPLINE_SURFACE ( 3, 1, ( 
 ( #9387, #61681 ),
 ( #18814, #37938 ),
 ( #51368, #52290 ),
 ( #4659, #56996 ) ),
 .UNSPECIFIED., .F., .F., .F. ) 
 B_SPLINE_SURFACE_WITH_KNOTS ( ( 4, 4 ),
 ( 2, 2 ),
 ( 0.000000000000000000, 1.000000000000000000 ),
 ( 0.000000000000000000, 1.000000000000000000 ),
 .UNSPECIFIED. ) 
 GEOMETRIC_REPRESENTATION_ITEM ( )  RATIONAL_B_SPLINE_SURFACE ( (
 ( 1.000000000000000000, 1.000000000000000000),
 ( 0.7223157951917476005, 0.9931996967497186413),
 ( 0.7223157951917476005, 0.9931996967497186413),
 ( 1.000000000000000000, 1.000000000000000000) ) ) 
 REPRESENTATION_ITEM ( '' )  SURFACE ( )  );
#3007 = CARTESIAN_POINT ( 'NONE',  ( 0.8557997880470599172, -38.55640757422458620, 28.43566216844957140 ) ) ;
#3008 = CARTESIAN_POINT ( 'NONE',  ( -6.016761891674565099, -7.214149619366484245, 17.40752468084780702 ) ) ;
#3009 = ORIENTED_EDGE ( 'NONE', *, *, #28279, .T. ) ;
#3010 = CARTESIAN_POINT ( 'NONE',  ( 0.5980271706414711508, -31.16543947089417443, 37.95740540958632891 ) ) ;
#3011 = CARTESIAN_POINT ( 'NONE',  ( 3.238018933889920792, 7.722174679335315872, 10.94419986063327777 ) ) ;
#3012 = EDGE_LOOP ( 'NONE', ( #34469, #21920 ) ) ;
#3013 = CARTESIAN_POINT ( 'NONE',  ( 3.782625744892855302, -32.30858446067052370, -26.89597505655302712 ) ) ;
#3014 = FACE_OUTER_BOUND ( 'NONE', #394, .T. ) ;
#3015 = CARTESIAN_POINT ( 'NONE',  ( 0.9787284016396604613, 4.008534792623077436, -41.71651528765511330 ) ) ;
#3016 = CARTESIAN_POINT ( 'NONE',  ( -6.001507490154111224, 16.32705935667520336, -9.408444979392148966 ) ) ;
#3017 = VERTEX_POINT ( 'NONE', #18490 ) ;
#3018 = EDGE_LOOP ( 'NONE', ( #58492, #39630, #26110, #795 ) ) ;
#3019 = CARTESIAN_POINT ( 'NONE',  ( 0.6031356755773454870, 44.44547243635321365, -18.40994522247712695 ) ) ;
#3020 = ADVANCED_FACE ( 'NONE', ( #56681 ), #33309, .F. ) ;
#3021 = VERTEX_POINT ( 'NONE', #53520 ) ;
#3022 = CARTESIAN_POINT ( 'NONE',  ( 0.9730545539215892381, -15.95224156741857691, 39.83279466599033469 ) ) ;
#3023 = VECTOR ( 'NONE', #13591, 1000.000000000000227 ) ;
#3024 = VERTEX_POINT ( 'NONE', #52287 ) ;
#3025 = CARTESIAN_POINT ( 'NONE',  ( 0.9762797500689124330, -39.75277516423506086, -13.26806888463731227 ) ) ;
#3027 = VERTEX_POINT ( 'NONE', #34143 ) ;
#3026 = ADVANCED_FACE ( 'NONE', ( #24413 ), #48125, .F. ) ;
#3028 = CARTESIAN_POINT ( 'NONE',  ( 1.227938101723748288, -41.23019537246701560, -11.92353943227992197 ) ) ;
#3029 = CARTESIAN_POINT ( 'NONE',  ( 0.6016117650947688800, -48.74769398499142170, -5.934086735979687610 ) ) ;
#3030 = EDGE_CURVE ( 'NONE', #57391, #57208, #19421, .T. ) ;
#3031 = VECTOR ( 'NONE', #20456, 1000.000000000000000 ) ;
#3032 = CARTESIAN_POINT ( 'NONE',  ( 0.1129192098497447394, -43.69739906996321110, 6.122834499276631703 ) ) ;
#3033 = ORIENTED_EDGE ( 'NONE', *, *, #21432, .T. ) ;
#3034 = CARTESIAN_POINT ( 'NONE',  ( 4.962356264823596597, 37.75702904547799932, 18.59145920903680249 ) ) ;
#3035 = EDGE_CURVE ( 'NONE', #40578, #41808, #39541, .T. ) ;
#3036 = DIRECTION ( 'NONE',  ( 0.07439287786467665975, -0.9262902123089823414, 0.3693942911085547620 ) ) ;
#3037 = CARTESIAN_POINT ( 'NONE',  ( 5.895596859100789899, -18.51832497669317945, -7.848555489392246010 ) ) ;
#3038 = ORIENTED_EDGE ( 'NONE', *, *, #31491, .T. ) ;
#3039 = ORIENTED_EDGE ( 'NONE', *, *, #38008, .T. ) ;
#3040 = CARTESIAN_POINT ( 'NONE',  ( 4.553261556744873317, 43.59419396814051595, 5.393126930805304475 ) ) ;
#3041 = CARTESIAN_POINT ( 'NONE',  ( 1.231276596079887264, -26.41281459480383376, 32.55211200826430229 ) ) ;
#3042 = CARTESIAN_POINT ( 'NONE',  ( 42.00000000000000711, 6.547216728259810428E-15, -1.617781153285278467E-30 ) ) ;
#3043 = EDGE_CURVE ( 'NONE', #26290, #28220, #24107, .T. ) ;
#3044 = CARTESIAN_POINT ( 'NONE',  ( 5.901463166500145796, -19.93509711719968891, 2.666415809369121259 ) ) ;
#3045 = CARTESIAN_POINT ( 'NONE',  ( 4.956653778116975495, 14.93973939759886704, 45.71126949320255761 ) ) ;
#3046 = ORIENTED_EDGE ( 'NONE', *, *, #47425, .T. ) ;
#3047 = CARTESIAN_POINT ( 'NONE',  ( 2.618530812446115519, -46.78761446237187016, 4.543778396736469105 ) ) ;
#3048 = CARTESIAN_POINT ( 'NONE',  ( 0.8744876279028306332, -48.79802643035336018, -5.394688766001929814 ) ) ;
#3049 = ORIENTED_EDGE ( 'NONE', *, *, #5210, .F. ) ;
#3050 = B_SPLINE_CURVE_WITH_KNOTS ( 'NONE', 3,
 ( #39099, #47554, #4594, #38475 ),
 .UNSPECIFIED., .F., .F.,
 ( 4, 4 ),
 ( 0.000000000000000000, 0.004446090762761381598 ),
 .UNSPECIFIED. ) ;
#3051 = DIRECTION ( 'NONE',  ( 1.000000000000000000, 1.836970198721027962E-16, -2.033782021272921061E-31 ) ) ;
#3052 = CARTESIAN_POINT ( 'NONE',  ( 0.7056313189692721144, -42.23391001524242938, -20.39719315940220667 ) ) ;
#3053 = DIRECTION ( 'NONE',  ( 0.09722883295013594329, 0.4670337431504633652, 0.8788777143619136423 ) ) ;
#3054 = LINE ( 'NONE', #56291, #8679 ) ;
#3055 = FACE_OUTER_BOUND ( 'NONE', #18462, .T. ) ;
#3056 = LINE ( 'NONE', #11881, #37628 ) ;
#3057 = FILL_AREA_STYLE ('',( #55057 ) ) ;
#3058 = CARTESIAN_POINT ( 'NONE',  ( 0.5817217712918324457, 10.42802360358725267, 45.72189057477174146 ) ) ;
#3059 = CARTESIAN_POINT ( 'NONE',  ( 0.9757402383260953549, -39.67468066200768817, 16.34189654378420187 ) ) ;
#3060 = CARTESIAN_POINT ( 'NONE',  ( 4.962356264823609031, 31.50371261889155150, -27.90612278853226513 ) ) ;
#3061 = CARTESIAN_POINT ( 'NONE',  ( 1.157644175074336479, 10.51841484064714471, -40.57542636521812796 ) ) ;
#3062 = CARTESIAN_POINT ( 'NONE',  ( 0.8753041380234471980, 46.31375555491744223, 16.31485134079786548 ) ) ;
#3063 = CARTESIAN_POINT ( 'NONE',  ( 4.967162193818130511, 13.42934394584164082, 40.93989340068615945 ) ) ;
#3064 = CARTESIAN_POINT ( 'NONE',  ( 0.3622758884714600280, 0.8252992914328071139, -43.10531414739104861 ) ) ;
#3065 = CARTESIAN_POINT ( 'NONE',  ( 0.5549461598389363592, 16.05292175970580715, 41.07945226562262064 ) ) ;
#3066 = CARTESIAN_POINT ( 'NONE',  ( 1.157643937452369043, -7.784786284043311966, -41.18736914524311743 ) ) ;
#3067 = DIRECTION ( 'NONE',  ( -1.000000000000000000, -0.000000000000000000, -0.000000000000000000 ) ) ;
#3068 = ADVANCED_FACE ( 'NONE', ( #57283 ), #53218, .F. ) ;
#3069 = VERTEX_POINT ( 'NONE', #58215 ) ;
#3070 = B_SPLINE_CURVE_WITH_KNOTS ( 'NONE', 3,
 ( #43460, #23404, #38149, #185, #38449, #3964 ),
 .UNSPECIFIED., .F., .F.,
 ( 4, 2, 4 ),
 ( 9.946927139006897773E-18, 0.0002445244328975399502, 0.0004890488657950700343 ),
 .UNSPECIFIED. ) ;
#3071 = CARTESIAN_POINT ( 'NONE',  ( 0.1103310638050662013, 11.24099191366999406, -41.63362651001254733 ) ) ;
#3072 = B_SPLINE_CURVE_WITH_KNOTS ( 'NONE', 3,
 ( #52894, #29703, #48819, #10304 ),
 .UNSPECIFIED., .F., .F.,
 ( 4, 4 ),
 ( 2.180944827630287245E-17, 0.004564976165746189446 ),
 .UNSPECIFIED. ) ;
#3073 = CARTESIAN_POINT ( 'NONE',  ( 2.185380717157383135, -32.61424324914600703, -29.58261212862606016 ) ) ;
#3074 = CARTESIAN_POINT ( 'NONE',  ( 0.9752570700956798566, -39.55341424149096241, -16.63323182627910768 ) ) ;
#3075 = DIRECTION ( 'NONE',  ( -1.000000000000000000, 0.000000000000000000, 0.000000000000000000 ) ) ;
#3076 = ORIENTED_EDGE ( 'NONE', *, *, #7655, .F. ) ;
#3077 = CARTESIAN_POINT ( 'NONE',  ( 1.834102595619085507, -40.32172980854549849, 17.73008319507659536 ) ) ;
#3078 = CARTESIAN_POINT ( 'NONE',  ( 1.231276596079887931, -41.24008908601417289, -7.518764738684258653 ) ) ;
#3079 = CARTESIAN_POINT ( 'NONE',  ( 0.5998501479064699549, -29.69975237324587169, -37.84527566984847624 ) ) ;
#3080 = ORIENTED_EDGE ( 'NONE', *, *, #61543, .T. ) ;
#3081 = CARTESIAN_POINT ( 'NONE',  ( 0.3676999524040366896, -26.85386693986640338, 34.99743438737744583 ) ) ;
#3082 = ORIENTED_EDGE ( 'NONE', *, *, #55762, .F. ) ;
#3083 = CARTESIAN_POINT ( 'NONE',  ( -6.077587904424778920, 12.01079512011132522, 15.05114022181178335 ) ) ;
#3084 = DIRECTION ( 'NONE',  ( 0.000000000000000000, 0.000000000000000000, -1.000000000000000000 ) ) ;
#3085 = EDGE_LOOP ( 'NONE', ( #44814, #33317 ) ) ;
#3086 = CARTESIAN_POINT ( 'NONE',  ( 1.231276596079881047, -30.51591784428347154, -28.74118176309054107 ) ) ;
#3087 = VERTEX_POINT ( 'NONE', #10018 ) ;
#3088 = CARTESIAN_POINT ( 'NONE',  ( 2.099999999999999645, 0.000000000000000000, -0.2800830152838832965 ) ) ;
#3089 = CARTESIAN_POINT ( 'NONE',  ( 3.407937589446178528, -4.815089211105147982, 12.82481284928202214 ) ) ;
#3090 = EDGE_CURVE ( 'NONE', #18280, #1366, #7126, .T. ) ;
#3091 = B_SPLINE_CURVE_WITH_KNOTS ( 'NONE', 3,
 ( #4425, #23566, #42692, #33298, #30412, #44252, #2208, #1907, #40174, #16330, #39863, #44557, #59539, #35143, #45178, #54514, #15729, #59222, #25108 ),
 .UNSPECIFIED., .F., .F.,
 ( 4, 3, 3, 3, 3, 3, 4 ),
 ( 3.469552829456483146E-18, 0.0002612768053151643365, 0.0003919133833142878897, 0.0005225499612322573924, 0.0006531865391693325975, 0.0008112755173415177974, 0.0009693688056799712720 ),
 .UNSPECIFIED. ) ;
#3092 = VERTEX_POINT ( 'NONE', #10635 ) ;
#3093 = CARTESIAN_POINT ( 'NONE',  ( 4.975610109902397937, 2.142807115709817189, -48.86571174967818365 ) ) ;
#3094 = ADVANCED_FACE ( 'NONE', ( #273, #23485 ), #33217, .F. ) ;
#3095 = ORIENTED_EDGE ( 'NONE', *, *, #9104, .T. ) ;
#3096 = CARTESIAN_POINT ( 'NONE',  ( 0.5839880159502348622, -37.97080096460561549, -29.19321933421534254 ) ) ;
#3098 = EDGE_CURVE ( 'NONE', #12553, #38470, #4657, .T. ) ;
#3097 = ORIENTED_EDGE ( 'NONE', *, *, #1827, .F. ) ;
#3099 = EDGE_LOOP ( 'NONE', ( #48891, #51529, #45073, #20272 ) ) ;
#3100 = CARTESIAN_POINT ( 'NONE',  ( -6.017396004339687465, -9.420565012089314294, -16.31924478664284806 ) ) ;
#3101 = CARTESIAN_POINT ( 'NONE',  ( 4.549368137175248350, 42.06008734272396765, -8.582197505783977221 ) ) ;
#3102 = CARTESIAN_POINT ( 'NONE',  ( 0.5806925824938499181, -44.47729014209976128, 14.86583411581871772 ) ) ;
#3103 = EDGE_CURVE ( 'NONE', #36669, #44819, #10148, .T. ) ;
#3104 = CARTESIAN_POINT ( 'NONE',  ( 5.910764540655177868, 19.00446553125926030, -6.582668785556639257 ) ) ;
#3105 = CARTESIAN_POINT ( 'NONE',  ( 0.6017666602106489515, 44.57804174182696499, 18.08695057064608136 ) ) ;
#3106 = EDGE_LOOP ( 'NONE', ( #22450, #37626, #44503, #53723 ) ) ;
#3107 = CARTESIAN_POINT ( 'NONE',  ( 0.8753041380234530822, 3.828530797421374032, -48.95386276695819561 ) ) ;
#3108 = EDGE_CURVE ( 'NONE', #1361, #7783, #39466, .T. ) ;
#3109 = CARTESIAN_POINT ( 'NONE',  ( 0.9789233960466710016, -17.76001420651944684, 37.95943390274106832 ) ) ;
#3110 = CARTESIAN_POINT ( 'NONE',  ( 2.114184763582917181, 7.651710973661706259E-12, 44.03514965515166324 ) ) ;
#3111 = ORIENTED_EDGE ( 'NONE', *, *, #14511, .T. ) ;
#3112 = B_SPLINE_CURVE_WITH_KNOTS ( 'NONE', 3,
 ( #34545, #30129, #48940, #10111, #6295, #25431 ),
 .UNSPECIFIED., .F., .F.,
 ( 4, 2, 4 ),
 ( 2.033052538357063276E-17, 0.0002293755540694316438, 0.0004587511081388429587 ),
 .UNSPECIFIED. ) ;
#3113 = ORIENTED_EDGE ( 'NONE', *, *, #24046, .T. ) ;
#3114 = CIRCLE ( 'NONE', #43172, 2.099999999999999645 ) ;
#3115 = CARTESIAN_POINT ( 'NONE',  ( -6.078075953587585900, -17.34679059108042765, 8.359666885488888255 ) ) ;
#3116 = CARTESIAN_POINT ( 'NONE',  ( 0.8753041380234524160, 23.49739456791611403, 43.11624724384818563 ) ) ;
#3117 = CARTESIAN_POINT ( 'NONE',  ( 0.5837800005270555870, -44.30119575061277004, 15.38308531172059723 ) ) ;
#3118 = ORIENTED_EDGE ( 'NONE', *, *, #60033, .F. ) ;
#3119 = CARTESIAN_POINT ( 'NONE',  ( 0.1095718737110178004, -42.72125633542930245, -5.883530294869984800 ) ) ;
#3120 = CARTESIAN_POINT ( 'NONE',  ( -6.017396004339686577, -16.31807101179377284, 9.422598049764564720 ) ) ;
#3121 = ADVANCED_FACE ( 'NONE', ( #26809 ), #46124, .F. ) ;
#3122 = VERTEX_POINT ( 'NONE', #2988 ) ;
#3123 = CARTESIAN_POINT ( 'NONE',  ( 2.347501380054781706, -0.2125736986915482685, -41.96959656111437198 ) ) ;
#3124 = EDGE_LOOP ( 'NONE', ( #40321, #51696, #41255, #17315 ) ) ;
#3125 = EDGE_CURVE ( 'NONE', #34487, #8248, #16327, .T. ) ;
#3126 = CARTESIAN_POINT ( 'NONE',  ( 0.9754642270333666598, -34.14824330022352683, 25.98138239028847352 ) ) ;
#3127 = CARTESIAN_POINT ( 'NONE',  ( 4.303969348037258058, -35.51084504003173947, -32.45857549159337907 ) ) ;
#3128 = CARTESIAN_POINT ( 'NONE',  ( 3.050102900204245682, -43.36385787569175676, 7.416271254132083435 ) ) ;
#3129 = CARTESIAN_POINT ( 'NONE',  ( -1.114299999999999846, 0.000000000000000000, 0.000000000000000000 ) ) ;
#3130 =( BOUNDED_SURFACE ( )  B_SPLINE_SURFACE ( 3, 1, ( 
 ( #16809, #32138 ),
 ( #36536, #12733 ),
 ( #41239, #12117 ),
 ( #60607, #45947 ) ),
 .UNSPECIFIED., .F., .F., .F. ) 
 B_SPLINE_SURFACE_WITH_KNOTS ( ( 4, 4 ),
 ( 2, 2 ),
 ( 0.000000000000000000, 1.000000000000000000 ),
 ( 0.000000000000000000, 1.000000000000000000 ),
 .UNSPECIFIED. ) 
 GEOMETRIC_REPRESENTATION_ITEM ( )  RATIONAL_B_SPLINE_SURFACE ( (
 ( 1.000000000000000000, 1.000000000000000000),
 ( 0.7223157951917480446, 0.9931996967497186413),
 ( 0.7223157951917480446, 0.9931996967497186413),
 ( 1.000000000000000000, 1.000000000000000000) ) ) 
 REPRESENTATION_ITEM ( '' )  SURFACE ( )  );
#3131 = ORIENTED_EDGE ( 'NONE', *, *, #11533, .T. ) ;
#3132 = CARTESIAN_POINT ( 'NONE',  ( 0.9756008150404595902, 21.33101788548782096, -37.23069985082522493 ) ) ;
#3133 = CARTESIAN_POINT ( 'NONE',  ( 2.618530812446115519, -18.50060774051936363, 43.21405214082143686 ) ) ;
#3134 = CARTESIAN_POINT ( 'NONE',  ( 3.407937589446178528, 3.099921468255189883, -13.34359005742686044 ) ) ;
#3135 = CARTESIAN_POINT ( 'NONE',  ( 0.1100053167205930493, -16.66867746965619546, -39.77279469894207864 ) ) ;
#3136 = LINE ( 'NONE', #36383, #4170 ) ;
#3137 = CARTESIAN_POINT ( 'NONE',  ( 0.5834584762367762689, 32.47060451932831171, 33.83630936084141183 ) ) ;
#3138 = CARTESIAN_POINT ( 'NONE',  ( 0.6064782688330851990, -38.25720568296584645, -27.12417113480179509 ) ) ;
#3139 = CARTESIAN_POINT ( 'NONE',  ( -2.601141883200662974, 2.883136076038183671, -14.64523655788583589 ) ) ;
#3140 = CARTESIAN_POINT ( 'NONE',  ( -6.016489644550736315, -11.47450955518478111, -14.94663725562927503 ) ) ;
#3141 = B_SPLINE_CURVE_WITH_KNOTS ( 'NONE', 3,
 ( #22316, #41446, #47066, #37055 ),
 .UNSPECIFIED., .F., .F.,
 ( 4, 4 ),
 ( 0.000000000000000000, 0.004447772540403798977 ),
 .UNSPECIFIED. ) ;
#3142 = B_SPLINE_CURVE_WITH_KNOTS ( 'NONE', 3,
 ( #47852, #52841, #61907, #14962, #43792, #24031 ),
 .UNSPECIFIED., .F., .F.,
 ( 4, 2, 4 ),
 ( 1.253145692779649283E-17, 0.0002293319059085063491, 0.0004586638118170001757 ),
 .UNSPECIFIED. ) ;
#3143 = EDGE_CURVE ( 'NONE', #17913, #53301, #52153, .T. ) ;
#3144 = LINE ( 'NONE', #11641, #21277 ) ;
#3145 = CARTESIAN_POINT ( 'NONE',  ( -6.057079549204054558, -16.14367994231351489, 10.49822980410900541 ) ) ;
#3146 = ORIENTED_EDGE ( 'NONE', *, *, #17564, .T. ) ;
#3147 = EDGE_CURVE ( 'NONE', #48016, #35743, #22417, .T. ) ;
#3148 = LINE ( 'NONE', #60770, #1849 ) ;
#3149 = CARTESIAN_POINT ( 'NONE',  ( 0.5804410086790514622, 10.33990028284823559, -45.74501408892724186 ) ) ;
#3150 = CARTESIAN_POINT ( 'NONE',  ( -6.072942160501519027, -4.299083787220820518, 18.77024349547643567 ) ) ;
#3151 = CARTESIAN_POINT ( 'NONE',  ( 0.2279481005628808954, -18.55039463836296321, 40.02981820885408126 ) ) ;
#3152 = ORIENTED_EDGE ( 'NONE', *, *, #42797, .F. ) ;
#3153 = CARTESIAN_POINT ( 'NONE',  ( 5.896782393890504181, 19.71107130340476132, -3.999969368645934775 ) ) ;
#3154 = CARTESIAN_POINT ( 'NONE',  ( 0.9787284016396613495, -41.82716437040105717, -2.612339882228906340 ) ) ;
#3155 = AXIS2_PLACEMENT_3D ( 'NONE', #36886, #13071, #23381 ) ;
#3156 = ORIENTED_EDGE ( 'NONE', *, *, #58570, .F. ) ;
#3157 = CARTESIAN_POINT ( 'NONE',  ( 0.7242486021783807182, -45.19981481568854775, -19.18301861025617683 ) ) ;
#3158 = CARTESIAN_POINT ( 'NONE',  ( 0.7057020205115055456, -41.05685587925817970, -24.67553336431228672 ) ) ;
#3159 = CARTESIAN_POINT ( 'NONE',  ( 0.5997462898726536595, 37.05192695178125462, 32.22896739432052016 ) ) ;
#3160 = VERTEX_POINT ( 'NONE', #41545 ) ;
#3161 = CARTESIAN_POINT ( 'NONE',  ( 0.6017667736363749853, 29.00830848931575900, 38.37782726569699321 ) ) ;
#3162 = ORIENTED_EDGE ( 'NONE', *, *, #6685, .T. ) ;
#3163 = ORIENTED_EDGE ( 'NONE', *, *, #6308, .F. ) ;
#3164 = CARTESIAN_POINT ( 'NONE',  ( 4.975801465491695552, 42.71626295676264817, -21.70134120755155394 ) ) ;
#3165 = ORIENTED_EDGE ( 'NONE', *, *, #18905, .T. ) ;
#3166 = CARTESIAN_POINT ( 'NONE',  ( 0.5850706913938534814, 0.1816364388700339449, 47.89601588673689037 ) ) ;
#3167 = ORIENTED_EDGE ( 'NONE', *, *, #48873, .T. ) ;
#3168 = CARTESIAN_POINT ( 'NONE',  ( 3.680882792899937250, 27.71664061799148371, -39.15943299201958894 ) ) ;
#3169 = CARTESIAN_POINT ( 'NONE',  ( 1.479689385636123067, -0.2368883799086275443, 44.06277033010017874 ) ) ;
#3170 = EDGE_CURVE ( 'NONE', #2911, #39295, #36852, .T. ) ;
#3171 = ORIENTED_EDGE ( 'NONE', *, *, #41295, .T. ) ;
#3172 = CARTESIAN_POINT ( 'NONE',  ( 0.1158516988532803382, 15.28513351191913294, 41.39211099177720143 ) ) ;
#3173 = CARTESIAN_POINT ( 'NONE',  ( 4.960156602257181468, 44.12083041402485151, -14.43621227656483796 ) ) ;
#3174 = CARTESIAN_POINT ( 'NONE',  ( 2.185380717157384023, -37.63955117804344752, 22.84915731887389256 ) ) ;
#3175 = CARTESIAN_POINT ( 'NONE',  ( 0.5806925824938502512, -29.85799195566318431, 36.16244846134061675 ) ) ;
#3176 = ORIENTED_EDGE ( 'NONE', *, *, #25244, .F. ) ;
#3177 = EDGE_CURVE ( 'NONE', #9918, #36162, #12574, .T. ) ;
#3178 = DIRECTION ( 'NONE',  ( 0.5000000000000025535, -0.8660254037844371533, 0.000000000000000000 ) ) ;
#3179 = EDGE_LOOP ( 'NONE', ( #47636, #54086, #41638, #28463 ) ) ;
#3180 = CARTESIAN_POINT ( 'NONE',  ( 4.975610109902397937, 39.54077024310134902, 28.79195887257488451 ) ) ;
#3181 = B_SPLINE_CURVE_WITH_KNOTS ( 'NONE', 3,
 ( #5499, #33434, #42840, #10537, #29325, #37844 ),
 .UNSPECIFIED., .F., .F.,
 ( 4, 2, 4 ),
 ( 1.509732741315237692E-16, 0.0002445252820015224966, 0.0004890505640028939638 ),
 .UNSPECIFIED. ) ;
#3182 =( BOUNDED_SURFACE ( )  B_SPLINE_SURFACE ( 3, 1, ( 
 ( #22452, #45053 ),
 ( #55020, #12150 ),
 ( #31538, #17756 ),
 ( #36883, #50630 ) ),
 .UNSPECIFIED., .F., .F., .F. ) 
 B_SPLINE_SURFACE_WITH_KNOTS ( ( 4, 4 ),
 ( 2, 2 ),
 ( 0.000000000000000000, 1.000000000000000000 ),
 ( 0.000000000000000000, 1.000000000000000000 ),
 .UNSPECIFIED. ) 
 GEOMETRIC_REPRESENTATION_ITEM ( )  RATIONAL_B_SPLINE_SURFACE ( (
 ( 1.000000000000000000, 1.000000000000000000),
 ( 0.7269869731126821222, 0.9931720237060910339),
 ( 0.7269869731126821222, 0.9931720237060910339),
 ( 1.000000000000000000, 1.000000000000000000) ) ) 
 REPRESENTATION_ITEM ( '' )  SURFACE ( )  );
#3183 = ORIENTED_EDGE ( 'NONE', *, *, #59745, .F. ) ;
#3184 = CARTESIAN_POINT ( 'NONE',  ( 0.5806925824938499181, -25.69265091980040339, 39.23149310256803801 ) ) ;
#3185 = CARTESIAN_POINT ( 'NONE',  ( 2.533389852662419894, 13.70698264761542617, -41.82785146803010434 ) ) ;
#3186 = ORIENTED_EDGE ( 'NONE', *, *, #53361, .T. ) ;
#3187 = CARTESIAN_POINT ( 'NONE',  ( 2.526464513654344657, -29.52129845577954370, 31.23609615087167057 ) ) ;
#3188 = CARTESIAN_POINT ( 'NONE',  ( -6.016104459813371719, -18.19977249352313819, 4.882138007282685876 ) ) ;
#3189 = CARTESIAN_POINT ( 'NONE',  ( 1.112077966505211846, 8.782297753024950637, -43.19608282362842999 ) ) ;
#3190 = CARTESIAN_POINT ( 'NONE',  ( 10.00000000000000533, 8.397924308530857731E-13, -80.00000000000001421 ) ) ;
#3191 = ORIENTED_EDGE ( 'NONE', *, *, #56927, .F. ) ;
#3192 = ORIENTED_EDGE ( 'NONE', *, *, #57942, .T. ) ;
#3193 = DIRECTION ( 'NONE',  ( 0.000000000000000000, 0.000000000000000000, 1.000000000000000000 ) ) ;
#3194 = CARTESIAN_POINT ( 'NONE',  ( 5.896782393890504181, -20.11283288166117345, 0.006352352428115353410 ) ) ;
#3195 = CARTESIAN_POINT ( 'NONE',  ( 0.9757402383260953549, -16.49876987395755279, 39.60970160107527960 ) ) ;
#3196 = EDGE_CURVE ( 'NONE', #29061, #26516, #61143, .T. ) ;
#3197 = CARTESIAN_POINT ( 'NONE',  ( 0.6031357023905875581, 6.322524267548581989, -47.69018446756502527 ) ) ;
#3198 = CIRCLE ( 'NONE', #15257, 5.000000000000000000 ) ;
#3199 =( BOUNDED_SURFACE ( )  B_SPLINE_SURFACE ( 3, 1, ( 
 ( #20944, #2117 ),
 ( #49440, #40088 ),
 ( #11879, #7121 ),
 ( #34438, #53507 ) ),
 .UNSPECIFIED., .F., .F., .F. ) 
 B_SPLINE_SURFACE_WITH_KNOTS ( ( 4, 4 ),
 ( 2, 2 ),
 ( 0.000000000000000000, 1.000000000000000000 ),
 ( 0.000000000000000000, 1.000000000000000000 ),
 .UNSPECIFIED. ) 
 GEOMETRIC_REPRESENTATION_ITEM ( )  RATIONAL_B_SPLINE_SURFACE ( (
 ( 1.000000000000000000, 1.000000000000000000),
 ( 0.7211978278499968642, 0.9934217856018975334),
 ( 0.7211978278499968642, 0.9934217856018975334),
 ( 1.000000000000000000, 1.000000000000000000) ) ) 
 REPRESENTATION_ITEM ( '' )  SURFACE ( )  );
#3200 = CARTESIAN_POINT ( 'NONE',  ( 2.881901169982995725, 1.330622528702777754E-16, 49.00591519830862808 ) ) ;
#3201 = DIRECTION ( 'NONE',  ( -1.000000000000000000, -0.000000000000000000, -0.000000000000000000 ) ) ;
#3202 = CARTESIAN_POINT ( 'NONE',  ( 1.231276596079887264, 10.53918392497828727, 40.57341954055075917 ) ) ;
#3203 = CARTESIAN_POINT ( 'NONE',  ( 0.9762797500689124330, -34.83496347773922963, -23.29914386174477059 ) ) ;
#3204 = CARTESIAN_POINT ( 'NONE',  ( 0.9787464366903563251, 32.77986221879337592, 26.11158030084323300 ) ) ;
#3205 = CARTESIAN_POINT ( 'NONE',  ( 4.956445790444041322, 46.03642002599030292, -9.908889005849065512 ) ) ;
#3206 = LINE ( 'NONE', #17330, #12493 ) ;
#3207 = CARTESIAN_POINT ( 'NONE',  ( -6.015611763856276717, 14.94556629257425584, 11.47596948473816170 ) ) ;
#3208 = CARTESIAN_POINT ( 'NONE',  ( 0.6009452777970410997, -6.711700115493219876, -47.63713033690751786 ) ) ;
#3209 = CARTESIAN_POINT ( 'NONE',  ( 0.8751705887134553219, 46.67919521768871505, 11.58504748649215976 ) ) ;
#3210 = EDGE_CURVE ( 'NONE', #3847, #61531, #49162, .T. ) ;
#3211 = CARTESIAN_POINT ( 'NONE',  ( 0.6029443449137434907, 16.91913962848288477, 46.10078363992560924 ) ) ;
#3212 = CARTESIAN_POINT ( 'NONE',  ( 0.6021447746440204973, -47.43443576215717883, 12.70887260988444289 ) ) ;
#3214 = VERTEX_POINT ( 'NONE', #23653 ) ;
#3213 = CARTESIAN_POINT ( 'NONE',  ( 0.8551540677456834771, 38.56334384152430772, 28.44084013485131379 ) ) ;
#3215 = VERTEX_POINT ( 'NONE', #19275 ) ;
#3216 = CARTESIAN_POINT ( 'NONE',  ( 0.6024113833632039894, 17.16413907095168057, -46.01015321702263350 ) ) ;
#3217 = CARTESIAN_POINT ( 'NONE',  ( 3.559346040607745287, 2.173097940776011594, -43.91705735681505018 ) ) ;
#3218 = CARTESIAN_POINT ( 'NONE',  ( 0.7948878604505659196, 44.60603605348585887, 20.51828927794751323 ) ) ;
#3219 = ORIENTED_EDGE ( 'NONE', *, *, #32047, .T. ) ;
#3220 = ORIENTED_EDGE ( 'NONE', *, *, #48384, .T. ) ;
#3221 = DIRECTION ( 'NONE',  ( -1.000000000000000000, -0.000000000000000000, -0.000000000000000000 ) ) ;
#3222 = CARTESIAN_POINT ( 'NONE',  ( 4.975801465491695552, 0.000000000000000000, 0.000000000000000000 ) ) ;
#3223 = EDGE_CURVE ( 'NONE', #21472, #22913, #3541, .T. ) ;
#3224 = ORIENTED_EDGE ( 'NONE', *, *, #17264, .F. ) ;
#3225 = ORIENTED_EDGE ( 'NONE', *, *, #17656, .T. ) ;
#3226 = CARTESIAN_POINT ( 'NONE',  ( 0.9762797500689124330, 19.69530149098714489, -36.99215976885945167 ) ) ;
#3227 = ADVANCED_FACE ( 'NONE', ( #37786 ), #44129, .F. ) ;
#3228 = CARTESIAN_POINT ( 'NONE',  ( 0.6001305935487315502, -33.64689939321966250, 34.38748867424654776 ) ) ;
#3229 = CARTESIAN_POINT ( 'NONE',  ( 0.6253024248130498730, 48.95676787329645663, 3.831332251033968017 ) ) ;
#3230 = ORIENTED_EDGE ( 'NONE', *, *, #24745, .F. ) ;
#3231 = FACE_OUTER_BOUND ( 'NONE', #60539, .T. ) ;
#3232 = PRESENTATION_LAYER_ASSIGNMENT (  '', '', ( #54242 ) ) ;
#3233 = CARTESIAN_POINT ( 'NONE',  ( 1.231276596079887264, 3.353048872156665805, -41.78556968953512296 ) ) ;
#3234 = CIRCLE ( 'NONE', #1225, 48.91267123290010943 ) ;
#3235 = CARTESIAN_POINT ( 'NONE',  ( 4.999999999999997335, 0.000000000000000000, 4.250000000000000000 ) ) ;
#3236 = ORIENTED_EDGE ( 'NONE', *, *, #37708, .T. ) ;
#3237 = EDGE_CURVE ( 'NONE', #48540, #19953, #18978, .T. ) ;
#3238 = ORIENTED_EDGE ( 'NONE', *, *, #53930, .F. ) ;
#3239 = CARTESIAN_POINT ( 'NONE',  ( -6.078075953587585900, 0.6224930363970364589, -19.24597819459362569 ) ) ;
#3240 = ORIENTED_EDGE ( 'NONE', *, *, #24431, .T. ) ;
#3241 = CARTESIAN_POINT ( 'NONE',  ( 0.8554163680231708922, -35.40260165760500399, 30.78735566729890749 ) ) ;
#3242 = CARTESIAN_POINT ( 'NONE',  ( -6.015611763856276717, -0.006214430185009750529, -18.84324252354755203 ) ) ;
#3243 = CARTESIAN_POINT ( 'NONE',  ( 0.8560838555295158248, -20.57050347530512724, 42.15717282805135113 ) ) ;
#3244 = CARTESIAN_POINT ( 'NONE',  ( 4.975610109902397937, -4.123593823332411645, 48.73854102369035957 ) ) ;
#3245 = CARTESIAN_POINT ( 'NONE',  ( 2.009741617377216460, -43.83235551399246077, -4.269506730058997945 ) ) ;
#3246 = EDGE_CURVE ( 'NONE', #50327, #2552, #10342, .T. ) ;
#3247 = ORIENTED_EDGE ( 'NONE', *, *, #59161, .T. ) ;
#3248 = CARTESIAN_POINT ( 'NONE',  ( 4.962356264823608143, 41.15374796524913847, 8.809348799718396350 ) ) ;
#3249 = CARTESIAN_POINT ( 'NONE',  ( 0.8753041380234471980, -47.71532843791173661, 11.59248721953970218 ) ) ;
#3250 = EDGE_CURVE ( 'NONE', #45810, #22775, #10917, .T. ) ;
#3251 = CARTESIAN_POINT ( 'NONE',  ( -6.063463321072276813, 3.057971819381750223, -19.01234495877183761 ) ) ;
#3252 = ORIENTED_EDGE ( 'NONE', *, *, #29798, .T. ) ;
#3253 = CARTESIAN_POINT ( 'NONE',  ( 7.999999999999986677, 56.56854249492371878, 56.56854249492391062 ) ) ;
#3254 = CARTESIAN_POINT ( 'NONE',  ( -6.001507490154111224, 13.31361390284159896, 13.33564355450112870 ) ) ;
#3255 = ORIENTED_EDGE ( 'NONE', *, *, #52298, .F. ) ;
#3256 = CARTESIAN_POINT ( 'NONE',  ( 0.9754292589017228288, -12.97161685674443454, -39.85052851615772340 ) ) ;
#3257 = CARTESIAN_POINT ( 'NONE',  ( 4.963659409799330291, 42.22332985082310586, 14.83726297270295014 ) ) ;
#3258 = CARTESIAN_POINT ( 'NONE',  ( 0.5980271706414711508, -2.273683837878000435, 49.05995928093535241 ) ) ;
#3259 = EDGE_CURVE ( 'NONE', #2365, #7116, #57347, .T. ) ;
#3260 = PRODUCT ( 'straight bevel gear(wobble in)_iso_ISO - Straight bevel gear 2M 49GT 48PT 20PA 5FW ---49O1H50MD20.0S1', 'straight bevel gear(wobble in)_iso_ISO - Straight bevel gear 2M 49GT 48PT 20PA 5FW ---49O1H50MD20.0S1', '', ( #2358 ) ) ;
#3261 = CARTESIAN_POINT ( 'NONE',  ( 2.282803330402972009, 33.58715474468253603, -32.83900034431218984 ) ) ;
#3262 = CARTESIAN_POINT ( 'NONE',  ( 0.9758171775293923433, 42.90848549292462621, -0.005919131625146459991 ) ) ;
#3263 = CARTESIAN_POINT ( 'NONE',  ( 4.967162193818130511, 0.000000000000000000, 0.000000000000000000 ) ) ;
#3264 = CARTESIAN_POINT ( 'NONE',  ( -5.439999999999997726, -15.43999999999999062, 1.890854657883512912E-15 ) ) ;
#3265 = CARTESIAN_POINT ( 'NONE',  ( 0.6008122571543326185, 40.91731943791382520, -27.15377543696339302 ) ) ;
#3266 =( BOUNDED_SURFACE ( )  B_SPLINE_SURFACE ( 3, 1, ( 
 ( #52368, #60849 ),
 ( #12968, #18895 ),
 ( #9160, #32064 ),
 ( #61152, #28570 ) ),
 .UNSPECIFIED., .F., .F., .F. ) 
 B_SPLINE_SURFACE_WITH_KNOTS ( ( 4, 4 ),
 ( 2, 2 ),
 ( 0.000000000000000000, 1.000000000000000000 ),
 ( 0.000000000000000000, 1.000000000000000000 ),
 .UNSPECIFIED. ) 
 GEOMETRIC_REPRESENTATION_ITEM ( )  RATIONAL_B_SPLINE_SURFACE ( (
 ( 1.000000000000000000, 1.000000000000000000),
 ( 0.9952954269826590483, 0.8620686068821339365),
 ( 0.9952954269826590483, 0.8620686068821339365),
 ( 1.000000000000000000, 1.000000000000000000) ) ) 
 REPRESENTATION_ITEM ( '' )  SURFACE ( )  );
#3267 = CARTESIAN_POINT ( 'NONE',  ( 0.5782707292762442330, 10.16715070324103287, 45.78608304152260189 ) ) ;
#3268 = ORIENTED_EDGE ( 'NONE', *, *, #25474, .T. ) ;
#3269 = CARTESIAN_POINT ( 'NONE',  ( 4.549368137175248350, 0.000000000000000000, 0.000000000000000000 ) ) ;
#3270 = CARTESIAN_POINT ( 'NONE',  ( 5.880360259849752858, 47.86623372148045519, 3.184717612778101614 ) ) ;
#3271 = CARTESIAN_POINT ( 'NONE',  ( 0.7954196712028483995, -33.39101545667313076, -34.61997730204570445 ) ) ;
#3272 = CARTESIAN_POINT ( 'NONE',  ( 0.5837157313716024865, -34.71940262318195636, -31.52459587483094694 ) ) ;
#3273 = CARTESIAN_POINT ( 'NONE',  ( 4.960386119450149955, 23.93873278148768691, -36.62476672265461985 ) ) ;
#3274 = AXIS2_PLACEMENT_3D ( 'NONE', #25580, #20889, #2062 ) ;
#3275 = CARTESIAN_POINT ( 'NONE',  ( 5.960221823109900008, 20.34928172836730553, -2.684531185214208193 ) ) ;
#3276 = PRODUCT_CONTEXT ( 'NONE', #17150, 'mechanical' ) ;
#3277 = CARTESIAN_POINT ( 'NONE',  ( 5.895596859100789899, 17.94951300836817865, -9.074313526372616678 ) ) ;
#3278 = CARTESIAN_POINT ( 'NONE',  ( 1.657374760986086493, 36.23257293270000190, -25.06174586753322231 ) ) ;
#3279 = CARTESIAN_POINT ( 'NONE',  ( 4.062725214796417461, -12.40828859588279798, -1.199999999999999956 ) ) ;
#3280 = EDGE_CURVE ( 'NONE', #5776, #33892, #7309, .T. ) ;
#3281 =( BOUNDED_SURFACE ( )  B_SPLINE_SURFACE ( 3, 1, ( 
 ( #51256, #8341 ),
 ( #20540, #805 ),
 ( #52805, #44671 ),
 ( #15846, #59038 ) ),
 .UNSPECIFIED., .F., .F., .F. ) 
 B_SPLINE_SURFACE_WITH_KNOTS ( ( 4, 4 ),
 ( 2, 2 ),
 ( 0.000000000000000000, 1.000000000000000000 ),
 ( 0.000000000000000000, 1.000000000000000000 ),
 .UNSPECIFIED. ) 
 GEOMETRIC_REPRESENTATION_ITEM ( )  RATIONAL_B_SPLINE_SURFACE ( (
 ( 1.000000000000000000, 1.000000000000000000),
 ( 0.7269869731126821222, 0.9931720237060910339),
 ( 0.7269869731126821222, 0.9931720237060910339),
 ( 1.000000000000000000, 1.000000000000000000) ) ) 
 REPRESENTATION_ITEM ( '' )  SURFACE ( )  );
#3283 = EDGE_LOOP ( 'NONE', ( #44355, #40516, #7947, #16615 ) ) ;
#3282 = CARTESIAN_POINT ( 'NONE',  ( 5.965394784446458765, -5.326334832595513546, -19.82223131420052198 ) ) ;
#3284 = VERTEX_POINT ( 'NONE', #47777 ) ;
#3285 = CARTESIAN_POINT ( 'NONE',  ( 4.322998006666165516, 46.85697641700708260, -10.36018990813264296 ) ) ;
#3286 = LINE ( 'NONE', #55602, #55514 ) ;
#3287 = CARTESIAN_POINT ( 'NONE',  ( 4.967162193818130511, 40.93989340068610261, 13.42934394584178648 ) ) ;
#3288 = EDGE_CURVE ( 'NONE', #18299, #23600, #46548, .T. ) ;
#3289 =( BOUNDED_SURFACE ( )  B_SPLINE_SURFACE ( 3, 1, ( 
 ( #33651, #27390 ),
 ( #52729, #3566 ),
 ( #47744, #4480 ),
 ( #14243, #56505 ) ),
 .UNSPECIFIED., .F., .F., .F. ) 
 B_SPLINE_SURFACE_WITH_KNOTS ( ( 4, 4 ),
 ( 2, 2 ),
 ( 0.000000000000000000, 1.000000000000000000 ),
 ( 0.000000000000000000, 1.000000000000000000 ),
 .UNSPECIFIED. ) 
 GEOMETRIC_REPRESENTATION_ITEM ( )  RATIONAL_B_SPLINE_SURFACE ( (
 ( 1.000000000000000000, 1.000000000000000000),
 ( 0.7282232189291694135, 0.9929344683865672927),
 ( 0.7282232189291694135, 0.9929344683865672927),
 ( 1.000000000000000000, 1.000000000000000000) ) ) 
 REPRESENTATION_ITEM ( '' )  SURFACE ( )  );
#3290 = ORIENTED_EDGE ( 'NONE', *, *, #20257, .F. ) ;
#3291 = CARTESIAN_POINT ( 'NONE',  ( 4.956445790443988031, 0.000000000000000000, -47.09074272231896430 ) ) ;
#3293 = CARTESIAN_POINT ( 'NONE',  ( 0.8557997880470697982, -23.15977007032352475, 41.93815086860250574 ) ) ;
#3292 = CIRCLE ( 'NONE', #37361, 47.09074272231896430 ) ;
#3294 = CARTESIAN_POINT ( 'NONE',  ( 0.8751705887134423323, -29.98056538504989277, 37.60752970653777538 ) ) ;
#3295 = EDGE_CURVE ( 'NONE', #42216, #55695, #21541, .T. ) ;
#3296 = ORIENTED_EDGE ( 'NONE', *, *, #45161, .T. ) ;
#3297 = EDGE_LOOP ( 'NONE', ( #57767, #51722, #50105, #38799 ) ) ;
#3298 = CARTESIAN_POINT ( 'NONE',  ( 0.9780106845699481077, 25.11113889175388181, -33.55237622009033771 ) ) ;
#3299 = EDGE_CURVE ( 'NONE', #5770, #31240, #24264, .T. ) ;
#3300 = CARTESIAN_POINT ( 'NONE',  ( 3.050102900204245682, 37.82667193297250208, 22.46259423248638498 ) ) ;
#3301 = CARTESIAN_POINT ( 'NONE',  ( 0.6017666602106489515, 41.83584962818284225, 23.75081624637636679 ) ) ;
#3302 = VERTEX_POINT ( 'NONE', #53668 ) ;
#3303 = CARTESIAN_POINT ( 'NONE',  ( 1.555462896905692949, -0.4926004118482715799, -49.06288753989547757 ) ) ;
#3304 = CARTESIAN_POINT ( 'NONE',  ( 42.00000000000000711, 7.715020029081011437E-15, -8.088905766426392334E-31 ) ) ;
#3305 = CARTESIAN_POINT ( 'NONE',  ( -6.078726893082806448, 5.475592473157355755, 18.46109228449450512 ) ) ;
#3306 = CARTESIAN_POINT ( 'NONE',  ( 0.1157991065609915715, 33.54534060093158132, 28.66448132280070382 ) ) ;
#3307 = ORIENTED_EDGE ( 'NONE', *, *, #22758, .T. ) ;
#3308 = EDGE_CURVE ( 'NONE', #26439, #49329, #55142, .T. ) ;
#3309 = CARTESIAN_POINT ( 'NONE',  ( 3.238741278300274029, 41.96285461600081135, -9.350673766180365831 ) ) ;
#3310 = SURFACE_SIDE_STYLE ('',( #41263 ) ) ;
#3311 = ORIENTED_EDGE ( 'NONE', *, *, #4533, .T. ) ;
#3312 = CARTESIAN_POINT ( 'NONE',  ( 4.975610109902397937, -48.11736577406850301, -8.784561349451310619 ) ) ;
#3313 = EDGE_CURVE ( 'NONE', #37210, #47783, #43198, .T. ) ;
#3314 = FACE_OUTER_BOUND ( 'NONE', #35504, .T. ) ;
#3315 = CARTESIAN_POINT ( 'NONE',  ( 0.9790850452238870627, 4.144492514655467197, -41.70324342373339022 ) ) ;
#3316 = SURFACE_STYLE_FILL_AREA ( #40051 ) ;
#3317 = AXIS2_PLACEMENT_3D ( 'NONE', #53422, #40301, #59354 ) ;
#3318 = ORIENTED_EDGE ( 'NONE', *, *, #41261, .T. ) ;
#3319 = ORIENTED_EDGE ( 'NONE', *, *, #397, .F. ) ;
#3320 = DIRECTION ( 'NONE',  ( 1.000000000000000000, 0.000000000000000000, 0.000000000000000000 ) ) ;
#3321 = CARTESIAN_POINT ( 'NONE',  ( 0.5806925824938502512, 45.37089516811273882, 11.86188155343358197 ) ) ;
#3322 = ORIENTED_EDGE ( 'NONE', *, *, #3588, .F. ) ;
#3323 = EDGE_CURVE ( 'NONE', #19581, #36353, #53070, .T. ) ;
#3324 = CARTESIAN_POINT ( 'NONE',  ( -6.016761891674565099, -2.456125503350587991, -18.68243340030205246 ) ) ;
#3325 = VERTEX_POINT ( 'NONE', #34601 ) ;
#3326 = DIRECTION ( 'NONE',  ( -0.000000000000000000, -0.000000000000000000, 1.000000000000000000 ) ) ;
#3327 = ORIENTED_EDGE ( 'NONE', *, *, #13810, .F. ) ;
#3328 = CARTESIAN_POINT ( 'NONE',  ( 4.226256110419178924, 43.52565652391797357, 6.028637835291145386 ) ) ;
#3329 = CARTESIAN_POINT ( 'NONE',  ( 0.6026777506516368677, -48.72629457415274601, -6.106931120465691087 ) ) ;
#3330 = CARTESIAN_POINT ( 'NONE',  ( 4.975610109902397937, -48.77192499014914517, 3.707929326866768349 ) ) ;
#3331 = ORIENTED_EDGE ( 'NONE', *, *, #45884, .T. ) ;
#3332 = CARTESIAN_POINT ( 'NONE',  ( 5.917102823773431552, 14.92182362673000284, -13.48439459910989946 ) ) ;
#3333 = CARTESIAN_POINT ( 'NONE',  ( 0.9722240741986376555, -11.66659279944005334, 41.29187377038497431 ) ) ;
#3334 = CARTESIAN_POINT ( 'NONE',  ( 0.9762797500689124330, 29.49606728235556830, -29.77090526101713763 ) ) ;
#3335 = EDGE_CURVE ( 'NONE', #44156, #21453, #16910, .T. ) ;
#3336 =( GEOMETRIC_REPRESENTATION_CONTEXT ( 3 ) GLOBAL_UNCERTAINTY_ASSIGNED_CONTEXT ( ( #22977 ) ) GLOBAL_UNIT_ASSIGNED_CONTEXT ( ( #55629, #50939, #7716 ) ) REPRESENTATION_CONTEXT ( 'NONE', 'WORKASPACE' ) );
#3337 = VERTEX_POINT ( 'NONE', #19900 ) ;
#3338 = CARTESIAN_POINT ( 'NONE',  ( 0.7245667037590732829, -37.65687897229943104, 29.92941129926883903 ) ) ;
#3339 = CARTESIAN_POINT ( 'NONE',  ( -6.015611763856276717, 17.40650793417854203, -7.216738110653091454 ) ) ;
#3340 = EDGE_CURVE ( 'NONE', #51387, #23810, #46188, .T. ) ;
#3341 = CARTESIAN_POINT ( 'NONE',  ( 0.3676999524040323597, 29.04098611012938136, 33.20499524279608750 ) ) ;
#3342 = CARTESIAN_POINT ( 'NONE',  ( 4.956445790444029775, 25.79263028817611314, -39.39896284113449809 ) ) ;
#3343 = ORIENTED_EDGE ( 'NONE', *, *, #40535, .T. ) ;
#3344 = CARTESIAN_POINT ( 'NONE',  ( 5.974727161628369032, -2.663664384318642497, -20.35137732084675122 ) ) ;
#3345 = FACE_OUTER_BOUND ( 'NONE', #44724, .T. ) ;
#3346 = VERTEX_POINT ( 'NONE', #33997 ) ;
#3347 = CARTESIAN_POINT ( 'NONE',  ( 0.9757892942422827787, -30.30456399643813370, 30.37715353261981122 ) ) ;
#3348 = CARTESIAN_POINT ( 'NONE',  ( 4.956653778116990594, -39.67974989265022145, -27.17045123668512474 ) ) ;
#3349 = CARTESIAN_POINT ( 'NONE',  ( 5.896278296736517710, -2.018661446113561908, -20.01129644926481532 ) ) ;
#3350 = CARTESIAN_POINT ( 'NONE',  ( 0.9757787079277443487, 5.639827755377256224, -42.53619983261571491 ) ) ;
#3351 = CARTESIAN_POINT ( 'NONE',  ( 4.975801465491694664, -35.64402118370934147, -32.01766832630300286 ) ) ;
#3352 = CARTESIAN_POINT ( 'NONE',  ( 2.648799415243708655, -24.22471848649547610, 42.63426412569639012 ) ) ;
#3353 = CARTESIAN_POINT ( 'NONE',  ( 0.6021448801613057400, 4.455338032995132203, 48.90491899225163763 ) ) ;
#3354 = CARTESIAN_POINT ( 'NONE',  ( 1.154321485836933725, -42.64911658695771735, -4.782433484301630955 ) ) ;
#3355 = CARTESIAN_POINT ( 'NONE',  ( 5.959547316686252039, 14.51128755440521267, 14.51632612601533801 ) ) ;
#3356 = CARTESIAN_POINT ( 'NONE',  ( 0.5997462898726536595, -39.04071682475767346, -29.78882441375276358 ) ) ;
#3357 = CARTESIAN_POINT ( 'NONE',  ( 1.231276596079881935, 10.53918392497884149, -40.57341954055061706 ) ) ;
#3358 = CARTESIAN_POINT ( 'NONE',  ( 4.975610109902397937, 0.000000000000000000, 0.000000000000000000 ) ) ;
#3359 = CARTESIAN_POINT ( 'NONE',  ( 0.8751705887134553219, -46.67919521768879321, -11.58504748649183647 ) ) ;
#3360 = CARTESIAN_POINT ( 'NONE',  ( 4.549368137175248350, -42.14271863032838894, 8.166781970325002860 ) ) ;
#3361 = CARTESIAN_POINT ( 'NONE',  ( 1.479689385636123067, 16.31572803950663442, 40.93141658687796536 ) ) ;
#3362 = ADVANCED_FACE ( 'NONE', ( #1358 ), #24885, .F. ) ;
#3363 = CONICAL_SURFACE ( 'NONE', #8378, 43.92652462719577500, 1.486293639869522343 ) ;
#3364 = CARTESIAN_POINT ( 'NONE',  ( 0.6253024248130478746, 40.77684555828908231, 27.36225673684618798 ) ) ;
#3365 = CARTESIAN_POINT ( 'NONE',  ( 0.5817217712918324457, 46.41469452300511023, 6.701573423047251232 ) ) ;
#3366 = CARTESIAN_POINT ( 'NONE',  ( 0.7245667037590747261, -42.06183421678311163, -23.33692989609096813 ) ) ;
#3367 = EDGE_CURVE ( 'NONE', #49832, #38633, #26752, .T. ) ;
#3368 =( BOUNDED_SURFACE ( )  B_SPLINE_SURFACE ( 3, 1, ( 
 ( #23535, #22619 ),
 ( #3486, #8194 ),
 ( #27313, #42661 ),
 ( #19170, #17932 ) ),
 .UNSPECIFIED., .F., .F., .F. ) 
 B_SPLINE_SURFACE_WITH_KNOTS ( ( 4, 4 ),
 ( 2, 2 ),
 ( 0.000000000000000000, 1.000000000000000000 ),
 ( 0.000000000000000000, 1.000000000000000000 ),
 .UNSPECIFIED. ) 
 GEOMETRIC_REPRESENTATION_ITEM ( )  RATIONAL_B_SPLINE_SURFACE ( (
 ( 1.000000000000000000, 1.000000000000000000),
 ( 0.9751682680413298332, 0.9999560080971552356),
 ( 0.9751682680413298332, 0.9999560080971552356),
 ( 1.000000000000000000, 1.000000000000000000) ) ) 
 REPRESENTATION_ITEM ( '' )  SURFACE ( )  );
#3369 = VERTEX_POINT ( 'NONE', #5443 ) ;
#3370 = CARTESIAN_POINT ( 'NONE',  ( 5.860006189529246790, -45.66786516969918353, -15.52021937683323927 ) ) ;
#3371 = EDGE_CURVE ( 'NONE', #37569, #18665, #37997, .T. ) ;
#3372 = EDGE_CURVE ( 'NONE', #44297, #47052, #32916, .T. ) ;
#3373 = CARTESIAN_POINT ( 'NONE',  ( 2.643462169533600914, -47.42536612906423699, -7.637863311827439716 ) ) ;
#3374 = CARTESIAN_POINT ( 'NONE',  ( 4.060580049360325461, 27.79286080241194057, -34.04445010243171055 ) ) ;
#3375 = DIRECTION ( 'NONE',  ( -1.850371707708593823E-16, 1.000000000000000000, 0.000000000000000000 ) ) ;
#3376 = EDGE_CURVE ( 'NONE', #11571, #4545, #2603, .T. ) ;
#3377 = EDGE_LOOP ( 'NONE', ( #255, #7217 ) ) ;
#3378 = CARTESIAN_POINT ( 'NONE',  ( 4.962356264823601926, -42.08379584346671720, 0.4355746408606013254 ) ) ;
#3379 = VECTOR ( 'NONE', #26608, 1000.000000000000000 ) ;
#3380 = CARTESIAN_POINT ( 'NONE',  ( 5.838029081930957709, -37.08173278831614539, -29.25765116288114243 ) ) ;
#3381 = ORIENTED_EDGE ( 'NONE', *, *, #9977, .T. ) ;
#3382 = EDGE_CURVE ( 'NONE', #3122, #23289, #61474, .T. ) ;
#3383 = DIRECTION ( 'NONE',  ( 0.1736481776669314969, -0.9848077530122079093, -4.496403249731880833E-15 ) ) ;
#3384 = EDGE_LOOP ( 'NONE', ( #1943, #39526, #52066, #17337 ) ) ;
#3385 = CARTESIAN_POINT ( 'NONE',  ( 0.5809828226811553087, -0.5448590168529036104, -47.89273459658654275 ) ) ;
#3386 = CARTESIAN_POINT ( 'NONE',  ( -6.015611763856276717, 18.19956619163658118, 4.882992715191364574 ) ) ;
#3387 = VERTEX_POINT ( 'NONE', #31748 ) ;
#3388 = CARTESIAN_POINT ( 'NONE',  ( 4.553261556744875094, -9.554252317234240621, -42.87488575474295516 ) ) ;
#3389 = CARTESIAN_POINT ( 'NONE',  ( 0.5839879327111905383, -29.08515285004915540, 38.05372318152046063 ) ) ;
#3390 = ORIENTED_EDGE ( 'NONE', *, *, #39633, .F. ) ;
#3391 = CARTESIAN_POINT ( 'NONE',  ( 4.975610109902397937, -16.35148546628888866, -46.09857188876371481 ) ) ;
#3392 = CARTESIAN_POINT ( 'NONE',  ( 0.1310142868023676521, -15.91230901232197326, -40.08041389954875200 ) ) ;
#3393 = ORIENTED_EDGE ( 'NONE', *, *, #40427, .T. ) ;
#3394 = CARTESIAN_POINT ( 'NONE',  ( 2.301529144917016101, -42.22700141647025873, -22.89307126379972601 ) ) ;
#3395 = VERTEX_POINT ( 'NONE', #49601 ) ;
#3396 = DIRECTION ( 'NONE',  ( 1.000000000000000000, 0.000000000000000000, 0.000000000000000000 ) ) ;
#3397 = ORIENTED_EDGE ( 'NONE', *, *, #10985, .F. ) ;
#3398 = ORIENTED_EDGE ( 'NONE', *, *, #11696, .T. ) ;
#3399 = DIRECTION ( 'NONE',  ( 1.000000000000000000, 0.000000000000000000, 0.000000000000000000 ) ) ;
#3400 = CARTESIAN_POINT ( 'NONE',  ( 4.833616638992208614, 45.27110352095247947, -9.466882727841657186 ) ) ;
#3401 = CARTESIAN_POINT ( 'NONE',  ( 0.6026777506516367566, -25.60575673810485497, -41.90336039634789955 ) ) ;
#3402 = CARTESIAN_POINT ( 'NONE',  ( 0.5807400328401574052, 46.40483864045145168, 11.87003418057259907 ) ) ;
#3403 = CARTESIAN_POINT ( 'NONE',  ( 0.8760168074886965917, 41.20610493656875661, 24.81951362746092826 ) ) ;
#3404 = ORIENTED_EDGE ( 'NONE', *, *, #867, .F. ) ;
#3405 = CARTESIAN_POINT ( 'NONE',  ( 1.157643937452367933, -39.31880107603836905, 14.52701471527025845 ) ) ;
#3406 = CARTESIAN_POINT ( 'NONE',  ( 5.981074661064941900, 19.82308078259091033, -5.320466518160730907 ) ) ;
#3407 = CARTESIAN_POINT ( 'NONE',  ( 4.226256110419178924, 0.9953287626735226601, 43.92990519727287335 ) ) ;
#3409 = ORIENTED_EDGE ( 'NONE', *, *, #18116, .F. ) ;
#3408 = ADVANCED_FACE ( 'NONE', ( #35844, #26731, #45253, #16411, #44942, #55220, #12654, #54282, #1983, #21108 ), #11405, .T. ) ;
#3410 = TOROIDAL_SURFACE ( 'NONE', #17429, 4.000000000000000000, 0.2500000000000000000 ) ;
#3411 = ORIENTED_EDGE ( 'NONE', *, *, #13810, .T. ) ;
#3412 = FACE_OUTER_BOUND ( 'NONE', #34524, .T. ) ;
#3414 = EDGE_CURVE ( 'NONE', #57834, #51445, #50839, .T. ) ;
#3413 = CARTESIAN_POINT ( 'NONE',  ( 3.678748215320120085, 6.540036259557823861, 48.53700382206501729 ) ) ;
#3415 = CARTESIAN_POINT ( 'NONE',  ( -31.75000000000000000, -15.43999999999999240, 1.890854657883512518E-15 ) ) ;
#3416 = ORIENTED_EDGE ( 'NONE', *, *, #9264, .T. ) ;
#3417 = CARTESIAN_POINT ( 'NONE',  ( 0.1087620492084206275, -42.70684898916392314, -5.987629195157659900 ) ) ;
#3418 = B_SPLINE_CURVE_WITH_KNOTS ( 'NONE', 3,
 ( #2126, #44783, #25035, #53819 ),
 .UNSPECIFIED., .F., .F.,
 ( 4, 4 ),
 ( 2.380737581620991176E-07, 0.002336974151641539946 ),
 .UNSPECIFIED. ) ;
#3420 = AXIS2_PLACEMENT_3D ( 'NONE', #43752, #41976, #38424 ) ;
#3419 = CARTESIAN_POINT ( 'NONE',  ( 4.553261556744875094, -33.59363643963393997, 28.30206982864213217 ) ) ;
#3421 = ORIENTED_EDGE ( 'NONE', *, *, #14387, .F. ) ;
#3422 = CARTESIAN_POINT ( 'NONE',  ( 4.956653778116949738, 45.71126949320249366, 14.93973939759898606 ) ) ;
#3423 = DIRECTION ( 'NONE',  ( 0.000000000000000000, 0.000000000000000000, 1.000000000000000000 ) ) ;
#3424 = CARTESIAN_POINT ( 'NONE',  ( 0.9730545539215883499, -33.73144377768576874, 26.52009130076758225 ) ) ;
#3425 = CONICAL_SURFACE ( 'NONE', #38477, 2.500000000000002220, 0.9599310885968777018 ) ;
#3426 = CARTESIAN_POINT ( 'NONE',  ( 0.5806925824938499181, -41.60618895332673617, -21.63671424046719594 ) ) ;
#3427 = CARTESIAN_POINT ( 'NONE',  ( 0.9972139404380304661, 22.02214929131140764, 36.82725283858614063 ) ) ;
#3428 = DIRECTION ( 'NONE',  ( 0.000000000000000000, 0.000000000000000000, -1.000000000000000000 ) ) ;
#3429 = EDGE_LOOP ( 'NONE', ( #43825, #41789, #34355, #35485 ) ) ;
#3430 = CARTESIAN_POINT ( 'NONE',  ( 0.1129192098497455998, 20.83764143887614040, -38.89401608281131928 ) ) ;
#3431 = CARTESIAN_POINT ( 'NONE',  ( -6.072942160501519915, -18.27069728648825730, 6.081593784077573339 ) ) ;
#3432 = CARTESIAN_POINT ( 'NONE',  ( 0.8551540677456834771, 37.45266983663536564, -29.88829867897776538 ) ) ;
#3433 = CARTESIAN_POINT ( 'NONE',  ( 1.827119703190780209, -1.232688548475726620, -43.03226500438893964 ) ) ;
#3434 = CARTESIAN_POINT ( 'NONE',  ( 0.9787464366903554369, 29.00705047156419525, 30.24772744902649890 ) ) ;
#3435 = CARTESIAN_POINT ( 'NONE',  ( 7.999999999999996447, -2.778489794828638662E-13, 80.00000000000001421 ) ) ;
#3436 = CARTESIAN_POINT ( 'NONE',  ( 4.967162193818130511, 42.34252806656594004, 7.970725651239941811 ) ) ;
#3437 = CARTESIAN_POINT ( 'NONE',  ( 0.5782707292762442330, 17.53027906811957237, -43.50201914281066706 ) ) ;
#3438 = EDGE_CURVE ( 'NONE', #57990, #5134, #33119, .T. ) ;
#3439 = ADVANCED_FACE ( 'NONE', ( #2287 ), #54493, .F. ) ;
#3440 = CARTESIAN_POINT ( 'NONE',  ( 4.975801465491695552, 0.000000000000000000, 0.000000000000000000 ) ) ;
#3441 = CARTESIAN_POINT ( 'NONE',  ( 0.5819845901640493535, -28.79568196372244060, -38.27312528999461705 ) ) ;
#3442 = ORIENTED_EDGE ( 'NONE', *, *, #8024, .T. ) ;
#3443 = EDGE_CURVE ( 'NONE', #47205, #54614, #46540, .T. ) ;
#3444 = CARTESIAN_POINT ( 'NONE',  ( 0.7056555295713298204, 47.89404551051138270, -0.8411712675129686678 ) ) ;
#3445 = CARTESIAN_POINT ( 'NONE',  ( 3.727782113643637096, 23.36895243144297396, -37.23801603419455120 ) ) ;
#3446 = CARTESIAN_POINT ( 'NONE',  ( 4.975610109902397937, 0.000000000000000000, 0.000000000000000000 ) ) ;
#3447 = CARTESIAN_POINT ( 'NONE',  ( 0.8560838555295223751, -45.77741231505103059, 10.23725333375835689 ) ) ;
#3448 = ADVANCED_FACE ( 'NONE', ( #36463 ), #59899, .F. ) ;
#3449 = ORIENTED_EDGE ( 'NONE', *, *, #16572, .T. ) ;
#3450 = CARTESIAN_POINT ( 'NONE',  ( 4.322998006666165516, -10.36018990813280816, -46.85697641700704708 ) ) ;
#3451 = CARTESIAN_POINT ( 'NONE',  ( 0.8551540677456739292, -24.74404575822804375, 41.03346287276421123 ) ) ;
#3452 = B_SPLINE_CURVE_WITH_KNOTS ( 'NONE', 3,
 ( #34260, #56580, #10135, #27776, #8978, #46591, #39278, #24227, #46910, #48646, #3635, #29538, #56266, #10447, #29232, #38662 ),
 .UNSPECIFIED., .F., .F.,
 ( 4, 3, 3, 3, 3, 4 ),
 ( 2.030557555191247372E-17, 0.0002612764279487735423, 0.0003919131003184789198, 0.0005225497727000641716, 0.0007837925190632434027, 0.001045051706266715216 ),
 .UNSPECIFIED. ) ;
#3453 =( NAMED_UNIT ( * ) SI_UNIT ( $, .STERADIAN. ) SOLID_ANGLE_UNIT ( ) );
#3454 = ORIENTED_EDGE ( 'NONE', *, *, #41368, .T. ) ;
#3455 = CARTESIAN_POINT ( 'NONE',  ( -6.078726893082806448, 19.25601281685051802, -0.003415553934477524867 ) ) ;
#3456 = CARTESIAN_POINT ( 'NONE',  ( 4.963659409799332067, -25.25989740981475506, -36.94443854030247110 ) ) ;
#3457 = CARTESIAN_POINT ( 'NONE',  ( 2.282803330402976005, 41.06968832204452013, -22.79863172620468603 ) ) ;
#3458 = EDGE_LOOP ( 'NONE', ( #18223, #12423, #55653, #51690 ) ) ;
#3459 = EDGE_CURVE ( 'NONE', #1887, #50598, #34882, .T. ) ;
#3460 = CARTESIAN_POINT ( 'NONE',  ( 0.5988103622719993524, 46.30780754281414602, 13.03604477829307129 ) ) ;
#3461 = VECTOR ( 'NONE', #126, 1000.000000000000114 ) ;
#3462 = VERTEX_POINT ( 'NONE', #9465 ) ;
#3463 = ORIENTED_EDGE ( 'NONE', *, *, #44142, .T. ) ;
#3464 = CARTESIAN_POINT ( 'NONE',  ( 0.1073791018717483448, -42.81622261970991161, -5.147744207006710759 ) ) ;
#3466 = EDGE_LOOP ( 'NONE', ( #6368, #50164, #18863, #18524 ) ) ;
#3465 = ADVANCED_FACE ( 'NONE', ( #23269 ), #31884, .F. ) ;
#3467 = CARTESIAN_POINT ( 'NONE',  ( -16.60577576646023701, 5.000000000000008882, -10.00000000000000711 ) ) ;
#3468 = CIRCLE ( 'NONE', #37544, 48.91267123290010943 ) ;
#3469 = ORIENTED_EDGE ( 'NONE', *, *, #1827, .T. ) ;
#3470 = LINE ( 'NONE', #22604, #1713 ) ;
#3471 = CARTESIAN_POINT ( 'NONE',  ( 0.9268187852002115479, -0.4216597870159004002, 44.08601292850874387 ) ) ;
#3472 = EDGE_LOOP ( 'NONE', ( #13047, #56227, #36663, #10106 ) ) ;
#3473 = DIRECTION ( 'NONE',  ( 1.000000000000000000, 0.000000000000000000, 0.000000000000000000 ) ) ;
#3474 = CARTESIAN_POINT ( 'NONE',  ( -6.057079549204054558, -14.66865672308403212, 12.47644745270303090 ) ) ;
#3475 = CARTESIAN_POINT ( 'NONE',  ( 3.727782113643637096, -37.21166825045877857, 23.41088468904526110 ) ) ;
#3476 = CARTESIAN_POINT ( 'NONE',  ( 0.5835226383429280572, -30.13809304758011010, 35.92962318201194449 ) ) ;
#3477 = VERTEX_POINT ( 'NONE', #22655 ) ;
#3478 = CARTESIAN_POINT ( 'NONE',  ( 4.691466044806102076, -29.14742760351085593, -33.74235639413318211 ) ) ;
#3479 = VERTEX_POINT ( 'NONE', #8534 ) ;
#3480 = CARTESIAN_POINT ( 'NONE',  ( 0.5806925824938499181, -30.69245420804209701, 35.45695442407318154 ) ) ;
#3481 = VERTEX_POINT ( 'NONE', #46791 ) ;
#3482 = CARTESIAN_POINT ( 'NONE',  ( 0.1073791018717578927, 37.10214135362858912, 21.98088480513677823 ) ) ;
#3483 = VECTOR ( 'NONE', #18982, 1000.000000000000000 ) ;
#3484 =( BOUNDED_SURFACE ( )  B_SPLINE_SURFACE ( 3, 1, ( 
 ( #52723, #42740 ),
 ( #19547, #38355 ),
 ( #33346, #23315 ),
 ( #56805, #43676 ) ),
 .UNSPECIFIED., .F., .F., .F. ) 
 B_SPLINE_SURFACE_WITH_KNOTS ( ( 4, 4 ),
 ( 2, 2 ),
 ( 0.000000000000000000, 1.000000000000000000 ),
 ( 0.000000000000000000, 1.000000000000000000 ),
 .UNSPECIFIED. ) 
 GEOMETRIC_REPRESENTATION_ITEM ( )  RATIONAL_B_SPLINE_SURFACE ( (
 ( 1.000000000000000000, 1.000000000000000000),
 ( 0.7282232189291694135, 0.9929344683865672927),
 ( 0.7282232189291694135, 0.9929344683865672927),
 ( 1.000000000000000000, 1.000000000000000000) ) ) 
 REPRESENTATION_ITEM ( '' )  SURFACE ( )  );
#3485 = EDGE_CURVE ( 'NONE', #44988, #9101, #7674, .T. ) ;
#3486 = CARTESIAN_POINT ( 'NONE',  ( -6.017396004339687465, 11.47192209077608815, -14.94857180791981222 ) ) ;
#3487 = VERTEX_POINT ( 'NONE', #42395 ) ;
#3488 = DIRECTION ( 'NONE',  ( 1.000000000000000000, 1.836909530733573776E-16, -1.925929944387235579E-32 ) ) ;
#3489 = CARTESIAN_POINT ( 'NONE',  ( 4.960156602257181468, -35.23783291257149841, -30.22163187094425396 ) ) ;
#3490 = CARTESIAN_POINT ( 'NONE',  ( 4.962356264823599261, -28.94323483023637777, 30.55363735178087126 ) ) ;
#3491 = CARTESIAN_POINT ( 'NONE',  ( 2.299652685299201416, -2.858710868356232560, 48.95007147113572898 ) ) ;
#3492 = ORIENTED_EDGE ( 'NONE', *, *, #34731, .T. ) ;
#3493 = EDGE_LOOP ( 'NONE', ( #60611, #18515, #45500, #1782 ) ) ;
#3494 = CARTESIAN_POINT ( 'NONE',  ( 4.975801465491694664, -8.787181743659814970, -47.10002938642139014 ) ) ;
#3495 = CARTESIAN_POINT ( 'NONE',  ( 5.960221823109900008, -16.28072933292539659, -12.49951306783083638 ) ) ;
#3496 = CARTESIAN_POINT ( 'NONE',  ( -2.601141883200665639, 14.01836437022350168, 5.126488842574115523 ) ) ;
#3497 = FACE_OUTER_BOUND ( 'NONE', #29084, .T. ) ;
#3498 = CARTESIAN_POINT ( 'NONE',  ( 4.549368137175248350, -8.166781970326043805, 42.14271863032818999 ) ) ;
#3499 = CARTESIAN_POINT ( 'NONE',  ( 5.901764892641307547, 48.57275408226684732, -6.219246602548297531 ) ) ;
#3500 = CARTESIAN_POINT ( 'NONE',  ( 3.559346040607745287, 11.77623459503632475, 42.36449669599129209 ) ) ;
#3501 = DIRECTION ( 'NONE',  ( -1.000000000000000000, -5.380183451256670742E-17, 1.298891185607911324E-16 ) ) ;
#3502 = DIRECTION ( 'NONE',  ( -1.000000000000000000, -0.000000000000000000, -0.000000000000000000 ) ) ;
#3503 = VECTOR ( 'NONE', #45114, 1000.000000000000227 ) ;
#3504 = CARTESIAN_POINT ( 'NONE',  ( 4.956445790444001354, -33.12351118015997997, 33.47194433010209025 ) ) ;
#3505 = CARTESIAN_POINT ( 'NONE',  ( 0.2885700199627516671, -15.75356883787179108, 40.13549263616297935 ) ) ;
#3506 = CARTESIAN_POINT ( 'NONE',  ( 0.3676999524040323597, 9.009680404095913531, 43.18305503711946614 ) ) ;
#3507 = AXIS2_PLACEMENT_3D ( 'NONE', #48407, #48108, #18374 ) ;
#3508 = CARTESIAN_POINT ( 'NONE',  ( 0.5997462898726536595, 16.46871699354475993, 46.26373299606117229 ) ) ;
#3509 = CARTESIAN_POINT ( 'NONE',  ( 1.227938101723756947, 26.79402671879326547, 33.52879263017872091 ) ) ;
#3510 = FACE_OUTER_BOUND ( 'NONE', #37387, .T. ) ;
#3511 = CARTESIAN_POINT ( 'NONE',  ( 0.9762797500689124330, -26.66896101499594707, 32.32787193067817810 ) ) ;
#3512 = CARTESIAN_POINT ( 'NONE',  ( 0.9736507210033060744, -36.93248879681195973, -21.84312502845830295 ) ) ;
#3513 = EDGE_CURVE ( 'NONE', #58236, #2002, #33900, .T. ) ;
#3514 = CARTESIAN_POINT ( 'NONE',  ( 0.6041374136657475802, -47.67304777898695534, -6.452348380035735076 ) ) ;
#3515 = CARTESIAN_POINT ( 'NONE',  ( 4.962356264823608143, -9.332162870646227404, -41.03835198954849517 ) ) ;
#3517 = ORIENTED_EDGE ( 'NONE', *, *, #21854, .T. ) ;
#3516 = CARTESIAN_POINT ( 'NONE',  ( 0.9756950546413946102, 39.67916378221936213, 16.33093981194336664 ) ) ;
#3518 = ORIENTED_EDGE ( 'NONE', *, *, #42055, .F. ) ;
#3519 = CARTESIAN_POINT ( 'NONE',  ( 4.956653778116992370, 21.75875759808766929, -42.88673967249108188 ) ) ;
#3520 = CARTESIAN_POINT ( 'NONE',  ( 0.5819845901640492425, 23.55368560422342483, 41.70428411658535595 ) ) ;
#3521 = CARTESIAN_POINT ( 'NONE',  ( 5.838029081930957709, 1.598329895848616067, 47.20710115752668656 ) ) ;
#3522 = ADVANCED_FACE ( 'NONE', ( #18271 ), #3266, .F. ) ;
#3523 = ORIENTED_EDGE ( 'NONE', *, *, #61931, .T. ) ;
#3524 = EDGE_LOOP ( 'NONE', ( #31887, #42957, #22308, #14831 ) ) ;
#3525 = CARTESIAN_POINT ( 'NONE',  ( 3.559346040607745287, -30.12298026119279015, 32.03180203681612426 ) ) ;
#3526 = CARTESIAN_POINT ( 'NONE',  ( 1.154321485836934169, 4.782433484301801485, -42.64911658695771024 ) ) ;
#3527 = PRODUCT_DEFINITION_CONTEXT ( 'detailed design', #54333, 'design' ) ;
#3528 = ORIENTED_EDGE ( 'NONE', *, *, #29071, .F. ) ;
#3529 = ORIENTED_EDGE ( 'NONE', *, *, #24899, .T. ) ;
#3530 = CARTESIAN_POINT ( 'NONE',  ( 5.895881250540457863, -19.39704354167978906, -5.318118412604147416 ) ) ;
#3531 = B_SPLINE_CURVE_WITH_KNOTS ( 'NONE', 3,
 ( #21320, #35127, #16945, #25704 ),
 .UNSPECIFIED., .F., .F.,
 ( 4, 4 ),
 ( 0.000000000000000000, 0.004444103432399265294 ),
 .UNSPECIFIED. ) ;
#3532 = EDGE_CURVE ( 'NONE', #44988, #34186, #60871, .T. ) ;
#3533 = CARTESIAN_POINT ( 'NONE',  ( 0.5807400328401574052, 44.04145271122565219, 18.83234461715198904 ) ) ;
#3534 = CARTESIAN_POINT ( 'NONE',  ( 0.9757402383260955769, -41.46830379850860027, 11.02350435907888482 ) ) ;
#3535 = ORIENTED_EDGE ( 'NONE', *, *, #39693, .T. ) ;
#3536 = ORIENTED_EDGE ( 'NONE', *, *, #37675, .T. ) ;
#3537 = EDGE_CURVE ( 'NONE', #34547, #42039, #44338, .T. ) ;
#3538 = DIRECTION ( 'NONE',  ( 0.000000000000000000, 0.000000000000000000, 1.000000000000000000 ) ) ;
#3539 = CARTESIAN_POINT ( 'NONE',  ( 0.8753041380234465318, -13.11588273819783623, -47.31925557181583741 ) ) ;
#3540 =( BOUNDED_SURFACE ( )  B_SPLINE_SURFACE ( 3, 1, ( 
 ( #18008, #37749 ),
 ( #3563, #27085 ),
 ( #51802, #18617 ),
 ( #56499, #4176 ) ),
 .UNSPECIFIED., .F., .F., .F. ) 
 B_SPLINE_SURFACE_WITH_KNOTS ( ( 4, 4 ),
 ( 2, 2 ),
 ( 0.000000000000000000, 1.000000000000000000 ),
 ( 0.000000000000000000, 1.000000000000000000 ),
 .UNSPECIFIED. ) 
 GEOMETRIC_REPRESENTATION_ITEM ( )  RATIONAL_B_SPLINE_SURFACE ( (
 ( 1.000000000000000000, 1.000000000000000000),
 ( 0.9729067724841187204, 0.9999501103223794596),
 ( 0.9729067724841187204, 0.9999501103223794596),
 ( 1.000000000000000000, 1.000000000000000000) ) ) 
 REPRESENTATION_ITEM ( '' )  SURFACE ( )  );
#3541 = B_SPLINE_CURVE_WITH_KNOTS ( 'NONE', 3,
 ( #61532, #4515, #32758, #27738, #42475, #18655 ),
 .UNSPECIFIED., .F., .F.,
 ( 4, 2, 4 ),
 ( 8.985151752445514084E-18, 0.0002291978881530154554, 0.0004583957763060219660 ),
 .UNSPECIFIED. ) ;
#3542 = VECTOR ( 'NONE', #6303, 1000.000000000000114 ) ;
#3543 = DIRECTION ( 'NONE',  ( 1.000000000000000000, 1.836909530733573776E-16, -1.925929944387235853E-32 ) ) ;
#3544 = ORIENTED_EDGE ( 'NONE', *, *, #15917, .F. ) ;
#3545 = ORIENTED_EDGE ( 'NONE', *, *, #292, .F. ) ;
#3546 = CIRCLE ( 'NONE', #38604, 72.00000000000002842 ) ;
#3547 = ORIENTED_EDGE ( 'NONE', *, *, #23484, .F. ) ;
#3548 = FACE_OUTER_BOUND ( 'NONE', #12124, .T. ) ;
#3549 = CARTESIAN_POINT ( 'NONE',  ( 4.549368137175248350, 23.67244292351640667, -35.80950303116076583 ) ) ;
#3550 = CARTESIAN_POINT ( 'NONE',  ( 0.6017667736363750963, 34.26315558341190837, -33.76945004754880131 ) ) ;
#3551 = CARTESIAN_POINT ( 'NONE',  ( 0.5832655196449124668, -38.79139163682725666, 26.35266813534483887 ) ) ;
#3552 = CARTESIAN_POINT ( 'NONE',  ( 0.8744876279028263033, -2.462621419133342204, 49.03351451941333750 ) ) ;
#3553 = B_SPLINE_CURVE_WITH_KNOTS ( 'NONE', 3,
 ( #37200, #13386, #37832, #43134, #37510, #24005 ),
 .UNSPECIFIED., .F., .F.,
 ( 4, 2, 4 ),
 ( 0.000000000000000000, 0.0002450742804987359109, 0.0004901485609974718218 ),
 .UNSPECIFIED. ) ;
#3554 = ORIENTED_EDGE ( 'NONE', *, *, #22993, .F. ) ;
#3555 = DIRECTION ( 'NONE',  ( 0.000000000000000000, 0.000000000000000000, 1.000000000000000000 ) ) ;
#3556 = CARTESIAN_POINT ( 'NONE',  ( -6.072942160501519915, -1.834587804586878645, 19.16868409349691049 ) ) ;
#3557 =( BOUNDED_SURFACE ( )  B_SPLINE_SURFACE ( 3, 1, ( 
 ( #41394, #61678 ),
 ( #51061, #22575 ),
 ( #8774, #8156 ),
 ( #47016, #51366 ) ),
 .UNSPECIFIED., .F., .F., .F. ) 
 B_SPLINE_SURFACE_WITH_KNOTS ( ( 4, 4 ),
 ( 2, 2 ),
 ( 0.000000000000000000, 1.000000000000000000 ),
 ( 0.000000000000000000, 1.000000000000000000 ),
 .UNSPECIFIED. ) 
 GEOMETRIC_REPRESENTATION_ITEM ( )  RATIONAL_B_SPLINE_SURFACE ( (
 ( 1.000000000000000000, 1.000000000000000000),
 ( 0.9953390228620291325, 0.8624445117760984880),
 ( 0.9953390228620291325, 0.8624445117760984880),
 ( 1.000000000000000000, 1.000000000000000000) ) ) 
 REPRESENTATION_ITEM ( '' )  SURFACE ( )  );
#3558 = CARTESIAN_POINT ( 'NONE',  ( -6.015611763856276717, -18.68284711750060367, 2.453375430804002111 ) ) ;
#3559 = ADVANCED_FACE ( 'NONE', ( #22342 ), #37332, .F. ) ;
#3560 = ORIENTED_EDGE ( 'NONE', *, *, #2239, .T. ) ;
#3561 = CARTESIAN_POINT ( 'NONE',  ( 0.1084644655670281704, 42.70194587816329346, -6.022910953206664253 ) ) ;
#3562 = CARTESIAN_POINT ( 'NONE',  ( 1.227938101723748288, -26.79402671879349640, 33.52879263017854328 ) ) ;
#3563 = CARTESIAN_POINT ( 'NONE',  ( 5.894904586330512508, 3.346579165707559866, -19.83254446482585820 ) ) ;
#3564 = CARTESIAN_POINT ( 'NONE',  ( 0.8751705887134423323, 46.67919521768887847, -11.58504748649151317 ) ) ;
#3565 = ORIENTED_EDGE ( 'NONE', *, *, #8765, .F. ) ;
#3566 = CARTESIAN_POINT ( 'NONE',  ( 2.618530812446111078, 37.74802994993080318, -28.01451452546210774 ) ) ;
#3567 = CARTESIAN_POINT ( 'NONE',  ( 0.6001305935487315502, -48.10757715638248300, -0.5236757026887732813 ) ) ;
#3568 = CARTESIAN_POINT ( 'NONE',  ( 4.975801465491695552, -47.10002938642136883, -8.787181743659990829 ) ) ;
#3569 = CARTESIAN_POINT ( 'NONE',  ( 0.7762783648524385072, -44.59086139387527226, -17.50713302551375961 ) ) ;
#3570 = CARTESIAN_POINT ( 'NONE',  ( 0.1149546198390368201, -17.60995280955134845, -40.45783146769726102 ) ) ;
#3571 = CARTESIAN_POINT ( 'NONE',  ( 0.1129192098497447394, 10.29049805561828101, 42.90754522869457332 ) ) ;
#3572 = CARTESIAN_POINT ( 'NONE',  ( 0.8557997880470599172, 41.02602466100778145, 24.73961900479265807 ) ) ;
#3573 = CARTESIAN_POINT ( 'NONE',  ( 0.9722240741986378776, 20.94823706911201100, 37.44729083276432391 ) ) ;
#3574 = CARTESIAN_POINT ( 'NONE',  ( 0.7245667037590776127, 29.92941129926897759, 37.65687897229936709 ) ) ;
#3575 = CARTESIAN_POINT ( 'NONE',  ( 0.9784957157296367836, -1.632997897510987118, -41.87679995963272717 ) ) ;
#3576 = CARTESIAN_POINT ( 'NONE',  ( 0.7764139734771262624, 11.73874210050403555, -45.41191919314488956 ) ) ;
#3577 = ORIENTED_EDGE ( 'NONE', *, *, #50850, .T. ) ;
#3578 = B_SPLINE_CURVE_WITH_KNOTS ( 'NONE', 3,
 ( #57343, #14175, #61428, #47360 ),
 .UNSPECIFIED., .F., .F.,
 ( 4, 4 ),
 ( 1.907487264466063683E-17, 0.004444306975806113294 ),
 .UNSPECIFIED. ) ;
#3579 = CARTESIAN_POINT ( 'NONE',  ( 0.6064782688330867533, -46.73948921451010108, -3.841170965404212101 ) ) ;
#3580 = CARTESIAN_POINT ( 'NONE',  ( 0.6064782688330858651, -25.83066036557900702, 39.14219502655511462 ) ) ;
#3581 = CARTESIAN_POINT ( 'NONE',  ( -6.016489644550736315, -11.46752133529394868, 14.95199950534944122 ) ) ;
#3582 = CARTESIAN_POINT ( 'NONE',  ( 0.5837800005270554760, -34.78054197040876971, -31.45710029367646143 ) ) ;
#3583 = CARTESIAN_POINT ( 'NONE',  ( 4.226256110419178924, -24.79946968843673716, -36.27414441664329559 ) ) ;
#3584 = CARTESIAN_POINT ( 'NONE',  ( 4.967162193818130511, -32.10009971360091896, 28.74031574030002645 ) ) ;
#3585 = APPLICATION_PROTOCOL_DEFINITION ( 'draft international standard', 'automotive_design', 1998, #20346 ) ;
#3586 = DIRECTION ( 'NONE',  ( 0.000000000000000000, 0.000000000000000000, -1.000000000000000000 ) ) ;
#3587 = CARTESIAN_POINT ( 'NONE',  ( 0.5832366564991521285, 12.65934068133983814, 46.19265750221173050 ) ) ;
#3588 = EDGE_CURVE ( 'NONE', #46801, #20008, #55869, .T. ) ;
#3589 = CARTESIAN_POINT ( 'NONE',  ( 0.6008122571543325074, -1.138706917017746623, 49.09437744816052884 ) ) ;
#3591 = ORIENTED_EDGE ( 'NONE', *, *, #32008, .F. ) ;
#3590 = CARTESIAN_POINT ( 'NONE',  ( 0.6029303876144825880, -46.43417959025982356, -12.57751758557253652 ) ) ;
#3592 = VERTEX_POINT ( 'NONE', #32367 ) ;
#3593 = TOROIDAL_SURFACE ( 'NONE', #38647, 15.71999999999999709, 0.2800000000000011924 ) ;
#3594 = CARTESIAN_POINT ( 'NONE',  ( 0.1156867017252034974, -7.165540636711854816, 43.53846385276836628 ) ) ;
#3595 = LINE ( 'NONE', #13044, #23508 ) ;
#3596 = FACE_OUTER_BOUND ( 'NONE', #14812, .T. ) ;
#3597 = EDGE_CURVE ( 'NONE', #56316, #32792, #40561, .T. ) ;
#3598 = ORIENTED_EDGE ( 'NONE', *, *, #5149, .T. ) ;
#3599 = CARTESIAN_POINT ( 'NONE',  ( 0.5998501479064699549, 0.5236536531308225717, 48.10473956285920138 ) ) ;
#3600 = DIRECTION ( 'NONE',  ( 1.000000000000000000, 0.000000000000000000, 0.000000000000000000 ) ) ;
#3601 = CARTESIAN_POINT ( 'NONE',  ( 0.7954196712028469562, -29.96539649507113623, 37.62416450255238232 ) ) ;
#3602 = EDGE_CURVE ( 'NONE', #34420, #35039, #21116, .T. ) ;
#3603 = ORIENTED_EDGE ( 'NONE', *, *, #52758, .F. ) ;
#3604 = EDGE_LOOP ( 'NONE', ( #2504, #52252, #52224, #46336 ) ) ;
#3605 = CARTESIAN_POINT ( 'NONE',  ( 0.2111111111111110827, -9.497654031326126400, -1.199999999999999956 ) ) ;
#3606 = AXIS2_PLACEMENT_3D ( 'NONE', #20256, #39997, #48138 ) ;
#3607 = CARTESIAN_POINT ( 'NONE',  ( -6.016761891674564211, -18.20201388312091950, -4.873659902332557081 ) ) ;
#3608 = CARTESIAN_POINT ( 'NONE',  ( 4.833616638992208614, 3.476827473557241976, 46.11947910922911120 ) ) ;
#3609 = EDGE_CURVE ( 'NONE', #49479, #41448, #41337, .T. ) ;
#3610 = DIRECTION ( 'NONE',  ( -0.000000000000000000, 1.000000000000000000, 0.000000000000000000 ) ) ;
#3611 = CARTESIAN_POINT ( 'NONE',  ( 0.6254311100348672881, -23.45480814408399084, -42.00127298835415246 ) ) ;
#3612 = CARTESIAN_POINT ( 'NONE',  ( 0.7948878604505668077, -24.70668313632145185, 42.42968837618095534 ) ) ;
#3613 = VERTEX_POINT ( 'NONE', #48606 ) ;
#3614 = CARTESIAN_POINT ( 'NONE',  ( 0.8753041380234530822, 10.05717963662871739, -48.06237057854679051 ) ) ;
#3615 = CARTESIAN_POINT ( 'NONE',  ( 4.967162193818130511, -38.44485641567084855, 19.45289607368810181 ) ) ;
#3616 = ORIENTED_EDGE ( 'NONE', *, *, #27171, .F. ) ;
#3617 = CARTESIAN_POINT ( 'NONE',  ( -6.078726893082806448, 3.076629396955071538, 19.00863995194059086 ) ) ;
#3618 = CARTESIAN_POINT ( 'NONE',  ( -1.200000000000006617, 0.000000000000000000, 0.000000000000000000 ) ) ;
#3619 = CARTESIAN_POINT ( 'NONE',  ( 0.9790724872846768845, 4.235103416345695315, -41.69411360173413073 ) ) ;
#3620 = CARTESIAN_POINT ( 'NONE',  ( 7.000000000000016875, -54.69470952477895054, -58.44237546506863623 ) ) ;
#3621 = ORIENTED_EDGE ( 'NONE', *, *, #27547, .T. ) ;
#3622 = ORIENTED_EDGE ( 'NONE', *, *, #60515, .F. ) ;
#3623 = CARTESIAN_POINT ( 'NONE',  ( 0.1149546198390367369, -44.12336736438651030, -0.2738931372102353934 ) ) ;
#3624 = CARTESIAN_POINT ( 'NONE',  ( 30.00000000000000711, 19.00000000000000000, -1.386669559958810165E-30 ) ) ;
#3625 = ORIENTED_EDGE ( 'NONE', *, *, #45679, .F. ) ;
#3626 = CARTESIAN_POINT ( 'NONE',  ( 0.6064515330803583737, -2.277169567790236382, -46.84174243980059060 ) ) ;
#3627 = ORIENTED_EDGE ( 'NONE', *, *, #53812, .T. ) ;
#3628 = LINE ( 'NONE', #31543, #21505 ) ;
#3629 = CIRCLE ( 'NONE', #11670, 43.92652462719577500 ) ;
#3630 = ORIENTED_EDGE ( 'NONE', *, *, #48205, .F. ) ;
#3631 = CARTESIAN_POINT ( 'NONE',  ( 0.6001305935487422083, 0.5236757026889211630, -48.10757715638248300 ) ) ;
#3632 = CARTESIAN_POINT ( 'NONE',  ( 3.678834586032788234, -12.15221970334232537, -47.44402940212869879 ) ) ;
#3633 =( BOUNDED_SURFACE ( )  B_SPLINE_SURFACE ( 3, 1, ( 
 ( #59937, #31439 ),
 ( #1991, #25195 ),
 ( #49609, #1365 ),
 ( #49930, #20814 ) ),
 .UNSPECIFIED., .F., .F., .F. ) 
 B_SPLINE_SURFACE_WITH_KNOTS ( ( 4, 4 ),
 ( 2, 2 ),
 ( 0.000000000000000000, 1.000000000000000000 ),
 ( 0.000000000000000000, 1.000000000000000000 ),
 .UNSPECIFIED. ) 
 GEOMETRIC_REPRESENTATION_ITEM ( )  RATIONAL_B_SPLINE_SURFACE ( (
 ( 1.000000000000000000, 1.000000000000000000),
 ( 0.7211978278499968642, 0.9934217856018975334),
 ( 0.7211978278499968642, 0.9934217856018975334),
 ( 1.000000000000000000, 1.000000000000000000) ) ) 
 REPRESENTATION_ITEM ( '' )  SURFACE ( )  );
#3634 = CIRCLE ( 'NONE', #40716, 43.92652462719577500 ) ;
#3635 = CARTESIAN_POINT ( 'NONE',  ( 0.6029442701453591180, -14.05591772168299158, -47.05291066618041640 ) ) ;
#3636 = ORIENTED_EDGE ( 'NONE', *, *, #34980, .T. ) ;
#3637 = CARTESIAN_POINT ( 'NONE',  ( 0.6252788684277220677, -8.514552591182596331, -48.36265837757115094 ) ) ;
#3638 = AXIS2_PLACEMENT_3D ( 'NONE', #31623, #16605, #16291 ) ;
#3639 = EDGE_CURVE ( 'NONE', #45306, #9574, #34220, .T. ) ;
#3640 = CARTESIAN_POINT ( 'NONE',  ( -6.078075953587585900, 19.25604180663921738, 0.005309246513133128106 ) ) ;
#3641 = CARTESIAN_POINT ( 'NONE',  ( 3.783278058412224087, -43.00370293663099375, 1.726763838446040644 ) ) ;
#3642 = B_SPLINE_CURVE_WITH_KNOTS ( 'NONE', 3,
 ( #44171, #57897, #582, #53208 ),
 .UNSPECIFIED., .F., .F.,
 ( 4, 4 ),
 ( 2.081470520767878803E-17, 0.004444306975806114161 ),
 .UNSPECIFIED. ) ;
#3643 = EDGE_CURVE ( 'NONE', #3830, #44540, #38313, .T. ) ;
#3644 = ORIENTED_EDGE ( 'NONE', *, *, #27146, .T. ) ;
#3645 = CARTESIAN_POINT ( 'NONE',  ( -19.36083530377080564, -12.39979437149483132, -1.582588903604334574 ) ) ;
#3646 = CYLINDRICAL_SURFACE ( 'NONE', #22822, 2.649999999999992806 ) ;
#3647 = CARTESIAN_POINT ( 'NONE',  ( 4.956445790444027999, 24.88142650099568698, -39.98065363916886383 ) ) ;
#3648 = LINE ( 'NONE', #50654, #30953 ) ;
#3649 = CARTESIAN_POINT ( 'NONE',  ( 0.8557997880470690211, 23.15977007032381607, -41.93815086860232810 ) ) ;
#3650 = EDGE_LOOP ( 'NONE', ( #36557, #49775, #54341, #33565 ) ) ;
#3651 = EDGE_CURVE ( 'NONE', #25227, #26701, #35913, .T. ) ;
#3652 = CARTESIAN_POINT ( 'NONE',  ( 1.231276596079881047, -39.86997064245551314, 12.94844438485960580 ) ) ;
#3653 = CARTESIAN_POINT ( 'NONE',  ( 0.8744876279028306332, -6.955970791788286256, 48.60004650947653460 ) ) ;
#3654 = ORIENTED_EDGE ( 'NONE', *, *, #36593, .T. ) ;
#3656 = CARTESIAN_POINT ( 'NONE',  ( 0.8551540677456834771, -46.51172240253112733, -11.51835730326528839 ) ) ;
#3655 =( BOUNDED_SURFACE ( )  B_SPLINE_SURFACE ( 3, 1, ( 
 ( #3332, #35969 ),
 ( #36896, #22463 ),
 ( #7731, #45367 ),
 ( #35658, #8345 ) ),
 .UNSPECIFIED., .F., .F., .F. ) 
 B_SPLINE_SURFACE_WITH_KNOTS ( ( 4, 4 ),
 ( 2, 2 ),
 ( 0.000000000000000000, 1.000000000000000000 ),
 ( 0.000000000000000000, 1.000000000000000000 ),
 .UNSPECIFIED. ) 
 GEOMETRIC_REPRESENTATION_ITEM ( )  RATIONAL_B_SPLINE_SURFACE ( (
 ( 1.000000000000000000, 1.000000000000000000),
 ( 0.7282232189291693025, 0.9929344683865674037),
 ( 0.7282232189291693025, 0.9929344683865674037),
 ( 1.000000000000000000, 1.000000000000000000) ) ) 
 REPRESENTATION_ITEM ( '' )  SURFACE ( )  );
#3657 = CARTESIAN_POINT ( 'NONE',  ( 2.648799415243708655, 46.08255460350053312, -16.76053771527007186 ) ) ;
#3658 = CARTESIAN_POINT ( 'NONE',  ( 0.7762783648524385072, 19.15108798908314469, 43.90991295203428280 ) ) ;
#3659 = CARTESIAN_POINT ( 'NONE',  ( 0.1073791018717578927, -11.62916352156179123, 41.52698815987148606 ) ) ;
#3660 = B_SPLINE_CURVE_WITH_KNOTS ( 'NONE', 3,
 ( #21259, #40093, #11243, #49755, #59142, #1821 ),
 .UNSPECIFIED., .F., .F.,
 ( 4, 2, 4 ),
 ( 6.149443329761889321E-18, 0.0002445244328975381071, 0.0004890488657950701427 ),
 .UNSPECIFIED. ) ;
#3661 = CARTESIAN_POINT ( 'NONE',  ( 0.8560838555295223751, 23.34035564869547841, 40.68907263964295851 ) ) ;
#3662 = CARTESIAN_POINT ( 'NONE',  ( 0.5997462898726536595, 5.235280152387000285, 48.82769165002921596 ) ) ;
#3663 = SURFACE_STYLE_FILL_AREA ( #20946 ) ;
#3664 = CARTESIAN_POINT ( 'NONE',  ( 0.5998501479064708430, 37.84527566984816360, 29.69975237324626605 ) ) ;
#3665 = CARTESIAN_POINT ( 'NONE',  ( 4.975610109902397937, 14.46773809681615575, -46.72401910687593585 ) ) ;
#3666 = CARTESIAN_POINT ( 'NONE',  ( 4.549368137175248350, -42.06008734272402450, 8.582197505783685898 ) ) ;
#3667 = EDGE_CURVE ( 'NONE', #55095, #36276, #45940, .T. ) ;
#3668 = CARTESIAN_POINT ( 'NONE',  ( 5.965394784446460541, 7.841344330024671017, 18.96850062921637559 ) ) ;
#3669 = CARTESIAN_POINT ( 'NONE',  ( 0.5998501479064699549, -46.60114184914309021, -11.94461217097453343 ) ) ;
#3670 = CARTESIAN_POINT ( 'NONE',  ( 0.6026777506516367566, -1.748060344709603253, -49.07637594269235137 ) ) ;
#3671 = CARTESIAN_POINT ( 'NONE',  ( 3.050102900204245682, 16.87969600441305573, 40.62635981695458298 ) ) ;
#3672 = CARTESIAN_POINT ( 'NONE',  ( 0.5800708057587377064, 37.61306623599842425, 29.65250565429455776 ) ) ;
#3673 = CARTESIAN_POINT ( 'NONE',  ( 4.956653778116966613, 0.000000000000000000, 0.000000000000000000 ) ) ;
#3674 = CARTESIAN_POINT ( 'NONE',  ( 1.834102595619085951, 32.68067448320012858, -29.53254577886568200 ) ) ;
#3675 = EDGE_CURVE ( 'NONE', #33022, #1834, #29498, .T. ) ;
#3676 = ORIENTED_EDGE ( 'NONE', *, *, #23344, .T. ) ;
#3677 = CONICAL_SURFACE ( 'NONE', #49756, 42.92674063221959813, 1.485477209440487556 ) ;
#3678 = CARTESIAN_POINT ( 'NONE',  ( 4.553261556744873317, 38.38432632180467863, 21.35844232721216684 ) ) ;
#3679 = CARTESIAN_POINT ( 'NONE',  ( 2.706805983486679335, 28.34065445965364205, -33.66873056885675908 ) ) ;
#3680 = CARTESIAN_POINT ( 'NONE',  ( 50.50000000000000000, 0.000000000000000000, 0.000000000000000000 ) ) ;
#3681 = AXIS2_PLACEMENT_3D ( 'NONE', #53613, #30438, #29829 ) ;
#3682 = ORIENTED_EDGE ( 'NONE', *, *, #32587, .F. ) ;
#3683 = CARTESIAN_POINT ( 'NONE',  ( 5.917102823773431552, 0.6634426252560792214, 20.10098410363869093 ) ) ;
#3684 = EDGE_CURVE ( 'NONE', #1788, #14276, #43549, .T. ) ;
#3685 = CARTESIAN_POINT ( 'NONE',  ( 4.956653778116975495, -31.29546495791875316, 36.51451553856407628 ) ) ;
#3686 = ORIENTED_EDGE ( 'NONE', *, *, #22881, .F. ) ;
#3687 = CARTESIAN_POINT ( 'NONE',  ( 0.7413678028165011646, -26.75786355817048090, 35.05000470146295299 ) ) ;
#3688 = ORIENTED_EDGE ( 'NONE', *, *, #12608, .T. ) ;
#3689 = CARTESIAN_POINT ( 'NONE',  ( 0.8760168074887090262, 48.09529047980637984, -0.8912768426701217495 ) ) ;
#3690 = CARTESIAN_POINT ( 'NONE',  ( 0.6846871229502932144, -33.25969555998718619, -34.48177377577871283 ) ) ;
#3691 = B_SPLINE_CURVE_WITH_KNOTS ( 'NONE', 3,
 ( #6481, #53795, #49125, #35050 ),
 .UNSPECIFIED., .F., .F.,
 ( 4, 4 ),
 ( 6.254634441385501517E-18, 0.004566006591234646368 ),
 .UNSPECIFIED. ) ;
#3692 = ORIENTED_EDGE ( 'NONE', *, *, #34905, .T. ) ;
#3693 = CARTESIAN_POINT ( 'NONE',  ( 5.960221823109900008, -12.49951306783101579, 16.28072933292526159 ) ) ;
#3694 = CARTESIAN_POINT ( 'NONE',  ( 4.967162193818130511, 0.000000000000000000, 0.000000000000000000 ) ) ;
#3695 = ORIENTED_EDGE ( 'NONE', *, *, #30939, .F. ) ;
#3696 = CARTESIAN_POINT ( 'NONE',  ( 0.9756354156337445627, 21.34128958497381845, 37.22481466014907170 ) ) ;
#3697 = LINE ( 'NONE', #27527, #19375 ) ;
#3698 = AXIS2_PLACEMENT_3D ( 'NONE', #10382, #19173, #61729 ) ;
#3699 = VERTEX_POINT ( 'NONE', #24807 ) ;
#3700 = CARTESIAN_POINT ( 'NONE',  ( -2.739355103387248747, -4.498893467419605940, -14.23402699589354370 ) ) ;
#3701 = ORIENTED_EDGE ( 'NONE', *, *, #58044, .F. ) ;
#3702 = CARTESIAN_POINT ( 'NONE',  ( -6.057079549204054558, 17.84642505839085302, -7.234386203056722309 ) ) ;
#3703 = ORIENTED_EDGE ( 'NONE', *, *, #15635, .T. ) ;
#3704 = VECTOR ( 'NONE', #25561, 1000.000000000000000 ) ;
#3705 = VERTEX_POINT ( 'NONE', #29190 ) ;
#3706 = PLANE ( 'NONE',  #2618 ) ;
#3707 = DIRECTION ( 'NONE',  ( 0.09835009131224567436, -0.9951218349151971232, -0.007732607185427117953 ) ) ;
#3708 = CARTESIAN_POINT ( 'NONE',  ( 0.3676999524040366896, -38.83470403830472151, -20.92406140260821346 ) ) ;
#3709 = CARTESIAN_POINT ( 'NONE',  ( 0.1101816497532063233, -16.37745527993615013, 39.89358705406957029 ) ) ;
#3710 = CARTESIAN_POINT ( 'NONE',  ( 4.060580049360325461, -29.17232330074064350, -32.87009655593170976 ) ) ;
#3711 = EDGE_LOOP ( 'NONE', ( #32062, #21018 ) ) ;
#3712 = CARTESIAN_POINT ( 'NONE',  ( 0.9762797500689124330, -39.42083772998332591, 14.22400568939802845 ) ) ;
#3713 = EDGE_CURVE ( 'NONE', #48545, #58092, #6890, .T. ) ;
#3714 = CARTESIAN_POINT ( 'NONE',  ( 5.960721111146673579, 2.685391721746036353, -20.34914600876572521 ) ) ;
#3715 = CARTESIAN_POINT ( 'NONE',  ( 4.963659409799330291, 3.403493583737961181, -44.62477100936213503 ) ) ;
#3716 = VERTEX_POINT ( 'NONE', #48919 ) ;
#3717 = B_SPLINE_CURVE_WITH_KNOTS ( 'NONE', 3,
 ( #20324, #9674, #48818, #39444 ),
 .UNSPECIFIED., .F., .F.,
 ( 4, 4 ),
 ( 0.000000000000000000, 0.004445488388166992516 ),
 .UNSPECIFIED. ) ;
#3718 = ADVANCED_FACE ( 'NONE', ( #25110 ), #46924, .T. ) ;
#3719 = EDGE_LOOP ( 'NONE', ( #57930, #23588, #42017, #58475 ) ) ;
#3720 = CARTESIAN_POINT ( 'NONE',  ( 0.9752570700956788574, 34.18150842933915357, -25.93764562640069826 ) ) ;
#3721 = CARTESIAN_POINT ( 'NONE',  ( 0.8751705887134423323, 47.55935879196461968, 7.160166390004468973 ) ) ;
#3722 = CARTESIAN_POINT ( 'NONE',  ( 0.8744876279028263033, 5.599149760998344050, -48.77498920895221346 ) ) ;
#3723 = CARTESIAN_POINT ( 'NONE',  ( 0.6041374136657476912, 41.57494627055144321, -24.20487816031478800 ) ) ;
#3724 = EDGE_CURVE ( 'NONE', #38743, #51844, #8884, .T. ) ;
#3725 = EDGE_CURVE ( 'NONE', #60472, #51862, #18128, .T. ) ;
#3726 = ORIENTED_EDGE ( 'NONE', *, *, #22675, .T. ) ;
#3728 = CARTESIAN_POINT ( 'NONE',  ( 0.5834872094924170582, 47.45604551759237211, 6.476680342366744725 ) ) ;
#3727 = CIRCLE ( 'NONE', #12758, 47.91270532121795611 ) ;
#3729 = CONICAL_SURFACE ( 'NONE', #741, 43.92652462719577500, 1.486293639869522343 ) ;
#3730 = EDGE_CURVE ( 'NONE', #39191, #24982, #911, .T. ) ;
#3731 = CARTESIAN_POINT ( 'NONE',  ( 0.9754292589017200532, -17.11069906115304562, 38.25639089791319947 ) ) ;
#3732 = CARTESIAN_POINT ( 'NONE',  ( -5.283180000000052168, -15.43999999999999417, 1.890854657883513307E-15 ) ) ;
#3733 = CARTESIAN_POINT ( 'NONE',  ( 4.226256110419178924, -39.40860114104851419, -19.43680544978874281 ) ) ;
#3734 = CARTESIAN_POINT ( 'NONE',  ( 1.296416391601052709, -43.55378818229317517, 6.736090041566987097 ) ) ;
#3735 = CARTESIAN_POINT ( 'NONE',  ( 0.3622758884714730732, 39.50828911766998175, -17.25816669464953534 ) ) ;
#3736 =( BOUNDED_SURFACE ( )  B_SPLINE_SURFACE ( 3, 1, ( 
 ( #38509, #14698 ),
 ( #563, #5866 ),
 ( #33810, #29087 ),
 ( #48204, #24701 ) ),
 .UNSPECIFIED., .F., .F., .F. ) 
 B_SPLINE_SURFACE_WITH_KNOTS ( ( 4, 4 ),
 ( 2, 2 ),
 ( 0.000000000000000000, 1.000000000000000000 ),
 ( 0.000000000000000000, 1.000000000000000000 ),
 .UNSPECIFIED. ) 
 GEOMETRIC_REPRESENTATION_ITEM ( )  RATIONAL_B_SPLINE_SURFACE ( (
 ( 1.000000000000000000, 1.000000000000000000),
 ( 0.7211978278499968642, 0.9934217856018975334),
 ( 0.7211978278499968642, 0.9934217856018975334),
 ( 1.000000000000000000, 1.000000000000000000) ) ) 
 REPRESENTATION_ITEM ( '' )  SURFACE ( )  );
#3737 = EDGE_CURVE ( 'NONE', #5739, #7607, #36122, .T. ) ;
#3738 = ORIENTED_EDGE ( 'NONE', *, *, #61847, .T. ) ;
#3739 = CARTESIAN_POINT ( 'NONE',  ( 1.231276596079887264, 41.65019306089983786, 4.747440258480190245 ) ) ;
#3740 = CARTESIAN_POINT ( 'NONE',  ( 5.910764540655177868, 8.479982303153068557, -18.23708141692013740 ) ) ;
#3741 = EDGE_CURVE ( 'NONE', #14535, #448, #16332, .T. ) ;
#3742 = CARTESIAN_POINT ( 'NONE',  ( 0.1081432562775997974, 21.92800090985269890, -37.13343246403903919 ) ) ;
#3743 = CARTESIAN_POINT ( 'NONE',  ( 5.894904586330512508, 19.70964338679887362, 4.007414331817764186 ) ) ;
#3744 = CARTESIAN_POINT ( 'NONE',  ( 0.5838002273316424962, 6.386683873061191896, -47.46823345111864256 ) ) ;
#3745 = CARTESIAN_POINT ( 'NONE',  ( 0.6846871229502932144, -46.04462816497477462, -13.23224427737877562 ) ) ;
#3746 = AXIS2_PLACEMENT_3D ( 'NONE', #21161, #54650, #35895 ) ;
#3747 = CARTESIAN_POINT ( 'NONE',  ( 0.8744876279028306332, -48.79802643035336018, -5.394688766001929814 ) ) ;
#3748 = FACE_OUTER_BOUND ( 'NONE', #4040, .T. ) ;
#3749 = ORIENTED_EDGE ( 'NONE', *, *, #40211, .T. ) ;
#3750 = CARTESIAN_POINT ( 'NONE',  ( 5.000000000000007994, -56.56854249492331377, -56.56854249492430142 ) ) ;
#3751 = CARTESIAN_POINT ( 'NONE',  ( 0.2940133293163009753, 44.06980802084461857, -2.023010277765129761 ) ) ;
#3752 = DIRECTION ( 'NONE',  ( -1.000000000000000000, -0.000000000000000000, -0.000000000000000000 ) ) ;
#3753 = CARTESIAN_POINT ( 'NONE',  ( 0.7764139734771247081, -2.458099863852005740, 46.84013467066674252 ) ) ;
#3754 = ORIENTED_EDGE ( 'NONE', *, *, #39719, .T. ) ;
#3755 = CARTESIAN_POINT ( 'NONE',  ( -6.015611763856276717, 4.882992715191300626, 18.19956619163659894 ) ) ;
#3756 = LINE ( 'NONE', #37313, #23956 ) ;
#3757 = EDGE_CURVE ( 'NONE', #41399, #16218, #7218, .T. ) ;
#3758 = B_SPLINE_CURVE_WITH_KNOTS ( 'NONE', 3,
 ( #19446, #28833, #44206, #19760 ),
 .UNSPECIFIED., .F., .F.,
 ( 4, 4 ),
 ( 0.000000000000000000, 0.005004741218457418872 ),
 .UNSPECIFIED. ) ;
#3759 = CARTESIAN_POINT ( 'NONE',  ( 0.000000000000000000, 0.000000000000000000, 0.000000000000000000 ) ) ;
#3760 = ORIENTED_EDGE ( 'NONE', *, *, #15720, .T. ) ;
#3761 = CARTESIAN_POINT ( 'NONE',  ( 0.3622758884714730732, -25.58609868863794290, 34.70015533914785522 ) ) ;
#3762 = EDGE_CURVE ( 'NONE', #46350, #8115, #58480, .T. ) ;
#3763 = CARTESIAN_POINT ( 'NONE',  ( 0.6001305935487315502, -47.76436356026964347, -5.760103278697851437 ) ) ;
#3764 = CARTESIAN_POINT ( 'NONE',  ( 4.960156602257181468, -44.12083041402454597, -14.43621227656575101 ) ) ;
#3765 = EDGE_LOOP ( 'NONE', ( #15448, #56790, #30990, #9629 ) ) ;
#3766 = DIRECTION ( 'NONE',  ( 0.000000000000000000, 0.000000000000000000, 1.000000000000000000 ) ) ;
#3767 = VECTOR ( 'NONE', #5831, 1000.000000000000000 ) ;
#3768 = ORIENTED_EDGE ( 'NONE', *, *, #38628, .F. ) ;
#3769 = ORIENTED_EDGE ( 'NONE', *, *, #2945, .F. ) ;
#3770 = CARTESIAN_POINT ( 'NONE',  ( -6.072942160501519915, -8.893884846139727074, 17.07931423191886822 ) ) ;
#3772 = CARTESIAN_POINT ( 'NONE',  ( -2.708315649062910779, -14.47261168455368185, -2.171184472130632148 ) ) ;
#3771 = PRODUCT_DEFINITION ( 'UNKNOWN', '', #29877, #38625 ) ;
#3773 = ORIENTED_EDGE ( 'NONE', *, *, #43228, .F. ) ;
#3774 = CARTESIAN_POINT ( 'NONE',  ( 0.9762797500689124330, 24.45014227843030596, -34.03697001423921620 ) ) ;
#3775 = PRODUCT ( 'housing left', 'housing left', '', ( #26178 ) ) ;
#3776 = ORIENTED_EDGE ( 'NONE', *, *, #15510, .F. ) ;
#3777 = CARTESIAN_POINT ( 'NONE',  ( 0.8751705887134553219, 28.56654290188653178, -38.69254731947804515 ) ) ;
#3778 = LINE ( 'NONE', #7003, #31838 ) ;
#3779 = FACE_OUTER_BOUND ( 'NONE', #28853, .T. ) ;
#3780 = VERTEX_POINT ( 'NONE', #21343 ) ;
#3781 = CARTESIAN_POINT ( 'NONE',  ( 1.231276596079881047, -35.03243822710529543, 23.02183839058294623 ) ) ;
#3782 = AXIS2_PLACEMENT_3D ( 'NONE', #29947, #34978, #26168 ) ;
#3783 = CARTESIAN_POINT ( 'NONE',  ( 5.895596859100789899, -9.669028665050335647, 17.63627137143570067 ) ) ;
#3784 = PLANE ( 'NONE',  #60246 ) ;
#3785 = CARTESIAN_POINT ( 'NONE',  ( 0.7056313189692711152, 46.89390071911098090, -0.8430416974981863598 ) ) ;
#3786 = VERTEX_POINT ( 'NONE', #59856 ) ;
#3787 = CARTESIAN_POINT ( 'NONE',  ( 4.549368137175248350, 0.000000000000000000, 0.000000000000000000 ) ) ;
#3788 = CARTESIAN_POINT ( 'NONE',  ( 0.1145239942831223490, -31.46852519861557340, -30.93020210940707315 ) ) ;
#3789 = ORIENTED_EDGE ( 'NONE', *, *, #49175, .T. ) ;
#3790 = AXIS2_PLACEMENT_3D ( 'NONE', #48663, #48979, #412 ) ;
#3791 = CARTESIAN_POINT ( 'NONE',  ( 0.9754402186311955658, -42.90805920318125288, 0.1875553420610092115 ) ) ;
#3792 = B_SPLINE_CURVE_WITH_KNOTS ( 'NONE', 3,
 ( #58770, #35013, #12135, #25903 ),
 .UNSPECIFIED., .F., .F.,
 ( 4, 4 ),
 ( 0.000000000000000000, 0.005004948556313781882 ),
 .UNSPECIFIED. ) ;
#3793 = EDGE_CURVE ( 'NONE', #59500, #9430, #56936, .T. ) ;
#3794 = VERTEX_POINT ( 'NONE', #11645 ) ;
#3795 = CARTESIAN_POINT ( 'NONE',  ( 4.549368137175248350, -8.166781970325423856, -42.14271863032831078 ) ) ;
#3796 = CARTESIAN_POINT ( 'NONE',  ( 5.959547316686252039, 10.26589671991338548, 17.77392908783937386 ) ) ;
#3797 = ORIENTED_EDGE ( 'NONE', *, *, #25454, .T. ) ;
#3798 = CARTESIAN_POINT ( 'NONE',  ( 0.5835226383429285013, 4.875290024808289324, 46.64197703485532998 ) ) ;
#3799 = CARTESIAN_POINT ( 'NONE',  ( -6.078726893082806448, 0.6205993875984882058, -19.24600991553398188 ) ) ;
#3800 = CARTESIAN_POINT ( 'NONE',  ( 5.965394784446458765, 14.52385693118982601, 14.50338846149138305 ) ) ;
#3801 = CARTESIAN_POINT ( 'NONE',  ( -5.995132425357893702, -11.47834865841086049, -14.94489030678163033 ) ) ;
#3802 = VECTOR ( 'NONE', #51739, 1000.000000000000114 ) ;
#3803 = EDGE_CURVE ( 'NONE', #61531, #57613, #26045, .T. ) ;
#3804 = VERTEX_POINT ( 'NONE', #41102 ) ;
#3805 = DIRECTION ( 'NONE',  ( -0.07500201931887527651, 0.9232442575324670830, 0.3768218916562764975 ) ) ;
#3806 = EDGE_CURVE ( 'NONE', #21146, #36659, #10699, .T. ) ;
#3807 = CARTESIAN_POINT ( 'NONE',  ( 0.8551540677456834771, -43.91216198251552782, 19.17641535420837684 ) ) ;
#3808 = CARTESIAN_POINT ( 'NONE',  ( 0.8560838555295158248, 9.983184696770717181, 45.83349056521764453 ) ) ;
#3809 = CARTESIAN_POINT ( 'NONE',  ( 0.1119898979215349921, -18.37259971277567416, -40.11743870246385768 ) ) ;
#3810 = CARTESIAN_POINT ( 'NONE',  ( 0.8554163680231708922, -46.86440027434177580, 2.221139355847124186 ) ) ;
#3811 = CARTESIAN_POINT ( 'NONE',  ( 0.5806925824938511393, 5.237374507879287044, 46.60249210726590263 ) ) ;
#3812 = CARTESIAN_POINT ( 'NONE',  ( 0.5832655196449136881, 4.920529935022127432, -46.63714794165569799 ) ) ;
#3813 = DIRECTION ( 'NONE',  ( 0.000000000000000000, 0.000000000000000000, 1.000000000000000000 ) ) ;
#3814 = CONICAL_SURFACE ( 'NONE', #60829, 43.92652462719577500, 1.486293639869522343 ) ;
#3815 = DIRECTION ( 'NONE',  ( 0.07439287786467665975, -0.9903339163990689809, 0.1170659376278736646 ) ) ;
#3816 = VECTOR ( 'NONE', #42312, 1000.000000000000114 ) ;
#3817 = B_SPLINE_CURVE_WITH_KNOTS ( 'NONE', 3,
 ( #49254, #6312, #44590, #29843, #40214, #2248 ),
 .UNSPECIFIED., .F., .F.,
 ( 4, 2, 4 ),
 ( 1.509951125874620249E-16, 0.0002445252820015219003, 0.0004890505640028928796 ),
 .UNSPECIFIED. ) ;
#3818 = CARTESIAN_POINT ( 'NONE',  ( 0.9769922540276048117, -12.83782684460722123, 39.89388119742184102 ) ) ;
#3819 = CARTESIAN_POINT ( 'NONE',  ( 1.227938101723747621, 6.439911493065174852, -42.43379953535178828 ) ) ;
#3820 = CARTESIAN_POINT ( 'NONE',  ( 0.5997462898726536595, -19.39900779840410294, -45.11352487427429736 ) ) ;
#3821 = CARTESIAN_POINT ( 'NONE',  ( 0.5782707292762423457, 42.89195216551532042, -18.97410849391256349 ) ) ;
#3822 = CARTESIAN_POINT ( 'NONE',  ( 3.783278058412224976, 27.54892951149544800, 33.06594414781506686 ) ) ;
#3823 = CARTESIAN_POINT ( 'NONE',  ( 0.6001305935487315502, -38.48510059944028683, -28.87057754790923880 ) ) ;
#3824 = CARTESIAN_POINT ( 'NONE',  ( 3.050102900204245682, -21.23864880574211256, 38.52719878325451930 ) ) ;
#3825 = CARTESIAN_POINT ( 'NONE',  ( -6.016489644550736315, 16.32089497094061059, 9.417787539062304702 ) ) ;
#3826 = CARTESIAN_POINT ( 'NONE',  ( 0.8560838555295223751, -6.899551485032601406, 46.39794201672221163 ) ) ;
#3827 = CARTESIAN_POINT ( 'NONE',  ( 0.6023142530420679819, 46.39979989577480524, -12.70386526143724026 ) ) ;
#3829 = VERTEX_POINT ( 'NONE', #39867 ) ;
#3828 = CARTESIAN_POINT ( 'NONE',  ( 0.8751705887134423323, 24.81530984069208401, -41.19904111682483716 ) ) ;
#3830 = VERTEX_POINT ( 'NONE', #2838 ) ;
#3831 = VECTOR ( 'NONE', #33372, 999.9999999999998863 ) ;
#3832 = CARTESIAN_POINT ( 'NONE',  ( 0.5809828226811617480, 41.20389530892307306, 24.41822904836939401 ) ) ;
#3833 = CARTESIAN_POINT ( 'NONE',  ( 3.407937589446174087, -13.10584870154463744, -3.987184287467924193 ) ) ;
#3834 = VERTEX_POINT ( 'NONE', #21970 ) ;
#3835 = ORIENTED_EDGE ( 'NONE', *, *, #43345, .F. ) ;
#3836 = CARTESIAN_POINT ( 'NONE',  ( 0.2940135542859036444, -23.55385452459446327, -37.30223164538097080 ) ) ;
#3837 = FACE_OUTER_BOUND ( 'NONE', #31708, .T. ) ;
#3838 = VERTEX_POINT ( 'NONE', #35145 ) ;
#3839 = ORIENTED_EDGE ( 'NONE', *, *, #23280, .F. ) ;
#3840 = EDGE_CURVE ( 'NONE', #33545, #27840, #19915, .T. ) ;
#3841 = CARTESIAN_POINT ( 'NONE',  ( 0.5263152470540364281, 0.000000000000000000, -42.88844316795388778 ) ) ;
#3842 = DIRECTION ( 'NONE',  ( -1.000000000000000000, -3.135800716341471541E-16, -1.298891185607920445E-16 ) ) ;
#3843 = CARTESIAN_POINT ( 'NONE',  ( 0.9752132459055865565, -41.38545930839056552, 11.33038172416138067 ) ) ;
#3844 = VERTEX_POINT ( 'NONE', #55763 ) ;
#3845 = ORIENTED_EDGE ( 'NONE', *, *, #17343, .F. ) ;
#3846 = CARTESIAN_POINT ( 'NONE',  ( 0.5809828226811617480, -11.86925843957133786, -46.40184912890851621 ) ) ;
#3847 = VERTEX_POINT ( 'NONE', #22891 ) ;
#3848 = CARTESIAN_POINT ( 'NONE',  ( 30.00000000000001066, 4.342925291379521108E-15, -1.386669559958810165E-30 ) ) ;
#3849 = CARTESIAN_POINT ( 'NONE',  ( -2.601141883200662974, -13.66110686928774953, 6.014115610402557266 ) ) ;
#3850 = CARTESIAN_POINT ( 'NONE',  ( 0.5988103622719985752, -18.96890139670021469, 44.21009254328972560 ) ) ;
#3851 = EDGE_LOOP ( 'NONE', ( #10410, #46252, #34471, #38827 ) ) ;
#3852 =( BOUNDED_SURFACE ( )  B_SPLINE_SURFACE ( 3, 1, ( 
 ( #20012, #15308 ),
 ( #17922, #56718 ),
 ( #56105, #56410 ),
 ( #42051, #24689 ) ),
 .UNSPECIFIED., .F., .F., .F. ) 
 B_SPLINE_SURFACE_WITH_KNOTS ( ( 4, 4 ),
 ( 2, 2 ),
 ( 0.000000000000000000, 1.000000000000000000 ),
 ( 0.000000000000000000, 1.000000000000000000 ),
 .UNSPECIFIED. ) 
 GEOMETRIC_REPRESENTATION_ITEM ( )  RATIONAL_B_SPLINE_SURFACE ( (
 ( 1.000000000000000000, 1.000000000000000000),
 ( 0.7211978278499970862, 0.9934217856018976445),
 ( 0.7211978278499970862, 0.9934217856018976445),
 ( 1.000000000000000000, 1.000000000000000000) ) ) 
 REPRESENTATION_ITEM ( '' )  SURFACE ( )  );
#3853 = CARTESIAN_POINT ( 'NONE',  ( 0.1073791018717578927, 0.4849339620933161288, -43.12183934961191056 ) ) ;
#3854 = ORIENTED_EDGE ( 'NONE', *, *, #51096, .T. ) ;
#3855 = AXIS2_PLACEMENT_3D ( 'NONE', #28346, #13342, #51520 ) ;
#3856 = VERTEX_POINT ( 'NONE', #51066 ) ;
#3857 = AXIS2_PLACEMENT_3D ( 'NONE', #13004, #13609, #33032 ) ;
#3858 = ORIENTED_EDGE ( 'NONE', *, *, #55941, .T. ) ;
#3859 = CARTESIAN_POINT ( 'NONE',  ( 0.5997462898726536595, 46.76781179977606229, 14.97743000668126001 ) ) ;
#3860 = LINE ( 'NONE', #42131, #49255 ) ;
#3861 = CARTESIAN_POINT ( 'NONE',  ( 0.3676999524040366896, 24.55639947021014180, -36.64606156713571750 ) ) ;
#3862 = CARTESIAN_POINT ( 'NONE',  ( 0.7948878604505675849, -29.92962973000293303, 38.92192070701729278 ) ) ;
#3863 = FACE_OUTER_BOUND ( 'NONE', #20398, .T. ) ;
#3864 = B_SPLINE_CURVE_WITH_KNOTS ( 'NONE', 3,
 ( #31428, #22966, #22038, #27653, #32060, #17961, #8224, #41162, #17642, #7926, #41782, #27039, #3212, #60844, #22338, #18267 ),
 .UNSPECIFIED., .F., .F.,
 ( 4, 3, 3, 3, 3, 4 ),
 ( 2.030557555191247372E-17, 0.0002612764279487740302, 0.0003919131003184784861, 0.0005225497727000667737, 0.0007837925190632469806, 0.001045051706266716300 ),
 .UNSPECIFIED. ) ;
#3865 = ORIENTED_EDGE ( 'NONE', *, *, #15052, .F. ) ;
#3866 = CARTESIAN_POINT ( 'NONE',  ( 0.6001305935487422083, -24.50730504006484978, 41.40054608060251695 ) ) ;
#3867 = CARTESIAN_POINT ( 'NONE',  ( 0.3622758884714600280, 40.13994584881781691, -15.73321244754812298 ) ) ;
#3868 = EDGE_CURVE ( 'NONE', #59695, #9789, #28867, .T. ) ;
#3869 = CARTESIAN_POINT ( 'NONE',  ( 0.5782707292762442330, 42.89195216551504330, 18.97410849391315324 ) ) ;
#3870 = ORIENTED_EDGE ( 'NONE', *, *, #40700, .T. ) ;
#3871 = CARTESIAN_POINT ( 'NONE',  ( 0.1102847568649952675, 42.74337176234129743, -5.720244683738159530 ) ) ;
#3872 = EDGE_CURVE ( 'NONE', #41417, #51070, #42773, .T. ) ;
#3873 = LINE ( 'NONE', #41511, #12713 ) ;
#3874 = CARTESIAN_POINT ( 'NONE',  ( 7.000000000000021316, -80.00000000000001421, 2.649999999999992806 ) ) ;
#3875 = CARTESIAN_POINT ( 'NONE',  ( 0.7954196712028464011, 46.67728755034884358, -11.60747899261471083 ) ) ;
#3876 = ORIENTED_EDGE ( 'NONE', *, *, #49989, .F. ) ;
#3877 = CARTESIAN_POINT ( 'NONE',  ( 0.5263152470540364281, 0.000000000000000000, 0.000000000000000000 ) ) ;
#3878 = EDGE_CURVE ( 'NONE', #24212, #18593, #18497, .T. ) ;
#3879 = CARTESIAN_POINT ( 'NONE',  ( 0.1073791018717578927, -42.81622261970997556, 5.147744207006151207 ) ) ;
#3880 = CARTESIAN_POINT ( 'NONE',  ( 0.8744876279028263033, 46.86690837902584406, -14.62336997314537790 ) ) ;
#3881 = DIRECTION ( 'NONE',  ( -1.000000000000000000, -0.000000000000000000, -0.000000000000000000 ) ) ;
#3882 = LINE ( 'NONE', #22701, #41520 ) ;
#3884 = CARTESIAN_POINT ( 'NONE',  ( 3.270143674763207553, 3.277085381513305418, -13.28976595685390016 ) ) ;
#3883 = AXIS2_PLACEMENT_3D ( 'NONE', #58135, #35289, #20267 ) ;
#3885 = CARTESIAN_POINT ( 'NONE',  ( 0.5997462898726536595, -7.321308210775749004, 48.55872811583040516 ) ) ;
#3886 = CARTESIAN_POINT ( 'NONE',  ( 1.227938101723747621, 20.72293514920750468, 37.58536632582787007 ) ) ;
#3887 = CARTESIAN_POINT ( 'NONE',  ( 0.5988103622719987973, -46.30780754281423128, -13.03604477829274444 ) ) ;
#3888 = CARTESIAN_POINT ( 'NONE',  ( 0.9790724872846784388, -1.359965803035979137, -41.88658141930447698 ) ) ;
#3889 = CARTESIAN_POINT ( 'NONE',  ( 4.975801465491695552, -40.15204426031515794, -26.14269827151666092 ) ) ;
#3891 = EDGE_LOOP ( 'NONE', ( #44011, #14653, #58884, #58223 ) ) ;
#3890 = EDGE_CURVE ( 'NONE', #13682, #40152, #17349, .T. ) ;
#3892 = CARTESIAN_POINT ( 'NONE',  ( 0.5797568665920713737, -46.74494072455451033, 3.759763989900801295 ) ) ;
#3893 = DIRECTION ( 'NONE',  ( 0.07439287786467665975, -0.7144194931003113869, 0.6957517427942997434 ) ) ;
#3895 = EDGE_CURVE ( 'NONE', #49037, #15399, #39906, .T. ) ;
#3894 = CARTESIAN_POINT ( 'NONE',  ( 0.8744876279028263033, -13.11369837310799547, -47.31153099783008997 ) ) ;
#3896 = CARTESIAN_POINT ( 'NONE',  ( -6.016761891674564211, -14.94721834528423088, 11.47373234755497862 ) ) ;
#3897 = CARTESIAN_POINT ( 'NONE',  ( 0.9268187852002115479, -23.69707065591206430, -37.17799315774504265 ) ) ;
#3898 = CARTESIAN_POINT ( 'NONE',  ( 0.1103744047535531458, 42.75042227379820048, 5.667281528142542157 ) ) ;
#3899 = CARTESIAN_POINT ( 'NONE',  ( 0.5817216825391118284, -24.84894157072779919, 39.77141002054133168 ) ) ;
#3900 = AXIS2_PLACEMENT_3D ( 'NONE', #3222, #37703, #22348 ) ;
#3901 = CARTESIAN_POINT ( 'NONE',  ( 5.896782393890504181, -4.668739246792323883, 19.56345983519973686 ) ) ;
#3902 = CARTESIAN_POINT ( 'NONE',  ( 0.1064266418746773329, 6.185136754498332223, -42.67882141624139081 ) ) ;
#3904 = ORIENTED_EDGE ( 'NONE', *, *, #6197, .F. ) ;
#3903 = CARTESIAN_POINT ( 'NONE',  ( 0.2285344041767085332, -35.80691465027930320, -25.77529890269112656 ) ) ;
#3905 = ORIENTED_EDGE ( 'NONE', *, *, #30816, .F. ) ;
#3906 = CONICAL_SURFACE ( 'NONE', #27944, 42.08604991992415023, 1.569615340895231137 ) ;
#3907 = CARTESIAN_POINT ( 'NONE',  ( 2.526552050251861914, -31.23611603144884441, 29.52128340070590085 ) ) ;
#3908 = CARTESIAN_POINT ( 'NONE',  ( 0.1103744047535531458, 39.82693656558409856, 16.53879706351786893 ) ) ;
#3909 = CARTESIAN_POINT ( 'NONE',  ( 2.618530812446115519, -41.30116959783759256, 22.44861196263268255 ) ) ;
#3910 = ORIENTED_EDGE ( 'NONE', *, *, #36823, .T. ) ;
#3911 = CARTESIAN_POINT ( 'NONE',  ( 0.8753041380234471980, 48.36002538446257404, -8.511537621788180630 ) ) ;
#3912 = CARTESIAN_POINT ( 'NONE',  ( 0.6067099128993252988, -23.33192673707561227, 41.82996792600769709 ) ) ;
#3913 = CARTESIAN_POINT ( 'NONE',  ( 0.6254311100348628472, -29.82834996731721233, 37.74260849418442376 ) ) ;
#3914 =( BOUNDED_SURFACE ( )  B_SPLINE_SURFACE ( 3, 1, ( 
 ( #59417, #45979 ),
 ( #26532, #21527 ),
 ( #31233, #1783 ),
 ( #30604, #41275 ) ),
 .UNSPECIFIED., .F., .F., .F. ) 
 B_SPLINE_SURFACE_WITH_KNOTS ( ( 4, 4 ),
 ( 2, 2 ),
 ( 0.000000000000000000, 1.000000000000000000 ),
 ( 0.000000000000000000, 1.000000000000000000 ),
 .UNSPECIFIED. ) 
 GEOMETRIC_REPRESENTATION_ITEM ( )  RATIONAL_B_SPLINE_SURFACE ( (
 ( 1.000000000000000000, 1.000000000000000000),
 ( 0.9952954269826590483, 0.8620686068821307169),
 ( 0.9952954269826590483, 0.8620686068821307169),
 ( 1.000000000000000000, 1.000000000000000000) ) ) 
 REPRESENTATION_ITEM ( '' )  SURFACE ( )  );
#3915 = VERTEX_POINT ( 'NONE', #37306 ) ;
#3916 = ORIENTED_EDGE ( 'NONE', *, *, #21348, .F. ) ;
#3917 = ADVANCED_FACE ( 'NONE', ( #13495 ), #43759, .F. ) ;
#3918 = CARTESIAN_POINT ( 'NONE',  ( 0.9754642270333709897, 41.40054989430073817, 11.27515941577587277 ) ) ;
#3919 = CARTESIAN_POINT ( 'NONE',  ( 1.112077966505211402, 37.50506094480364538, 23.16032660942239474 ) ) ;
#3920 = CARTESIAN_POINT ( 'NONE',  ( 0.6023142530420679819, 41.79260242564367189, 23.82662387835881646 ) ) ;
#3921 = CARTESIAN_POINT ( 'NONE',  ( 0.8744876279028306332, -47.70753782033967383, -11.59055156152427557 ) ) ;
#3922 = CARTESIAN_POINT ( 'NONE',  ( 4.975610109902397937, 25.84633036597884725, -41.52609557555889808 ) ) ;
#3923 =( BOUNDED_SURFACE ( )  B_SPLINE_SURFACE ( 3, 1, ( 
 ( #44112, #5219 ),
 ( #38467, #43800 ),
 ( #19980, #39092 ),
 ( #52533, #14658 ) ),
 .UNSPECIFIED., .F., .F., .F. ) 
 B_SPLINE_SURFACE_WITH_KNOTS ( ( 4, 4 ),
 ( 2, 2 ),
 ( 0.000000000000000000, 1.000000000000000000 ),
 ( 0.000000000000000000, 1.000000000000000000 ),
 .UNSPECIFIED. ) 
 GEOMETRIC_REPRESENTATION_ITEM ( )  RATIONAL_B_SPLINE_SURFACE ( (
 ( 1.000000000000000000, 1.000000000000000000),
 ( 0.9732289882329797637, 0.9999525324661233672),
 ( 0.9732289882329797637, 0.9999525324661233672),
 ( 1.000000000000000000, 1.000000000000000000) ) ) 
 REPRESENTATION_ITEM ( '' )  SURFACE ( )  );
#3924 = ORIENTED_EDGE ( 'NONE', *, *, #24771, .F. ) ;
#3925 = CARTESIAN_POINT ( 'NONE',  ( -2.601141883200665639, -12.22474371604808496, 8.564523836520711697 ) ) ;
#3926 = CARTESIAN_POINT ( 'NONE',  ( 4.967162193818130511, -2.375726030842277403, -43.02067033766020643 ) ) ;
#3927 = VERTEX_POINT ( 'NONE', #51994 ) ;
#3928 = CARTESIAN_POINT ( 'NONE',  ( 0.6009452777970413218, -47.75105029762388398, -5.846392105360362912 ) ) ;
#3929 = CARTESIAN_POINT ( 'NONE',  ( 0.8753041380234530822, 44.61941359694259290, 20.49990873486889598 ) ) ;
#3930 = CARTESIAN_POINT ( 'NONE',  ( 0.9788927965476029724, 4.053859047820351336, -41.71214259004423752 ) ) ;
#3931 = CARTESIAN_POINT ( 'NONE',  ( 1.231276596079887264, 32.36747132271594296, -26.63876069172940930 ) ) ;
#3932 = ORIENTED_EDGE ( 'NONE', *, *, #4714, .F. ) ;
#3933 = ORIENTED_EDGE ( 'NONE', *, *, #32790, .F. ) ;
#3934 = CARTESIAN_POINT ( 'NONE',  ( 5.960721111146673579, 7.860635756377893912, -18.96073515164540879 ) ) ;
#3935 = CARTESIAN_POINT ( 'NONE',  ( 0.5832366564991491309, 41.61464700196777500, 23.71163571971538886 ) ) ;
#3936 = CARTESIAN_POINT ( 'NONE',  ( 4.960386119450139297, -3.911092338299068327, 43.57912139308960064 ) ) ;
#3937 = AXIS2_PLACEMENT_3D ( 'NONE', #59230, #49229, #44260 ) ;
#3938 =( REPRESENTATION_RELATIONSHIP ('NONE','NONE', #44881, #53251 ) REPRESENTATION_RELATIONSHIP_WITH_TRANSFORMATION ( #34910 )SHAPE_REPRESENTATION_RELATIONSHIP( ) );
#3939 = ORIENTED_EDGE ( 'NONE', *, *, #30256, .F. ) ;
#3940 = CARTESIAN_POINT ( 'NONE',  ( 1.092182651088184242, -39.84386646767028850, -13.00874664788052115 ) ) ;
#3941 = EDGE_CURVE ( 'NONE', #3856, #8543, #3148, .T. ) ;
#3942 = ORIENTED_EDGE ( 'NONE', *, *, #6996, .T. ) ;
#3943 = CARTESIAN_POINT ( 'NONE',  ( 0.6041374136657475802, 0.1745662470644584741, -48.10739871142803992 ) ) ;
#3944 = DIRECTION ( 'NONE',  ( -1.000000000000000000, -0.000000000000000000, -0.000000000000000000 ) ) ;
#3945 = CIRCLE ( 'NONE', #30977, 43.08621763946400307 ) ;
#3946 = CARTESIAN_POINT ( 'NONE',  ( 0.1145239942831223490, 37.15712298330992525, -23.79692611048441364 ) ) ;
#3947 = ORIENTED_EDGE ( 'NONE', *, *, #51571, .T. ) ;
#3948 = CARTESIAN_POINT ( 'NONE',  ( 0.5836750258453354823, -47.46217286060748108, -6.431686642655249031 ) ) ;
#3949 = EDGE_CURVE ( 'NONE', #3021, #31508, #39791, .T. ) ;
#3950 = CARTESIAN_POINT ( 'NONE',  ( 0.1145239942831223490, -27.76557412857819429, 34.29312429649860405 ) ) ;
#3951 = CARTESIAN_POINT ( 'NONE',  ( 0.5804410086790514622, 42.96136033320046010, 18.81067170986478487 ) ) ;
#3952 = VERTEX_POINT ( 'NONE', #27893 ) ;
#3953 = CARTESIAN_POINT ( 'NONE',  ( 4.956653778116991482, -14.93973939759855263, -45.71126949320266419 ) ) ;
#3954 = FACE_OUTER_BOUND ( 'NONE', #11802, .T. ) ;
#3955 = CARTESIAN_POINT ( 'NONE',  ( -6.016104459813371719, 17.40682403289259028, -7.215917642688879141 ) ) ;
#3956 = CARTESIAN_POINT ( 'NONE',  ( 0.1100247026804066219, 26.38690693952957034, -34.10937070541719152 ) ) ;
#3957 = B_SPLINE_CURVE_WITH_KNOTS ( 'NONE', 3,
 ( #34630, #57164, #28373, #154, #57467, #47494 ),
 .UNSPECIFIED., .F., .F.,
 ( 4, 2, 4 ),
 ( 7.023086426956682172E-18, 0.0002448709889506543377, 0.0004897419779013016282 ),
 .UNSPECIFIED. ) ;
#3958 = EDGE_LOOP ( 'NONE', ( #41079, #26700, #60785, #20842 ) ) ;
#3959 = CARTESIAN_POINT ( 'NONE',  ( 0.8760168074886960365, 23.27577685234539473, 42.09738177923962610 ) ) ;
#3960 = B_SPLINE_CURVE_WITH_KNOTS ( 'NONE', 3,
 ( #29309, #52181, #23384, #14307, #43129, #33414 ),
 .UNSPECIFIED., .F., .F.,
 ( 4, 2, 4 ),
 ( 7.023086426956682172E-18, 0.0002445244328975370771, 0.0004890488657950671069 ),
 .UNSPECIFIED. ) ;
#3961 = CARTESIAN_POINT ( 'NONE',  ( -5.995132425357893702, 18.68405145320027572, -2.451215106828155577 ) ) ;
#3962 = CONICAL_SURFACE ( 'NONE', #60003, 43.08621763946400307, 1.568696531533066763 ) ;
#3963 = ORIENTED_EDGE ( 'NONE', *, *, #11547, .T. ) ;
#3964 = CARTESIAN_POINT ( 'NONE',  ( 0.8557997880470697982, 38.55640757422439435, 28.43566216844983074 ) ) ;
#3965 = CARTESIAN_POINT ( 'NONE',  ( 0.9762797500689124330, -26.66896101499594707, 32.32787193067817810 ) ) ;
#3967 = EDGE_CURVE ( 'NONE', #14355, #59171, #24900, .T. ) ;
#3966 = DIRECTION ( 'NONE',  ( 0.07906939808003032866, 0.9752531043637134855, 0.2064689146486738125 ) ) ;
#3968 = CARTESIAN_POINT ( 'NONE',  ( 0.1129192098497447394, 19.97823103613683315, -39.34236993944178806 ) ) ;
#3969 = CARTESIAN_POINT ( 'NONE',  ( 4.956653778117001252, 47.94889704119056972, -3.690426056929486887 ) ) ;
#3970 = CARTESIAN_POINT ( 'NONE',  ( 4.549368137175248350, 13.59764261105751793, -40.71620287708331176 ) ) ;
#3971 = CARTESIAN_POINT ( 'NONE',  ( 0.5839879882012697365, -47.89596766821089346, 3.018602120542737986E-05 ) ) ;
#3972 = CARTESIAN_POINT ( 'NONE',  ( 0.8744876279028263033, -29.90976330662845939, -38.93271258621668096 ) ) ;
#3973 = DIRECTION ( 'NONE',  ( 1.000000000000000000, 1.836909530733573776E-16, 0.000000000000000000 ) ) ;
#3974 = FACE_OUTER_BOUND ( 'NONE', #38562, .T. ) ;
#3975 = DIRECTION ( 'NONE',  ( 0.000000000000000000, 0.000000000000000000, 1.000000000000000000 ) ) ;
#3976 = ORIENTED_EDGE ( 'NONE', *, *, #32612, .F. ) ;
#3977 = CARTESIAN_POINT ( 'NONE',  ( 0.2940133293163015304, 40.08987453976585158, -18.41310698833514792 ) ) ;
#3978 = FACE_OUTER_BOUND ( 'NONE', #18229, .T. ) ;
#3979 = CARTESIAN_POINT ( 'NONE',  ( 4.303969348037246512, 8.413118729224734693, -47.36875205922763143 ) ) ;
#3980 = CARTESIAN_POINT ( 'NONE',  ( 0.8751705887134423323, -48.08707113907595243, -0.8911681664086732457 ) ) ;
#3981 = CARTESIAN_POINT ( 'NONE',  ( 0.5806925824938494740, 46.54710689580857519, 5.708695295225819422 ) ) ;
#3982 = CARTESIAN_POINT ( 'NONE',  ( 3.727782113643636652, 32.05026110430742392, -30.09249971424265269 ) ) ;
#3983 = B_SPLINE_CURVE_WITH_KNOTS ( 'NONE', 3,
 ( #3243, #61186, #27376, #46499, #46197, #55876 ),
 .UNSPECIFIED., .F., .F.,
 ( 4, 2, 4 ),
 ( 1.202235021059306678E-16, 0.0002448718616795958068, 0.0004897437233590713757 ),
 .UNSPECIFIED. ) ;
#3984 = VERTEX_POINT ( 'NONE', #4052 ) ;
#3985 = CARTESIAN_POINT ( 'NONE',  ( 0.9741495583595157770, 11.48707840139643466, -41.34222751889817005 ) ) ;
#3986 = CARTESIAN_POINT ( 'NONE',  ( 2.879087469061463178, -32.78830311798584063, -29.34329319327431307 ) ) ;
#3987 = CARTESIAN_POINT ( 'NONE',  ( 4.390527457369401532, 27.64241534123164712, -34.14794592258018469 ) ) ;
#3988 = DIRECTION ( 'NONE',  ( 1.000000000000000000, 1.836909530733573776E-16, -1.925929944387235853E-32 ) ) ;
#3989 = VERTEX_POINT ( 'NONE', #42323 ) ;
#3990 = CARTESIAN_POINT ( 'NONE',  ( 4.691466044806102964, -14.64802401911257235, 42.11359095667464203 ) ) ;
#3991 = EDGE_CURVE ( 'NONE', #47069, #50438, #43933, .T. ) ;
#3992 = CARTESIAN_POINT ( 'NONE',  ( 0.6031357023905874470, 24.09149424676616391, -41.64046004335391871 ) ) ;
#3993 = ORIENTED_EDGE ( 'NONE', *, *, #54998, .F. ) ;
#3994 = CLOSED_SHELL ( 'NONE', ( #54130, #16326, #21800, #32420, #60555, #17854, #48300, #19035, #47503, #31319, #8760, #13309, #37233, #21166, #10050, #57395, #49127, #61148, #35906, #49288, #10186, #2080, #58713, #14983, #52657, #35997, #921, #30125, #26803, #27121 ) ) ;
#3995 = EDGE_CURVE ( 'NONE', #41370, #53492, #1673, .T. ) ;
#3996 = CARTESIAN_POINT ( 'NONE',  ( 0.5806925824938499181, 37.13995815321135296, -28.63295078613577971 ) ) ;
#3997 = VERTEX_POINT ( 'NONE', #31669 ) ;
#3998 = CARTESIAN_POINT ( 'NONE',  ( 0.5839879882104919151, -1.006200701304952040E-05, -47.89596766822081264 ) ) ;
#3999 = AXIS2_PLACEMENT_3D ( 'NONE', #37277, #47278, #4324 ) ;
#4000 = CARTESIAN_POINT ( 'NONE',  ( 5.959547316686252039, 14.51632612601508754, 14.51128755440546314 ) ) ;
#4001 = ORIENTED_EDGE ( 'NONE', *, *, #31684, .T. ) ;
#4002 = CARTESIAN_POINT ( 'NONE',  ( 0.8753041380234471980, 41.63161868429074985, -26.03740873433439162 ) ) ;
#4003 = CARTESIAN_POINT ( 'NONE',  ( 0.1101816497532063233, 26.36013219694225640, 34.13008584880301299 ) ) ;
#4004 = VERTEX_POINT ( 'NONE', #7853 ) ;
#4005 = CARTESIAN_POINT ( 'NONE',  ( 0.5837800304671212359, -7.755313095589508876, -46.25032379312472131 ) ) ;
#4006 = B_SPLINE_CURVE_WITH_KNOTS ( 'NONE', 3,
 ( #4506, #58667, #1350, #20486, #11097, #9857 ),
 .UNSPECIFIED., .F., .F.,
 ( 4, 2, 4 ),
 ( 8.274813951709019538E-19, 0.0002293801035737093178, 0.0004587602071474177682 ),
 .UNSPECIFIED. ) ;
#4007 = VERTEX_POINT ( 'NONE', #26972 ) ;
#4008 = CARTESIAN_POINT ( 'NONE',  ( 0.9788927965476035276, -7.110334182851104856, -41.30108667383892396 ) ) ;
#4009 = VERTEX_POINT ( 'NONE', #46100 ) ;
#4010 = CARTESIAN_POINT ( 'NONE',  ( 4.967162193818130511, 40.65506779172185503, -14.26841313271238221 ) ) ;
#4011 = ORIENTED_EDGE ( 'NONE', *, *, #13738, .F. ) ;
#4012 = EDGE_CURVE ( 'NONE', #32300, #17561, #55379, .T. ) ;
#4013 = ORIENTED_EDGE ( 'NONE', *, *, #28082, .F. ) ;
#4014 = CARTESIAN_POINT ( 'NONE',  ( 0.6027444965799114707, -42.72396661545605667, -24.21159211057460681 ) ) ;
#4015 = CARTESIAN_POINT ( 'NONE',  ( 0.6028618097248864549, -33.89350006451850561, 34.14037999462312456 ) ) ;
#4016 = CARTESIAN_POINT ( 'NONE',  ( 0.5998501479064699549, 44.64337787626223530, 17.92509395669123862 ) ) ;
#4017 = CARTESIAN_POINT ( 'NONE',  ( 0.2279481005628804513, -43.65339889723670552, -6.394079432697511223 ) ) ;
#4018 = ORIENTED_EDGE ( 'NONE', *, *, #12134, .T. ) ;
#4019 = CARTESIAN_POINT ( 'NONE',  ( 0.5980271706414734822, 4.018631420205467819, -48.94792992916248409 ) ) ;
#4020 = EDGE_CURVE ( 'NONE', #3387, #24101, #40936, .T. ) ;
#4021 = CARTESIAN_POINT ( 'NONE',  ( 4.833616638992205949, -26.07076047129164564, 38.20222678111891668 ) ) ;
#4022 = VERTEX_POINT ( 'NONE', #43553 ) ;
#4023 = EDGE_CURVE ( 'NONE', #41472, #56267, #57289, .T. ) ;
#4024 = EDGE_LOOP ( 'NONE', ( #28100, #44874 ) ) ;
#4025 =( BOUNDED_SURFACE ( )  B_SPLINE_SURFACE ( 3, 1, ( 
 ( #11605, #34486 ),
 ( #30074, #39828 ),
 ( #20995, #20689 ),
 ( #5932, #34180 ) ),
 .UNSPECIFIED., .F., .F., .F. ) 
 B_SPLINE_SURFACE_WITH_KNOTS ( ( 4, 4 ),
 ( 2, 2 ),
 ( 0.000000000000000000, 1.000000000000000000 ),
 ( 0.000000000000000000, 1.000000000000000000 ),
 .UNSPECIFIED. ) 
 GEOMETRIC_REPRESENTATION_ITEM ( )  RATIONAL_B_SPLINE_SURFACE ( (
 ( 1.000000000000000000, 1.000000000000000000),
 ( 0.9953040768229013402, 0.8617119497784988535),
 ( 0.9953040768229013402, 0.8617119497784988535),
 ( 1.000000000000000000, 1.000000000000000000) ) ) 
 REPRESENTATION_ITEM ( '' )  SURFACE ( )  );
#4026 = CARTESIAN_POINT ( 'NONE',  ( 3.270143674763207553, 13.68510027222513337, 0.2742231296310058686 ) ) ;
#4027 = CARTESIAN_POINT ( 'NONE',  ( 5.860006189529234355, 15.48781697582111327, -45.67886430272015730 ) ) ;
#4028 = CARTESIAN_POINT ( 'NONE',  ( 0.1084644655670283786, -33.96951444491441663, 26.56696682928998143 ) ) ;
#4029 = CYLINDRICAL_SURFACE ( 'NONE', #41805, 2.649999999999992806 ) ;
#4030 = ORIENTED_EDGE ( 'NONE', *, *, #20649, .T. ) ;
#4031 = CARTESIAN_POINT ( 'NONE',  ( 4.975610109902397937, 39.54077024310177535, -28.79195887257430897 ) ) ;
#4032 = CARTESIAN_POINT ( 'NONE',  ( 0.3622758884714600280, -11.95365414648526148, 41.42293301073604539 ) ) ;
#4034 = ADVANCED_FACE ( 'NONE', ( #39166 ), #56517, .F. ) ;
#4033 = CARTESIAN_POINT ( 'NONE',  ( 0.9785694773339266295, -41.11263117936924516, 8.129388859184128791 ) ) ;
#4035 = CARTESIAN_POINT ( 'NONE',  ( -2.739355103387248747, -13.13414140434190180, -7.095202359465781150 ) ) ;
#4036 = CARTESIAN_POINT ( 'NONE',  ( 3.559346040607745287, -41.48356477534394315, -14.57889347899322452 ) ) ;
#4037 = FILL_AREA_STYLE_COLOUR ( '', #22710 ) ;
#4038 = CARTESIAN_POINT ( 'NONE',  ( 0.5800708119828327236, -34.30831427709729553, -33.42085299104054741 ) ) ;
#4039 = CIRCLE ( 'NONE', #51088, 47.91270532121795611 ) ;
#4040 = EDGE_LOOP ( 'NONE', ( #56864, #30678, #8339, #46487 ) ) ;
#4041 = CARTESIAN_POINT ( 'NONE',  ( 3.660176727303073196, 47.34518114598545679, 8.130955556893987080 ) ) ;
#4042 = CARTESIAN_POINT ( 'NONE',  ( 4.834790513006555379, 40.94190515849784617, -23.58706728096878891 ) ) ;
#4043 = FACE_OUTER_BOUND ( 'NONE', #14161, .T. ) ;
#4044 = FACE_OUTER_BOUND ( 'NONE', #21656, .T. ) ;
#4045 = CARTESIAN_POINT ( 'NONE',  ( 0.9785694773339244090, 28.97418037048111827, 30.27923839156954955 ) ) ;
#4046 = CARTESIAN_POINT ( 'NONE',  ( -6.078075953587585900, 18.62492360731181407, -4.889518879085647640 ) ) ;
#4047 = CARTESIAN_POINT ( 'NONE',  ( 5.960721111146673579, 19.82781442290490403, 5.306302591836648652 ) ) ;
#4048 = CARTESIAN_POINT ( 'NONE',  ( 0.8751705887134423323, 44.76769609654235893, -17.57879340691497561 ) ) ;
#4049 = CARTESIAN_POINT ( 'NONE',  ( 5.901463166500146684, -13.99254106127013841, -14.44737571288660760 ) ) ;
#4050 = VERTEX_POINT ( 'NONE', #14423 ) ;
#4051 = EDGE_CURVE ( 'NONE', #41864, #46085, #40442, .T. ) ;
#4052 = CARTESIAN_POINT ( 'NONE',  ( 0.5809828226811617480, -41.74875432577665890, 23.47450554821694979 ) ) ;
#4053 = CARTESIAN_POINT ( 'NONE',  ( 3.559346040607745287, 23.44433175904301692, -37.19937620329021399 ) ) ;
#4054 = B_SPLINE_CURVE_WITH_KNOTS ( 'NONE', 3,
 ( #49275, #24868, #25465, #1337 ),
 .UNSPECIFIED., .F., .F.,
 ( 4, 4 ),
 ( 2.501853776554200607E-17, 0.005004741218457455301 ),
 .UNSPECIFIED. ) ;
#4055 = CARTESIAN_POINT ( 'NONE',  ( 3.782542959838395724, 40.05509967486248257, 12.76036219836252705 ) ) ;
#4056 = CARTESIAN_POINT ( 'NONE',  ( 1.499999999999999556, 5.100000000000000533, 0.000000000000000000 ) ) ;
#4057 = EDGE_LOOP ( 'NONE', ( #59854, #35436, #34264, #58108, #27155 ) ) ;
#4058 = ADVANCED_FACE ( 'NONE', ( #52605 ), #7283, .F. ) ;
#4059 = CARTESIAN_POINT ( 'NONE',  ( -6.010958268070873523, 4.891065400978385824, 18.19761767765831806 ) ) ;
#4060 = CARTESIAN_POINT ( 'NONE',  ( 0.6024113833632039894, 44.33830889028068611, -21.11057161355237000 ) ) ;
#4061 = B_SPLINE_CURVE_WITH_KNOTS ( 'NONE', 3,
 ( #40366, #10924, #25308, #54723 ),
 .UNSPECIFIED., .F., .F.,
 ( 4, 4 ),
 ( 0.000000000000000000, 0.005013413432710150247 ),
 .UNSPECIFIED. ) ;
#4062 = EDGE_CURVE ( 'NONE', #22341, #42399, #26994, .T. ) ;
#4063 = ORIENTED_EDGE ( 'NONE', *, *, #5152, .T. ) ;
#4064 = CARTESIAN_POINT ( 'NONE',  ( 4.975801465491695552, 0.000000000000000000, 0.000000000000000000 ) ) ;
#4065 = DIRECTION ( 'NONE',  ( 0.09722883295013594329, -0.7201826484181126364, -0.6869377751737254512 ) ) ;
#4066 = EDGE_CURVE ( 'NONE', #5305, #44819, #39472, .T. ) ;
#4067 = CARTESIAN_POINT ( 'NONE',  ( 4.833616638992205949, -8.578242093415418879, -45.44786513329594158 ) ) ;
#4068 = ORIENTED_EDGE ( 'NONE', *, *, #24947, .F. ) ;
#4069 = EDGE_CURVE ( 'NONE', #41171, #22554, #9879, .T. ) ;
#4070 = CARTESIAN_POINT ( 'NONE',  ( 4.956445790444031552, 30.81386304088997719, -35.60960396630257208 ) ) ;
#4071 = ORIENTED_EDGE ( 'NONE', *, *, #61372, .T. ) ;
#4072 = ORIENTED_EDGE ( 'NONE', *, *, #47899, .T. ) ;
#4073 = CARTESIAN_POINT ( 'NONE',  ( 0.5838002273316424962, -6.116619957188429879, -47.50378804015151957 ) ) ;
#4074 = DIRECTION ( 'NONE',  ( 0.09835009131224567436, -0.9855991218957022015, -0.1375559175655256539 ) ) ;
#4075 = ORIENTED_EDGE ( 'NONE', *, *, #846, .F. ) ;
#4076 = CARTESIAN_POINT ( 'NONE',  ( 5.960721111146673579, 20.52557019979492026, 0.006321279846891981850 ) ) ;
#4077 = ORIENTED_EDGE ( 'NONE', *, *, #31678, .T. ) ;
#4078 = FACE_OUTER_BOUND ( 'NONE', #1486, .T. ) ;
#4079 = CONICAL_SURFACE ( 'NONE', #58103, 42.08604991992415023, 1.569615340895231137 ) ;
#4080 = CARTESIAN_POINT ( 'NONE',  ( 4.956653778116966613, 0.000000000000000000, 0.000000000000000000 ) ) ;
#4081 = CARTESIAN_POINT ( 'NONE',  ( 5.965394784446458765, -18.95742317323950843, 7.868087674480618965 ) ) ;
#4082 = EDGE_CURVE ( 'NONE', #46482, #1947, #14121, .T. ) ;
#4083 = VERTEX_POINT ( 'NONE', #52293 ) ;
#4084 = FACE_OUTER_BOUND ( 'NONE', #33964, .T. ) ;
#4085 = CARTESIAN_POINT ( 'NONE',  ( 4.967162193818130511, -42.96271701169388280, 3.259922920617591924 ) ) ;
#4086 = CARTESIAN_POINT ( 'NONE',  ( 0.1149546198390367646, -22.63900799641087147, -37.87376244792249480 ) ) ;
#4087 = ORIENTED_EDGE ( 'NONE', *, *, #45623, .F. ) ;
#4088 = EDGE_CURVE ( 'NONE', #21034, #9246, #47198, .T. ) ;
#4089 = CARTESIAN_POINT ( 'NONE',  ( 0.5819845079324653669, 44.42187385013365031, 17.90867223323903445 ) ) ;
#4090 = CARTESIAN_POINT ( 'NONE',  ( 0.7954196712028460681, 29.96539649507085201, -37.62416450255258837 ) ) ;
#4091 = ORIENTED_EDGE ( 'NONE', *, *, #35439, .F. ) ;
#4092 = CARTESIAN_POINT ( 'NONE',  ( 4.549368137175248350, 0.000000000000000000, 0.000000000000000000 ) ) ;
#4093 = EDGE_CURVE ( 'NONE', #13939, #43595, #2132, .T. ) ;
#4094 =( BOUNDED_SURFACE ( )  B_SPLINE_SURFACE ( 3, 1, ( 
 ( #47441, #28944 ),
 ( #9840, #37761 ),
 ( #33049, #58041 ),
 ( #56819, #13948 ) ),
 .UNSPECIFIED., .F., .F., .F. ) 
 B_SPLINE_SURFACE_WITH_KNOTS ( ( 4, 4 ),
 ( 2, 2 ),
 ( 0.000000000000000000, 1.000000000000000000 ),
 ( 0.000000000000000000, 1.000000000000000000 ),
 .UNSPECIFIED. ) 
 GEOMETRIC_REPRESENTATION_ITEM ( )  RATIONAL_B_SPLINE_SURFACE ( (
 ( 1.000000000000000000, 1.000000000000000000),
 ( 0.7211978278499970862, 0.9934217856018976445),
 ( 0.7211978278499970862, 0.9934217856018976445),
 ( 1.000000000000000000, 1.000000000000000000) ) ) 
 REPRESENTATION_ITEM ( '' )  SURFACE ( )  );
#4095 = ORIENTED_EDGE ( 'NONE', *, *, #6123, .T. ) ;
#4096 = B_SPLINE_CURVE_WITH_KNOTS ( 'NONE', 3,
 ( #42262, #26906, #61321, #32228 ),
 .UNSPECIFIED., .F., .F.,
 ( 4, 4 ),
 ( 4.336808689942017736E-19, 0.004048833967417085622 ),
 .UNSPECIFIED. ) ;
#4097 = DIRECTION ( 'NONE',  ( -0.5000000000000051070, 1.060575238724903217E-16, -0.8660254037844355990 ) ) ;
#4098 = CARTESIAN_POINT ( 'NONE',  ( 0.6846871229502932144, -23.20185915381527408, -41.91507847151822119 ) ) ;
#4099 = VERTEX_POINT ( 'NONE', #20655 ) ;
#4100 = CARTESIAN_POINT ( 'NONE',  ( 4.963659409799330291, 8.262218268421102962, -43.98510776953393986 ) ) ;
#4101 = CARTESIAN_POINT ( 'NONE',  ( 5.960721111146673579, 14.51823969584079599, 14.50930005615021656 ) ) ;
#4102 = CARTESIAN_POINT ( 'NONE',  ( 4.956445790444035104, 38.51510088324747016, -27.09474218539284252 ) ) ;
#4103 = ORIENTED_EDGE ( 'NONE', *, *, #42824, .F. ) ;
#4104 = FACE_OUTER_BOUND ( 'NONE', #53464, .T. ) ;
#4105 = CARTESIAN_POINT ( 'NONE',  ( 2.624215991343620935, -43.79392271049083263, 19.66774719432963892 ) ) ;
#4106 = CARTESIAN_POINT ( 'NONE',  ( 0.7242486021783848260, -26.15101222305781192, 41.55882604313377726 ) ) ;
#4107 = B_SPLINE_CURVE_WITH_KNOTS ( 'NONE', 3,
 ( #18239, #17935, #26697, #32645 ),
 .UNSPECIFIED., .F., .F.,
 ( 4, 4 ),
 ( 7.376145397762941244E-17, 0.005004741218457468312 ),
 .UNSPECIFIED. ) ;
#4109 = ADVANCED_FACE ( 'NONE', ( #6831, #16573 ), #6510, .F. ) ;
#4108 = CARTESIAN_POINT ( 'NONE',  ( 5.896782393890504181, 10.81700609697900894, -16.95636948099241792 ) ) ;
#4110 = FACE_OUTER_BOUND ( 'NONE', #56973, .T. ) ;
#4111 = CARTESIAN_POINT ( 'NONE',  ( -6.057079549204054558, 5.470993133660444485, 18.46346298046979939 ) ) ;
#4112 = EDGE_CURVE ( 'NONE', #21617, #16942, #53162, .T. ) ;
#4113 = CARTESIAN_POINT ( 'NONE',  ( 0.6041374136657476912, -29.42442150067172335, -38.05989626241419899 ) ) ;
#4114 = LINE ( 'NONE', #56439, #53863 ) ;
#4115 = B_SPLINE_CURVE_WITH_KNOTS ( 'NONE', 3,
 ( #20433, #6599, #39563, #54225, #1608, #24827 ),
 .UNSPECIFIED., .F., .F.,
 ( 4, 2, 4 ),
 ( 2.538052214298621590E-18, 0.0002447193893791693286, 0.0004894387787583360551 ),
 .UNSPECIFIED. ) ;
#4116 = CARTESIAN_POINT ( 'NONE',  ( 0.5806925824938502512, 40.06810415365508504, -24.36738377166110325 ) ) ;
#4117 = CARTESIAN_POINT ( 'NONE',  ( 0.1064266379913939298, -37.06314005629928232, 22.04679939086769380 ) ) ;
#4118 = CARTESIAN_POINT ( 'NONE',  ( 0.9722240750034584211, 33.68410530487908261, -26.58024222649010682 ) ) ;
#4119 = CARTESIAN_POINT ( 'NONE',  ( 0.1100053167205931326, -21.40663161101019796, 37.43629428538725534 ) ) ;
#4120 = CARTESIAN_POINT ( 'NONE',  ( 0.6041374136657476912, 29.42442150067147821, 38.05989626241439794 ) ) ;
#4121 = AXIS2_PLACEMENT_3D ( 'NONE', #29998, #53777, #5853 ) ;
#4122 = CARTESIAN_POINT ( 'NONE',  ( 1.227938101723756947, -33.52879263017882039, 26.79402671879314823 ) ) ;
#4123 = LINE ( 'NONE', #38006, #35901 ) ;
#4124 = AXIS2_PLACEMENT_3D ( 'NONE', #50604, #51840, #51526 ) ;
#4125 = CARTESIAN_POINT ( 'NONE',  ( -6.016761891674564211, 16.32039929810256851, 9.418621820384554866 ) ) ;
#4126 = LINE ( 'NONE', #52365, #6213 ) ;
#4127 = CARTESIAN_POINT ( 'NONE',  ( 0.1129192098497447394, 20.83764143887560749, 38.89401608281161060 ) ) ;
#4129 = VERTEX_POINT ( 'NONE', #20964 ) ;
#4128 = CARTESIAN_POINT ( 'NONE',  ( 4.975610109902397937, -40.67634447773578898, -27.16402781375298403 ) ) ;
#4130 = CARTESIAN_POINT ( 'NONE',  ( 4.999999999999997335, 9.184547653667862963E-16, -9.629649721936174886E-32 ) ) ;
#4131 = CARTESIAN_POINT ( 'NONE',  ( 0.5832367798473382381, 23.71165515427716031, 41.61463593465314403 ) ) ;
#4132 = DIRECTION ( 'NONE',  ( -0.1011922191286467460, 0.9655114622251724787, -0.2398911234281693727 ) ) ;
#4133 = ORIENTED_EDGE ( 'NONE', *, *, #25324, .F. ) ;
#4134 = EDGE_CURVE ( 'NONE', #9388, #59309, #7554, .T. ) ;
#4135 = ORIENTED_EDGE ( 'NONE', *, *, #35118, .T. ) ;
#4136 = DIRECTION ( 'NONE',  ( -1.000000000000000000, -0.000000000000000000, -0.000000000000000000 ) ) ;
#4137 = CARTESIAN_POINT ( 'NONE',  ( 4.956653778116480780, -21.75875759808806720, 42.88673967249081898 ) ) ;
#4138 = B_SPLINE_CURVE_WITH_KNOTS ( 'NONE', 3,
 ( #47300, #38778, #18488, #9079 ),
 .UNSPECIFIED., .F., .F.,
 ( 4, 4 ),
 ( 0.000000000000000000, 0.005014147105413699519 ),
 .UNSPECIFIED. ) ;
#4139 = EDGE_CURVE ( 'NONE', #2726, #15046, #12815, .T. ) ;
#4140 = UNCERTAINTY_MEASURE_WITH_UNIT (LENGTH_MEASURE( 1.000000000000000082E-05 ), #18478, 'distance_accuracy_value', 'NONE');
#4141 = ORIENTED_EDGE ( 'NONE', *, *, #15136, .T. ) ;
#4142 = ORIENTED_EDGE ( 'NONE', *, *, #56953, .T. ) ;
#4143 = B_SPLINE_CURVE_WITH_KNOTS ( 'NONE', 3,
 ( #259, #57894, #38523, #33821 ),
 .UNSPECIFIED., .F., .F.,
 ( 4, 4 ),
 ( 2.148040924471974165E-17, 0.004559932413162187670 ),
 .UNSPECIFIED. ) ;
#4144 = CARTESIAN_POINT ( 'NONE',  ( 0.6031357023905875581, -38.13964912630314075, -29.32055886552309332 ) ) ;
#4145 = ADVANCED_FACE ( 'NONE', ( #31286 ), #13739, .F. ) ;
#4146 = ADVANCED_FACE ( 'NONE', ( #37241 ), #45758, .F. ) ;
#4147 = DIRECTION ( 'NONE',  ( 0.000000000000000000, 0.000000000000000000, 1.000000000000000000 ) ) ;
#4148 = CARTESIAN_POINT ( 'NONE',  ( 0.5997462898726536595, 48.97040376101512749, 3.667585803694950464 ) ) ;
#4149 = ADVANCED_FACE ( 'NONE', ( #50997 ), #27264, .F. ) ;
#4150 = ORIENTED_EDGE ( 'NONE', *, *, #38097, .F. ) ;
#4151 = ORIENTED_EDGE ( 'NONE', *, *, #33324, .F. ) ;
#4152 = CARTESIAN_POINT ( 'NONE',  ( 0.5827357941260206120, -12.74691551863599059, -46.16863402900294489 ) ) ;
#4153 = ORIENTED_EDGE ( 'NONE', *, *, #23919, .F. ) ;
#4154 = DIRECTION ( 'NONE',  ( 0.1024043820194936311, -0.2701391291102787640, -0.9573600124648750098 ) ) ;
#4155 = CARTESIAN_POINT ( 'NONE',  ( 0.1368894036331276542, 9.195786968782886817, -43.15436047432628186 ) ) ;
#4156 = VERTEX_POINT ( 'NONE', #51609 ) ;
#4157 = ADVANCED_FACE ( 'NONE', ( #13124 ), #33679, .F. ) ;
#4158 = CARTESIAN_POINT ( 'NONE',  ( 0.9791128995231619392, -39.58816053567403515, 13.75190821842056543 ) ) ;
#4159 = ORIENTED_EDGE ( 'NONE', *, *, #51197, .F. ) ;
#4160 = ORIENTED_EDGE ( 'NONE', *, *, #15560, .F. ) ;
#4161 = CARTESIAN_POINT ( 'NONE',  ( 0.1129192098497455998, -12.08918212651712132, -42.43587472053631160 ) ) ;
#4162 = ORIENTED_EDGE ( 'NONE', *, *, #8999, .T. ) ;
#4163 = CARTESIAN_POINT ( 'NONE',  ( 1.657374760986086271, 34.33505663815240183, 27.60424483493635606 ) ) ;
#4164 = CARTESIAN_POINT ( 'NONE',  ( 5.880360259849739535, -3.090325311465197178, 47.87242051977160173 ) ) ;
#4165 = CARTESIAN_POINT ( 'NONE',  ( 0.9762797500689124330, -0.8945891712305065191, 41.89897964629235361 ) ) ;
#4166 = FACE_OUTER_BOUND ( 'NONE', #41028, .T. ) ;
#4167 = CARTESIAN_POINT ( 'NONE',  ( 5.895596859100789899, 16.57987064389762111, 11.38578379577399069 ) ) ;
#4168 = ORIENTED_EDGE ( 'NONE', *, *, #35231, .T. ) ;
#4169 = CARTESIAN_POINT ( 'NONE',  ( 4.962356264823608143, 0.000000000000000000, 0.000000000000000000 ) ) ;
#4170 = VECTOR ( 'NONE', #22264, 1000.000000000000227 ) ;
#4171 = CARTESIAN_POINT ( 'NONE',  ( 0.9730545539215883499, 6.101350888305258735, -42.47233286818610054 ) ) ;
#4172 = VECTOR ( 'NONE', #48172, 1000.000000000000000 ) ;
#4173 = DIRECTION ( 'NONE',  ( -1.000000000000000000, -1.836909530733573776E-16, 1.925929944387234758E-32 ) ) ;
#4174 = ORIENTED_EDGE ( 'NONE', *, *, #20872, .T. ) ;
#4175 = CARTESIAN_POINT ( 'NONE',  ( 4.956445790443993360, 20.31112743693043399, 42.48524629068788983 ) ) ;
#4176 = CARTESIAN_POINT ( 'NONE',  ( 0.5804410086790514622, -8.338934868871040962, 46.15172821366631695 ) ) ;
#4177 = CARTESIAN_POINT ( 'NONE',  ( 3.050102900204245682, -5.228472987645193193, 43.68167029081563868 ) ) ;
#4178 = VERTEX_POINT ( 'NONE', #46032 ) ;
#4179 = ORIENTED_EDGE ( 'NONE', *, *, #16249, .T. ) ;
#4180 = CARTESIAN_POINT ( 'NONE',  ( 4.960156602257182357, 46.28683144126601690, -3.546989772329427915 ) ) ;
#4181 = CARTESIAN_POINT ( 'NONE',  ( 0.8554163680231708922, 21.74163052365331694, 41.57531689939074226 ) ) ;
#4182 = DIRECTION ( 'NONE',  ( 0.000000000000000000, 0.000000000000000000, -1.000000000000000000 ) ) ;
#4183 = CARTESIAN_POINT ( 'NONE',  ( 0.9756008150404585910, -42.52260101821271121, 5.741579752919493629 ) ) ;
#4184 = CARTESIAN_POINT ( 'NONE',  ( 5.981074661064941900, 10.26976685693823121, -17.77058762078867460 ) ) ;
#4185 = CARTESIAN_POINT ( 'NONE',  ( 5.960721111146673579, -5.318514366755071165, 19.82454228767736382 ) ) ;
#4186 = EDGE_CURVE ( 'NONE', #61767, #17579, #41328, .T. ) ;
#4187 = CARTESIAN_POINT ( 'NONE',  ( -6.079354080745853928, -8.907665152502719508, -17.07180297388212864 ) ) ;
#4188 = CARTESIAN_POINT ( 'NONE',  ( 4.291220156522060236, 39.39367666905506127, -25.83654844981511189 ) ) ;
#4189 = B_SPLINE_CURVE_WITH_KNOTS ( 'NONE', 3,
 ( #21793, #12403, #17101, #31490 ),
 .UNSPECIFIED., .F., .F.,
 ( 4, 4 ),
 ( 4.336808689942017736E-19, 0.004041751736740989073 ),
 .UNSPECIFIED. ) ;
#4190 = CARTESIAN_POINT ( 'NONE',  ( 2.643462169533613793, -4.896978544602504257, 47.78621045426866232 ) ) ;
#4191 = FACE_BOUND ( 'NONE', #45738, .T. ) ;
#4192 = ORIENTED_EDGE ( 'NONE', *, *, #22081, .T. ) ;
#4193 = LINE ( 'NONE', #33664, #46941 ) ;
#4194 = CARTESIAN_POINT ( 'NONE',  ( -6.079354080745853928, 0.6160181061929859148, 19.24612888195972715 ) ) ;
#4195 = CARTESIAN_POINT ( 'NONE',  ( 0.7048096507298579061, 29.95256433478725455, -37.64898672361922394 ) ) ;
#4196 = LINE ( 'NONE', #12718, #33024 ) ;
#4197 = B_SPLINE_CURVE_WITH_KNOTS ( 'NONE', 3,
 ( #28418, #19055, #33458, #47548, #53147, #9627, #9316, #23733, #19662, #38168, #10255, #43170, #24040, #204, #14970, #19351, #48455, #57522, #5824 ),
 .UNSPECIFIED., .F., .F.,
 ( 4, 3, 3, 3, 3, 3, 4 ),
 ( 5.204170427930420513E-18, 0.0002724573126191753760, 0.0004086839781548465798, 0.0005449106435901828957, 0.0006811373090491458200, 0.0008459866663933683986, 0.001010840725717211848 ),
 .UNSPECIFIED. ) ;
#4198 = CARTESIAN_POINT ( 'NONE',  ( 4.975801465491695552, 45.18341283946458020, -15.94009207553003016 ) ) ;
#4199 = CARTESIAN_POINT ( 'NONE',  ( 0.5980894510889448457, 44.17723055703925183, 19.05812566676522124 ) ) ;
#4200 = ITEM_DEFINED_TRANSFORMATION ( 'NONE', 'NONE', #61872,  #14677 ) ;
#4201 = CARTESIAN_POINT ( 'NONE',  ( 0.5837799406558226156, -25.15713538965591667, 39.57729258759022883 ) ) ;
#4202 = CARTESIAN_POINT ( 'NONE',  ( -4.467300000000000715, 0.000000000000000000, 0.000000000000000000 ) ) ;
#4203 = CARTESIAN_POINT ( 'NONE',  ( 0.6039202388192952409, -42.87364092186839315, 23.94607748571118933 ) ) ;
#4205 = ORIENTED_EDGE ( 'NONE', *, *, #8467, .T. ) ;
#4204 = CARTESIAN_POINT ( 'NONE',  ( 0.8751705887134423323, 42.09020928323375443, -23.27176129838382224 ) ) ;
#4206 = ORIENTED_EDGE ( 'NONE', *, *, #42033, .T. ) ;
#4207 = CARTESIAN_POINT ( 'NONE',  ( 0.1140933569871964703, -7.416386428228847194, 43.49651896912084226 ) ) ;
#4208 = CARTESIAN_POINT ( 'NONE',  ( 0.8753041380234530822, -6.957149426674413384, 48.60798699522440813 ) ) ;
#4209 = CARTESIAN_POINT ( 'NONE',  ( 5.880360259849752858, 36.09847387447859290, -31.59460303415945148 ) ) ;
#4210 = EDGE_CURVE ( 'NONE', #31513, #22365, #799, .T. ) ;
#4211 = ORIENTED_EDGE ( 'NONE', *, *, #15130, .T. ) ;
#4212 = CARTESIAN_POINT ( 'NONE',  ( 0.5997462898726536595, 10.41743419021343087, -47.98988117339822423 ) ) ;
#4213 = CARTESIAN_POINT ( 'NONE',  ( 0.2500000000000002220, 0.000000000000000000, 4.250000000000000000 ) ) ;
#4214 = CARTESIAN_POINT ( 'NONE',  ( 0.6023142530420679819, -44.54505940664473940, -18.16775455049929988 ) ) ;
#4215 = CIRCLE ( 'NONE', #13240, 42.92674063221959813 ) ;
#4216 = EDGE_CURVE ( 'NONE', #28210, #16902, #1561, .T. ) ;
#4217 = VECTOR ( 'NONE', #23916, 1000.000000000000000 ) ;
#4218 = B_SPLINE_CURVE_WITH_KNOTS ( 'NONE', 3,
 ( #38322, #28276, #18282, #14206, #22981, #19212, #56466, #13582, #4144, #32686, #27978, #47100, #23282, #52380, #33308, #42408 ),
 .UNSPECIFIED., .F., .F.,
 ( 4, 3, 3, 3, 3, 4 ),
 ( 1.962735358247463844E-17, 0.0002618515315864410552, 0.0003927756766341956060, 0.0005236998216950555047, 0.0007855159896329858872, 0.001047349442285930472 ),
 .UNSPECIFIED. ) ;
#4219 = ORIENTED_EDGE ( 'NONE', *, *, #58747, .F. ) ;
#4220 = VERTEX_POINT ( 'NONE', #7036 ) ;
#4221 = ADVANCED_FACE ( 'NONE', ( #22092 ), #31172, .F. ) ;
#4222 = CARTESIAN_POINT ( 'NONE',  ( 0.9769922540276039236, 25.21368293196807286, -33.47539018581124282 ) ) ;
#4223 = ADVANCED_FACE ( 'NONE', ( #35896 ), #20132, .F. ) ;
#4224 = CARTESIAN_POINT ( 'NONE',  ( 0.5786265663353196143, -17.66171603226047182, -44.52624106864163167 ) ) ;
#4225 = CARTESIAN_POINT ( 'NONE',  ( 0.1119899015040010243, 14.71105729511424087, 41.59983294981330459 ) ) ;
#4226 = EDGE_CURVE ( 'NONE', #21310, #593, #21781, .T. ) ;
#4227 = CARTESIAN_POINT ( 'NONE',  ( 4.958415959904823644, -45.08182420577205818, -5.552754280760447969 ) ) ;
#4228 = B_SPLINE_CURVE_WITH_KNOTS ( 'NONE', 3,
 ( #9662, #18154, #9353, #24383 ),
 .UNSPECIFIED., .F., .F.,
 ( 4, 4 ),
 ( 4.336808689942017736E-19, 0.004446298630425045070 ),
 .UNSPECIFIED. ) ;
#4229 = CARTESIAN_POINT ( 'NONE',  ( 0.1313383488274116884, 10.54394128763557781, -41.81465294768275243 ) ) ;
#4230 = CARTESIAN_POINT ( 'NONE',  ( 0.1152339509894530906, 33.74256222853660603, 28.43206261790687961 ) ) ;
#4231 = VERTEX_POINT ( 'NONE', #7657 ) ;
#4232 = CARTESIAN_POINT ( 'NONE',  ( 4.956445790444005794, -33.12351118015950391, -33.47194433010255921 ) ) ;
#4233 = ADVANCED_FACE ( 'NONE', ( #30240 ), #52126, .F. ) ;
#4234 = FACE_OUTER_BOUND ( 'NONE', #18941, .T. ) ;
#4235 = B_SPLINE_CURVE_WITH_KNOTS ( 'NONE', 3,
 ( #48146, #58432, #38451, #44692, #1124, #14956, #49363, #43783, #29952, #34663, #15867, #20263, #10235, #39378, #15252, #53128 ),
 .UNSPECIFIED., .F., .F.,
 ( 4, 3, 3, 3, 3, 4 ),
 ( 2.501947744657918636E-17, 0.0002612764279487730544, 0.0003919131003184758298, 0.0005225497727000631958, 0.0007837925190632400417, 0.001045051706266714566 ),
 .UNSPECIFIED. ) ;
#4236 = EDGE_LOOP ( 'NONE', ( #11283, #12412 ) ) ;
#4237 = CARTESIAN_POINT ( 'NONE',  ( 0.1156495703730067576, 41.83314862904525455, -14.03319739087566731 ) ) ;
#4238 = CARTESIAN_POINT ( 'NONE',  ( 5.960721111146673579, 20.52557019979492026, -0.006321279846608376246 ) ) ;
#4239 = CARTESIAN_POINT ( 'NONE',  ( 0.9791128995231609400, 4.189801958621016453, -41.69871693222346209 ) ) ;
#4240 = CARTESIAN_POINT ( 'NONE',  ( 3.783198216974394068, -18.05208553945175254, 39.06945274417385860 ) ) ;
#4241 = EDGE_CURVE ( 'NONE', #9401, #20518, #21004, .T. ) ;
#4242 = ORIENTED_EDGE ( 'NONE', *, *, #20097, .T. ) ;
#4243 = ORIENTED_EDGE ( 'NONE', *, *, #22486, .F. ) ;
#4244 = CARTESIAN_POINT ( 'NONE',  ( 0.1157506346131639274, -44.12405299995102581, 0.09277208818792900824 ) ) ;
#4245 = CARTESIAN_POINT ( 'NONE',  ( 4.975801465491695552, -39.51822597168514051, 27.09127437476313816 ) ) ;
#4246 = DIRECTION ( 'NONE',  ( 0.09722883295013594329, -0.03945211390406794250, -0.9944798061055111216 ) ) ;
#4247 = ORIENTED_EDGE ( 'NONE', *, *, #59597, .T. ) ;
#4248 = CARTESIAN_POINT ( 'NONE',  ( 0.6001305935487422083, -46.60388846085731274, 11.94532529598298964 ) ) ;
#4249 = ORIENTED_EDGE ( 'NONE', *, *, #54835, .T. ) ;
#4250 = FACE_OUTER_BOUND ( 'NONE', #32382, .T. ) ;
#4251 = DIRECTION ( 'NONE',  ( 0.07906939808003035641, 0.04137963570464910784, -0.9960099176394842102 ) ) ;
#4252 = ORIENTED_EDGE ( 'NONE', *, *, #17548, .F. ) ;
#4253 = CARTESIAN_POINT ( 'NONE',  ( 0.5804410086790514622, 40.62771722849995371, -23.42879520283626604 ) ) ;
#4254 = CARTESIAN_POINT ( 'NONE',  ( -6.079354080745853928, -4.285997663762750598, 18.77293741731384813 ) ) ;
#4255 = CARTESIAN_POINT ( 'NONE',  ( 0.9754642270333691023, 26.26019354539084105, -33.93430397636383589 ) ) ;
#4256 = VECTOR ( 'NONE', #58844, 1000.000000000000000 ) ;
#4257 = CARTESIAN_POINT ( 'NONE',  ( 0.3622758884714730732, 37.74294673546557988, 20.83792692158985460 ) ) ;
#4258 = CARTESIAN_POINT ( 'NONE',  ( 10.00000000000000533, 2.650000000000832134, -79.99999999999998579 ) ) ;
#4259 = CARTESIAN_POINT ( 'NONE',  ( 0.1064266379913938326, 26.69589650908239165, 33.86837498006634206 ) ) ;
#4260 = CARTESIAN_POINT ( 'NONE',  ( 0.6009452777970413218, 47.63713033690753917, -6.711700115493053787 ) ) ;
#4261 = ADVANCED_FACE ( 'NONE', ( #45952 ), #2373, .T. ) ;
#4262 = CARTESIAN_POINT ( 'NONE',  ( -90.00000000000000000, 0.000000000000000000, 0.000000000000000000 ) ) ;
#4263 = ORIENTED_EDGE ( 'NONE', *, *, #3035, .F. ) ;
#4264 = CARTESIAN_POINT ( 'NONE',  ( 0.9772918015221172539, 41.58800822122364593, 5.174401215804053322 ) ) ;
#4265 = CARTESIAN_POINT ( 'NONE',  ( 4.691466044806103852, 37.25818859570272679, 24.49380602310827371 ) ) ;
#4266 = ORIENTED_EDGE ( 'NONE', *, *, #27095, .F. ) ;
#4267 = CARTESIAN_POINT ( 'NONE',  ( 0.9745511491811751359, -30.58068216140355489, 30.09905547141343263 ) ) ;
#4268 = CARTESIAN_POINT ( 'NONE',  ( 1.088313998177380615, 42.90642884828985615, 0.7798619649922788888 ) ) ;
#4269 = CARTESIAN_POINT ( 'NONE',  ( 4.691466044806103852, 42.32811009116535672, 14.01607102724557841 ) ) ;
#4270 = CARTESIAN_POINT ( 'NONE',  ( 0.5804410086790514622, 40.07081992599750464, -24.36902218624453909 ) ) ;
#4271 = CARTESIAN_POINT ( 'NONE',  ( 5.901764892641288895, -10.93876531158257492, -47.73190631954474838 ) ) ;
#4272 = FACE_OUTER_BOUND ( 'NONE', #21523, .T. ) ;
#4273 = CARTESIAN_POINT ( 'NONE',  ( 0.5839880159502355284, -47.89596769806546206, -0.04537901683531408298 ) ) ;
#4274 = SHAPE_REPRESENTATION_RELATIONSHIP ( 'NONE' , 'NONE' ,  #53251, #33281 ) ;
#4275 = CARTESIAN_POINT ( 'NONE',  ( 0.5997462898726536595, -30.20781297212564454, -38.71743361310750231 ) ) ;
#4276 =( BOUNDED_SURFACE ( )  B_SPLINE_SURFACE ( 3, 1, ( 
 ( #57495, #33126 ),
 ( #27792, #37843 ),
 ( #9928, #29026 ),
 ( #51897, #8990 ) ),
 .UNSPECIFIED., .F., .F., .F. ) 
 B_SPLINE_SURFACE_WITH_KNOTS ( ( 4, 4 ),
 ( 2, 2 ),
 ( 0.000000000000000000, 1.000000000000000000 ),
 ( 0.000000000000000000, 1.000000000000000000 ),
 .UNSPECIFIED. ) 
 GEOMETRIC_REPRESENTATION_ITEM ( )  RATIONAL_B_SPLINE_SURFACE ( (
 ( 1.000000000000000000, 1.000000000000000000),
 ( 0.9952954269826590483, 0.8620686068821307169),
 ( 0.9952954269826590483, 0.8620686068821307169),
 ( 1.000000000000000000, 1.000000000000000000) ) ) 
 REPRESENTATION_ITEM ( '' )  SURFACE ( )  );
#4277 = AXIS2_PLACEMENT_3D ( 'NONE', #39956, #6676, #39027 ) ;
#4278 = CARTESIAN_POINT ( 'NONE',  ( -5.995132425357893702, 18.19985213254578937, -4.885449473615140370 ) ) ;
#4279 = CARTESIAN_POINT ( 'NONE',  ( 0.5817217712918331118, 32.27292434475872085, 34.02489247956344798 ) ) ;
#4280 = CARTESIAN_POINT ( 'NONE',  ( 0.1103310638050662151, -5.710544932889240144, 42.74468893497607525 ) ) ;
#4281 = EDGE_LOOP ( 'NONE', ( #39821, #12005, #60026, #17707 ) ) ;
#4282 = CARTESIAN_POINT ( 'NONE',  ( 1.231276596079881047, -2.246340108600348717, 41.85965512441018888 ) ) ;
#4283 = CARTESIAN_POINT ( 'NONE',  ( 5.860006189529234355, 9.393028332205414443, -47.30964106197847485 ) ) ;
#4284 = LINE ( 'NONE', #51599, #32496 ) ;
#4285 = CARTESIAN_POINT ( 'NONE',  ( 2.301430502907646947, -11.18388433759685441, -46.71331171933228887 ) ) ;
#4286 = LINE ( 'NONE', #47549, #1807 ) ;
#4287 =( BOUNDED_SURFACE ( )  B_SPLINE_SURFACE ( 3, 1, ( 
 ( #36763, #42690 ),
 ( #56754, #28565 ),
 ( #37073, #9456 ),
 ( #55836, #23562 ) ),
 .UNSPECIFIED., .F., .F., .F. ) 
 B_SPLINE_SURFACE_WITH_KNOTS ( ( 4, 4 ),
 ( 2, 2 ),
 ( 0.000000000000000000, 1.000000000000000000 ),
 ( 0.000000000000000000, 1.000000000000000000 ),
 .UNSPECIFIED. ) 
 GEOMETRIC_REPRESENTATION_ITEM ( )  RATIONAL_B_SPLINE_SURFACE ( (
 ( 1.000000000000000000, 1.000000000000000000),
 ( 0.9729067724841187204, 0.9999501103223794596),
 ( 0.9729067724841187204, 0.9999501103223794596),
 ( 1.000000000000000000, 1.000000000000000000) ) ) 
 REPRESENTATION_ITEM ( '' )  SURFACE ( )  );
#4288 = ORIENTED_EDGE ( 'NONE', *, *, #4841, .T. ) ;
#4289 = EDGE_CURVE ( 'NONE', #19981, #2478, #46959, .T. ) ;
#4290 = CARTESIAN_POINT ( 'NONE',  ( 0.3622758884714600280, -11.95365414648526148, 41.42293301073604539 ) ) ;
#4291 = CARTESIAN_POINT ( 'NONE',  ( 5.901463166500146684, -11.94204572599448966, -16.18349202795532094 ) ) ;
#4292 = DIRECTION ( 'NONE',  ( -1.826024711554534160E-16, 1.000000000000000000, 0.000000000000000000 ) ) ;
#4293 = EDGE_LOOP ( 'NONE', ( #51650, #8712, #2785, #8608 ) ) ;
#4294 = EDGE_CURVE ( 'NONE', #22826, #13003, #49381, .T. ) ;
#4295 = CARTESIAN_POINT ( 'NONE',  ( 0.6039202388192953519, 32.88598194813106090, -36.47020570487901381 ) ) ;
#4296 = VECTOR ( 'NONE', #32147, 1000.000000000000227 ) ;
#4297 = CARTESIAN_POINT ( 'NONE',  ( 0.8554163680231708922, 44.99993935735606243, 13.27444654010463942 ) ) ;
#4298 = ORIENTED_EDGE ( 'NONE', *, *, #14781, .F. ) ;
#4299 = CARTESIAN_POINT ( 'NONE',  ( 0.9268187852002115479, -26.70623247702148362, 35.07893213585482783 ) ) ;
#4300 = VERTEX_POINT ( 'NONE', #26190 ) ;
#4301 = B_SPLINE_CURVE_WITH_KNOTS ( 'NONE', 3,
 ( #648, #10384, #28857, #19175, #10070, #48582 ),
 .UNSPECIFIED., .F., .F.,
 ( 4, 2, 4 ),
 ( 1.870559545977334001E-17, 0.0002293319059085093307, 0.0004586638118169999588 ),
 .UNSPECIFIED. ) ;
#4302 = CARTESIAN_POINT ( 'NONE',  ( -6.016761891674565099, 17.41015286184812894, -7.207804629151121745 ) ) ;
#4303 = CARTESIAN_POINT ( 'NONE',  ( 0.5786265663353196143, -33.35675271369515116, -34.37803667029846366 ) ) ;
#4304 = ORIENTED_EDGE ( 'NONE', *, *, #28194, .F. ) ;
#4305 = CARTESIAN_POINT ( 'NONE',  ( 0.3622758884714730732, 42.84426538328725798, 4.808133778522027058 ) ) ;
#4306 = CARTESIAN_POINT ( 'NONE',  ( 0.1098349054025746230, 26.08296594991493933, 34.34238705454311713 ) ) ;
#4307 = DIRECTION ( 'NONE',  ( 1.000000000000000000, 0.000000000000000000, 0.000000000000000000 ) ) ;
#4308 = CARTESIAN_POINT ( 'NONE',  ( 0.5832367798473392373, -38.16362489683108805, 28.94059862654978943 ) ) ;
#4309 = EDGE_CURVE ( 'NONE', #25319, #44352, #60010, .T. ) ;
#4310 = VECTOR ( 'NONE', #6048, 1000.000000000000000 ) ;
#4311 = VERTEX_POINT ( 'NONE', #25577 ) ;
#4312 = CARTESIAN_POINT ( 'NONE',  ( 3.680974057930772592, 32.59081219553981867, 35.20670187740670798 ) ) ;
#4313 = VERTEX_POINT ( 'NONE', #26816 ) ;
#4314 = CARTESIAN_POINT ( 'NONE',  ( 4.962356264823608143, 42.01891079680549268, -2.376285612557975213 ) ) ;
#4315 = ORIENTED_EDGE ( 'NONE', *, *, #28635, .T. ) ;
#4316 = VERTEX_POINT ( 'NONE', #54992 ) ;
#4317 = CARTESIAN_POINT ( 'NONE',  ( 0.6021447746440204973, -42.91583701453753719, -23.86989887766889140 ) ) ;
#4318 = CARTESIAN_POINT ( 'NONE',  ( 0.5998501479064699549, -33.64490850298868452, 34.38546660123239462 ) ) ;
#4319 = CARTESIAN_POINT ( 'NONE',  ( 4.553261556744875094, -29.36425772793644029, -32.66925058691983708 ) ) ;
#4320 = CARTESIAN_POINT ( 'NONE',  ( 5.959547316686252039, 16.28624005235082350, 12.49238070347981910 ) ) ;
#4321 = ORIENTED_EDGE ( 'NONE', *, *, #48667, .F. ) ;
#4322 = CARTESIAN_POINT ( 'NONE',  ( -6.010958268070873523, -7.197664668556314815, -17.41463273278786161 ) ) ;
#4323 = FACE_OUTER_BOUND ( 'NONE', #11629, .T. ) ;
#4324 = DIRECTION ( 'NONE',  ( 0.000000000000000000, 0.000000000000000000, -1.000000000000000000 ) ) ;
#4325 = ORIENTED_EDGE ( 'NONE', *, *, #21791, .F. ) ;
#4326 = ORIENTED_EDGE ( 'NONE', *, *, #19124, .T. ) ;
#4327 = CARTESIAN_POINT ( 'NONE',  ( 0.6001305935487315502, 5.760103278697374485, 47.76436356026970032 ) ) ;
#4328 = B_SPLINE_CURVE_WITH_KNOTS ( 'NONE', 3,
 ( #48007, #28884, #29809, #39868 ),
 .UNSPECIFIED., .F., .F.,
 ( 4, 4 ),
 ( 0.000000000000000000, 0.005014147105413702121 ),
 .UNSPECIFIED. ) ;
#4329 = CARTESIAN_POINT ( 'NONE',  ( 5.965394784446458765, -19.82972329408682199, -5.298374383010567179 ) ) ;
#4330 = FACE_OUTER_BOUND ( 'NONE', #6866, .T. ) ;
#4331 = EDGE_CURVE ( 'NONE', #52228, #58926, #44223, .T. ) ;
#4332 = CARTESIAN_POINT ( 'NONE',  ( 4.553261556744873317, 43.53643125131393532, -5.841123155973635406 ) ) ;
#4333 = CARTESIAN_POINT ( 'NONE',  ( 0.9780303403264770656, 38.70851733140969486, 16.06207643485240766 ) ) ;
#4334 = ORIENTED_EDGE ( 'NONE', *, *, #1048, .T. ) ;
#4335 = CARTESIAN_POINT ( 'NONE',  ( 2.500000000000000000, -2.357898499370432166, 3.035766082959412415E-15 ) ) ;
#4336 = CARTESIAN_POINT ( 'NONE',  ( 48.39278666958532682, 15.41618682757451353, 1.616172141987365363 ) ) ;
#4337 = CARTESIAN_POINT ( 'NONE',  ( 0.8744876279028263033, -24.68559978112701714, -42.43785119236734715 ) ) ;
#4338 = B_SPLINE_CURVE_WITH_KNOTS ( 'NONE', 3,
 ( #1553, #54168, #20082, #44830 ),
 .UNSPECIFIED., .F., .F.,
 ( 4, 4 ),
 ( 2.168404344971008868E-19, 0.004446298630425069356 ),
 .UNSPECIFIED. ) ;
#4339 = AXIS2_PLACEMENT_3D ( 'NONE', #29402, #24400, #52273 ) ;
#4340 = CARTESIAN_POINT ( 'NONE',  ( 1.231276596079881047, -35.03243822710529543, 23.02183839058294623 ) ) ;
#4341 = CARTESIAN_POINT ( 'NONE',  ( 1.231276596079887264, -6.136529359146732254, 41.46829847537028257 ) ) ;
#4342 = ORIENTED_EDGE ( 'NONE', *, *, #3878, .T. ) ;
#4343 = CARTESIAN_POINT ( 'NONE',  ( 5.965394784446460541, 0.01447339372453102999, -20.52536205633085231 ) ) ;
#4344 = CARTESIAN_POINT ( 'NONE',  ( 4.335381028904201628, 47.11764506933897678, -13.40463989759294527 ) ) ;
#4345 = CARTESIAN_POINT ( 'NONE',  ( 5.965394784446458765, -20.35165389555756477, -2.664747781316041841 ) ) ;
#4346 = CARTESIAN_POINT ( 'NONE',  ( 5.895881250540457863, 20.06826253866635668, 1.338850360369496784 ) ) ;
#4347 = CARTESIAN_POINT ( 'NONE',  ( 0.5980271706414711508, -0.8742700727934676896, -49.10483575658795985 ) ) ;
#4348 = CARTESIAN_POINT ( 'NONE',  ( 0.9790320750461911636, -34.59983469426835967, 23.64716836476394235 ) ) ;
#4349 = VECTOR ( 'NONE', #51474, 1000.000000000000000 ) ;
#4350 = CARTESIAN_POINT ( 'NONE',  ( 1.231276596079887264, -31.65135013586864332, -27.48579279545554144 ) ) ;
#4351 = EDGE_CURVE ( 'NONE', #52459, #58767, #50947, .T. ) ;
#4352 = CARTESIAN_POINT ( 'NONE',  ( 0.8744876279028263033, 21.91587810745035725, 43.93226988398016886 ) ) ;
#4353 =( BOUNDED_SURFACE ( )  B_SPLINE_SURFACE ( 3, 1, ( 
 ( #4450, #23590 ),
 ( #18915, #33319 ),
 ( #52391, #5074 ),
 ( #24204, #9485 ) ),
 .UNSPECIFIED., .F., .F., .F. ) 
 B_SPLINE_SURFACE_WITH_KNOTS ( ( 4, 4 ),
 ( 2, 2 ),
 ( 0.000000000000000000, 1.000000000000000000 ),
 ( 0.000000000000000000, 1.000000000000000000 ),
 .UNSPECIFIED. ) 
 GEOMETRIC_REPRESENTATION_ITEM ( )  RATIONAL_B_SPLINE_SURFACE ( (
 ( 1.000000000000000000, 1.000000000000000000),
 ( 0.7211978278499970862, 0.9934217856018976445),
 ( 0.7211978278499970862, 0.9934217856018976445),
 ( 1.000000000000000000, 1.000000000000000000) ) ) 
 REPRESENTATION_ITEM ( '' )  SURFACE ( )  );
#4354 = ORIENTED_EDGE ( 'NONE', *, *, #48234, .F. ) ;
#4355 = CARTESIAN_POINT ( 'NONE',  ( 1.227938101723756947, -39.96870412324324917, -15.63977281655884077 ) ) ;
#4356 = CARTESIAN_POINT ( 'NONE',  ( 0.9790724872846777727, 20.10506717481070282, 36.77120454755054624 ) ) ;
#4357 = DIRECTION ( 'NONE',  ( 0.000000000000000000, 0.000000000000000000, 1.000000000000000000 ) ) ;
#4358 = CARTESIAN_POINT ( 'NONE',  ( 4.960386119450145515, -16.16390115411087791, -40.65912891531831974 ) ) ;
#4359 = VERTEX_POINT ( 'NONE', #15887 ) ;
#4360 = ADVANCED_FACE ( 'NONE', ( #44712 ), #21049, .T. ) ;
#4361 = CARTESIAN_POINT ( 'NONE',  ( 0.7762783648524390623, -46.03397615175193636, 13.25585403815104613 ) ) ;
#4362 = CARTESIAN_POINT ( 'NONE',  ( 0.5848930533535030563, -44.24150702629557941, 15.55513222154659125 ) ) ;
#4363 = EDGE_CURVE ( 'NONE', #32404, #54938, #32059, .T. ) ;
#4364 = ORIENTED_EDGE ( 'NONE', *, *, #46286, .F. ) ;
#4365 = CARTESIAN_POINT ( 'NONE',  ( 0.1135584504625007790, 4.666723112812798391, -43.87680192907855314 ) ) ;
#4366 = CARTESIAN_POINT ( 'NONE',  ( 4.834790513006555379, 34.26126461650152777, 32.53851698836996320 ) ) ;
#4367 = FACE_OUTER_BOUND ( 'NONE', #47776, .T. ) ;
#4368 = EDGE_LOOP ( 'NONE', ( #50316, #11596, #32917, #34494 ) ) ;
#4369 = B_SPLINE_CURVE_WITH_KNOTS ( 'NONE', 3,
 ( #2274, #21406, #35834, #40540 ),
 .UNSPECIFIED., .F., .F.,
 ( 4, 4 ),
 ( 0.000000000000000000, 0.004442905043737214836 ),
 .UNSPECIFIED. ) ;
#4370 = CARTESIAN_POINT ( 'NONE',  ( 4.960156602257182357, -15.40604254112674987, 43.79161740034471251 ) ) ;
#4371 = ORIENTED_EDGE ( 'NONE', *, *, #26645, .F. ) ;
#4372 = ORIENTED_EDGE ( 'NONE', *, *, #5786, .T. ) ;
#4373 = CARTESIAN_POINT ( 'NONE',  ( 0.5997462898726536595, 41.43917033312134635, -26.35046094941917971 ) ) ;
#4374 = CARTESIAN_POINT ( 'NONE',  ( 4.322998006666165516, -43.48102276965688873, -20.30542865297633881 ) ) ;
#4375 = ORIENTED_EDGE ( 'NONE', *, *, #29725, .F. ) ;
#4376 = CARTESIAN_POINT ( 'NONE',  ( 4.956653778116973719, 27.17045123668471973, 39.67974989265048436 ) ) ;
#4377 = ADVANCED_FACE ( 'NONE', ( #16493 ), #40106, .F. ) ;
#4378 = CIRCLE ( 'NONE', #32418, 48.91267123290010943 ) ;
#4379 = ORIENTED_EDGE ( 'NONE', *, *, #18689, .T. ) ;
#4380 = CARTESIAN_POINT ( 'NONE',  ( 3.783278058412224087, -12.79810311738825668, -41.09146792477079657 ) ) ;
#4381 = CYLINDRICAL_SURFACE ( 'NONE', #50819, 75.00000000000001421 ) ;
#4382 = FACE_OUTER_BOUND ( 'NONE', #10805, .T. ) ;
#4383 = ORIENTED_EDGE ( 'NONE', *, *, #23262, .T. ) ;
#4384 = CARTESIAN_POINT ( 'NONE',  ( 4.962356264823608143, 0.000000000000000000, 0.000000000000000000 ) ) ;
#4385 = CARTESIAN_POINT ( 'NONE',  ( 0.8554163680231816613, -45.78608427674282666, 10.23913862172123146 ) ) ;
#4386 = CARTESIAN_POINT ( 'NONE',  ( 5.960721111146673579, 2.672857320903303968, -20.35079619394243267 ) ) ;
#4387 = CARTESIAN_POINT ( 'NONE',  ( 0.5834584762367742705, 16.68472608544807301, 43.82757014102836024 ) ) ;
#4388 = VERTEX_POINT ( 'NONE', #35622 ) ;
#4389 = CARTESIAN_POINT ( 'NONE',  ( 0.5819845901640485764, -33.54497622115107447, -34.18710267837688832 ) ) ;
#4390 = CARTESIAN_POINT ( 'NONE',  ( 0.1156867017252033725, -31.60951488276809940, -30.78605814571343657 ) ) ;
#4391 = CIRCLE ( 'NONE', #53419, 48.09070567114147110 ) ;
#4392 = EDGE_LOOP ( 'NONE', ( #39835, #8337, #19205, #8331 ) ) ;
#4393 = ORIENTED_EDGE ( 'NONE', *, *, #49227, .T. ) ;
#4394 = CARTESIAN_POINT ( 'NONE',  ( 3.376099380956838925, -5.222100608646857545, -12.34658045230489165 ) ) ;
#4395 = CARTESIAN_POINT ( 'NONE',  ( 0.5806925824938499181, 11.40214825760356376, -45.48860711711441240 ) ) ;
#4396 = VERTEX_POINT ( 'NONE', #54680 ) ;
#4397 = CARTESIAN_POINT ( 'NONE',  ( 0.9789889208857696090, -34.60556929628447165, -23.63872821711065342 ) ) ;
#4398 = DIRECTION ( 'NONE',  ( 0.000000000000000000, -1.000000000000000000, 0.000000000000000000 ) ) ;
#4399 = CARTESIAN_POINT ( 'NONE',  ( 4.956445790444040433, 46.94638516972321440, -3.684422564748698115 ) ) ;
#4400 = CARTESIAN_POINT ( 'NONE',  ( 0.6039202388192952409, 46.66051417535201296, -15.30882522405831914 ) ) ;
#4401 = ORIENTED_EDGE ( 'NONE', *, *, #61136, .F. ) ;
#4402 = CARTESIAN_POINT ( 'NONE',  ( 4.549368137175248350, -40.58005590356700765, 13.99871866169291579 ) ) ;
#4403 = CARTESIAN_POINT ( 'NONE',  ( 0.8554163680231708922, 46.90810212776801791, 0.9140174411379320407 ) ) ;
#4404 = EDGE_CURVE ( 'NONE', #20911, #41448, #46554, .T. ) ;
#4405 = FACE_OUTER_BOUND ( 'NONE', #21105, .T. ) ;
#4406 = CARTESIAN_POINT ( 'NONE',  ( 0.9730545539215883499, 34.34678117142591702, -25.71816799638743944 ) ) ;
#4407 = APPLICATION_CONTEXT ( 'automotive_design' ) ;
#4408 = B_SPLINE_CURVE_WITH_KNOTS ( 'NONE', 3,
 ( #44775, #59138, #58208, #6496 ),
 .UNSPECIFIED., .F., .F.,
 ( 4, 4 ),
 ( 0.000000000000000000, 0.004446298630425099714 ),
 .UNSPECIFIED. ) ;
#4409 = EDGE_CURVE ( 'NONE', #29673, #33762, #33082, .T. ) ;
#4410 = CARTESIAN_POINT ( 'NONE',  ( 0.6845945791218034371, -46.85360930762398368, 2.268439014493165651 ) ) ;
#4411 = CARTESIAN_POINT ( 'NONE',  ( -6.016104459813374383, -16.32137543786089040, 9.416989654584247305 ) ) ;
#4412 = CARTESIAN_POINT ( 'NONE',  ( -6.017396004339686577, 11.47192209077586789, 14.94857180791997209 ) ) ;
#4413 = EDGE_CURVE ( 'NONE', #19627, #4009, #29196, .T. ) ;
#4414 = CARTESIAN_POINT ( 'NONE',  ( 0.5980894510889457338, 6.974827154143460994, 47.60453381548694551 ) ) ;
#4415 = CARTESIAN_POINT ( 'NONE',  ( 0.5837800304671217910, 40.37258561079670471, -23.85983368086184697 ) ) ;
#4416 = LINE ( 'NONE', #8845, #31422 ) ;
#4417 = CARTESIAN_POINT ( 'NONE',  ( 0.9749527285493296835, 30.54214995146816491, -30.13822974582783232 ) ) ;
#4418 = CARTESIAN_POINT ( 'NONE',  ( 0.6064782688330851990, 33.10963464956490299, -33.21274664629680018 ) ) ;
#4419 = CARTESIAN_POINT ( 'NONE',  ( 0.5804410086790514622, 46.55025363952972128, -5.709092568074903618 ) ) ;
#4420 = CARTESIAN_POINT ( 'NONE',  ( 0.9757892942422814464, 37.18547544211216405, 21.40977514834397866 ) ) ;
#4421 = CARTESIAN_POINT ( 'NONE',  ( 3.727782113643637096, -20.93509053340439152, 38.65876045948883188 ) ) ;
#4422 = B_SPLINE_CURVE_WITH_KNOTS ( 'NONE', 3,
 ( #27353, #3526, #56767, #37092, #55852, #2920 ),
 .UNSPECIFIED., .F., .F.,
 ( 4, 2, 4 ),
 ( 9.055522398700297199E-18, 0.0002291978881530152385, 0.0004583957763060214239 ),
 .UNSPECIFIED. ) ;
#4423 = CARTESIAN_POINT ( 'NONE',  ( -6.016104459813371719, 16.32137543786083000, 9.416989654584362768 ) ) ;
#4424 = ADVANCED_FACE ( 'NONE', ( #8943 ), #31285, .F. ) ;
#4425 = CARTESIAN_POINT ( 'NONE',  ( 0.1129192098497447394, 37.24220309526806005, 23.66368729500878842 ) ) ;
#4427 = ORIENTED_EDGE ( 'NONE', *, *, #61563, .T. ) ;
#4426 = CARTESIAN_POINT ( 'NONE',  ( 4.975801465491695552, 26.14269827151680659, -40.15204426031507268 ) ) ;
#4428 = CARTESIAN_POINT ( 'NONE',  ( -6.077587904424778920, 13.83688374988438241, -13.39166417911216911 ) ) ;
#4429 = CONICAL_SURFACE ( 'NONE', #34618, 42.08604991992415023, 1.569615340895231137 ) ;
#4430 = CARTESIAN_POINT ( 'NONE',  ( 0.5827357941260193908, 24.26189667805002870, 41.29633147056624409 ) ) ;
#4432 = EDGE_CURVE ( 'NONE', #31934, #41987, #29980, .T. ) ;
#4431 = CARTESIAN_POINT ( 'NONE',  ( 0.8751705887134423323, -33.37254303619531726, -34.63284514348573850 ) ) ;
#4433 = VERTEX_POINT ( 'NONE', #36858 ) ;
#4434 = CARTESIAN_POINT ( 'NONE',  ( 5.283180000000047727, 0.000000000000000000, 0.000000000000000000 ) ) ;
#4435 = AXIS2_PLACEMENT_3D ( 'NONE', #39525, #5637, #24783 ) ;
#4436 = CARTESIAN_POINT ( 'NONE',  ( 3.407937589446174087, -11.14158115674378990, 7.970324840161918445 ) ) ;
#4437 = B_SPLINE_CURVE_WITH_KNOTS ( 'NONE', 3,
 ( #56026, #3394, #32243, #17521 ),
 .UNSPECIFIED., .F., .F.,
 ( 4, 4 ),
 ( 2.071251839531113129E-17, 0.004444306975806115029 ),
 .UNSPECIFIED. ) ;
#4438 = EDGE_CURVE ( 'NONE', #52417, #21984, #50181, .T. ) ;
#4439 = ORIENTED_EDGE ( 'NONE', *, *, #21791, .T. ) ;
#4440 = ORIENTED_EDGE ( 'NONE', *, *, #14558, .T. ) ;
#4441 = CARTESIAN_POINT ( 'NONE',  ( 4.956445790444031552, 30.81386304088997719, -35.60960396630257208 ) ) ;
#4442 = VERTEX_POINT ( 'NONE', #37165 ) ;
#4443 = CARTESIAN_POINT ( 'NONE',  ( 4.694002226626920127, 13.30107597157337196, 43.60465742835927472 ) ) ;
#4444 = CARTESIAN_POINT ( 'NONE',  ( 0.8557997880470599172, -43.90420959842167292, -19.17299735372055736 ) ) ;
#4445 = ORIENTED_EDGE ( 'NONE', *, *, #10402, .T. ) ;
#4446 = ORIENTED_EDGE ( 'NONE', *, *, #21155, .T. ) ;
#4447 = FACE_OUTER_BOUND ( 'NONE', #48206, .T. ) ;
#4448 = ORIENTED_EDGE ( 'NONE', *, *, #50872, .F. ) ;
#4449 = CARTESIAN_POINT ( 'NONE',  ( -2.601141883200665639, -13.99736252863769259, 5.183557630747252176 ) ) ;
#4450 = CARTESIAN_POINT ( 'NONE',  ( -6.077587904424778920, -8.912150607695132010, -17.06955163264957420 ) ) ;
#4451 = ADVANCED_FACE ( 'NONE', ( #12738 ), #7024, .T. ) ;
#4452 = CARTESIAN_POINT ( 'NONE',  ( 0.1092355843206037486, -30.28032287551058488, -30.70542469027314070 ) ) ;
#4453 = ORIENTED_EDGE ( 'NONE', *, *, #15942, .F. ) ;
#4454 = DIRECTION ( 'NONE',  ( 1.000000000000000000, 0.000000000000000000, 0.000000000000000000 ) ) ;
#4455 =( BOUNDED_SURFACE ( )  B_SPLINE_SURFACE ( 3, 1, ( 
 ( #43940, #18557 ),
 ( #61746, #33592 ),
 ( #4726, #52359 ),
 ( #14183, #9452 ) ),
 .UNSPECIFIED., .F., .F., .F. ) 
 B_SPLINE_SURFACE_WITH_KNOTS ( ( 4, 4 ),
 ( 2, 2 ),
 ( 0.000000000000000000, 1.000000000000000000 ),
 ( 0.000000000000000000, 1.000000000000000000 ),
 .UNSPECIFIED. ) 
 GEOMETRIC_REPRESENTATION_ITEM ( )  RATIONAL_B_SPLINE_SURFACE ( (
 ( 1.000000000000000000, 1.000000000000000000),
 ( 0.7223157951917480446, 0.9931996967497186413),
 ( 0.7223157951917480446, 0.9931996967497186413),
 ( 1.000000000000000000, 1.000000000000000000) ) ) 
 REPRESENTATION_ITEM ( '' )  SURFACE ( )  );
#4456 = AXIS2_PLACEMENT_3D ( 'NONE', #52364, #46164, #18264 ) ;
#4457 = CARTESIAN_POINT ( 'NONE',  ( 0.9772918015221170318, -39.45178799254951230, 14.13836199641267122 ) ) ;
#4458 = EDGE_LOOP ( 'NONE', ( #58068, #25684, #17201, #37951 ) ) ;
#4459 = ORIENTED_EDGE ( 'NONE', *, *, #16402, .F. ) ;
#4460 = DIRECTION ( 'NONE',  ( -1.000000000000000000, -0.000000000000000000, -0.000000000000000000 ) ) ;
#4461 = VERTEX_POINT ( 'NONE', #37793 ) ;
#4462 = CARTESIAN_POINT ( 'NONE',  ( 3.390910168358336918, 34.73058703434708150, 26.97931542465967070 ) ) ;
#4463 = CARTESIAN_POINT ( 'NONE',  ( 1.227938101723756947, -41.23019537246717903, 11.92353943227934998 ) ) ;
#4464 = CARTESIAN_POINT ( 'NONE',  ( 0.5807400328401574052, -38.33001520688930697, -28.72484455891681421 ) ) ;
#4465 = CARTESIAN_POINT ( 'NONE',  ( 0.1103310638050661874, 5.547176740492965052, 42.76619676553138305 ) ) ;
#4466 = CARTESIAN_POINT ( 'NONE',  ( 5.880360259849752858, -9.312491912827802309, -47.05949693022704849 ) ) ;
#4467 = B_SPLINE_CURVE_WITH_KNOTS ( 'NONE', 3,
 ( #17753, #42812, #4240, #22755 ),
 .UNSPECIFIED., .F., .F.,
 ( 4, 4 ),
 ( 8.673617379884035472E-19, 0.004048833967417087357 ),
 .UNSPECIFIED. ) ;
#4468 = ORIENTED_EDGE ( 'NONE', *, *, #24042, .F. ) ;
#4469 = FACE_OUTER_BOUND ( 'NONE', #58234, .T. ) ;
#4470 = CARTESIAN_POINT ( 'NONE',  ( 0.5797568599927143129, 46.55714417914590797, -5.626511757139216918 ) ) ;
#4471 = CARTESIAN_POINT ( 'NONE',  ( 5.896782393890504181, 18.99788783847851548, 6.603510017755907846 ) ) ;
#4472 = AXIS2_PLACEMENT_3D ( 'NONE', #56348, #47281, #33193 ) ;
#4473 = ORIENTED_EDGE ( 'NONE', *, *, #38138, .T. ) ;
#4474 = CARTESIAN_POINT ( 'NONE',  ( 0.6000166863083090663, -30.20952222014404143, -38.71961065066482632 ) ) ;
#4475 = CARTESIAN_POINT ( 'NONE',  ( 0.5980894510889448457, -46.65000524237095192, 11.77356634613236963 ) ) ;
#4476 = CARTESIAN_POINT ( 'NONE',  ( 0.8557997880470697982, -5.347802024197571669, 47.60865952216997243 ) ) ;
#4478 = ORIENTED_EDGE ( 'NONE', *, *, #38452, .F. ) ;
#4477 = VECTOR ( 'NONE', #13728, 1000.000000000000114 ) ;
#4479 = VERTEX_POINT ( 'NONE', #34004 ) ;
#4480 = CARTESIAN_POINT ( 'NONE',  ( 4.291220156522059348, 38.26855966511131157, -27.47555892904659913 ) ) ;
#4481 = CARTESIAN_POINT ( 'NONE',  ( 0.1100247026804066219, -42.77732815928603571, 5.460606496326182224 ) ) ;
#4482 = EDGE_CURVE ( 'NONE', #45673, #59272, #23066, .T. ) ;
#4483 = CARTESIAN_POINT ( 'NONE',  ( 4.956445790444006683, -32.34643101787064978, -34.22347806032829709 ) ) ;
#4484 = AXIS2_PLACEMENT_3D ( 'NONE', #7006, #16435, #29602 ) ;
#4485 = CARTESIAN_POINT ( 'NONE',  ( 1.830465331921978356, 42.98436206491231104, 9.629157478768243905 ) ) ;
#4486 = B_SPLINE_CURVE_WITH_KNOTS ( 'NONE', 3,
 ( #49126, #20028, #42913, #19100, #38214, #57260, #14396, #58198, #15321, #33504, #40076, #44463, #35051, #55348, #16865, #7421, #41001, #30622, #1490 ),
 .UNSPECIFIED., .F., .F.,
 ( 4, 3, 3, 3, 3, 3, 4 ),
 ( 1.153344816771540786E-16, 0.0002618519381806260794, 0.0003927759815485984689, 0.0005237000248299445142, 0.0006546240681324982588, 0.0007855481115631334681, 0.0009699050456655117008 ),
 .UNSPECIFIED. ) ;
#4487 = CARTESIAN_POINT ( 'NONE',  ( 4.553261556744875094, 0.000000000000000000, 0.000000000000000000 ) ) ;
#4488 = EDGE_CURVE ( 'NONE', #30530, #10287, #51603, .T. ) ;
#4489 = CARTESIAN_POINT ( 'NONE',  ( 0.9754642270333688803, -42.56393738774954727, 5.426415525315669619 ) ) ;
#4490 = CARTESIAN_POINT ( 'NONE',  ( 0.9972139404380270244, -22.02214929131115895, -36.82725283858632537 ) ) ;
#4491 = CYLINDRICAL_SURFACE ( 'NONE', #43043, 15.99999999999999645 ) ;
#4492 = DIRECTION ( 'NONE',  ( 1.000000000000000000, -0.000000000000000000, -0.000000000000000000 ) ) ;
#4493 = CARTESIAN_POINT ( 'NONE',  ( 3.661933894777875675, -41.09997021044436138, -22.87845304325095697 ) ) ;
#4494 = EDGE_CURVE ( 'NONE', #7287, #36466, #2341, .T. ) ;
#4495 = DIRECTION ( 'NONE',  ( 1.000000000000000000, 0.000000000000000000, 0.000000000000000000 ) ) ;
#4496 = EDGE_CURVE ( 'NONE', #34059, #31779, #54586, .T. ) ;
#4497 = CARTESIAN_POINT ( 'NONE',  ( 0.5850706913938534814, 12.57184842332017460, 46.21698775168649576 ) ) ;
#4498 = ORIENTED_EDGE ( 'NONE', *, *, #40509, .F. ) ;
#4499 = ADVANCED_FACE ( 'NONE', ( #57445 ), #46484, .F. ) ;
#4500 = CARTESIAN_POINT ( 'NONE',  ( 0.7056313189692713372, -46.73287197163856632, 3.973326218673276511 ) ) ;
#4501 = CARTESIAN_POINT ( 'NONE',  ( 3.660087539127331535, 22.37124151181838627, -42.51124390328609337 ) ) ;
#4502 = CARTESIAN_POINT ( 'NONE',  ( 4.303969348037246512, -14.52400616872400896, 45.86537346639053681 ) ) ;
#4503 = CARTESIAN_POINT ( 'NONE',  ( 10.00000000000000888, -2.549224068967256091E-30, 75.00000000000001421 ) ) ;
#4504 = CARTESIAN_POINT ( 'NONE',  ( 4.962356264823608143, 23.01169039590672938, -35.23773124060741679 ) ) ;
#4505 = DIRECTION ( 'NONE',  ( -1.000000000000000000, -0.000000000000000000, -0.000000000000000000 ) ) ;
#4506 = CARTESIAN_POINT ( 'NONE',  ( 0.3676999524040366896, 44.06746933160592050, 2.002181318165502599 ) ) ;
#4507 = CARTESIAN_POINT ( 'NONE',  ( 0.6028777368367060907, 48.21841697337477939, -9.301832824386606191 ) ) ;
#4508 = ADVANCED_FACE ( 'NONE', ( #14279 ), #52865, .F. ) ;
#4509 = CARTESIAN_POINT ( 'NONE',  ( 5.901463166500145796, -4.676581321914135003, 19.56137667650619960 ) ) ;
#4510 = ADVANCED_FACE ( 'NONE', ( #5450 ), #42110, .F. ) ;
#4511 = CARTESIAN_POINT ( 'NONE',  ( 0.6001305935487422083, -11.94532529598347814, -46.60388846085719194 ) ) ;
#4513 = EDGE_LOOP ( 'NONE', ( #27565, #49130, #52774, #5751 ) ) ;
#4512 = CARTESIAN_POINT ( 'NONE',  ( 4.967162193818130511, 3.259922920617742914, 42.96271701169386859 ) ) ;
#4514 = ORIENTED_EDGE ( 'NONE', *, *, #12981, .T. ) ;
#4515 = CARTESIAN_POINT ( 'NONE',  ( 1.154321485836933725, -42.90848031452335221, 0.8253076867717469289 ) ) ;
#4516 = CARTESIAN_POINT ( 'NONE',  ( 0.1100053167205930771, 39.91014771056754995, 16.33707796615720653 ) ) ;
#4517 = CARTESIAN_POINT ( 'NONE',  ( -6.010958268070873523, -14.95835081545482304, 11.45964880703821187 ) ) ;
#4518 = VERTEX_POINT ( 'NONE', #28975 ) ;
#4519 = CARTESIAN_POINT ( 'NONE',  ( 0.6021448801613057400, 11.18197771114837558, -47.81740805495764590 ) ) ;
#4520 = CARTESIAN_POINT ( 'NONE',  ( 0.5830081025819944252, -45.90105815717110715, 9.608584413650092415 ) ) ;
#4521 = CARTESIAN_POINT ( 'NONE',  ( 0.1092565886968785288, 5.321013289171662386, -42.79503959566648064 ) ) ;
#4522 = EDGE_LOOP ( 'NONE', ( #13999, #53612, #5981, #56012 ) ) ;
#4523 = ORIENTED_EDGE ( 'NONE', *, *, #58325, .F. ) ;
#4524 = VECTOR ( 'NONE', #80, 1000.000000000000000 ) ;
#4525 = FILL_AREA_STYLE ('',( #27429 ) ) ;
#4526 = CARTESIAN_POINT ( 'NONE',  ( 3.727782113643637096, -39.89987845506692565, 18.46015913194848679 ) ) ;
#4527 = CIRCLE ( 'NONE', #34570, 47.09074272231896430 ) ;
#4528 = CARTESIAN_POINT ( 'NONE',  ( -6.072942160501519027, -16.13052748855422180, -10.51714054436931889 ) ) ;
#4530 = CARTESIAN_POINT ( 'NONE',  ( 0.8560838555295223751, -41.44626783305086093, 21.96769712083507287 ) ) ;
#4529 = AXIS2_PLACEMENT_3D ( 'NONE', #47141, #35361, #8584 ) ;
#4531 = ADVANCED_FACE ( 'NONE', ( #48089 ), #59253, .F. ) ;
#4532 = DIRECTION ( 'NONE',  ( 0.000000000000000000, 0.000000000000000000, -1.000000000000000000 ) ) ;
#4533 = EDGE_CURVE ( 'NONE', #37398, #46412, #36099, .T. ) ;
#4534 = CARTESIAN_POINT ( 'NONE',  ( 0.1140933569871964981, 33.35113380425563179, 28.89034136272091402 ) ) ;
#4535 = VERTEX_POINT ( 'NONE', #26423 ) ;
#4536 =( BOUNDED_SURFACE ( )  B_SPLINE_SURFACE ( 3, 1, ( 
 ( #15979, #1534 ),
 ( #48860, #30668 ),
 ( #35093, #6846 ),
 ( #11912, #21287 ) ),
 .UNSPECIFIED., .F., .F., .F. ) 
 B_SPLINE_SURFACE_WITH_KNOTS ( ( 4, 4 ),
 ( 2, 2 ),
 ( 0.000000000000000000, 1.000000000000000000 ),
 ( 0.000000000000000000, 1.000000000000000000 ),
 .UNSPECIFIED. ) 
 GEOMETRIC_REPRESENTATION_ITEM ( )  RATIONAL_B_SPLINE_SURFACE ( (
 ( 1.000000000000000000, 1.000000000000000000),
 ( 0.7269869731126817891, 0.9931720237060910339),
 ( 0.7269869731126817891, 0.9931720237060910339),
 ( 1.000000000000000000, 1.000000000000000000) ) ) 
 REPRESENTATION_ITEM ( '' )  SURFACE ( )  );
#4537 = LINE ( 'NONE', #18998, #57830 ) ;
#4538 = CARTESIAN_POINT ( 'NONE',  ( -6.015611763856276717, 13.31979030221817695, -13.32857883366819429 ) ) ;
#4539 = ORIENTED_EDGE ( 'NONE', *, *, #20231, .F. ) ;
#4540 = CYLINDRICAL_SURFACE ( 'NONE', #31521, 5.000000000000000000 ) ;
#4541 = CARTESIAN_POINT ( 'NONE',  ( 0.7057020205115025480, -47.89404687311019870, -0.8412108057957802254 ) ) ;
#4542 = CARTESIAN_POINT ( 'NONE',  ( 4.956653778116981712, -42.88673967249145846, 21.75875759808692322 ) ) ;
#4543 = CARTESIAN_POINT ( 'NONE',  ( 0.7246131072078556556, -7.091231226025147549, 47.57651137777902051 ) ) ;
#4544 = VERTEX_POINT ( 'NONE', #50537 ) ;
#4545 = VERTEX_POINT ( 'NONE', #11114 ) ;
#4546 = CARTESIAN_POINT ( 'NONE',  ( 0.9740398440564311811, 0.4145941695173028241, 42.90647580953695694 ) ) ;
#4547 = CARTESIAN_POINT ( 'NONE',  ( -2.601141883200662974, 14.86024923780644436, -1.403003941427712009 ) ) ;
#4548 = CARTESIAN_POINT ( 'NONE',  ( 4.956445790444027999, 19.33052208089617352, -42.94029536716791995 ) ) ;
#4549 = ORIENTED_EDGE ( 'NONE', *, *, #28358, .F. ) ;
#4550 = CARTESIAN_POINT ( 'NONE',  ( 0.6029442701453591180, 4.628739180449442436, -48.88885352263488926 ) ) ;
#4551 = VERTEX_POINT ( 'NONE', #55227 ) ;
#4552 = CARTESIAN_POINT ( 'NONE',  ( 3.559346040607745287, 43.50545415529854409, 6.380105037004119239 ) ) ;
#4553 = LINE ( 'NONE', #33417, #43447 ) ;
#4554 = ORIENTED_EDGE ( 'NONE', *, *, #33256, .F. ) ;
#4555 = CARTESIAN_POINT ( 'NONE',  ( 0.5837374860065634996, -47.50965286059333437, -6.071555045025093911 ) ) ;
#4556 = CARTESIAN_POINT ( 'NONE',  ( -6.573139779782565029, 8.399367431416496999, 5.684374357154926636E-14 ) ) ;
#4557 = ADVANCED_FACE ( 'NONE', ( #54917 ), #56048, .F. ) ;
#4558 = DIRECTION ( 'NONE',  ( -1.000000000000000000, -0.000000000000000000, -0.000000000000000000 ) ) ;
#4559 = EDGE_LOOP ( 'NONE', ( #44351, #11142, #17776, #29089, #19454, #53381, #6531, #16915, #53615, #20973, #20892, #60016, #50175, #35917, #51876, #8872, #49689, #37409, #53604, #11031, #21911, #14495, #33238, #45642, #43438, #49008, #10934, #32120, #46419, #33954, #61890, #47392, #31652, #55862, #27283, #19608, #18843, #55225, #20094, #16822, #26224, #18869, #21248, #59101, #39721, #53608, #34108, #41338, #38975, #21458, #11306, #16421, #48951, #49240, #20935, #30908, #28844, #4806, #43842, #22367, #32853, #19656, #32226, #51152, #8412, #22351, #8867, #24268, #30430, #14931, #45658, #28278, #56728, #32554, #31721, #45985, #45791, #59759, #6911, #30551, #46476, #20138, #56255, #21763, #52499, #25826, #2576, #25813, #48668, #1796, #45739, #8441, #16824, #15983, #60428, #55472, #11104, #6582, #50235, #58855, #13070, #29326, #15937, #46897, #13612, #41421, #53946, #6871, #46794, #8647, #61251, #19790, #2065, #1000, #55502, #123, #43400, #46573, #41332, #40104, #30671, #55262, #52006, #10450, #51658, #16627, #54691, #13938, #1870, #12790, #11163, #48695, #54140, #24458, #40030, #6609, #39447, #49996, #10914, #51947, #27983, #7070, #52997, #47604 ) ) ;
#4560 = EDGE_CURVE ( 'NONE', #1315, #37210, #36783, .T. ) ;
#4561 = B_SPLINE_CURVE_WITH_KNOTS ( 'NONE', 3,
 ( #55860, #41800, #50855, #22984 ),
 .UNSPECIFIED., .F., .F.,
 ( 4, 4 ),
 ( 0.000000000000000000, 0.004442905043737214836 ),
 .UNSPECIFIED. ) ;
#4562 = CARTESIAN_POINT ( 'NONE',  ( 0.3622758884714730732, -20.83792692158999316, 37.74294673546550172 ) ) ;
#4563 = CARTESIAN_POINT ( 'NONE',  ( -2.000000000000022649, -3.464101615137742396, 0.000000000000000000 ) ) ;
#4564 = CARTESIAN_POINT ( 'NONE',  ( -6.078457390727109555, -8.910533588204199162, -17.07035155499126233 ) ) ;
#4565 = CARTESIAN_POINT ( 'NONE',  ( 4.956653778116975495, -27.17045123668499684, 39.67974989265029961 ) ) ;
#4566 = CARTESIAN_POINT ( 'NONE',  ( 0.1073791018717483448, 16.05399293000815675, -40.02496097243042072 ) ) ;
#4567 = ORIENTED_EDGE ( 'NONE', *, *, #13268, .F. ) ;
#4568 = EDGE_CURVE ( 'NONE', #23055, #59500, #30926, .T. ) ;
#4569 = CARTESIAN_POINT ( 'NONE',  ( -16.60577576646023346, 5.000000000000006217, 4.095239503579248533E-30 ) ) ;
#4570 = EDGE_CURVE ( 'NONE', #4686, #38412, #25495, .T. ) ;
#4571 = CARTESIAN_POINT ( 'NONE',  ( 0.5848930533535030563, 36.69111421824766239, -29.20676667847815722 ) ) ;
#4572 = ORIENTED_EDGE ( 'NONE', *, *, #27146, .F. ) ;
#4573 = AXIS2_PLACEMENT_3D ( 'NONE', #30505, #45268, #54303 ) ;
#4574 = ADVANCED_FACE ( 'NONE', ( #35540 ), #3633, .F. ) ;
#4575 = CARTESIAN_POINT ( 'NONE',  ( 0.5797568665920713737, 16.26612276559258063, -43.98452635616917661 ) ) ;
#4576 = CARTESIAN_POINT ( 'NONE',  ( -6.001507490154111224, -11.48377994779711386, 14.94036486426009525 ) ) ;
#4577 = CARTESIAN_POINT ( 'NONE',  ( 3.376099380956842921, 12.15487954915009716, -5.653962042472503668 ) ) ;
#4578 = CARTESIAN_POINT ( 'NONE',  ( 0.6041374136657475802, 38.05989626241390766, 29.42442150067210349 ) ) ;
#4579 = CARTESIAN_POINT ( 'NONE',  ( 0.9762797500689124330, -6.471194619075845367, 41.40589843715202534 ) ) ;
#4580 = FACE_OUTER_BOUND ( 'NONE', #55032, .T. ) ;
#4581 = CARTESIAN_POINT ( 'NONE',  ( -6.015611763856276717, 4.882992715191555533, -18.19956619163653500 ) ) ;
#4582 = CARTESIAN_POINT ( 'NONE',  ( 0.6023143664670691511, 47.66103278671581478, 6.538774821499355738 ) ) ;
#4583 = LINE ( 'NONE', #57831, #36410 ) ;
#4584 = DIRECTION ( 'NONE',  ( 1.000000000000000000, 1.836909530733573776E-16, 0.000000000000000000 ) ) ;
#4585 = EDGE_LOOP ( 'NONE', ( #53563, #31360, #38347, #61022 ) ) ;
#4586 = CARTESIAN_POINT ( 'NONE',  ( -6.015611763856276717, 0.006214430185405465240, -18.84324252354755203 ) ) ;
#4587 = CARTESIAN_POINT ( 'NONE',  ( 5.974727161628367256, -2.663664384318932932, 20.35137732084671214 ) ) ;
#4588 = CARTESIAN_POINT ( 'NONE',  ( -4.000000000000000000, -2.309401076758531346, -0.3572655899081733644 ) ) ;
#4589 = CARTESIAN_POINT ( 'NONE',  ( 1.231276596079881935, -41.24008908601427237, 7.518764738683684001 ) ) ;
#4590 = DIRECTION ( 'NONE',  ( 0.1305261922200468827, -0.9914448613738110483, 0.000000000000000000 ) ) ;
#4591 = ORIENTED_EDGE ( 'NONE', *, *, #29836, .F. ) ;
#4592 = CARTESIAN_POINT ( 'NONE',  ( 0.9736507210033050752, 11.54000710819872033, -41.32746151989287853 ) ) ;
#4593 = DIRECTION ( 'NONE',  ( -0.000000000000000000, -1.000000000000000000, -0.000000000000000000 ) ) ;
#4594 = CARTESIAN_POINT ( 'NONE',  ( 2.281351352603297133, -32.98025003937392086, -34.83869092251595134 ) ) ;
#4595 = ORIENTED_EDGE ( 'NONE', *, *, #17307, .T. ) ;
#4596 = CARTESIAN_POINT ( 'NONE',  ( 0.9762797500689124330, -41.16654106227468901, -7.851158013551661874 ) ) ;
#4597 = B_SPLINE_CURVE_WITH_KNOTS ( 'NONE', 3,
 ( #48096, #5147, #26904, #47480, #47792, #61548 ),
 .UNSPECIFIED., .F., .F.,
 ( 4, 2, 4 ),
 ( 2.538052214298621590E-18, 0.0002447193893791698707, 0.0004894387787583371393 ),
 .UNSPECIFIED. ) ;
#4598 = FACE_OUTER_BOUND ( 'NONE', #7332, .T. ) ;
#4599 = FACE_OUTER_BOUND ( 'NONE', #27913, .T. ) ;
#4600 = VERTEX_POINT ( 'NONE', #54602 ) ;
#4601 = EDGE_CURVE ( 'NONE', #40739, #47659, #33783, .T. ) ;
#4602 = AXIS2_PLACEMENT_3D ( 'NONE', #19390, #61048, #61651 ) ;
#4603 = ORIENTED_EDGE ( 'NONE', *, *, #51852, .F. ) ;
#4604 = CARTESIAN_POINT ( 'NONE',  ( 0.1129192098497447394, 42.02659449688918869, 13.44310763102032702 ) ) ;
#4605 = CARTESIAN_POINT ( 'NONE',  ( 1.227938101723756947, 42.91134962331487657, -0.8460948827226678626 ) ) ;
#4606 = VECTOR ( 'NONE', #56488, 1000.000000000000114 ) ;
#4607 = ORIENTED_EDGE ( 'NONE', *, *, #60043, .F. ) ;
#4608 = VECTOR ( 'NONE', #1950, 1000.000000000000000 ) ;
#4609 = CARTESIAN_POINT ( 'NONE',  ( 0.8560838555295158248, -46.85553835019179303, 2.220666565569249684 ) ) ;
#4610 = CARTESIAN_POINT ( 'NONE',  ( 5.999999999999998224, 6.934333478519240412E-15, 0.000000000000000000 ) ) ;
#4611 = CARTESIAN_POINT ( 'NONE',  ( 0.9756008150404605894, 21.57722292874457892, 37.08855330282507623 ) ) ;
#4612 = CARTESIAN_POINT ( 'NONE',  ( 0.5839254288179563934, -38.05364096126336193, 29.08514953649804369 ) ) ;
#4613 = ORIENTED_EDGE ( 'NONE', *, *, #10966, .T. ) ;
#4614 = CARTESIAN_POINT ( 'NONE',  ( 0.6027444965799114707, -7.708572526967942373, -48.49862292358326954 ) ) ;
#4615 = ORIENTED_EDGE ( 'NONE', *, *, #48856, .T. ) ;
#4616 = CARTESIAN_POINT ( 'NONE',  ( 5.901764892641288895, -46.46096922681069685, 15.47158058974670425 ) ) ;
#4617 = ORIENTED_EDGE ( 'NONE', *, *, #10329, .F. ) ;
#4618 = ORIENTED_EDGE ( 'NONE', *, *, #33526, .F. ) ;
#4619 = CARTESIAN_POINT ( 'NONE',  ( -69.95594261585601714, 9.797174393178825657E-16, -8.000000000000000000 ) ) ;
#4621 = VECTOR ( 'NONE', #44183, 1000.000000000000114 ) ;
#4620 = LINE ( 'NONE', #9660, #22403 ) ;
#4622 = CARTESIAN_POINT ( 'NONE',  ( 4.967162193818130511, 0.000000000000000000, 0.000000000000000000 ) ) ;
#4623 = CARTESIAN_POINT ( 'NONE',  ( 4.999999999999983125, 80.00000000000001421, -3.562970397116383044E-32 ) ) ;
#4624 = ORIENTED_EDGE ( 'NONE', *, *, #39334, .T. ) ;
#4625 = CARTESIAN_POINT ( 'NONE',  ( 0.9741495583595159991, 0.3955098476637576299, -42.90659993968958474 ) ) ;
#4626 = CARTESIAN_POINT ( 'NONE',  ( 0.1135584504625008206, -38.65644560369402427, 21.27513255949062554 ) ) ;
#4627 = VERTEX_POINT ( 'NONE', #8864 ) ;
#4628 = B_SPLINE_CURVE_WITH_KNOTS ( 'NONE', 3,
 ( #40861, #41470, #12650, #7600 ),
 .UNSPECIFIED., .F., .F.,
 ( 4, 4 ),
 ( 0.000000000000000000, 0.005014147105413710795 ),
 .UNSPECIFIED. ) ;
#4629 = EDGE_CURVE ( 'NONE', #35341, #15373, #10576, .T. ) ;
#4630 =( BOUNDED_SURFACE ( )  B_SPLINE_SURFACE ( 3, 1, ( 
 ( #13170, #56357 ),
 ( #56976, #32270 ),
 ( #31647, #50738 ),
 ( #51661, #60432 ) ),
 .UNSPECIFIED., .F., .F., .F. ) 
 B_SPLINE_SURFACE_WITH_KNOTS ( ( 4, 4 ),
 ( 2, 2 ),
 ( 0.000000000000000000, 1.000000000000000000 ),
 ( 0.000000000000000000, 1.000000000000000000 ),
 .UNSPECIFIED. ) 
 GEOMETRIC_REPRESENTATION_ITEM ( )  RATIONAL_B_SPLINE_SURFACE ( (
 ( 1.000000000000000000, 1.000000000000000000),
 ( 0.7223157951917476005, 0.9931996967497186413),
 ( 0.7223157951917476005, 0.9931996967497186413),
 ( 1.000000000000000000, 1.000000000000000000) ) ) 
 REPRESENTATION_ITEM ( '' )  SURFACE ( )  );
#4631 = VERTEX_POINT ( 'NONE', #26739 ) ;
#4632 = CARTESIAN_POINT ( 'NONE',  ( 0.1098349054025746230, -21.37724154645476204, -37.45309339978476970 ) ) ;
#4633 = CARTESIAN_POINT ( 'NONE',  ( 4.999999999999997335, 8.388739760877188892E-13, -80.00000000000001421 ) ) ;
#4634 = CARTESIAN_POINT ( 'NONE',  ( 0.8753041380234524160, 28.81806460335452158, 39.75748332565662935 ) ) ;
#4635 = CARTESIAN_POINT ( 'NONE',  ( 0.3622758884714600280, -42.62881903538205108, -6.444611261694439541 ) ) ;
#4636 = CARTESIAN_POINT ( 'NONE',  ( 0.1119898979215350338, -42.53546966996757561, 11.73435674449596533 ) ) ;
#4637 = ORIENTED_EDGE ( 'NONE', *, *, #31836, .T. ) ;
#4638 = EDGE_CURVE ( 'NONE', #43273, #9908, #27664, .T. ) ;
#4639 = ORIENTED_EDGE ( 'NONE', *, *, #48856, .F. ) ;
#4640 = EDGE_CURVE ( 'NONE', #47523, #47700, #46798, .T. ) ;
#4641 = CARTESIAN_POINT ( 'NONE',  ( 0.6252788684277217346, -34.79439316893326861, 34.65248238119973934 ) ) ;
#4642 = CARTESIAN_POINT ( 'NONE',  ( 2.359973842542475886, 42.89855597191755976, -9.891905284461445902 ) ) ;
#4643 = CARTESIAN_POINT ( 'NONE',  ( 4.060580049360325461, -39.37537800281265987, -19.52043292283310549 ) ) ;
#4644 = CARTESIAN_POINT ( 'NONE',  ( 0.9754642270333668819, -21.60621846558666803, 37.07163437210444101 ) ) ;
#4645 = CARTESIAN_POINT ( 'NONE',  ( 0.6031356755852232965, 4.336951783013129340E-16, 48.10744332413860747 ) ) ;
#4646 =( BOUNDED_SURFACE ( )  B_SPLINE_SURFACE ( 3, 1, ( 
 ( #46311, #16879 ),
 ( #17181, #8368 ),
 ( #50978, #17795 ),
 ( #41310, #50069 ) ),
 .UNSPECIFIED., .F., .F., .F. ) 
 B_SPLINE_SURFACE_WITH_KNOTS ( ( 4, 4 ),
 ( 2, 2 ),
 ( 0.000000000000000000, 1.000000000000000000 ),
 ( 0.000000000000000000, 1.000000000000000000 ),
 .UNSPECIFIED. ) 
 GEOMETRIC_REPRESENTATION_ITEM ( )  RATIONAL_B_SPLINE_SURFACE ( (
 ( 1.000000000000000000, 1.000000000000000000),
 ( 0.7269869731126817891, 0.9931720237060910339),
 ( 0.7269869731126817891, 0.9931720237060910339),
 ( 1.000000000000000000, 1.000000000000000000) ) ) 
 REPRESENTATION_ITEM ( '' )  SURFACE ( )  );
#4647 = ORIENTED_EDGE ( 'NONE', *, *, #16498, .T. ) ;
#4648 = CARTESIAN_POINT ( 'NONE',  ( 4.549368137175248350, 0.000000000000000000, 0.000000000000000000 ) ) ;
#4649 = CARTESIAN_POINT ( 'NONE',  ( 0.8753041380234471980, -24.68967207985765100, -42.44476905888495111 ) ) ;
#4650 = CONICAL_SURFACE ( 'NONE', #33726, 43.92652462719577500, 1.486293639869522343 ) ;
#4651 = CARTESIAN_POINT ( 'NONE',  ( 0.7056555295713299314, -46.47980662829223775, -11.58338207350448457 ) ) ;
#4653 = ADVANCED_FACE ( 'NONE', ( #3837 ), #10071, .F. ) ;
#4652 = CARTESIAN_POINT ( 'NONE',  ( 0.8554163680231708922, -46.74230100997657900, -4.045092014350431420 ) ) ;
#4654 = VECTOR ( 'NONE', #43590, 1000.000000000000000 ) ;
#4655 = LINE ( 'NONE', #42931, #1183 ) ;
#4656 = EDGE_CURVE ( 'NONE', #59176, #22696, #56161, .T. ) ;
#4657 = LINE ( 'NONE', #28485, #50169 ) ;
#4658 = CARTESIAN_POINT ( 'NONE',  ( 0.5837800005270546988, 22.53733638163336650, -41.12546324921934371 ) ) ;
#4659 = CARTESIAN_POINT ( 'NONE',  ( -6.015611763856276717, 14.95313250337445332, -11.46610900684707701 ) ) ;
#4660 = VECTOR ( 'NONE', #33607, 1000.000000000000114 ) ;
#4661 = EDGE_LOOP ( 'NONE', ( #53308, #17039 ) ) ;
#4662 = CARTESIAN_POINT ( 'NONE',  ( 0.1092565886968784733, 37.50119754628579472, 21.29292791075599567 ) ) ;
#4663 = CARTESIAN_POINT ( 'NONE',  ( 0.5807400328401574052, -41.75144119563869793, -23.47602859900758787 ) ) ;
#4664 = CARTESIAN_POINT ( 'NONE',  ( 3.680882792899935918, 39.15943299201950367, 27.71664061799161871 ) ) ;
#4665 = CARTESIAN_POINT ( 'NONE',  ( 0.5980894510889457338, -41.31170365136905787, 24.66136644716748449 ) ) ;
#4666 = VERTEX_POINT ( 'NONE', #18578 ) ;
#4667 = CARTESIAN_POINT ( 'NONE',  ( 4.967162193818130511, -2.375726030842872927, 43.02067033766017801 ) ) ;
#4668 = CARTESIAN_POINT ( 'NONE',  ( 4.967162193818131399, 18.65818244221258126, 38.83676580803773248 ) ) ;
#4669 = AXIS2_PLACEMENT_3D ( 'NONE', #42241, #57511, #14038 ) ;
#4670 = B_SPLINE_CURVE_WITH_KNOTS ( 'NONE', 3,
 ( #36128, #59583, #12313, #35812, #54251, #16377, #48965, #7260, #26388, #16693, #54879, #45519, #11370, #25148, #1323, #53949, #49261, #30456, #37667, #32029, #3189, #2879, #60200, #27940, #22010 ),
 .UNSPECIFIED., .F., .F.,
 ( 4, 3, 3, 3, 3, 3, 3, 3, 4 ),
 ( 5.818439421673296370E-18, 0.0005656085177311399653, 0.001131215744874499839, 0.001696821861372766350, 0.002262427090022498151, 0.002828031679238745492, 0.003393635864401603995, 0.003977030878808131623, 0.004561030005651159000 ),
 .UNSPECIFIED. ) ;
#4671 = B_SPLINE_CURVE_WITH_KNOTS ( 'NONE', 3,
 ( #48222, #57579, #14714, #14106 ),
 .UNSPECIFIED., .F., .F.,
 ( 4, 4 ),
 ( 2.168404344971008868E-19, 0.004041751736740997747 ),
 .UNSPECIFIED. ) ;
#4672 = CARTESIAN_POINT ( 'NONE',  ( 0.3622758884714600280, 36.91764744403290166, 22.26738722580180507 ) ) ;
#4673 = EDGE_LOOP ( 'NONE', ( #18615, #11678, #52264, #16868 ) ) ;
#4674 = CARTESIAN_POINT ( 'NONE',  ( 0.8551540677456834771, 46.03951182599446668, -13.28067116677153692 ) ) ;
#4675 = EDGE_CURVE ( 'NONE', #14380, #60198, #4422, .T. ) ;
#4676 = CARTESIAN_POINT ( 'NONE',  ( 1.227938101723756947, 42.43379953535195170, -6.439911493064139236 ) ) ;
#4677 = CARTESIAN_POINT ( 'NONE',  ( 4.967162193818130511, -7.970725651240091025, 42.34252806656591162 ) ) ;
#4678 = ORIENTED_EDGE ( 'NONE', *, *, #51528, .F. ) ;
#4679 = CARTESIAN_POINT ( 'NONE',  ( 4.956653778116982600, -47.94889704119054130, 3.690426056929806631 ) ) ;
#4680 = VERTEX_POINT ( 'NONE', #37389 ) ;
#4681 = CARTESIAN_POINT ( 'NONE',  ( 0.5988103564986356764, 33.58571500783059349, -34.44345003622217405 ) ) ;
#4682 = VERTEX_POINT ( 'NONE', #17653 ) ;
#4683 = CARTESIAN_POINT ( 'NONE',  ( 0.9762797500689124330, -6.471194619075235188, -41.40589843715211771 ) ) ;
#4684 = DIRECTION ( 'NONE',  ( -1.000000000000000000, 0.000000000000000000, 0.000000000000000000 ) ) ;
#4685 = EDGE_CURVE ( 'NONE', #28949, #9908, #9014, .T. ) ;
#4686 = VERTEX_POINT ( 'NONE', #32682 ) ;
#4687 = CARTESIAN_POINT ( 'NONE',  ( 5.895596859100789899, 5.955534046174526530, -19.21092911436986128 ) ) ;
#4688 = ORIENTED_EDGE ( 'NONE', *, *, #19755, .F. ) ;
#4689 = CARTESIAN_POINT ( 'NONE',  ( 0.1365634738349431054, -43.83788975358855566, 5.010193766259522619 ) ) ;
#4690 = CARTESIAN_POINT ( 'NONE',  ( 0.5837800304671211249, 40.32620748771655883, 23.93813530409446599 ) ) ;
#4691 = AXIS2_PLACEMENT_3D ( 'NONE', #16594, #60110, #25989 ) ;
#4692 = ORIENTED_EDGE ( 'NONE', *, *, #7190, .T. ) ;
#4693 = CARTESIAN_POINT ( 'NONE',  ( 0.9757892942422820015, -16.46777583825573998, -39.62259979733200765 ) ) ;
#4694 = AXIS2_PLACEMENT_3D ( 'NONE', #28379, #10514, #39346 ) ;
#4695 = B_SPLINE_CURVE_WITH_KNOTS ( 'NONE', 3,
 ( #35484, #1306, #24837, #34549 ),
 .UNSPECIFIED., .F., .F.,
 ( 4, 4 ),
 ( 4.670885906470169154E-18, 0.004566006591234645501 ),
 .UNSPECIFIED. ) ;
#4696 = CARTESIAN_POINT ( 'NONE',  ( 0.5988103622719990193, 5.677495780220407795, 47.77151394449999344 ) ) ;
#4697 = AXIS2_PLACEMENT_3D ( 'NONE', #59102, #58786, #14995 ) ;
#4698 = CARTESIAN_POINT ( 'NONE',  ( 0.9730545539215883499, -34.34678117142574649, 25.71816799638765971 ) ) ;
#4699 = VERTEX_POINT ( 'NONE', #51448 ) ;
#4700 = CARTESIAN_POINT ( 'NONE',  ( 0.09136607875274982415, 12.80000000000000071, 0.000000000000000000 ) ) ;
#4701 = CARTESIAN_POINT ( 'NONE',  ( -6.010958268070873523, 16.31164801516955620, -9.434296419346035023 ) ) ;
#4702 = EDGE_LOOP ( 'NONE', ( #43025, #54070, #21052, #59739 ) ) ;
#4703 = CARTESIAN_POINT ( 'NONE',  ( 2.624215991343608501, 38.92973006074551279, -28.09277600149179932 ) ) ;
#4704 = ORIENTED_EDGE ( 'NONE', *, *, #37160, .F. ) ;
#4705 = CARTESIAN_POINT ( 'NONE',  ( 0.7762777257811899201, -47.60264404062384358, 5.369627942761460382 ) ) ;
#4706 = ORIENTED_EDGE ( 'NONE', *, *, #6470, .T. ) ;
#4707 = CARTESIAN_POINT ( 'NONE',  ( 0.5824936645240097466, 4.331538183493719885, 46.69556677036101888 ) ) ;
#4708 = CARTESIAN_POINT ( 'NONE',  ( 0.1158516988532803521, 25.20378146029254296, -36.21755871030804741 ) ) ;
#4709 = CARTESIAN_POINT ( 'NONE',  ( 4.956445790444026223, 13.43466403631445338, -45.13366650706537797 ) ) ;
#4710 = CARTESIAN_POINT ( 'NONE',  ( 0.9790320750461890542, -22.47781024749384926, -35.37068247885321171 ) ) ;
#4711 = EDGE_CURVE ( 'NONE', #18686, #2381, #41879, .T. ) ;
#4712 = ORIENTED_EDGE ( 'NONE', *, *, #60431, .T. ) ;
#4713 = CARTESIAN_POINT ( 'NONE',  ( 3.238741278300275805, -40.38334873621894161, 14.74792908357233401 ) ) ;
#4714 = EDGE_CURVE ( 'NONE', #12101, #3989, #7937, .T. ) ;
#4715 = CARTESIAN_POINT ( 'NONE',  ( 0.7948884756798498818, -26.19034543985806351, 41.53028353311662357 ) ) ;
#4716 = CARTESIAN_POINT ( 'NONE',  ( 5.965394784446458765, -10.25014670152127394, 17.78272165951783279 ) ) ;
#4717 = CIRCLE ( 'NONE', #54725, 42.08604991992415023 ) ;
#4718 = EDGE_CURVE ( 'NONE', #22109, #42733, #33093, .T. ) ;
#4719 = CARTESIAN_POINT ( 'NONE',  ( 4.956653778116992370, 31.29546495791903027, -36.51451553856384180 ) ) ;
#4720 = CARTESIAN_POINT ( 'NONE',  ( 5.958863334805807099, -16.28335246510375356, 12.49619391867154761 ) ) ;
#4721 = CARTESIAN_POINT ( 'NONE',  ( 0.5997462898726536595, -42.52950339524503676, 24.55184251941493301 ) ) ;
#4722 = DIRECTION ( 'NONE',  ( 0.07836865515943411409, -0.7104869166657137303, 0.6993330359244791516 ) ) ;
#4723 = B_SPLINE_CURVE_WITH_KNOTS ( 'NONE', 3,
 ( #15611, #10912, #3940, #32171, #45984, #3025 ),
 .UNSPECIFIED., .F., .F.,
 ( 4, 2, 4 ),
 ( 6.523258043322125742E-18, 0.0002291472222819933150, 0.0004582944445639800706 ),
 .UNSPECIFIED. ) ;
#4724 = CARTESIAN_POINT ( 'NONE',  ( 0.8560838555295223751, -34.16988317699956923, 32.13708010619405542 ) ) ;
#4725 = CARTESIAN_POINT ( 'NONE',  ( 4.549368137175248350, -32.41327393324121431, -28.14399996863486209 ) ) ;
#4726 = CARTESIAN_POINT ( 'NONE',  ( -6.001507490154110336, -16.31148204059953954, 9.435425682280760284 ) ) ;
#4727 = EDGE_CURVE ( 'NONE', #19604, #47629, #25420, .T. ) ;
#4728 = CARTESIAN_POINT ( 'NONE',  ( 0.1154773475650540809, -43.78456205353491271, -5.464042077644623241 ) ) ;
#4729 = DIRECTION ( 'NONE',  ( 1.836766033387207149E-16, -1.000000000000000000, 0.000000000000000000 ) ) ;
#4730 = CARTESIAN_POINT ( 'NONE',  ( 5.958863334805807099, -7.855954700275490588, -18.96276366205790964 ) ) ;
#4731 = CARTESIAN_POINT ( 'NONE',  ( 2.648799415243708655, 44.76338677751262907, 20.01890774983506205 ) ) ;
#4732 = CARTESIAN_POINT ( 'NONE',  ( 0.5850706913938533704, 47.89601588673689037, 0.1816364388702041144 ) ) ;
#4733 = CARTESIAN_POINT ( 'NONE',  ( 3.661921753702001237, -5.960919088269102772, 46.65938884573115786 ) ) ;
#4734 = CARTESIAN_POINT ( 'NONE',  ( 2.643462169533600914, 47.78621045426875469, -4.896978544601653383 ) ) ;
#4735 = ORIENTED_EDGE ( 'NONE', *, *, #57090, .F. ) ;
#4736 = AXIS2_PLACEMENT_3D ( 'NONE', #11626, #967, #54189 ) ;
#4737 = CARTESIAN_POINT ( 'NONE',  ( 3.238741278300274029, -1.828728677532126312, 42.95313747363660895 ) ) ;
#4738 = CARTESIAN_POINT ( 'NONE',  ( 0.5838002273316438284, 23.82993264414563228, 41.54704836736056706 ) ) ;
#4739 = VECTOR ( 'NONE', #5256, 1000.000000000000114 ) ;
#4740 = CARTESIAN_POINT ( 'NONE',  ( -2.601141883200665639, -14.54530301301458550, 3.351057703021155909 ) ) ;
#4741 = ORIENTED_EDGE ( 'NONE', *, *, #39916, .T. ) ;
#4742 = CARTESIAN_POINT ( 'NONE',  ( 0.2285344041767122802, -23.51740999911909924, -37.32871009328864176 ) ) ;
#4743 = DIRECTION ( 'NONE',  ( -1.718001593797181987E-16, 1.000000000000000000, 0.000000000000000000 ) ) ;
#4744 = UNCERTAINTY_MEASURE_WITH_UNIT (LENGTH_MEASURE( 1.000000000000000082E-05 ), #37630, 'distance_accuracy_value', 'NONE');
#4745 = ORIENTED_EDGE ( 'NONE', *, *, #37228, .T. ) ;
#4746 = ORIENTED_EDGE ( 'NONE', *, *, #5983, .T. ) ;
#4747 =( BOUNDED_SURFACE ( )  B_SPLINE_SURFACE ( 3, 1, ( 
 ( #38068, #18947 ),
 ( #47749, #13944 ),
 ( #23938, #53346 ),
 ( #43062, #29548 ) ),
 .UNSPECIFIED., .F., .F., .F. ) 
 B_SPLINE_SURFACE_WITH_KNOTS ( ( 4, 4 ),
 ( 2, 2 ),
 ( 0.000000000000000000, 1.000000000000000000 ),
 ( 0.000000000000000000, 1.000000000000000000 ),
 .UNSPECIFIED. ) 
 GEOMETRIC_REPRESENTATION_ITEM ( )  RATIONAL_B_SPLINE_SURFACE ( (
 ( 1.000000000000000000, 1.000000000000000000),
 ( 0.9751682680413298332, 0.9999560080971552356),
 ( 0.9751682680413298332, 0.9999560080971552356),
 ( 1.000000000000000000, 1.000000000000000000) ) ) 
 REPRESENTATION_ITEM ( '' )  SURFACE ( )  );
#4748 = CARTESIAN_POINT ( 'NONE',  ( 0.8744876279028263033, -31.30103973185235233, 37.82320666052117275 ) ) ;
#4749 = VERTEX_POINT ( 'NONE', #52374 ) ;
#4750 = CARTESIAN_POINT ( 'NONE',  ( 0.5809828226811617480, -23.47450554821680413, -41.74875432577673706 ) ) ;
#4751 = CARTESIAN_POINT ( 'NONE',  ( 0.8760168074886965917, 24.81951362746078615, -41.20610493656884188 ) ) ;
#4752 = AXIS2_PLACEMENT_3D ( 'NONE', #12793, #7745, #61590 ) ;
#4753 = VERTEX_POINT ( 'NONE', #38318 ) ;
#4754 = EDGE_CURVE ( 'NONE', #7287, #11517, #23890, .T. ) ;
#4755 = ORIENTED_EDGE ( 'NONE', *, *, #3090, .F. ) ;
#4756 = CARTESIAN_POINT ( 'NONE',  ( 0.5999999999999994227, -11.64055411052240352, -1.199999999999999956 ) ) ;
#4757 = EDGE_LOOP ( 'NONE', ( #54458, #18320, #2400, #20330 ) ) ;
#4758 = CARTESIAN_POINT ( 'NONE',  ( 0.1129192098497455998, 42.02659449688937343, -13.44310763101974260 ) ) ;
#4759 = DIRECTION ( 'NONE',  ( -1.000000000000000000, -3.673819061467147552E-16, 1.925929944387234758E-32 ) ) ;
#4760 = AXIS2_PLACEMENT_3D ( 'NONE', #34973, #34350, #54035 ) ;
#4761 = EDGE_CURVE ( 'NONE', #59492, #5803, #11956, .T. ) ;
#4762 = DIRECTION ( 'NONE',  ( 0.9848077530122080203, 0.1736481776669314692, -5.551115123125783935E-17 ) ) ;
#4763 = ORIENTED_EDGE ( 'NONE', *, *, #47753, .F. ) ;
#4764 = CARTESIAN_POINT ( 'NONE',  ( 0.1073791018717483448, 0.4849339620927342054, 43.12183934961191767 ) ) ;
#4765 = B_SPLINE_CURVE_WITH_KNOTS ( 'NONE', 3,
 ( #48497, #38207, #15316, #57255 ),
 .UNSPECIFIED., .F., .F.,
 ( 4, 4 ),
 ( 2.100108283942811974E-17, 0.004444306975806115896 ),
 .UNSPECIFIED. ) ;
#4766 = CARTESIAN_POINT ( 'NONE',  ( 0.8744876279028263033, 48.35212675551510841, -8.510105087370661181 ) ) ;
#4767 = EDGE_LOOP ( 'NONE', ( #52767, #57020, #53304, #7902 ) ) ;
#4768 = EDGE_CURVE ( 'NONE', #55943, #9477, #24497, .T. ) ;
#4769 = TOROIDAL_SURFACE ( 'NONE', #12829, 5.633200000000004870, 0.02570000000000154800 ) ;
#4770 = ORIENTED_EDGE ( 'NONE', *, *, #3143, .T. ) ;
#4771 = CARTESIAN_POINT ( 'NONE',  ( 0.9730545539215883499, -39.44597740938072405, 16.88610103448544209 ) ) ;
#4772 = ORIENTED_EDGE ( 'NONE', *, *, #58101, .F. ) ;
#4773 = CARTESIAN_POINT ( 'NONE',  ( 1.834102595619085285, 34.36982342788820688, 27.54837531313729215 ) ) ;
#4774 = CARTESIAN_POINT ( 'NONE',  ( 3.376099380956838925, 1.798919266859539512, -13.28428669908131354 ) ) ;
#4775 = CARTESIAN_POINT ( 'NONE',  ( 4.975610109902397937, 30.94437158899580353, 37.88001153774800400 ) ) ;
#4776 = CARTESIAN_POINT ( 'NONE',  ( 0.1103744047535531458, 5.590449877750019780, 42.76053735246613741 ) ) ;
#4778 = ORIENTED_EDGE ( 'NONE', *, *, #28555, .T. ) ;
#4777 = B_SPLINE_CURVE_WITH_KNOTS ( 'NONE', 3,
 ( #45613, #36845, #60600, #12409 ),
 .UNSPECIFIED., .F., .F.,
 ( 4, 4 ),
 ( 4.336808689942017255E-19, 0.004048833967417086489 ),
 .UNSPECIFIED. ) ;
#4779 = CARTESIAN_POINT ( 'NONE',  ( 3.270143674763207553, 13.60381564321236425, -1.514386915940453271 ) ) ;
#4780 = CARTESIAN_POINT ( 'NONE',  ( 1.157644175074336923, 41.42449707941300829, 6.404164051371970423 ) ) ;
#4781 = CARTESIAN_POINT ( 'NONE',  ( 0.5806925824938502512, -30.69245420804159252, -35.45695442407362208 ) ) ;
#4782 = ORIENTED_EDGE ( 'NONE', *, *, #14859, .F. ) ;
#4783 = CARTESIAN_POINT ( 'NONE',  ( -6.078075953587585900, 12.01009662667709499, 15.05166945109463406 ) ) ;
#4784 = CARTESIAN_POINT ( 'NONE',  ( 4.956653778116991482, -9.917440902360828758, -47.05699031914960528 ) ) ;
#4785 = CARTESIAN_POINT ( 'NONE',  ( 0.7242486021783839378, -24.75018186179863378, -42.40801764032205057 ) ) ;
#4786 = ADVANCED_FACE ( 'NONE', ( #19821 ), #16465, .F. ) ;
#4787 = VECTOR ( 'NONE', #626, 1000.000000000000000 ) ;
#4788 = AXIS2_PLACEMENT_3D ( 'NONE', #11876, #22481, #36916 ) ;
#4789 = ORIENTED_EDGE ( 'NONE', *, *, #13660, .F. ) ;
#4790 = ORIENTED_EDGE ( 'NONE', *, *, #9257, .F. ) ;
#4791 = CARTESIAN_POINT ( 'NONE',  ( 5.960221823109900008, 18.96526051813969360, 7.849768660536623699 ) ) ;
#4792 = CARTESIAN_POINT ( 'NONE',  ( -6.016761891674564211, 13.32172022638610365, -13.32657647165341253 ) ) ;
#4793 = ADVANCED_FACE ( 'NONE', ( #14809 ), #48471, .F. ) ;
#4794 = CARTESIAN_POINT ( 'NONE',  ( 1.227938101723756947, -17.20315230597815059, -39.32113113558984452 ) ) ;
#4795 = CARTESIAN_POINT ( 'NONE',  ( 0.6845945791218023269, 27.12315006394096883, -38.27193817045177582 ) ) ;
#4796 = PRODUCT_DEFINITION_SHAPE ( 'NONE', 'NONE',  #61999 ) ;
#4797 = CARTESIAN_POINT ( 'NONE',  ( 4.553261556744875094, -39.67390170502071811, 18.85526688551479424 ) ) ;
#4798 = EDGE_CURVE ( 'NONE', #49037, #29670, #17975, .T. ) ;
#4799 = CARTESIAN_POINT ( 'NONE',  ( 0.9752132459055863345, -42.51031254975317353, 5.831562321021412920 ) ) ;
#4800 = CARTESIAN_POINT ( 'NONE',  ( 5.960721111146673579, 10.26825948882926021, -17.77250458025982027 ) ) ;
#4801 = CARTESIAN_POINT ( 'NONE',  ( 0.3622758884714730732, -17.25816669464967035, -39.50828911766992491 ) ) ;
#4802 = CARTESIAN_POINT ( 'NONE',  ( -31.75000000000000000, 0.000000000000000000, 0.000000000000000000 ) ) ;
#4803 = CARTESIAN_POINT ( 'NONE',  ( 0.5848930533535030563, -30.41648929863175255, -35.69468113226083972 ) ) ;
#4804 = CARTESIAN_POINT ( 'NONE',  ( 0.9789233960466692253, 41.90846494442085657, 0.1315022227620240847 ) ) ;
#4805 = DIRECTION ( 'NONE',  ( 0.000000000000000000, 0.000000000000000000, 1.000000000000000000 ) ) ;
#4806 = ORIENTED_EDGE ( 'NONE', *, *, #40163, .T. ) ;
#4807 = CIRCLE ( 'NONE', #8856, 13.50000000000000178 ) ;
#4808 = CARTESIAN_POINT ( 'NONE',  ( -1.139999999999998570, 0.000000000000000000, -6.866799999999992465 ) ) ;
#4809 = CARTESIAN_POINT ( 'NONE',  ( 0.6024113833632039894, 41.03720235841333164, 26.97202053416656042 ) ) ;
#4810 = PLANE ( 'NONE',  #34838 ) ;
#4811 = DIRECTION ( 'NONE',  ( -1.000000000000000000, -3.135800716341471541E-16, -1.298891185607920445E-16 ) ) ;
#4812 = ADVANCED_FACE ( 'NONE', ( #43638 ), #61269, .F. ) ;
#4813 = CARTESIAN_POINT ( 'NONE',  ( 0.6029303876144825880, -24.16699908817990661, 41.59667219751840861 ) ) ;
#4814 = CARTESIAN_POINT ( 'NONE',  ( 0.1101816497532063371, 42.77304337559935732, 5.494186916735864123 ) ) ;
#4815 = ITEM_DEFINED_TRANSFORMATION ( 'NONE', 'NONE', #49916,  #14677 ) ;
#4816 = LINE ( 'NONE', #43083, #3831 ) ;
#4817 = DIRECTION ( 'NONE',  ( 0.000000000000000000, 0.000000000000000000, 1.000000000000000000 ) ) ;
#4818 = AXIS2_PLACEMENT_3D ( 'NONE', #8761, #5275, #56670 ) ;
#4819 = CARTESIAN_POINT ( 'NONE',  ( 0.8551540677456739292, 0.9122407826482417104, -47.90804413217340141 ) ) ;
#4821 = ORIENTED_EDGE ( 'NONE', *, *, #14084, .F. ) ;
#4820 = CARTESIAN_POINT ( 'NONE',  ( 0.9968887458511649369, -6.251925120321736529, 42.45154664631704833 ) ) ;
#4822 = ORIENTED_EDGE ( 'NONE', *, *, #28935, .F. ) ;
#4823 = CARTESIAN_POINT ( 'NONE',  ( 3.270143674763207553, -4.983712007628135154, -12.74832469035458082 ) ) ;
#4824 = B_SPLINE_CURVE_WITH_KNOTS ( 'NONE', 3,
 ( #44811, #6522, #25667, #7784 ),
 .UNSPECIFIED., .F., .F.,
 ( 4, 4 ),
 ( 2.380212715961138075E-17, 0.004564976165746188579 ),
 .UNSPECIFIED. ) ;
#4825 = CARTESIAN_POINT ( 'NONE',  ( 0.1095718737110177587, 39.74279513315650547, 16.74012863188518807 ) ) ;
#4826 = CARTESIAN_POINT ( 'NONE',  ( 4.975801465491694664, 40.15204426031534268, -26.14269827151636605 ) ) ;
#4827 = VERTEX_POINT ( 'NONE', #21659 ) ;
#4828 = CARTESIAN_POINT ( 'NONE',  ( 4.833616638992205949, 35.06988470649569223, -30.15290813935864733 ) ) ;
#4829 = DIRECTION ( 'NONE',  ( 0.000000000000000000, -1.000000000000000000, 1.224646799147349509E-16 ) ) ;
#4830 = CARTESIAN_POINT ( 'NONE',  ( 0.8760168074887076939, -44.77533136581870110, -17.58183840866384884 ) ) ;
#4831 = ADVANCED_BREP_SHAPE_REPRESENTATION ( '', ( #52245, #14677 ), #24835 ) ;
#4832 =( BOUNDED_SURFACE ( )  B_SPLINE_SURFACE ( 3, 1, ( 
 ( #41612, #60680 ),
 ( #17797, #25955 ),
 ( #41311, #17485 ),
 ( #2123, #31271 ) ),
 .UNSPECIFIED., .F., .F., .F. ) 
 B_SPLINE_SURFACE_WITH_KNOTS ( ( 4, 4 ),
 ( 2, 2 ),
 ( 0.000000000000000000, 1.000000000000000000 ),
 ( 0.000000000000000000, 1.000000000000000000 ),
 .UNSPECIFIED. ) 
 GEOMETRIC_REPRESENTATION_ITEM ( )  RATIONAL_B_SPLINE_SURFACE ( (
 ( 1.000000000000000000, 1.000000000000000000),
 ( 0.9751682680413298332, 0.9999560080971552356),
 ( 0.9751682680413298332, 0.9999560080971552356),
 ( 1.000000000000000000, 1.000000000000000000) ) ) 
 REPRESENTATION_ITEM ( '' )  SURFACE ( )  );
#4833 = EDGE_LOOP ( 'NONE', ( #10139, #3603, #36909, #8122 ) ) ;
#4834 = ORIENTED_EDGE ( 'NONE', *, *, #10534, .T. ) ;
#4835 = CARTESIAN_POINT ( 'NONE',  ( 3.238741278300273585, 36.28414388564863913, 23.06029422819016972 ) ) ;
#4836 = VECTOR ( 'NONE', #16035, 1000.000000000000114 ) ;
#4837 = EDGE_CURVE ( 'NONE', #30729, #45266, #5221, .T. ) ;
#4838 = AXIS2_PLACEMENT_3D ( 'NONE', #38064, #61503, #23933 ) ;
#4839 = FACE_OUTER_BOUND ( 'NONE', #54239, .T. ) ;
#4840 = CARTESIAN_POINT ( 'NONE',  ( 0.5834584762367737154, 17.02460257627602402, -43.69666916520123578 ) ) ;
#4841 = EDGE_CURVE ( 'NONE', #2015, #30367, #45981, .T. ) ;
#4842 = FACE_OUTER_BOUND ( 'NONE', #42035, .T. ) ;
#4843 = EDGE_CURVE ( 'NONE', #25596, #57756, #21350, .T. ) ;
#4844 = CARTESIAN_POINT ( 'NONE',  ( 0.6001305935487315502, 18.89378601236001387, 44.24520387813834787 ) ) ;
#4845 = DIRECTION ( 'NONE',  ( 1.000000000000000000, 0.000000000000000000, 0.000000000000000000 ) ) ;
#4846 = ORIENTED_EDGE ( 'NONE', *, *, #1472, .T. ) ;
#4847 = ADVANCED_FACE ( 'NONE', ( #16657, #6283, #35463 ), #6913, .F. ) ;
#4848 = EDGE_CURVE ( 'NONE', #45517, #57237, #34971, .T. ) ;
#4849 = B_SPLINE_CURVE_WITH_KNOTS ( 'NONE', 3,
 ( #12761, #31854, #8031, #3312 ),
 .UNSPECIFIED., .F., .F.,
 ( 4, 4 ),
 ( 0.000000000000000000, 0.005013413432710148512 ),
 .UNSPECIFIED. ) ;
#4850 = DIRECTION ( 'NONE',  ( 0.000000000000000000, 0.000000000000000000, 1.000000000000000000 ) ) ;
#4851 = CARTESIAN_POINT ( 'NONE',  ( 0.8753041380234471980, -48.57841546934875510, -7.160717726619150625 ) ) ;
#4852 = CIRCLE ( 'NONE', #61910, 11.40403086437694569 ) ;
#4853 = VERTEX_POINT ( 'NONE', #45186 ) ;
#4854 = CARTESIAN_POINT ( 'NONE',  ( 2.301430502907645170, 17.18551536142187786, 44.85388302506913050 ) ) ;
#4855 = DIRECTION ( 'NONE',  ( 0.09722883295013597105, -0.02434548463872390767, -0.9949642463027805750 ) ) ;
#4856 = CARTESIAN_POINT ( 'NONE',  ( 0.8760168074886965917, -23.27577685234568605, -42.09738177923946978 ) ) ;
#4857 = CARTESIAN_POINT ( 'NONE',  ( 4.549368137175248350, 0.000000000000000000, 0.000000000000000000 ) ) ;
#4858 = VERTEX_POINT ( 'NONE', #10722 ) ;
#4859 = ORIENTED_EDGE ( 'NONE', *, *, #3030, .F. ) ;
#4860 = CARTESIAN_POINT ( 'NONE',  ( 0.8760168074887076939, 28.57146030081979760, -38.69913431881793997 ) ) ;
#4861 = CARTESIAN_POINT ( 'NONE',  ( 4.958415959904821868, 18.66009313388002155, -41.41261737752838457 ) ) ;
#4862 = CARTESIAN_POINT ( 'NONE',  ( 0.1102144999581332746, -37.28370465375341780, -21.67128446981366707 ) ) ;
#4863 = AXIS2_PLACEMENT_3D ( 'NONE', #34990, #49066, #59370 ) ;
#4864 = EDGE_CURVE ( 'NONE', #38640, #44157, #16337, .T. ) ;
#4865 = CARTESIAN_POINT ( 'NONE',  ( 1.600000000000000089, -11.64055411052240352, -1.199999999999999956 ) ) ;
#4866 = ORIENTED_EDGE ( 'NONE', *, *, #32109, .T. ) ;
#4867 = CARTESIAN_POINT ( 'NONE',  ( 0.6041374136657475802, -46.51335992032627331, 12.28249295041966782 ) ) ;
#4868 = ORIENTED_EDGE ( 'NONE', *, *, #53523, .F. ) ;
#4869 = FACE_OUTER_BOUND ( 'NONE', #49548, .T. ) ;
#4870 = CARTESIAN_POINT ( 'NONE',  ( 0.5837800005270549208, 27.81778570091245584, 37.75455015411910153 ) ) ;
#4871 = EDGE_CURVE ( 'NONE', #2370, #34487, #49274, .T. ) ;
#4872 = ORIENTED_EDGE ( 'NONE', *, *, #23185, .F. ) ;
#4873 = CARTESIAN_POINT ( 'NONE',  ( 0.5836750258453351492, -0.1816059738419740499, 47.89563095930319747 ) ) ;
#4874 = CARTESIAN_POINT ( 'NONE',  ( 4.967162193818130511, 0.000000000000000000, 0.000000000000000000 ) ) ;
#4875 = VERTEX_POINT ( 'NONE', #35777 ) ;
#4876 = B_SPLINE_CURVE_WITH_KNOTS ( 'NONE', 3,
 ( #46061, #45135, #17227, #46357, #6862, #2169, #55718, #60412, #36651, #27234, #26001, #3401, #2792, #49803, #59495, #12231 ),
 .UNSPECIFIED., .F., .F.,
 ( 4, 3, 3, 3, 3, 4 ),
 ( 2.221635811791082109E-17, 0.0002612764279487773370, 0.0003919131003184819014, 0.0005225497727000633042, 0.0007837925190632458964, 0.001045051706266715867 ),
 .UNSPECIFIED. ) ;
#4877 = CARTESIAN_POINT ( 'NONE',  ( 0.5832367798473387932, -18.07699868820156652, -44.35360901387667099 ) ) ;
#4878 = CARTESIAN_POINT ( 'NONE',  ( 4.962356264823608143, 0.000000000000000000, 0.000000000000000000 ) ) ;
#4879 = CARTESIAN_POINT ( 'NONE',  ( 1.088313998177380837, 26.73848503423903722, -33.56520876252038477 ) ) ;
#4880 = B_SPLINE_CURVE_WITH_KNOTS ( 'NONE', 3,
 ( #30902, #15896, #44123, #1152, #6445, #21201, #54689, #20288, #59396, #49090, #35316, #50016, #30281 ),
 .UNSPECIFIED., .F., .F.,
 ( 4, 3, 3, 3, 4 ),
 ( 0.0004849530346204834448, 0.0005237000248299427795, 0.0006546240681324977167, 0.0007855481115631319502, 0.0009699050456655105082 ),
 .UNSPECIFIED. ) ;
#4881 = CARTESIAN_POINT ( 'NONE',  ( 4.000000000000003553, -0.7779732554280839318, -0.03354435108168055818 ) ) ;
#4882 = CYLINDRICAL_SURFACE ( 'NONE', #58784, 5.612499999999999822 ) ;
#4883 = ORIENTED_EDGE ( 'NONE', *, *, #31403, .F. ) ;
#4884 = CARTESIAN_POINT ( 'NONE',  ( 0.7764139734771230428, -42.25777068362622657, 20.35488363407972656 ) ) ;
#4885 = CARTESIAN_POINT ( 'NONE',  ( 0.9268187852002115479, -16.93486955123884385, 40.70582914265657593 ) ) ;
#4886 = ORIENTED_EDGE ( 'NONE', *, *, #5994, .F. ) ;
#4887 = AXIS2_PLACEMENT_3D ( 'NONE', #34819, #1263, #29472 ) ;
#4888 = CARTESIAN_POINT ( 'NONE',  ( 4.549368137175248350, 32.13400537129885493, 28.46244473166684941 ) ) ;
#4889 = CARTESIAN_POINT ( 'NONE',  ( 1.092182651088185796, 32.40425343836902528, -26.58431010096432345 ) ) ;
#4890 = CARTESIAN_POINT ( 'NONE',  ( 1.827119703190779765, 4.394694966566483174, -42.82501615430326325 ) ) ;
#4891 = DIRECTION ( 'NONE',  ( -0.1024043820194934645, 0.5950744814819184381, 0.7971196296869318410 ) ) ;
#4892 = B_SPLINE_CURVE_WITH_KNOTS ( 'NONE', 3,
 ( #45453, #13167, #31959, #31330, #36365, #41077 ),
 .UNSPECIFIED., .F., .F.,
 ( 4, 2, 4 ),
 ( 7.152448122690996019E-18, 0.0002291472222819938029, 0.0004582944445639804501 ),
 .UNSPECIFIED. ) ;
#4893 = EDGE_CURVE ( 'NONE', #19414, #8016, #17236, .T. ) ;
#4894 = CARTESIAN_POINT ( 'NONE',  ( 4.956445790443988031, 47.01859095792194410, 2.605792484304518375 ) ) ;
#4895 = PLANE ( 'NONE',  #1056 ) ;
#4896 = CARTESIAN_POINT ( 'NONE',  ( 0.5832367798473377940, -47.89515946578899985, -0.2724222379465481292 ) ) ;
#4897 = CARTESIAN_POINT ( 'NONE',  ( -20.52630000000024069, 1.965116437629976787E-15, 1.136610612372677487E-20 ) ) ;
#4898 = DIRECTION ( 'NONE',  ( 3.273063162220391312E-16, -1.000000000000000000, -5.236901059552626099E-15 ) ) ;
#4899 = EDGE_CURVE ( 'NONE', #58253, #61214, #33657, .T. ) ;
#4900 = CARTESIAN_POINT ( 'NONE',  ( 4.975801465491695552, 0.000000000000000000, 0.000000000000000000 ) ) ;
#4901 = AXIS2_PLACEMENT_3D ( 'NONE', #38435, #9283, #18701 ) ;
#4902 = CARTESIAN_POINT ( 'NONE',  ( 4.956653778116991482, -31.29546495791826644, -36.51451553856450971 ) ) ;
#4904 = VERTEX_POINT ( 'NONE', #50166 ) ;
#4903 = DIRECTION ( 'NONE',  ( -0.07439287786467652097, 0.9903339163990674265, 0.1170659376278869457 ) ) ;
#4905 = ORIENTED_EDGE ( 'NONE', *, *, #40245, .T. ) ;
#4906 = CIRCLE ( 'NONE', #24969, 2.649999999999997691 ) ;
#4907 = CARTESIAN_POINT ( 'NONE',  ( 1.157644175074337145, -2.225587469958278941, 41.85748482521073299 ) ) ;
#4908 = CARTESIAN_POINT ( 'NONE',  ( 5.960721111146673579, -20.52557019979492026, -0.006321279846748652925 ) ) ;
#4909 = CARTESIAN_POINT ( 'NONE',  ( 0.000000000000000000, 0.000000000000000000, -5.600000000000000533 ) ) ;
#4910 = CARTESIAN_POINT ( 'NONE',  ( 0.1073791018717483448, 16.95003405440257893, 39.65380858626220828 ) ) ;
#4911 = DIRECTION ( 'NONE',  ( 0.07836865515943411409, -0.3742079063794905847, -0.9240274869783798861 ) ) ;
#4912 = ORIENTED_EDGE ( 'NONE', *, *, #5318, .T. ) ;
#4913 = CARTESIAN_POINT ( 'NONE',  ( 4.956653778116990594, -35.79382859084093127, -32.11725092155079864 ) ) ;
#4914 =( BOUNDED_SURFACE ( )  B_SPLINE_SURFACE ( 3, 1, ( 
 ( #32158, #27757 ),
 ( #45966, #3010 ),
 ( #31850, #50932 ),
 ( #13060, #31529 ) ),
 .UNSPECIFIED., .F., .F., .F. ) 
 B_SPLINE_SURFACE_WITH_KNOTS ( ( 4, 4 ),
 ( 2, 2 ),
 ( 0.000000000000000000, 1.000000000000000000 ),
 ( 0.000000000000000000, 1.000000000000000000 ),
 .UNSPECIFIED. ) 
 GEOMETRIC_REPRESENTATION_ITEM ( )  RATIONAL_B_SPLINE_SURFACE ( (
 ( 1.000000000000000000, 1.000000000000000000),
 ( 0.9953485035131437453, 0.8621029689291523912),
 ( 0.9953485035131437453, 0.8621029689291523912),
 ( 1.000000000000000000, 1.000000000000000000) ) ) 
 REPRESENTATION_ITEM ( '' )  SURFACE ( )  );
#4915 = PLANE ( 'NONE',  #47230 ) ;
#4916 = CARTESIAN_POINT ( 'NONE',  ( -2.739355103387247858, -14.37091041638168676, -4.040358988425336584 ) ) ;
#4917 = ORIENTED_EDGE ( 'NONE', *, *, #7261, .F. ) ;
#4918 = EDGE_CURVE ( 'NONE', #27859, #32871, #61249, .T. ) ;
#4919 = EDGE_CURVE ( 'NONE', #16981, #13219, #32888, .T. ) ;
#4920 = CARTESIAN_POINT ( 'NONE',  ( 5.838029081930955932, 7.836690858011332139, 46.57951625499005388 ) ) ;
#4921 = CARTESIAN_POINT ( 'NONE',  ( 0.5837157313716021534, -25.15714033038016950, -39.57720750608339699 ) ) ;
#4922 = ORIENTED_EDGE ( 'NONE', *, *, #10884, .T. ) ;
#4923 = CIRCLE ( 'NONE', #56938, 42.92674063221959813 ) ;
#4924 = B_SPLINE_CURVE_WITH_KNOTS ( 'NONE', 3,
 ( #453, #24905, #33389, #1074, #18987, #29280 ),
 .UNSPECIFIED., .F., .F.,
 ( 4, 2, 4 ),
 ( 5.421010862427522170E-18, 0.0002291472222819961068, 0.0004582944445639867926 ),
 .UNSPECIFIED. ) ;
#4925 = CARTESIAN_POINT ( 'NONE',  ( -6.077587904424778920, -8.901182807328710922, -17.07527352707552382 ) ) ;
#4926 = ORIENTED_EDGE ( 'NONE', *, *, #42946, .F. ) ;
#4927 = ADVANCED_FACE ( 'NONE', ( #42027 ), #28168, .F. ) ;
#4928 = EDGE_CURVE ( 'NONE', #8016, #33629, #12039, .T. ) ;
#4929 =( BOUNDED_SURFACE ( )  B_SPLINE_SURFACE ( 3, 1, ( 
 ( #53652, #20186 ),
 ( #14566, #16637 ),
 ( #29252, #24248 ),
 ( #39298, #58352 ) ),
 .UNSPECIFIED., .F., .F., .F. ) 
 B_SPLINE_SURFACE_WITH_KNOTS ( ( 4, 4 ),
 ( 2, 2 ),
 ( 0.000000000000000000, 1.000000000000000000 ),
 ( 0.000000000000000000, 1.000000000000000000 ),
 .UNSPECIFIED. ) 
 GEOMETRIC_REPRESENTATION_ITEM ( )  RATIONAL_B_SPLINE_SURFACE ( (
 ( 1.000000000000000000, 1.000000000000000000),
 ( 0.9953485035131437453, 0.8621029689291523912),
 ( 0.9953485035131437453, 0.8621029689291523912),
 ( 1.000000000000000000, 1.000000000000000000) ) ) 
 REPRESENTATION_ITEM ( '' )  SURFACE ( )  );
#4930 = CARTESIAN_POINT ( 'NONE',  ( 52.60613790598473116, 15.41603472375467909, -1.617730826299683899 ) ) ;
#4932 = CARTESIAN_POINT ( 'NONE',  ( 0.8744876279028263033, -14.81965677138014037, 46.80521149998127584 ) ) ;
#4931 = VECTOR ( 'NONE', #6371, 1000.000000000000227 ) ;
#4933 = ORIENTED_EDGE ( 'NONE', *, *, #9400, .F. ) ;
#4934 = EDGE_CURVE ( 'NONE', #44905, #35873, #23219, .T. ) ;
#4935 = CARTESIAN_POINT ( 'NONE',  ( 5.917102823773431552, -20.11192790512648543, 0.008601786823265991991 ) ) ;
#4936 = DIRECTION ( 'NONE',  ( 0.000000000000000000, 0.000000000000000000, 1.000000000000000000 ) ) ;
#4937 = CARTESIAN_POINT ( 'NONE',  ( 0.5980271706414711508, -48.79397779905849575, 5.585425085581966265 ) ) ;
#4938 =( BOUNDED_SURFACE ( )  B_SPLINE_SURFACE ( 3, 1, ( 
 ( #23529, #14159 ),
 ( #57328, #4703 ),
 ( #23848, #52337 ),
 ( #19465, #14462 ) ),
 .UNSPECIFIED., .F., .F., .F. ) 
 B_SPLINE_SURFACE_WITH_KNOTS ( ( 4, 4 ),
 ( 2, 2 ),
 ( 0.000000000000000000, 1.000000000000000000 ),
 ( 0.000000000000000000, 1.000000000000000000 ),
 .UNSPECIFIED. ) 
 GEOMETRIC_REPRESENTATION_ITEM ( )  RATIONAL_B_SPLINE_SURFACE ( (
 ( 1.000000000000000000, 1.000000000000000000),
 ( 0.7269869731126821222, 0.9931720237060910339),
 ( 0.7269869731126821222, 0.9931720237060910339),
 ( 1.000000000000000000, 1.000000000000000000) ) ) 
 REPRESENTATION_ITEM ( '' )  SURFACE ( )  );
#4939 = ORIENTED_EDGE ( 'NONE', *, *, #56201, .T. ) ;
#4940 = CARTESIAN_POINT ( 'NONE',  ( 0.9780106845699476636, -6.661169069550109789, -41.37583924323842410 ) ) ;
#4941 = ORIENTED_EDGE ( 'NONE', *, *, #32751, .T. ) ;
#4942 = FACE_OUTER_BOUND ( 'NONE', #1378, .T. ) ;
#4943 = EDGE_CURVE ( 'NONE', #55095, #58934, #3756, .T. ) ;
#4944 = ORIENTED_EDGE ( 'NONE', *, *, #27298, .F. ) ;
#4945 = VERTEX_POINT ( 'NONE', #41714 ) ;
#4946 = CARTESIAN_POINT ( 'NONE',  ( 3.238931869106854489, 38.11291514434414296, 19.89273896137497033 ) ) ;
#4947 = CARTESIAN_POINT ( 'NONE',  ( 0.6846871229502932144, 44.58493949244030574, -17.53234844287693761 ) ) ;
#4948 = DIRECTION ( 'NONE',  ( -1.000000000000000000, -0.000000000000000000, -0.000000000000000000 ) ) ;
#4949 = CARTESIAN_POINT ( 'NONE',  ( -1.400000000000000355, 0.000000000000000000, 0.000000000000000000 ) ) ;
#4950 = ORIENTED_EDGE ( 'NONE', *, *, #14403, .F. ) ;
#4951 = CARTESIAN_POINT ( 'NONE',  ( 5.896782393890504181, -4.656380635072583374, -19.56640504178867346 ) ) ;
#4952 = CARTESIAN_POINT ( 'NONE',  ( 5.901463166500146684, 12.97422524546425926, -15.36838799681328105 ) ) ;
#4953 = CARTESIAN_POINT ( 'NONE',  ( 0.2279481005628812007, -28.09744832277539928, 34.01524488845964100 ) ) ;
#4954 = ORIENTED_EDGE ( 'NONE', *, *, #51336, .F. ) ;
#4955 = ORIENTED_EDGE ( 'NONE', *, *, #2318, .F. ) ;
#4956 = SURFACE_STYLE_USAGE ( .BOTH. , #56659 ) ;
#4957 = DIRECTION ( 'NONE',  ( -1.000000000000000000, -1.836909530733554547E-16, -1.836909530733573529E-16 ) ) ;
#4958 = CARTESIAN_POINT ( 'NONE',  ( 4.962356264823608143, 30.91935898304044272, 28.55221248765537467 ) ) ;
#4959 = DIRECTION ( 'NONE',  ( 0.9848077530122080203, 0.1736481776669314692, -5.551115123125783935E-17 ) ) ;
#4960 = CARTESIAN_POINT ( 'NONE',  ( 0.9730545539215883499, -26.52009130076748278, -33.73144377768585400 ) ) ;
#4961 = VERTEX_POINT ( 'NONE', #60776 ) ;
#4962 = VERTEX_POINT ( 'NONE', #27282 ) ;
#4963 = CARTESIAN_POINT ( 'NONE',  ( 0.6025881611877910160, 12.24025891548858347, 46.52425620537273687 ) ) ;
#4964 = CARTESIAN_POINT ( 'NONE',  ( 0.3676999524040366896, 43.13409918076302318, -9.241215893319285613 ) ) ;
#4965 = FACE_OUTER_BOUND ( 'NONE', #39554, .T. ) ;
#4966 = CARTESIAN_POINT ( 'NONE',  ( 0.9730545539215883499, -21.01499094264575618, 37.40983423658466478 ) ) ;
#4967 = CARTESIAN_POINT ( 'NONE',  ( 0.5806925824938499181, 5.237374507879953178, -46.60249210726582447 ) ) ;
#4968 = CARTESIAN_POINT ( 'NONE',  ( -2.708315649062910779, -5.356004933109375088, -13.61924161399631394 ) ) ;
#4969 = EDGE_CURVE ( 'NONE', #16055, #20290, #28420, .T. ) ;
#4970 = VERTEX_POINT ( 'NONE', #32607 ) ;
#4971 = CARTESIAN_POINT ( 'NONE',  ( 1.231276596079881047, -39.86997064245551314, 12.94844438485960580 ) ) ;
#4972 = CARTESIAN_POINT ( 'NONE',  ( 1.231276596079881935, 10.53918392497884149, -40.57341954055061706 ) ) ;
#4973 = LINE ( 'NONE', #61370, #48861 ) ;
#4974 = AXIS2_PLACEMENT_3D ( 'NONE', #49408, #20908, #58787 ) ;
#4975 = CARTESIAN_POINT ( 'NONE',  ( 5.272379999999998290, 0.000000000000000000, 0.000000000000000000 ) ) ;
#4976 = DIRECTION ( 'NONE',  ( 0.1736481776669316079, -0.9848077530122079093, -5.551115123125822145E-17 ) ) ;
#4977 = CARTESIAN_POINT ( 'NONE',  ( 4.553261556744875094, 27.56395660609745235, -34.20186927699732138 ) ) ;
#4978 = VERTEX_POINT ( 'NONE', #27899 ) ;
#4979 = CARTESIAN_POINT ( 'NONE',  ( 1.227938101723748288, -39.32113113558953899, -17.20315230597885758 ) ) ;
#4980 = VECTOR ( 'NONE', #14404, 1000.000000000000000 ) ;
#4981 = CARTESIAN_POINT ( 'NONE',  ( 0.5850706913938534814, 29.30134895053053867, 37.88789093229816274 ) ) ;
#4982 = CARTESIAN_POINT ( 'NONE',  ( 2.879087469061463178, 40.36424033792948052, 17.51655727376944327 ) ) ;
#4983 = CARTESIAN_POINT ( 'NONE',  ( 0.5804410086790514622, 40.07081992599749043, -24.36902218624454619 ) ) ;
#4984 = VERTEX_POINT ( 'NONE', #37950 ) ;
#4985 = CARTESIAN_POINT ( 'NONE',  ( 0.3676999524040323597, -0.5887207181719652516, -44.10900124961835900 ) ) ;
#4986 = DIRECTION ( 'NONE',  ( -1.000000000000000000, 0.000000000000000000, -0.000000000000000000 ) ) ;
#4987 = B_SPLINE_CURVE_WITH_KNOTS ( 'NONE', 3,
 ( #23244, #18870, #46449, #51415 ),
 .UNSPECIFIED., .F., .F.,
 ( 4, 4 ),
 ( 0.000000000000000000, 0.005013413432710144176 ),
 .UNSPECIFIED. ) ;
#4988 = EDGE_CURVE ( 'NONE', #41892, #54620, #42002, .T. ) ;
#4989 = CARTESIAN_POINT ( 'NONE',  ( 2.301529144917015657, 33.04216096093403365, -34.86298839095296387 ) ) ;
#4990 = ORIENTED_EDGE ( 'NONE', *, *, #17270, .T. ) ;
#4991 = CARTESIAN_POINT ( 'NONE',  ( 0.5980894510889457338, 47.78766676462068119, 5.583794302585419977 ) ) ;
#4992 = EDGE_CURVE ( 'NONE', #40811, #28532, #55252, .T. ) ;
#4993 = CARTESIAN_POINT ( 'NONE',  ( 0.8557997880470599172, -5.347802024196930404, -47.60865952217005059 ) ) ;
#4994 = VERTEX_POINT ( 'NONE', #9394 ) ;
#4995 = ADVANCED_FACE ( 'NONE', ( #9091 ), #55778, .F. ) ;
#4996 = CARTESIAN_POINT ( 'NONE',  ( 0.9972139404380280236, -6.252633471303094659, -42.45145681504347834 ) ) ;
#4997 = ORIENTED_EDGE ( 'NONE', *, *, #4186, .F. ) ;
#4998 = CARTESIAN_POINT ( 'NONE',  ( 4.956653778116986153, -48.02038484091102077, 2.599733001514167086 ) ) ;
#4999 = EDGE_CURVE ( 'NONE', #28755, #18623, #30638, .T. ) ;
#5000 = ORIENTED_EDGE ( 'NONE', *, *, #30602, .T. ) ;
#5001 = CARTESIAN_POINT ( 'NONE',  ( 0.2285344041767082557, -13.27967145753882505, -42.07316836506711866 ) ) ;
#5002 = CARTESIAN_POINT ( 'NONE',  ( 50.00005079999999680, 12.80000000000000071, -3.000000000000000000 ) ) ;
#5003 = ORIENTED_EDGE ( 'NONE', *, *, #41797, .F. ) ;
#5004 = CARTESIAN_POINT ( 'NONE',  ( 0.1073791018717483448, -37.10214135362904386, 21.98088480513601795 ) ) ;
#5005 = ORIENTED_EDGE ( 'NONE', *, *, #38708, .F. ) ;
#5006 = CARTESIAN_POINT ( 'NONE',  ( 0.8560838555295223751, 11.76118766017263972, 45.40977096290989579 ) ) ;
#5007 =( BOUNDED_SURFACE ( )  B_SPLINE_SURFACE ( 3, 1, ( 
 ( #12817, #12502 ),
 ( #12200, #21267 ),
 ( #60090, #17194 ),
 ( #7448, #11895 ) ),
 .UNSPECIFIED., .F., .F., .F. ) 
 B_SPLINE_SURFACE_WITH_KNOTS ( ( 4, 4 ),
 ( 2, 2 ),
 ( 0.000000000000000000, 1.000000000000000000 ),
 ( 0.000000000000000000, 1.000000000000000000 ),
 .UNSPECIFIED. ) 
 GEOMETRIC_REPRESENTATION_ITEM ( )  RATIONAL_B_SPLINE_SURFACE ( (
 ( 1.000000000000000000, 1.000000000000000000),
 ( 0.9952954269826590483, 0.8620686068821307169),
 ( 0.9952954269826590483, 0.8620686068821307169),
 ( 1.000000000000000000, 1.000000000000000000) ) ) 
 REPRESENTATION_ITEM ( '' )  SURFACE ( )  );
#5008 = CARTESIAN_POINT ( 'NONE',  ( 4.553261556744875094, 0.000000000000000000, 0.000000000000000000 ) ) ;
#5009 = VECTOR ( 'NONE', #27425, 1000.000000000000114 ) ;
#5010 = ORIENTED_EDGE ( 'NONE', *, *, #1530, .T. ) ;
#5011 = CARTESIAN_POINT ( 'NONE',  ( 4.962356264823601926, 34.44911810793277596, -24.17630781256817940 ) ) ;
#5012 = ADVANCED_FACE ( 'NONE', ( #28817 ), #25788, .F. ) ;
#5013 = B_SPLINE_CURVE_WITH_KNOTS ( 'NONE', 3,
 ( #60989, #57197, #28722, #18097, #3658, #13404 ),
 .UNSPECIFIED., .F., .F.,
 ( 4, 2, 4 ),
 ( 7.040638946443416885E-18, 0.0002445244328975361555, 0.0004890488657950652638 ),
 .UNSPECIFIED. ) ;
#5014 = CARTESIAN_POINT ( 'NONE',  ( 0.6846871229502899947, 19.12907057981204773, 43.92355552798044016 ) ) ;
#5015 = CARTESIAN_POINT ( 'NONE',  ( 0.5837157313716019313, 16.76980906724618947, 43.79509752735039996 ) ) ;
#5016 = VERTEX_POINT ( 'NONE', #52927 ) ;
#5017 = FACE_OUTER_BOUND ( 'NONE', #18234, .T. ) ;
#5018 = EDGE_CURVE ( 'NONE', #44940, #13226, #18822, .T. ) ;
#5019 = CARTESIAN_POINT ( 'NONE',  ( 0.8753041380234465318, 5.600023814136007694, -48.78296896616778611 ) ) ;
#5020 = ORIENTED_EDGE ( 'NONE', *, *, #50205, .F. ) ;
#5021 = CARTESIAN_POINT ( 'NONE',  ( 0.5817216825391120505, 42.99501409996830148, -18.72601705518253823 ) ) ;
#5022 = ORIENTED_EDGE ( 'NONE', *, *, #23207, .T. ) ;
#5023 =( BOUNDED_SURFACE ( )  B_SPLINE_SURFACE ( 3, 1, ( 
 ( #44777, #15334 ),
 ( #20947, #901 ),
 ( #16248, #58513 ),
 ( #6190, #53814 ) ),
 .UNSPECIFIED., .F., .F., .F. ) 
 B_SPLINE_SURFACE_WITH_KNOTS ( ( 4, 4 ),
 ( 2, 2 ),
 ( 0.000000000000000000, 1.000000000000000000 ),
 ( 0.000000000000000000, 1.000000000000000000 ),
 .UNSPECIFIED. ) 
 GEOMETRIC_REPRESENTATION_ITEM ( )  RATIONAL_B_SPLINE_SURFACE ( (
 ( 1.000000000000000000, 1.000000000000000000),
 ( 0.7269869731126821222, 0.9931720237060910339),
 ( 0.7269869731126821222, 0.9931720237060910339),
 ( 1.000000000000000000, 1.000000000000000000) ) ) 
 REPRESENTATION_ITEM ( '' )  SURFACE ( )  );
#5024 = CLOSED_SHELL ( 'NONE', ( #54890, #37656, #19044, #6905, #59239, #60975, #59537, #39181, #4451, #17461, #49863, #60996, #22437, #54355, #7740, #60328, #60028, #15212, #19187, #69, #60294, #27393, #11311, #4360, #22571, #44176, #27324, #42489, #26440, #15604, #28674, #24531, #41241, #23283, #14422, #25542, #25460, #31331, #9949, #39417, #30842, #46764, #55420, #38500, #18972, #51607, #55899, #12000, #18055, #8170, #12556, #56600, #8700, #25819, #59590, #33598, #18849, #41000, #36603, #11904, #28356, #20853, #690, #28326, #391, #14112, #15261, #43799, #47576, #2872, #54371, #17333, #20533, #19453, #15352, #48615, #22640, #2831, #55286, #28983, #55234, #50485, #50302, #61224, #37240, #20528, #11989, #55931, #12226, #20723, #61579, #27740, #59517, #53509, #26925, #5619, #4034, #41323, #57245, #48179, #19601, #26568, #30055, #10485, #17125, #61488, #14431, #6344, #49982, #36023, #4233, #27584, #37449, #48698, #44890, #1118, #13966, #19880, #29834, #22886, #59599, #1196, #36258, #17108, #29284, #55428, #35764, #10913, #49089, #14738, #58841, #38109, #44384, #8053, #42380, #47004, #28543, #32194, #4927, #20654, #14910, #46813, #60483, #53518, #35176, #18402, #23758, #60797, #38621, #54202, #5230, #32281, #22398, #41668, #25307, #58801, #1601, #25360, #22936, #37295, #23936, #49315, #37245, #10700, #56501, #25170, #8200, #7623, #36244, #33666, #34888, #33978, #58405, #14256, #29916, #56724, #5761, #22357, #60645, #1277, #14883, #54933, #57615, #1524, #2492, #7830, #14865, #29058, #42417, #2191, #2949, #12571, #31406, #52108, #30409, #43512, #1606, #57711, #51884, #29353, #8081, #58319, #43599, #46110, #25876, #61662, #61145, #23923, #40589, #55223, #7453, #19970, #46977, #24, #5696, #14509, #28619, #43325, #5195, #34425, #25739, #27502, #49522, #4510, #55076, #22428, #22731, #48802, #22058, #4531, #24904, #21311, #61111, #24382, #45561, #61680, #19525, #6034, #34374, #39963, #56771, #7717, #27660, #11916, #19377, #28226, #11469, #12259, #23161, #23706, #54573, #29991, #30890, #42328, #29019, #29034, #30068, #57384, #48170, #29448, #24196, #54958, #19603, #54639, #53641, #22506, #49203, #57589, #29245, #36481, #54558, #16978, #28219, #47080, #4793, #13678, #10401, #8775, #12961, #20157, #28031, #2237, #50982, #46149, #58217, #51776, #19444, #240, #10784, #53137, #54997, #18630, #23910, #26371, #21940, #51770, #35240, #15101, #52581, #23862, #51108 ) ) ;
#5025 = CARTESIAN_POINT ( 'NONE',  ( 5.838029081930955932, -28.03445132514733729, 38.01492597718512911 ) ) ;
#5026 = CARTESIAN_POINT ( 'NONE',  ( 4.967162193818130511, 28.07411493385295032, 32.68434214048178177 ) ) ;
#5027 = VERTEX_POINT ( 'NONE', #57603 ) ;
#5028 = CARTESIAN_POINT ( 'NONE',  ( 0.9787464366903567692, -34.45072202728288602, -23.86381664129499924 ) ) ;
#5029 = CARTESIAN_POINT ( 'NONE',  ( 0.1156867017252034141, 25.34656052724063358, -36.11778892338390534 ) ) ;
#5030 = CARTESIAN_POINT ( 'NONE',  ( 4.960156602257181468, -26.21519897043455316, 38.31207700265944993 ) ) ;
#5031 = CARTESIAN_POINT ( 'NONE',  ( 0.7246131072078558777, 13.24054562911126176, -46.24389631750676699 ) ) ;
#5032 = AXIS2_PLACEMENT_3D ( 'NONE', #48345, #5404, #393 ) ;
#5033 = VERTEX_POINT ( 'NONE', #24740 ) ;
#5034 = CARTESIAN_POINT ( 'NONE',  ( 0.6001305935487315502, 47.62765676940934867, 6.798494447612393188 ) ) ;
#5035 = FACE_OUTER_BOUND ( 'NONE', #16510, .T. ) ;
#5036 = CARTESIAN_POINT ( 'NONE',  ( 5.895596859100789899, 10.81936814621394127, -16.95492424427719413 ) ) ;
#5037 = DIRECTION ( 'NONE',  ( -0.9848077530122079093, -0.1736481776669316357, -2.245658157333249735E-31 ) ) ;
#5038 = CARTESIAN_POINT ( 'NONE',  ( 3.238018933889920792, 9.111992562714181787, -9.817284955867094709 ) ) ;
#5039 = ADVANCED_FACE ( 'NONE', ( #32925 ), #24119, .T. ) ;
#5040 = CARTESIAN_POINT ( 'NONE',  ( 2.009741617377216460, -8.378475480318341440, -43.23546260014745002 ) ) ;
#5041 = B_SPLINE_CURVE_WITH_KNOTS ( 'NONE', 3,
 ( #33606, #14498, #8858, #61758, #38016, #54 ),
 .UNSPECIFIED., .F., .F.,
 ( 4, 2, 4 ),
 ( 3.402737038855563874E-18, 0.0002447193893791695996, 0.0004894387787583357298 ),
 .UNSPECIFIED. ) ;
#5042 = DIRECTION ( 'NONE',  ( 0.07836865515943411409, -0.3887811538706257286, 0.9179910502197319300 ) ) ;
#5043 = CARTESIAN_POINT ( 'NONE',  ( -16.13943151895728434, -7.933737026945285820, 1.058406808655014908 ) ) ;
#5044 = CARTESIAN_POINT ( 'NONE',  ( 0.2224561200757632085, -22.21411683958078243, 36.95704201588751658 ) ) ;
#5045 = CARTESIAN_POINT ( 'NONE',  ( 0.6017666602106489515, 48.10631669010027878, -0.3491145841133775907 ) ) ;
#5046 = CARTESIAN_POINT ( 'NONE',  ( 0.1095718737110179114, -21.78439022773181932, 37.21776476380618703 ) ) ;
#5047 = CARTESIAN_POINT ( 'NONE',  ( 4.553261556744873317, -9.554252317234828595, 42.87488575474283437 ) ) ;
#5048 = CARTESIAN_POINT ( 'NONE',  ( 4.694002226626920127, -30.39302829899148506, 33.97864921186298659 ) ) ;
#5049 = CARTESIAN_POINT ( 'NONE',  ( 0.9780106845699487739, 9.409895146977072855, 40.83852494616247242 ) ) ;
#5050 = DIRECTION ( 'NONE',  ( -0.07439287786467650709, -0.9262902123089744588, -0.3693942911085744685 ) ) ;
#5051 = CARTESIAN_POINT ( 'NONE',  ( 0.5806925824938499181, -13.37132486740634540, -44.94919391528445374 ) ) ;
#5052 = CARTESIAN_POINT ( 'NONE',  ( -6.078726893082806448, 19.09748444646209009, -2.465791776662926260 ) ) ;
#5053 = EDGE_LOOP ( 'NONE', ( #18208, #9699, #29853, #5600, #14746, #55559 ) ) ;
#5054 = DIRECTION ( 'NONE',  ( 0.000000000000000000, -1.000000000000000000, 0.000000000000000000 ) ) ;
#5055 = CARTESIAN_POINT ( 'NONE',  ( 0.9780303403264759554, -1.076676298148392830, 41.89487297443557878 ) ) ;
#5056 = CARTESIAN_POINT ( 'NONE',  ( -6.016489644550736315, 9.417787539062475233, -16.32089497094051467 ) ) ;
#5057 = VERTEX_POINT ( 'NONE', #24424 ) ;
#5058 = CARTESIAN_POINT ( 'NONE',  ( 0.9756008150404595902, 5.741579752919638402, 42.52260101821268279 ) ) ;
#5059 = CARTESIAN_POINT ( 'NONE',  ( 0.8753041380234465318, -39.87785955339043653, 28.65125905284175190 ) ) ;
#5060 = B_SPLINE_CURVE_WITH_KNOTS ( 'NONE', 3,
 ( #30310, #29695, #48495, #40069, #34417, #15315, #883, #15619, #20020, #39130, #10923, #48811, #5864, #20617, #30007, #25012 ),
 .UNSPECIFIED., .F., .F.,
 ( 4, 3, 3, 3, 3, 4 ),
 ( 1.040890552917501732E-17, 0.0002724568934985577696, 0.0004086836638483818274, 0.0005449104342063615250, 0.0008173270854453666733, 0.001089761613562689659 ),
 .UNSPECIFIED. ) ;
#5062 = EDGE_LOOP ( 'NONE', ( #29514, #1605 ) ) ;
#5061 = AXIS2_PLACEMENT_3D ( 'NONE', #55055, #31895, #12181 ) ;
#5063 = ORIENTED_EDGE ( 'NONE', *, *, #48003, .F. ) ;
#5064 = CARTESIAN_POINT ( 'NONE',  ( 0.9757402383260944667, -11.02350435907874449, -41.46830379850865711 ) ) ;
#5065 = ADVANCED_FACE ( 'NONE', ( #29430, #28196 ), #5298, .T. ) ;
#5066 = ORIENTED_EDGE ( 'NONE', *, *, #2082, .T. ) ;
#5067 = CARTESIAN_POINT ( 'NONE',  ( 0.6846871229502932144, 28.47437962186126370, 38.52803883689310283 ) ) ;
#5068 = ORIENTED_EDGE ( 'NONE', *, *, #27576, .F. ) ;
#5069 = EDGE_CURVE ( 'NONE', #61163, #21206, #29861, .T. ) ;
#5070 = VERTEX_POINT ( 'NONE', #38551 ) ;
#5071 = FACE_OUTER_BOUND ( 'NONE', #34121, .T. ) ;
#5072 = ORIENTED_EDGE ( 'NONE', *, *, #58755, .F. ) ;
#5073 = CARTESIAN_POINT ( 'NONE',  ( -2.708315649062910779, 1.648584381066855897, 14.54141329178162678 ) ) ;
#5074 = CARTESIAN_POINT ( 'NONE',  ( 4.335381028904201628, 20.75278752742067567, 44.37430176922311631 ) ) ;
#5075 = DIRECTION ( 'NONE',  ( 1.000000000000000000, 0.000000000000000000, 0.000000000000000000 ) ) ;
#5076 = EDGE_LOOP ( 'NONE', ( #54357, #40370, #27279, #42837 ) ) ;
#5077 = CARTESIAN_POINT ( 'NONE',  ( 0.6254087463353942278, -44.70339519268203787, -17.77193046492936546 ) ) ;
#5078 = CARTESIAN_POINT ( 'NONE',  ( 0.9757402383260935785, -33.98983788393805128, -26.18833306844188513 ) ) ;
#5079 = EDGE_LOOP ( 'NONE', ( #60052, #47870, #27152, #38634 ) ) ;
#5080 = ORIENTED_EDGE ( 'NONE', *, *, #18952, .T. ) ;
#5081 = CARTESIAN_POINT ( 'NONE',  ( 5.959547316686252039, 18.96183906913543282, -7.858107265727552360 ) ) ;
#5082 = B_SPLINE_CURVE_WITH_KNOTS ( 'NONE', 3,
 ( #58332, #94, #52725, #57719, #11071, #53632, #10762, #15457, #9826, #20460, #14848, #5707, #24540, #399, #19243, #5099 ),
 .UNSPECIFIED., .F., .F.,
 ( 4, 3, 3, 3, 3, 4 ),
 ( 1.962735358247463844E-17, 0.0002612764279487760901, 0.0003919131003184865634, 0.0005225497727000665569, 0.0007837925190632416680, 0.001045051706266717602 ),
 .UNSPECIFIED. ) ;
#5083 = ORIENTED_EDGE ( 'NONE', *, *, #52548, .T. ) ;
#5084 = CARTESIAN_POINT ( 'NONE',  ( 0.6029442701453592290, 46.63311652831155385, 15.39148037114014045 ) ) ;
#5085 = CARTESIAN_POINT ( 'NONE',  ( 0.9722240750034570889, -41.29187379046131667, 11.66659272802842473 ) ) ;
#5086 = CARTESIAN_POINT ( 'NONE',  ( 2.624215991343620935, -7.662883702704355926, -47.39206852872464992 ) ) ;
#5087 = CARTESIAN_POINT ( 'NONE',  ( 4.975801465491694664, 20.67815041659077835, 43.22084481528228395 ) ) ;
#5088 = ADVANCED_FACE ( 'NONE', ( #42945 ), #17383, .F. ) ;
#5089 = B_SPLINE_CURVE_WITH_KNOTS ( 'NONE', 3,
 ( #36926, #13411, #32516, #49285, #44318, #20484 ),
 .UNSPECIFIED., .F., .F.,
 ( 4, 2, 4 ),
 ( 1.283058336952897540E-16, 0.0002450741128632361911, 0.0004901482257263440126 ),
 .UNSPECIFIED. ) ;
#5090 = VERTEX_POINT ( 'NONE', #11578 ) ;
#5091 = CARTESIAN_POINT ( 'NONE',  ( 0.6029303876144825880, -12.57751758557302146, 46.43417959025969566 ) ) ;
#5092 = CARTESIAN_POINT ( 'NONE',  ( 4.967162193818130511, 0.000000000000000000, 0.000000000000000000 ) ) ;
#5093 = CARTESIAN_POINT ( 'NONE',  ( 0.5832655196449136881, 36.94460163995477586, -28.88479864285675447 ) ) ;
#5094 = CARTESIAN_POINT ( 'NONE',  ( -6.079354080745853928, 9.983157571106950456, 16.46601105789171271 ) ) ;
#5095 = ORIENTED_EDGE ( 'NONE', *, *, #4023, .T. ) ;
#5096 = CARTESIAN_POINT ( 'NONE',  ( -6.078457390727109555, 12.00936083188087089, 15.05223450013962250 ) ) ;
#5097 = CARTESIAN_POINT ( 'NONE',  ( 0.1129192098497455998, 37.24220309526837980, -23.66368729500826618 ) ) ;
#5098 = CARTESIAN_POINT ( 'NONE',  ( 4.956445790443988031, 5.766952734435944596E-15, 47.09074272231896430 ) ) ;
#5099 = CARTESIAN_POINT ( 'NONE',  ( 0.5997462898726536595, -35.63787911784747564, -33.78599121124021565 ) ) ;
#5100 = ORIENTED_EDGE ( 'NONE', *, *, #57322, .F. ) ;
#5101 = VERTEX_POINT ( 'NONE', #54769 ) ;
#5102 = CARTESIAN_POINT ( 'NONE',  ( 3.238018933889920792, 12.98832471626936247, -3.272753188433144445 ) ) ;
#5103 = CARTESIAN_POINT ( 'NONE',  ( 1.227938101723747621, -20.72293514920724533, -37.58536632582800507 ) ) ;
#5104 = LINE ( 'NONE', #48355, #48836 ) ;
#5105 = CARTESIAN_POINT ( 'NONE',  ( -6.016489644550737204, 9.417787539062247859, 16.32089497094064967 ) ) ;
#5106 = DIRECTION ( 'NONE',  ( 0.07439287786467664587, 0.2708295585865134192, -0.9597484305373181757 ) ) ;
#5107 = B_SPLINE_CURVE_WITH_KNOTS ( 'NONE', 3,
 ( #21751, #59639, #47335, #26441 ),
 .UNSPECIFIED., .F., .F.,
 ( 4, 4 ),
 ( 2.302551629917873038E-17, 0.004564976165746188579 ),
 .UNSPECIFIED. ) ;
#5108 = CARTESIAN_POINT ( 'NONE',  ( 0.1155031312995260795, -31.81355560820710338, 30.57514206173575033 ) ) ;
#5109 = CARTESIAN_POINT ( 'NONE',  ( 0.6029442701453591180, -42.74546001881537904, 24.17376414500094839 ) ) ;
#5110 = AXIS2_PLACEMENT_3D ( 'NONE', #43, #666, #19806 ) ;
#5111 = CARTESIAN_POINT ( 'NONE',  ( 0.8557997880470599172, 0.9121262075952832893, -47.89938907511592703 ) ) ;
#5112 = EDGE_CURVE ( 'NONE', #2075, #50613, #39993, .T. ) ;
#5113 = CARTESIAN_POINT ( 'NONE',  ( -6.077587904424778920, 19.09876248768971152, -2.456276212632990674 ) ) ;
#5114 = CARTESIAN_POINT ( 'NONE',  ( -6.001507490154111224, -13.33564355450117844, 13.31361390284155277 ) ) ;
#5115 = CARTESIAN_POINT ( 'NONE',  ( -6.016761891674564211, 17.41015286184802946, 7.207804629151374876 ) ) ;
#5116 = ORIENTED_EDGE ( 'NONE', *, *, #43146, .F. ) ;
#5117 = CARTESIAN_POINT ( 'NONE',  ( 0.7048096507298579061, 23.32077812596822852, 42.08020459959988813 ) ) ;
#5118 = DIRECTION ( 'NONE',  ( 0.000000000000000000, 0.7071067811865527908, -0.7071067811865421326 ) ) ;
#5119 = CARTESIAN_POINT ( 'NONE',  ( 4.691466044806102076, -39.84135254923121749, -20.01963481131645750 ) ) ;
#5120 = CARTESIAN_POINT ( 'NONE',  ( 4.956653778116975495, -39.67974989265057673, 27.17045123668458828 ) ) ;
#5121 = CARTESIAN_POINT ( 'NONE',  ( 0.8751705887134553219, -46.67919521768879321, -11.58504748649183647 ) ) ;
#5122 = CARTESIAN_POINT ( 'NONE',  ( 0.6027444965799114707, 33.11153390055023493, -36.26520148351796990 ) ) ;
#5123 = EDGE_CURVE ( 'NONE', #19546, #50188, #43880, .T. ) ;
#5124 = CARTESIAN_POINT ( 'NONE',  ( 4.549368137175248350, 0.000000000000000000, 0.000000000000000000 ) ) ;
#5125 = DIRECTION ( 'NONE',  ( -0.1011922191286467321, 0.9589869809184654592, 0.2647717983787297169 ) ) ;
#5126 = CARTESIAN_POINT ( 'NONE',  ( 0.5809828226811544205, 47.55412398569205834, 5.711058609465488267 ) ) ;
#5127 =( BOUNDED_SURFACE ( )  B_SPLINE_SURFACE ( 3, 1, ( 
 ( #28039, #51823 ),
 ( #23953, #4199 ),
 ( #18646, #23642 ),
 ( #14569, #38383 ) ),
 .UNSPECIFIED., .F., .F., .F. ) 
 B_SPLINE_SURFACE_WITH_KNOTS ( ( 4, 4 ),
 ( 2, 2 ),
 ( 0.000000000000000000, 1.000000000000000000 ),
 ( 0.000000000000000000, 1.000000000000000000 ),
 .UNSPECIFIED. ) 
 GEOMETRIC_REPRESENTATION_ITEM ( )  RATIONAL_B_SPLINE_SURFACE ( (
 ( 1.000000000000000000, 1.000000000000000000),
 ( 0.9953040768229013402, 0.8617119497784988535),
 ( 0.9953040768229013402, 0.8617119497784988535),
 ( 1.000000000000000000, 1.000000000000000000) ) ) 
 REPRESENTATION_ITEM ( '' )  SURFACE ( )  );
#5128 = CARTESIAN_POINT ( 'NONE',  ( 0.6027444965799114707, -30.71998326625707776, 38.31215399854628600 ) ) ;
#5129 = EDGE_CURVE ( 'NONE', #55350, #25443, #29738, .T. ) ;
#5130 = CARTESIAN_POINT ( 'NONE',  ( 6.189768672337906175, 1.091423221261470733, -2.362915713819767774E-16 ) ) ;
#5131 = CARTESIAN_POINT ( 'NONE',  ( 1.827326673878743035, 42.50320212329570779, 6.839036141888717779 ) ) ;
#5133 = ORIENTED_EDGE ( 'NONE', *, *, #18827, .T. ) ;
#5132 = FACE_OUTER_BOUND ( 'NONE', #51188, .T. ) ;
#5134 = VERTEX_POINT ( 'NONE', #35085 ) ;
#5135 = B_SPLINE_CURVE_WITH_KNOTS ( 'NONE', 3,
 ( #16235, #35358, #30621, #49739, #7420, #40373, #6795, #26234, #12468, #2729, #22168, #26550, #16540, #45677, #59749, #59433, #31254, #7738, #46000 ),
 .UNSPECIFIED., .F., .F.,
 ( 4, 3, 3, 3, 3, 3, 4 ),
 ( 1.551621725782133898E-17, 0.0002732106629380501805, 0.0004098138914053729926, 0.0005464171197651409434, 0.0006830203481512506702, 0.0008196235766963562604, 0.001011968216111135740 ),
 .UNSPECIFIED. ) ;
#5136 = CARTESIAN_POINT ( 'NONE',  ( 0.1104177457020373149, -43.12445244485484608, 0.004894317366673364873 ) ) ;
#5137 = CARTESIAN_POINT ( 'NONE',  ( 0.1073791018717483448, 40.02496097243036388, 16.05399293000829175 ) ) ;
#5138 = CARTESIAN_POINT ( 'NONE',  ( 5.860006189529234355, 31.81514841426757911, 36.25227510158474331 ) ) ;
#5139 = ORIENTED_EDGE ( 'NONE', *, *, #1037, .T. ) ;
#5140 = CARTESIAN_POINT ( 'NONE',  ( 0.5980271706414734822, -2.273683837877277902, -49.05995928093539504 ) ) ;
#5141 = CARTESIAN_POINT ( 'NONE',  ( 0.8744876279028306332, -47.25615711918273121, 13.31186180466906954 ) ) ;
#5142 = CARTESIAN_POINT ( 'NONE',  ( 0.5839880159502347512, -41.45643525694588760, -23.98728323041091670 ) ) ;
#5143 = ORIENTED_EDGE ( 'NONE', *, *, #43272, .T. ) ;
#5144 = VERTEX_POINT ( 'NONE', #11903 ) ;
#5145 = CARTESIAN_POINT ( 'NONE',  ( -6.010958268070873523, 11.45964880703848543, -14.95835081545462053 ) ) ;
#5146 = EDGE_CURVE ( 'NONE', #48858, #14994, #26953, .T. ) ;
#5147 = CARTESIAN_POINT ( 'NONE',  ( 0.7948884756798504370, -6.978576367878667419, -48.60039214325163925 ) ) ;
#5148 = CARTESIAN_POINT ( 'NONE',  ( 0.5830081025819923157, 16.59954784437812947, -43.85985688239814095 ) ) ;
#5149 = EDGE_CURVE ( 'NONE', #16494, #57030, #27648, .T. ) ;
#5150 = CARTESIAN_POINT ( 'NONE',  ( 0.7242003506639983490, -47.69730471853326037, -11.66099467084223207 ) ) ;
#5151 = VECTOR ( 'NONE', #58495, 1000.000000000000114 ) ;
#5152 = EDGE_CURVE ( 'NONE', #20064, #24696, #61930, .T. ) ;
#5153 = CIRCLE ( 'NONE', #25162, 2.698940690764985550 ) ;
#5154 = B_SPLINE_CURVE_WITH_KNOTS ( 'NONE', 3,
 ( #30183, #48992, #44323, #6045, #1353, #20488 ),
 .UNSPECIFIED., .F., .F.,
 ( 4, 2, 4 ),
 ( 1.271806119729192492E-16, 0.0002450741128632357032, 0.0004901482257263442294 ),
 .UNSPECIFIED. ) ;
#5155 = CARTESIAN_POINT ( 'NONE',  ( 0.08486401232817714080, 9.539392014169456147, 3.000000000000000000 ) ) ;
#5156 = ORIENTED_EDGE ( 'NONE', *, *, #31156, .T. ) ;
#5157 = B_SPLINE_CURVE_WITH_KNOTS ( 'NONE', 3,
 ( #51746, #3822, #60524, #3509 ),
 .UNSPECIFIED., .F., .F.,
 ( 4, 4 ),
 ( 1.734723475976807094E-18, 0.004050076154993005086 ),
 .UNSPECIFIED. ) ;
#5158 = ORIENTED_EDGE ( 'NONE', *, *, #4351, .F. ) ;
#5159 = CARTESIAN_POINT ( 'NONE',  ( 4.975801465491695552, -47.76942479135487929, 3.702618843596635401 ) ) ;
#5160 = CARTESIAN_POINT ( 'NONE',  ( 2.359973842542475886, 44.00467994243045666, 1.313026198047289705 ) ) ;
#5161 = ORIENTED_EDGE ( 'NONE', *, *, #37834, .F. ) ;
#5162 = CARTESIAN_POINT ( 'NONE',  ( 0.1154773475650540532, 41.81928631232078430, -14.07447769454556408 ) ) ;
#5163 = CARTESIAN_POINT ( 'NONE',  ( 0.7056759521544990754, 5.532722967652889068, -46.57400353931571857 ) ) ;
#5164 = CARTESIAN_POINT ( 'NONE',  ( 0.6001305935487315502, -23.60027211631799915, -41.92422178329161397 ) ) ;
#5165 = DIRECTION ( 'NONE',  ( -1.000000000000000000, -0.000000000000000000, -0.000000000000000000 ) ) ;
#5166 = EDGE_CURVE ( 'NONE', #34686, #38949, #56817, .T. ) ;
#5167 = ORIENTED_EDGE ( 'NONE', *, *, #2821, .F. ) ;
#5168 = VERTEX_POINT ( 'NONE', #59470 ) ;
#5169 = CARTESIAN_POINT ( 'NONE',  ( 0.5830082357119570347, 46.51316245118321291, -5.979778735720702620 ) ) ;
#5170 = CARTESIAN_POINT ( 'NONE',  ( 0.5782707292762442330, -2.290569157858767912, 46.84538020595716290 ) ) ;
#5171 = LINE ( 'NONE', #6084, #41199 ) ;
#5172 = CARTESIAN_POINT ( 'NONE',  ( 0.5819845079324652559, 29.51613512130382588, 37.72030202710084978 ) ) ;
#5173 = EDGE_LOOP ( 'NONE', ( #7417, #2870, #13833, #22426 ) ) ;
#5174 = CARTESIAN_POINT ( 'NONE',  ( 4.834790513006555379, -22.26269597880774143, -41.67687258755817226 ) ) ;
#5175 = ORIENTED_EDGE ( 'NONE', *, *, #43157, .F. ) ;
#5176 = CARTESIAN_POINT ( 'NONE',  ( 3.782542959838394836, 39.34345065763542237, -14.80981916657911235 ) ) ;
#5177 = CARTESIAN_POINT ( 'NONE',  ( 0.1145239942831223490, 9.499891895270792475, 43.08941325526308219 ) ) ;
#5178 = ORIENTED_EDGE ( 'NONE', *, *, #4363, .F. ) ;
#5179 = CARTESIAN_POINT ( 'NONE',  ( 5.895881250540457863, -17.30282815192082779, 10.25377099185450902 ) ) ;
#5180 = CARTESIAN_POINT ( 'NONE',  ( 0.5998501479064699549, -47.62484632993692912, 6.798102206413326520 ) ) ;
#5181 = CARTESIAN_POINT ( 'NONE',  ( 0.5804410086790514622, -35.14691939471148885, -31.05179397260405949 ) ) ;
#5182 = B_SPLINE_CURVE_WITH_KNOTS ( 'NONE', 3,
 ( #19776, #29770, #36355, #21929, #46066, #2491 ),
 .UNSPECIFIED., .F., .F.,
 ( 4, 2, 4 ),
 ( 1.764953265579307567E-18, 0.0002450742804987332546, 0.0004901485609974646660 ),
 .UNSPECIFIED. ) ;
#5183 = ORIENTED_EDGE ( 'NONE', *, *, #16154, .F. ) ;
#5184 =( BOUNDED_SURFACE ( )  B_SPLINE_SURFACE ( 3, 1, ( 
 ( #43363, #48648 ),
 ( #93, #61801 ),
 ( #5706, #23928 ),
 ( #20164, #48349 ) ),
 .UNSPECIFIED., .F., .F., .F. ) 
 B_SPLINE_SURFACE_WITH_KNOTS ( ( 4, 4 ),
 ( 2, 2 ),
 ( 0.000000000000000000, 1.000000000000000000 ),
 ( 0.000000000000000000, 1.000000000000000000 ),
 .UNSPECIFIED. ) 
 GEOMETRIC_REPRESENTATION_ITEM ( )  RATIONAL_B_SPLINE_SURFACE ( (
 ( 1.000000000000000000, 1.000000000000000000),
 ( 0.9953485035131437453, 0.8621029689291515030),
 ( 0.9953485035131437453, 0.8621029689291515030),
 ( 1.000000000000000000, 1.000000000000000000) ) ) 
 REPRESENTATION_ITEM ( '' )  SURFACE ( )  );
#5185 = CARTESIAN_POINT ( 'NONE',  ( 0.7242486021783832717, -0.7549377848418828973, -49.09624762968133638 ) ) ;
#5186 = DIRECTION ( 'NONE',  ( 0.000000000000000000, 0.000000000000000000, -1.000000000000000000 ) ) ;
#5187 = CARTESIAN_POINT ( 'NONE',  ( 0.1064266418746773885, 10.61815661559940338, 41.79703894102875239 ) ) ;
#5188 = CARTESIAN_POINT ( 'NONE',  ( 4.000000000000000000, 0.000000000000000000, 0.000000000000000000 ) ) ;
#5189 = CARTESIAN_POINT ( 'NONE',  ( 0.8751705887134553219, 11.58504748649199811, -46.67919521768876479 ) ) ;
#5190 = ORIENTED_EDGE ( 'NONE', *, *, #2905, .F. ) ;
#5191 = CARTESIAN_POINT ( 'NONE',  ( 0.9736507210033069626, 39.81239086052237042, -16.00326134587874094 ) ) ;
#5192 = CARTESIAN_POINT ( 'NONE',  ( 0.9754292589017210524, 14.51724368765255768, -39.31382838911252975 ) ) ;
#5193 = CARTESIAN_POINT ( 'NONE',  ( 0.5804410086790514622, 36.46521478791949988, -29.49250688439850876 ) ) ;
#5194 = ORIENTED_EDGE ( 'NONE', *, *, #4482, .T. ) ;
#5195 = ADVANCED_FACE ( 'NONE', ( #15972 ), #53752, .F. ) ;
#5196 = CARTESIAN_POINT ( 'NONE',  ( 0.5326698147273805084, 0.000000000000000000, 0.000000000000000000 ) ) ;
#5197 = LINE ( 'NONE', #47525, #49347 ) ;
#5198 = CARTESIAN_POINT ( 'NONE',  ( 4.958415959904820092, -45.41969080731320219, -0.5056093261671902317 ) ) ;
#5199 = FACE_OUTER_BOUND ( 'NONE', #4757, .T. ) ;
#5200 = CARTESIAN_POINT ( 'NONE',  ( 4.833616638992205949, 3.476827473557875692, -46.11947910922904725 ) ) ;
#5201 = CARTESIAN_POINT ( 'NONE',  ( 0.8554163680231708922, 33.26717477998096228, -33.08323677136227303 ) ) ;
#5202 = VECTOR ( 'NONE', #50152, 1000.000000000000000 ) ;
#5203 = CARTESIAN_POINT ( 'NONE',  ( -6.016761891674565099, 4.880293656735219088, -18.20023637398594119 ) ) ;
#5204 = EDGE_CURVE ( 'NONE', #7531, #40743, #36623, .T. ) ;
#5205 = FILL_AREA_STYLE_COLOUR ( '', #25905 ) ;
#5206 = CARTESIAN_POINT ( 'NONE',  ( 0.2285344041767107259, 39.41443120982247450, -19.82432300739741748 ) ) ;
#5207 =( BOUNDED_SURFACE ( )  B_SPLINE_SURFACE ( 3, 1, ( 
 ( #60816, #22009 ),
 ( #31715, #41445 ),
 ( #27625, #2877 ),
 ( #55496, #45833 ) ),
 .UNSPECIFIED., .F., .F., .F. ) 
 B_SPLINE_SURFACE_WITH_KNOTS ( ( 4, 4 ),
 ( 2, 2 ),
 ( 0.000000000000000000, 1.000000000000000000 ),
 ( 0.000000000000000000, 1.000000000000000000 ),
 .UNSPECIFIED. ) 
 GEOMETRIC_REPRESENTATION_ITEM ( )  RATIONAL_B_SPLINE_SURFACE ( (
 ( 1.000000000000000000, 1.000000000000000000),
 ( 0.9953040768229013402, 0.8617119497784988535),
 ( 0.9953040768229013402, 0.8617119497784988535),
 ( 1.000000000000000000, 1.000000000000000000) ) ) 
 REPRESENTATION_ITEM ( '' )  SURFACE ( )  );
#5208 = AXIS2_PLACEMENT_3D ( 'NONE', #22202, #55079, #41330 ) ;
#5209 = CARTESIAN_POINT ( 'NONE',  ( 0.5809828226811617480, -37.66417181417530458, -29.58751527316218954 ) ) ;
#5210 = EDGE_CURVE ( 'NONE', #34340, #16449, #53815, .T. ) ;
#5211 = CARTESIAN_POINT ( 'NONE',  ( 1.157644175074336923, -11.62785181577198657, -40.27152018026674796 ) ) ;
#5213 = ORIENTED_EDGE ( 'NONE', *, *, #23530, .T. ) ;
#5212 = CARTESIAN_POINT ( 'NONE',  ( 2.643462169533600914, 19.65219740572190332, -43.83256147628713961 ) ) ;
#5214 = ORIENTED_EDGE ( 'NONE', *, *, #34303, .F. ) ;
#5215 = DIRECTION ( 'NONE',  ( 0.000000000000000000, 0.000000000000000000, 1.000000000000000000 ) ) ;
#5216 = CARTESIAN_POINT ( 'NONE',  ( 1.227938101723748288, -33.52879263017845091, -26.79402671879361364 ) ) ;
#5217 = DIRECTION ( 'NONE',  ( 0.000000000000000000, 0.000000000000000000, 1.000000000000000000 ) ) ;
#5218 = CARTESIAN_POINT ( 'NONE',  ( 0.6064515330803637028, 23.15851657376443740, 40.78011091377467778 ) ) ;
#5219 = CARTESIAN_POINT ( 'NONE',  ( 0.5807400328401574052, 47.55718917606843377, 5.711437504336132953 ) ) ;
#5220 = CARTESIAN_POINT ( 'NONE',  ( 5.895596859100789899, -11.93344155749905866, 16.19015613903219730 ) ) ;
#5221 = B_SPLINE_CURVE_WITH_KNOTS ( 'NONE', 3,
 ( #49852, #2215, #40480, #21041, #26050, #35151 ),
 .UNSPECIFIED., .F., .F.,
 ( 4, 2, 4 ),
 ( 8.848046324741092137E-18, 0.0002291978881530156722, 0.0004583957763060225081 ),
 .UNSPECIFIED. ) ;
#5222 = ORIENTED_EDGE ( 'NONE', *, *, #889, .F. ) ;
#5223 = CARTESIAN_POINT ( 'NONE',  ( 4.967162193818130511, 32.10009971360111791, -28.74031574029977776 ) ) ;
#5224 = EDGE_CURVE ( 'NONE', #54810, #48392, #41035, .T. ) ;
#5225 = CARTESIAN_POINT ( 'NONE',  ( 4.975801465491694664, 46.87746200127440943, 9.906103548668390602 ) ) ;
#5226 = CARTESIAN_POINT ( 'NONE',  ( 3.783278058412226308, -7.325100730114020742, -42.41041238787302348 ) ) ;
#5227 = ADVANCED_FACE ( 'NONE', ( #32227 ), #2770, .F. ) ;
#5228 = VERTEX_POINT ( 'NONE', #55690 ) ;
#5229 = CARTESIAN_POINT ( 'NONE',  ( 4.967162193818130511, 0.000000000000000000, 0.000000000000000000 ) ) ;
#5230 = ADVANCED_FACE ( 'NONE', ( #36943 ), #21769, .F. ) ;
#5231 = CARTESIAN_POINT ( 'NONE',  ( 0.5839880159502353063, 47.49213420504723615, -6.206687493267210698 ) ) ;
#5232 = VERTEX_POINT ( 'NONE', #3378 ) ;
#5233 = CARTESIAN_POINT ( 'NONE',  ( 0.8751705887134553219, 46.21789262997757675, -13.30665218149314200 ) ) ;
#5234 = VERTEX_POINT ( 'NONE', #12508 ) ;
#5235 = CARTESIAN_POINT ( 'NONE',  ( 0.5988103564986360094, -13.03604522143325006, -46.30780741915661736 ) ) ;
#5236 = CARTESIAN_POINT ( 'NONE',  ( 0.6031357023905875581, 33.98625823839253002, 34.04794059289660879 ) ) ;
#5237 = VERTEX_POINT ( 'NONE', #26275 ) ;
#5238 = CARTESIAN_POINT ( 'NONE',  ( 2.282803330402962683, -46.93788402311890451, 1.825363221177198403 ) ) ;
#5239 = DIRECTION ( 'NONE',  ( -1.655270492344282294E-16, 1.000000000000000000, 0.000000000000000000 ) ) ;
#5240 = CARTESIAN_POINT ( 'NONE',  ( 0.9784957157296367836, 40.48045361714974177, 10.84739286382488999 ) ) ;
#5241 = CARTESIAN_POINT ( 'NONE',  ( 0.6252788684277218456, 28.65511785929881938, 39.87892365201650335 ) ) ;
#5242 = EDGE_CURVE ( 'NONE', #26755, #55625, #4923, .T. ) ;
#5243 = EDGE_LOOP ( 'NONE', ( #53000, #17728, #1539, #9040 ) ) ;
#5244 = DIRECTION ( 'NONE',  ( -1.000000000000000000, -0.000000000000000000, -0.000000000000000000 ) ) ;
#5245 = ORIENTED_EDGE ( 'NONE', *, *, #48085, .F. ) ;
#5246 = CARTESIAN_POINT ( 'NONE',  ( 0.9754292580325136797, 40.56950064046846904, -10.50919048676124667 ) ) ;
#5247 = CONICAL_SURFACE ( 'NONE', #54244, 43.08621763946400307, 1.568696531533066763 ) ;
#5248 = ADVANCED_FACE ( 'NONE', ( #13129 ), #38990, .F. ) ;
#5249 = ORIENTED_EDGE ( 'NONE', *, *, #44191, .F. ) ;
#5250 = ORIENTED_EDGE ( 'NONE', *, *, #1934, .T. ) ;
#5251 = CARTESIAN_POINT ( 'NONE',  ( 5.917102823773431552, 0.6806365918034013029, -20.10040924662083128 ) ) ;
#5252 = B_SPLINE_CURVE_WITH_KNOTS ( 'NONE', 3,
 ( #55804, #17005, #8819, #13534 ),
 .UNSPECIFIED., .F., .F.,
 ( 4, 4 ),
 ( 9.813077866773594792E-18, 0.005013413432710153717 ),
 .UNSPECIFIED. ) ;
#5253 = CARTESIAN_POINT ( 'NONE',  ( 0.9756008150404594792, 34.12792951168108857, 26.00810955565524907 ) ) ;
#5254 = VERTEX_POINT ( 'NONE', #36018 ) ;
#5255 = CARTESIAN_POINT ( 'NONE',  ( -6.015611763856276717, 11.46610900684722623, 14.95313250337433963 ) ) ;
#5256 = DIRECTION ( 'NONE',  ( 0.07439287786467665975, -0.6957517427943072930, -0.7144194931003039484 ) ) ;
#5257 = CARTESIAN_POINT ( 'NONE',  ( 5.959828726073459926, 16.28130559351247442, 12.49879082830573829 ) ) ;
#5258 = VERTEX_POINT ( 'NONE', #12207 ) ;
#5259 = EDGE_LOOP ( 'NONE', ( #10232, #39171, #52640, #43675 ) ) ;
#5260 = CARTESIAN_POINT ( 'NONE',  ( 0.1100247026804066219, -21.41511734445772674, -37.43141430507365186 ) ) ;
#5261 = CARTESIAN_POINT ( 'NONE',  ( 0.1129192098497447394, -27.88830454350447852, -34.19348267541494124 ) ) ;
#5262 = CARTESIAN_POINT ( 'NONE',  ( 4.960386119450153508, 32.13287905145099899, 29.69704612477748640 ) ) ;
#5263 = AXIS2_PLACEMENT_3D ( 'NONE', #57004, #37312, #27586 ) ;
#5264 = CARTESIAN_POINT ( 'NONE',  ( 0.5809828226811617480, 38.32755012159184815, -28.72298383114449294 ) ) ;
#5265 = FACE_OUTER_BOUND ( 'NONE', #41410, .T. ) ;
#5266 = ORIENTED_EDGE ( 'NONE', *, *, #28630, .T. ) ;
#5267 = ORIENTED_EDGE ( 'NONE', *, *, #24619, .T. ) ;
#5268 = ADVANCED_FACE ( 'NONE', ( #55084 ), #57778, .F. ) ;
#5269 = CARTESIAN_POINT ( 'NONE',  ( 0.6031356219577718170, 12.53544563195234929, 46.44562759437258848 ) ) ;
#5270 = CARTESIAN_POINT ( 'NONE',  ( 5.895596859100789899, 0.6756533542673609505, 20.10153416427101192 ) ) ;
#5271 = CARTESIAN_POINT ( 'NONE',  ( 6.999999999999995559, 58.44237546506807490, 54.69470952477956871 ) ) ;
#5272 = DIRECTION ( 'NONE',  ( 0.000000000000000000, 0.000000000000000000, -1.000000000000000000 ) ) ;
#5273 = CARTESIAN_POINT ( 'NONE',  ( 0.3622758884714730732, 33.69533458712344753, -26.89560658783350178 ) ) ;
#5274 = ADVANCED_FACE ( 'NONE', ( #22206 ), #13427, .T. ) ;
#5275 = DIRECTION ( 'NONE',  ( -1.000000000000000000, -0.000000000000000000, -0.000000000000000000 ) ) ;
#5276 = ORIENTED_EDGE ( 'NONE', *, *, #15235, .T. ) ;
#5277 = CARTESIAN_POINT ( 'NONE',  ( 0.8744876279028306332, 43.84003649649945089, -22.09980204357244560 ) ) ;
#5278 = CARTESIAN_POINT ( 'NONE',  ( 5.901764892641288895, 25.42221402738026725, 41.85334516362757995 ) ) ;
#5279 = EDGE_CURVE ( 'NONE', #23457, #7531, #13463, .T. ) ;
#5280 =( BOUNDED_SURFACE ( )  B_SPLINE_SURFACE ( 3, 1, ( 
 ( #57120, #34275 ),
 ( #6029, #53351 ),
 ( #9842, #14560 ),
 ( #48980, #33360 ) ),
 .UNSPECIFIED., .F., .F., .F. ) 
 B_SPLINE_SURFACE_WITH_KNOTS ( ( 4, 4 ),
 ( 2, 2 ),
 ( 0.000000000000000000, 1.000000000000000000 ),
 ( 0.000000000000000000, 1.000000000000000000 ),
 .UNSPECIFIED. ) 
 GEOMETRIC_REPRESENTATION_ITEM ( )  RATIONAL_B_SPLINE_SURFACE ( (
 ( 1.000000000000000000, 1.000000000000000000),
 ( 0.7269869731126821222, 0.9931720237060910339),
 ( 0.7269869731126821222, 0.9931720237060910339),
 ( 1.000000000000000000, 1.000000000000000000) ) ) 
 REPRESENTATION_ITEM ( '' )  SURFACE ( )  );
#5281 = CARTESIAN_POINT ( 'NONE',  ( 0.1135584504625008484, 29.34358894678132756, 32.95308543759726660 ) ) ;
#5282 = EDGE_CURVE ( 'NONE', #33419, #26755, #2218, .T. ) ;
#5283 = ADVANCED_FACE ( 'NONE', ( #46955 ), #41019, .F. ) ;
#5284 = CARTESIAN_POINT ( 'NONE',  ( 2.299652685299200972, -6.551234707231919252, -48.59385813730900594 ) ) ;
#5285 = CARTESIAN_POINT ( 'NONE',  ( 0.9788927965476029724, -34.47085361914916035, 23.83478263796355634 ) ) ;
#5286 = VECTOR ( 'NONE', #6749, 1000.000000000000000 ) ;
#5287 = ADVANCED_FACE ( 'NONE', ( #42872 ), #6918, .F. ) ;
#5288 = ORIENTED_EDGE ( 'NONE', *, *, #44717, .F. ) ;
#5289 = CARTESIAN_POINT ( 'NONE',  ( 0.3676999524040323597, 24.55639947020961600, 36.64606156713607277 ) ) ;
#5290 =( BOUNDED_SURFACE ( )  B_SPLINE_SURFACE ( 3, 1, ( 
 ( #39768, #58823 ),
 ( #30957, #2430 ),
 ( #3349, #17788 ),
 ( #40693, #7430 ) ),
 .UNSPECIFIED., .F., .F., .F. ) 
 B_SPLINE_SURFACE_WITH_KNOTS ( ( 4, 4 ),
 ( 2, 2 ),
 ( 0.000000000000000000, 1.000000000000000000 ),
 ( 0.000000000000000000, 1.000000000000000000 ),
 .UNSPECIFIED. ) 
 GEOMETRIC_REPRESENTATION_ITEM ( )  RATIONAL_B_SPLINE_SURFACE ( (
 ( 1.000000000000000000, 1.000000000000000000),
 ( 0.9952954269826590483, 0.8620686068821339365),
 ( 0.9952954269826590483, 0.8620686068821339365),
 ( 1.000000000000000000, 1.000000000000000000) ) ) 
 REPRESENTATION_ITEM ( '' )  SURFACE ( )  );
#5291 = DIRECTION ( 'NONE',  ( -1.000000000000000000, -5.380183451256670742E-17, 1.298891185607911324E-16 ) ) ;
#5292 = CARTESIAN_POINT ( 'NONE',  ( 0.5809828226811617480, 18.83114015454759738, -44.03860873105676177 ) ) ;
#5293 = CARTESIAN_POINT ( 'NONE',  ( 4.060580049360325461, 40.54515549719436507, 16.95753696936963451 ) ) ;
#5294 = CARTESIAN_POINT ( 'NONE',  ( 0.7245667037590730608, -23.33692989609141222, 42.06183421678288425 ) ) ;
#5295 = ORIENTED_EDGE ( 'NONE', *, *, #46659, .F. ) ;
#5296 =( BOUNDED_SURFACE ( )  B_SPLINE_SURFACE ( 3, 1, ( 
 ( #38558, #24746 ),
 ( #33543, #57925 ),
 ( #10035, #30054 ),
 ( #29133, #43886 ) ),
 .UNSPECIFIED., .F., .F., .F. ) 
 B_SPLINE_SURFACE_WITH_KNOTS ( ( 4, 4 ),
 ( 2, 2 ),
 ( 0.000000000000000000, 1.000000000000000000 ),
 ( 0.000000000000000000, 1.000000000000000000 ),
 .UNSPECIFIED. ) 
 GEOMETRIC_REPRESENTATION_ITEM ( )  RATIONAL_B_SPLINE_SURFACE ( (
 ( 1.000000000000000000, 1.000000000000000000),
 ( 0.9953390228620291325, 0.8624445117760984880),
 ( 0.9953390228620291325, 0.8624445117760984880),
 ( 1.000000000000000000, 1.000000000000000000) ) ) 
 REPRESENTATION_ITEM ( '' )  SURFACE ( )  );
#5297 = CARTESIAN_POINT ( 'NONE',  ( 0.9757402383260929124, -37.20221273948027374, 21.38067434779568998 ) ) ;
#5298 = PLANE ( 'NONE',  #21950 ) ;
#5299 = CIRCLE ( 'NONE', #50346, 47.91270532121795611 ) ;
#5300 = CARTESIAN_POINT ( 'NONE',  ( 4.975801465491694664, 32.01766832630313075, -35.64402118370923489 ) ) ;
#5301 = ORIENTED_EDGE ( 'NONE', *, *, #13686, .T. ) ;
#5302 = CARTESIAN_POINT ( 'NONE',  ( 0.7246131072078586532, -44.74808308960866299, 17.64706930304217636 ) ) ;
#5303 = ORIENTED_EDGE ( 'NONE', *, *, #2997, .F. ) ;
#5304 = CARTESIAN_POINT ( 'NONE',  ( 0.8751705887134423323, -0.8911681664091769539, 48.08707113907594533 ) ) ;
#5305 = VERTEX_POINT ( 'NONE', #28127 ) ;
#5306 = CARTESIAN_POINT ( 'NONE',  ( 0.7245667037590721726, 33.42814706018020843, -34.58857005974916632 ) ) ;
#5307 = ORIENTED_EDGE ( 'NONE', *, *, #30077, .T. ) ;
#5308 = CARTESIAN_POINT ( 'NONE',  ( 0.1149546198390367091, 29.86693622343102561, -32.47941941674333322 ) ) ;
#5309 = CARTESIAN_POINT ( 'NONE',  ( 5.958863334805807099, -17.77512673691311917, -10.26388325355081221 ) ) ;
#5310 = ORIENTED_EDGE ( 'NONE', *, *, #42602, .T. ) ;
#5311 = CARTESIAN_POINT ( 'NONE',  ( 0.7242003506639987931, 3.899036689095574992, -48.94700386155533778 ) ) ;
#5312 = EDGE_CURVE ( 'NONE', #5855, #1320, #59162, .T. ) ;
#5313 = PRODUCT_DEFINITION_SHAPE ( 'NONE', 'NONE',  #61995 ) ;
#5314 = B_SPLINE_CURVE_WITH_KNOTS ( 'NONE', 3,
 ( #35242, #34312, #49314, #25821 ),
 .UNSPECIFIED., .F., .F.,
 ( 4, 4 ),
 ( 5.421010862427522170E-19, 0.004444878191957670442 ),
 .UNSPECIFIED. ) ;
#5315 = ORIENTED_EDGE ( 'NONE', *, *, #17354, .F. ) ;
#5316 = CARTESIAN_POINT ( 'NONE',  ( 4.303969348037246512, -39.44373910178629927, 27.54579249306195976 ) ) ;
#5317 = CARTESIAN_POINT ( 'NONE',  ( -2.569797478183790229, 13.34095667500596427, 6.011723966604196612 ) ) ;
#5318 = EDGE_CURVE ( 'NONE', #46497, #23973, #10954, .T. ) ;
#5319 = CARTESIAN_POINT ( 'NONE',  ( 0.6017667736363749853, -38.37782726569709268, 29.00830848931562400 ) ) ;
#5320 = EDGE_LOOP ( 'NONE', ( #35865, #19753 ) ) ;
#5321 = CARTESIAN_POINT ( 'NONE',  ( 4.390527457369401532, -36.64446048591713634, -24.23569376611028403 ) ) ;
#5322 = B_SPLINE_CURVE_WITH_KNOTS ( 'NONE', 3,
 ( #1249, #48273, #24456, #43594 ),
 .UNSPECIFIED., .F., .F.,
 ( 4, 4 ),
 ( 0.000000000000000000, 0.004444878191957677381 ),
 .UNSPECIFIED. ) ;
#5323 = CARTESIAN_POINT ( 'NONE',  ( 5.894904586330512508, 17.95060305802262590, -9.072224750024185269 ) ) ;
#5324 = CARTESIAN_POINT ( 'NONE',  ( 0.1152339509894530906, -23.06439601559337760, -37.61617108227687822 ) ) ;
#5325 = ORIENTED_EDGE ( 'NONE', *, *, #9816, .F. ) ;
#5326 = CARTESIAN_POINT ( 'NONE',  ( 0.5838002273316424962, -33.77111476497751852, -33.96372661229970902 ) ) ;
#5327 = CARTESIAN_POINT ( 'NONE',  ( 0.6000166863083090663, 5.235566842225173545, -48.83044461756462340 ) ) ;
#5328 = VERTEX_POINT ( 'NONE', #56625 ) ;
#5329 = CIRCLE ( 'NONE', #54330, 85.00000000000001421 ) ;
#5330 = CARTESIAN_POINT ( 'NONE',  ( 4.975801465491695552, 39.51822597168496287, -27.09127437476339395 ) ) ;
#5331 = EDGE_LOOP ( 'NONE', ( #58794, #29130, #686, #46241 ) ) ;
#5332 = CARTESIAN_POINT ( 'NONE',  ( 4.553261556744875094, 0.000000000000000000, 0.000000000000000000 ) ) ;
#5333 = VERTEX_POINT ( 'NONE', #48702 ) ;
#5334 = CARTESIAN_POINT ( 'NONE',  ( 4.956653778116982600, -45.35992544608539845, 15.97476558431867844 ) ) ;
#5335 = CARTESIAN_POINT ( 'NONE',  ( 0.1135584504625007374, 25.59731996755785133, -35.94063525612362753 ) ) ;
#5336 = CARTESIAN_POINT ( 'NONE',  ( 3.238931869106853600, 14.74782013370846734, -40.38337734129189016 ) ) ;
#5337 = CARTESIAN_POINT ( 'NONE',  ( -6.057079549204054558, 15.43788712751053360, -11.51098919024698830 ) ) ;
#5338 = ORIENTED_EDGE ( 'NONE', *, *, #35086, .T. ) ;
#5339 = CARTESIAN_POINT ( 'NONE',  ( 4.291220156522059348, 0.5803847665936985312, -47.10681639453468250 ) ) ;
#5340 = CARTESIAN_POINT ( 'NONE',  ( -1.400000000000000355, 0.000000000000000000, 0.000000000000000000 ) ) ;
#5341 = CARTESIAN_POINT ( 'NONE',  ( 0.5836750258453344831, -44.18029554260620984, -18.49664649301237773 ) ) ;
#5342 = AXIS2_PLACEMENT_3D ( 'NONE', #26762, #36183, #20836 ) ;
#5343 = EDGE_CURVE ( 'NONE', #42745, #57673, #57590, .T. ) ;
#5344 = B_SPLINE_CURVE_WITH_KNOTS ( 'NONE', 3,
 ( #8548, #28281, #32691, #18284 ),
 .UNSPECIFIED., .F., .F.,
 ( 4, 4 ),
 ( 0.000000000000000000, 0.005014147105413707325 ),
 .UNSPECIFIED. ) ;
#5345 = CARTESIAN_POINT ( 'NONE',  ( -6.016489644550736315, 0.004404229197775727175, 18.84320342686341121 ) ) ;
#5346 = CARTESIAN_POINT ( 'NONE',  ( 3.680974057930773480, 20.05478739720736314, -43.58300585207901889 ) ) ;
#5347 = B_SPLINE_CURVE_WITH_KNOTS ( 'NONE', 3,
 ( #40785, #59848, #45781, #16965, #55136, #21959 ),
 .UNSPECIFIED., .F., .F.,
 ( 4, 2, 4 ),
 ( 0.000000000000000000, 0.0002450742804987332004, 0.0004901485609974664008 ),
 .UNSPECIFIED. ) ;
#5348 = CARTESIAN_POINT ( 'NONE',  ( 1.834102595619085729, -8.313124016454807474, -43.25609452949638012 ) ) ;
#5349 = EDGE_CURVE ( 'NONE', #26311, #4316, #19590, .T. ) ;
#5350 = DIRECTION ( 'NONE',  ( -1.000000000000000000, -0.000000000000000000, -0.000000000000000000 ) ) ;
#5351 = EDGE_CURVE ( 'NONE', #45517, #47841, #10590, .T. ) ;
#5352 = EDGE_CURVE ( 'NONE', #44883, #52969, #40458, .T. ) ;
#5353 = CARTESIAN_POINT ( 'NONE',  ( 0.9730545539215892381, 39.83279466599039154, 15.95224156741843835 ) ) ;
#5354 = CARTESIAN_POINT ( 'NONE',  ( 0.2230388203127562363, -36.95676097786397207, 22.21453373073326532 ) ) ;
#5355 = CARTESIAN_POINT ( 'NONE',  ( 5.910764540655177868, -4.647344284406774939, -19.56791837603976703 ) ) ;
#5356 = CARTESIAN_POINT ( 'NONE',  ( 7.839426360173757047, -8.264250432354510068, 2.910643653149724807E-16 ) ) ;
#5357 = DIRECTION ( 'NONE',  ( 0.000000000000000000, 0.000000000000000000, 1.000000000000000000 ) ) ;
#5358 = CARTESIAN_POINT ( 'NONE',  ( 4.975801465491695552, 47.84403947906839960, 2.564218696447662982 ) ) ;
#5359 = CARTESIAN_POINT ( 'NONE',  ( 0.2940135542859012574, 21.11549841703935826, 38.73469085059837624 ) ) ;
#5360 = ORIENTED_EDGE ( 'NONE', *, *, #605, .F. ) ;
#5361 = EDGE_CURVE ( 'NONE', #8488, #41223, #58379, .T. ) ;
#5362 = DIRECTION ( 'NONE',  ( 0.000000000000000000, 0.000000000000000000, 1.000000000000000000 ) ) ;
#5363 = B_SPLINE_CURVE_WITH_KNOTS ( 'NONE', 3,
 ( #20532, #30523, #55881, #36494, #61490, #32406 ),
 .UNSPECIFIED., .F., .F.,
 ( 4, 2, 4 ),
 ( 3.471140604459641645E-18, 0.0002291459268755693403, 0.0004582918537511352112 ),
 .UNSPECIFIED. ) ;
#5364 = CARTESIAN_POINT ( 'NONE',  ( 0.9787284016396597952, -1.213227321156433725, 41.89109784185695418 ) ) ;
#5365 = CARTESIAN_POINT ( 'NONE',  ( -6.017396004339687465, -9.422598049764740580, 16.31807101179367692 ) ) ;
#5366 = ORIENTED_EDGE ( 'NONE', *, *, #6044, .F. ) ;
#5367 = CARTESIAN_POINT ( 'NONE',  ( 0.8551540677456715978, 47.37911285756630519, -7.157691013573887595 ) ) ;
#5368 = CARTESIAN_POINT ( 'NONE',  ( 0.6846871229502899947, 37.47592888575288583, -29.84551600520595116 ) ) ;
#5369 = AXIS2_PLACEMENT_3D ( 'NONE', #5958, #15099, #40168 ) ;
#5370 =( BOUNDED_SURFACE ( )  B_SPLINE_SURFACE ( 3, 1, ( 
 ( #6098, #59349 ),
 ( #21157, #34343 ),
 ( #53418, #39671 ),
 ( #34644, #6710 ) ),
 .UNSPECIFIED., .F., .F., .F. ) 
 B_SPLINE_SURFACE_WITH_KNOTS ( ( 4, 4 ),
 ( 2, 2 ),
 ( 0.000000000000000000, 1.000000000000000000 ),
 ( 0.000000000000000000, 1.000000000000000000 ),
 .UNSPECIFIED. ) 
 GEOMETRIC_REPRESENTATION_ITEM ( )  RATIONAL_B_SPLINE_SURFACE ( (
 ( 1.000000000000000000, 1.000000000000000000),
 ( 0.7269869731126821222, 0.9931720237060910339),
 ( 0.7269869731126821222, 0.9931720237060910339),
 ( 1.000000000000000000, 1.000000000000000000) ) ) 
 REPRESENTATION_ITEM ( '' )  SURFACE ( )  );
#5371 = ORIENTED_EDGE ( 'NONE', *, *, #10985, .T. ) ;
#5372 = ORIENTED_EDGE ( 'NONE', *, *, #23413, .T. ) ;
#5373 = LINE ( 'NONE', #54218, #20571 ) ;
#5374 = ORIENTED_EDGE ( 'NONE', *, *, #14351, .T. ) ;
#5375 =( BOUNDED_SURFACE ( )  B_SPLINE_SURFACE ( 3, 1, ( 
 ( #26070, #54543 ),
 ( #27301, #31081 ),
 ( #2241, #11674 ),
 ( #46429, #12299 ) ),
 .UNSPECIFIED., .F., .F., .F. ) 
 B_SPLINE_SURFACE_WITH_KNOTS ( ( 4, 4 ),
 ( 2, 2 ),
 ( 0.000000000000000000, 1.000000000000000000 ),
 ( 0.000000000000000000, 1.000000000000000000 ),
 .UNSPECIFIED. ) 
 GEOMETRIC_REPRESENTATION_ITEM ( )  RATIONAL_B_SPLINE_SURFACE ( (
 ( 1.000000000000000000, 1.000000000000000000),
 ( 0.9953390228620291325, 0.8624445117761032620),
 ( 0.9953390228620291325, 0.8624445117761032620),
 ( 1.000000000000000000, 1.000000000000000000) ) ) 
 REPRESENTATION_ITEM ( '' )  SURFACE ( )  );
#5376 = CARTESIAN_POINT ( 'NONE',  ( 1.227938101723756947, 25.45152231597106507, -34.55893248994479450 ) ) ;
#5377 = B_SPLINE_CURVE_WITH_KNOTS ( 'NONE', 3,
 ( #20344, #39468, #34757, #35695, #54440, #53824 ),
 .UNSPECIFIED., .F., .F.,
 ( 4, 2, 4 ),
 ( 1.266823315017301927E-16, 0.0002450741128632351611, 0.0004901482257263435789 ),
 .UNSPECIFIED. ) ;
#5378 = VERTEX_POINT ( 'NONE', #44958 ) ;
#5379 = ORIENTED_EDGE ( 'NONE', *, *, #16062, .F. ) ;
#5380 = CARTESIAN_POINT ( 'NONE',  ( 0.1103878639767399694, 11.20830530106134759, 41.64243544356632754 ) ) ;
#5381 = ORIENTED_EDGE ( 'NONE', *, *, #44725, .T. ) ;
#5382 = CARTESIAN_POINT ( 'NONE',  ( 4.962356264823608143, 0.000000000000000000, 0.000000000000000000 ) ) ;
#5383 = CARTESIAN_POINT ( 'NONE',  ( 3.376099380956842921, 7.576724406378523291, -11.05900677736726223 ) ) ;
#5384 = AXIS2_PLACEMENT_3D ( 'NONE', #27538, #17226, #2791 ) ;
#5385 = B_SPLINE_CURVE_WITH_KNOTS ( 'NONE', 3,
 ( #25630, #35365, #52972, #35984 ),
 .UNSPECIFIED., .F., .F.,
 ( 4, 4 ),
 ( 0.000000000000000000, 0.004447772540403805916 ),
 .UNSPECIFIED. ) ;
#5386 = CARTESIAN_POINT ( 'NONE',  ( 0.3622758884714600280, 22.26738722580168073, -36.91764744403298693 ) ) ;
#5387 = VERTEX_POINT ( 'NONE', #60239 ) ;
#5388 = CYLINDRICAL_SURFACE ( 'NONE', #6662, 11.40403086437694569 ) ;
#5389 = ADVANCED_FACE ( 'NONE', ( #25501 ), #51381, .F. ) ;
#5390 = CARTESIAN_POINT ( 'NONE',  ( 0.9756008150404610335, -34.12792951168087541, -26.00810955565548355 ) ) ;
#5391 = ORIENTED_EDGE ( 'NONE', *, *, #53261, .T. ) ;
#5392 = ORIENTED_EDGE ( 'NONE', *, *, #30491, .T. ) ;
#5393 = B_SPLINE_CURVE_WITH_KNOTS ( 'NONE', 3,
 ( #51801, #8900, #28009, #42436, #23927, #92 ),
 .UNSPECIFIED., .F., .F.,
 ( 4, 2, 4 ),
 ( 0.000000000000000000, 0.0002447195606305749629, 0.0004894391212611499259 ),
 .UNSPECIFIED. ) ;
#5394 = CARTESIAN_POINT ( 'NONE',  ( -6.016489644550736315, 11.46752133529406414, -14.95199950534935951 ) ) ;
#5395 = ORIENTED_EDGE ( 'NONE', *, *, #3090, .T. ) ;
#5396 = CARTESIAN_POINT ( 'NONE',  ( 5.880360259849752858, 45.41096578730625311, 15.46489389606771780 ) ) ;
#5397 = CARTESIAN_POINT ( 'NONE',  ( 1.227938101723748288, -30.94118573761333479, 29.74462687941215222 ) ) ;
#5398 = CARTESIAN_POINT ( 'NONE',  ( 2.528100132419516921, 28.30161947981979864, -31.00438861599369034 ) ) ;
#5399 = CARTESIAN_POINT ( 'NONE',  ( 7.999999999999996447, 8.394250489469390599E-13, -80.00000000000001421 ) ) ;
#5400 = VERTEX_POINT ( 'NONE', #11421 ) ;
#5401 = CARTESIAN_POINT ( 'NONE',  ( 0.1139756605157202785, -1.811577870781945654, -44.08711155556820671 ) ) ;
#5402 = FACE_OUTER_BOUND ( 'NONE', #16126, .T. ) ;
#5403 = CARTESIAN_POINT ( 'NONE',  ( 0.5837799406558226156, 36.74750401072321893, -29.13527927717670707 ) ) ;
#5404 = DIRECTION ( 'NONE',  ( 0.000000000000000000, 0.000000000000000000, -1.000000000000000000 ) ) ;
#5405 = ORIENTED_EDGE ( 'NONE', *, *, #2360, .T. ) ;
#5406 = DIRECTION ( 'NONE',  ( -0.9990097760809876215, 0.000000000000000000, 0.04449120468828399177 ) ) ;
#5407 = CARTESIAN_POINT ( 'NONE',  ( 0.1147471544378676628, 36.80973225548471817, -24.33096380649096346 ) ) ;
#5408 = CARTESIAN_POINT ( 'NONE',  ( 0.8760168074886965917, -46.68716261866184425, 11.58706983520244194 ) ) ;
#5409 = CARTESIAN_POINT ( 'NONE',  ( 1.296416391601052265, -5.934581262136242152, 43.67022005118890604 ) ) ;
#5410 = ORIENTED_EDGE ( 'NONE', *, *, #3299, .F. ) ;
#5411 = ORIENTED_EDGE ( 'NONE', *, *, #22486, .T. ) ;
#5412 = CARTESIAN_POINT ( 'NONE',  ( 5.860006189529246790, -40.09484204000580831, -26.81109398084748818 ) ) ;
#5413 = CARTESIAN_POINT ( 'NONE',  ( 4.553261556744875094, 0.000000000000000000, 0.000000000000000000 ) ) ;
#5414 = DIRECTION ( 'NONE',  ( -0.1736481776669316357, 0.9848077530122079093, -5.551115123125819680E-17 ) ) ;
#5415 = ADVANCED_FACE ( 'NONE', ( #45265 ), #36608, .F. ) ;
#5416 = CARTESIAN_POINT ( 'NONE',  ( 0.5980894510889457338, -24.66136644716792148, -41.31170365136879497 ) ) ;
#5417 = CARTESIAN_POINT ( 'NONE',  ( 4.962356264823608143, -9.332162870646227404, -41.03835198954849517 ) ) ;
#5418 = CARTESIAN_POINT ( 'NONE',  ( 0.1156495703730067437, -31.60158840537683034, 30.79419691253894342 ) ) ;
#5419 = DIRECTION ( 'NONE',  ( -1.000000000000000000, -0.000000000000000000, -0.000000000000000000 ) ) ;
#5420 = CARTESIAN_POINT ( 'NONE',  ( 0.6254311100348625141, 19.04346769887692759, -44.17670535157489553 ) ) ;
#5421 = EDGE_CURVE ( 'NONE', #24638, #4666, #15038, .T. ) ;
#5422 = CARTESIAN_POINT ( 'NONE',  ( 0.6017666602106490625, -18.73203020817331321, -44.31084100715245455 ) ) ;
#5423 = CARTESIAN_POINT ( 'NONE',  ( 0.9754292589017218296, 3.614901353133219253, -41.75236466479944397 ) ) ;
#5424 = ORIENTED_EDGE ( 'NONE', *, *, #30259, .T. ) ;
#5425 = EDGE_CURVE ( 'NONE', #2500, #8307, #29213, .T. ) ;
#5426 = CARTESIAN_POINT ( 'NONE',  ( -15.25000000000000711, -2.688986455804108555, -9.952330921218299798E-16 ) ) ;
#5427 = CARTESIAN_POINT ( 'NONE',  ( 0.1101816497532062955, -34.29544870207495677, -26.14462713083283063 ) ) ;
#5428 = CARTESIAN_POINT ( 'NONE',  ( 0.1149546198390366952, -35.52488601809844226, 26.17114897027513010 ) ) ;
#5429 = CARTESIAN_POINT ( 'NONE',  ( 0.2940133293163023631, -26.87228827769844131, -34.98743592060318974 ) ) ;
#5430 = AXIS2_PLACEMENT_3D ( 'NONE', #23512, #52940, #52316 ) ;
#5431 = CARTESIAN_POINT ( 'NONE',  ( 0.6254311100348654007, -34.49956326955439323, 33.52633430496167932 ) ) ;
#5432 = CARTESIAN_POINT ( 'NONE',  ( 0.6023142530420679819, -46.39979989577489761, 12.70386526143691697 ) ) ;
#5433 = CARTESIAN_POINT ( 'NONE',  ( 4.962356264823608143, 12.05238263218917716, 40.32338863178108568 ) ) ;
#5434 = CARTESIAN_POINT ( 'NONE',  ( 3.407937589446174087, 13.34359005742693682, -3.099921468254863921 ) ) ;
#5435 = CARTESIAN_POINT ( 'NONE',  ( 0.5807400328401574052, -29.58941477092990979, -37.66660715020896077 ) ) ;
#5436 = CARTESIAN_POINT ( 'NONE',  ( 0.9736507210033062965, -11.54000710819843256, 41.32746151989296379 ) ) ;
#5437 = CARTESIAN_POINT ( 'NONE',  ( 0.7242003506639974608, 23.43456264649780962, 43.14896230146672451 ) ) ;
#5438 = CARTESIAN_POINT ( 'NONE',  ( 1.000433927950261870, -37.10347441663083856, 19.48719743491265888 ) ) ;
#5440 = ORIENTED_EDGE ( 'NONE', *, *, #42526, .F. ) ;
#5439 = DIRECTION ( 'NONE',  ( -1.000000000000000000, -0.000000000000000000, -0.000000000000000000 ) ) ;
#5441 = ORIENTED_EDGE ( 'NONE', *, *, #40913, .T. ) ;
#5442 = ADVANCED_FACE ( 'NONE', ( #6678 ), #21122, .F. ) ;
#5443 = CARTESIAN_POINT ( 'NONE',  ( 0.5809828226811617480, -0.5448590168535863976, 47.89273459658653564 ) ) ;
#5444 = LINE ( 'NONE', #1666, #44521 ) ;
#5445 = DIRECTION ( 'NONE',  ( 0.1736481776669314414, -0.9848077530122079093, 5.551115123125779621E-17 ) ) ;
#5446 = EDGE_CURVE ( 'NONE', #60852, #6434, #56173, .T. ) ;
#5447 = ORIENTED_EDGE ( 'NONE', *, *, #31514, .T. ) ;
#5448 = CARTESIAN_POINT ( 'NONE',  ( 0.1102144999581333162, -11.28312052188176473, 41.62223437741650400 ) ) ;
#5449 = CARTESIAN_POINT ( 'NONE',  ( 0.7242003506639991262, -47.28180849633769611, 13.24546184327587994 ) ) ;
#5450 = FACE_OUTER_BOUND ( 'NONE', #585, .T. ) ;
#5451 = ORIENTED_EDGE ( 'NONE', *, *, #61228, .F. ) ;
#5452 = ORIENTED_EDGE ( 'NONE', *, *, #1325, .T. ) ;
#5453 = FACE_OUTER_BOUND ( 'NONE', #50463, .T. ) ;
#5454 = CARTESIAN_POINT ( 'NONE',  ( 4.967162193818129623, 40.65506779172164897, 14.26841313271295952 ) ) ;
#5455 = DIRECTION ( 'NONE',  ( -1.000000000000000000, -0.000000000000000000, -0.000000000000000000 ) ) ;
#5456 = CARTESIAN_POINT ( 'NONE',  ( 0.9730545539215883499, -34.34678117142538412, -25.71816799638815354 ) ) ;
#5457 = CARTESIAN_POINT ( 'NONE',  ( 1.154321713695927398, -10.30834583266701898, -41.66001467525153856 ) ) ;
#5458 = B_SPLINE_CURVE_WITH_KNOTS ( 'NONE', 3,
 ( #49038, #24621, #15536, #39353 ),
 .UNSPECIFIED., .F., .F.,
 ( 4, 4 ),
 ( 0.000000000000000000, 0.004447772540403795508 ),
 .UNSPECIFIED. ) ;
#5459 = CARTESIAN_POINT ( 'NONE',  ( 0.000000000000000000, 0.000000000000000000, 0.000000000000000000 ) ) ;
#5460 = B_SPLINE_CURVE_WITH_KNOTS ( 'NONE', 3,
 ( #43140, #19321, #57489, #56889 ),
 .UNSPECIFIED., .F., .F.,
 ( 4, 4 ),
 ( 0.000000000000000000, 0.005014147105413699519 ),
 .UNSPECIFIED. ) ;
#5461 = ADVANCED_FACE ( 'NONE', ( #31134 ), #2164, .F. ) ;
#5462 = AXIS2_PLACEMENT_3D ( 'NONE', #2727, #12165, #51268 ) ;
#5463 = CARTESIAN_POINT ( 'NONE',  ( 0.9730545539215883499, 42.60426903087353878, 5.099196237955034405 ) ) ;
#5464 = VERTEX_POINT ( 'NONE', #27672 ) ;
#5465 = ORIENTED_EDGE ( 'NONE', *, *, #8672, .F. ) ;
#5466 = CARTESIAN_POINT ( 'NONE',  ( 0.8751705887134423323, 44.76769609654235893, -17.57879340691497561 ) ) ;
#5467 = CARTESIAN_POINT ( 'NONE',  ( 3.050102900204245682, 43.98187602336167856, 1.009866646495158671 ) ) ;
#5468 = AXIS2_PLACEMENT_3D ( 'NONE', #18420, #23729, #23419 ) ;
#5469 = ORIENTED_EDGE ( 'NONE', *, *, #61650, .F. ) ;
#5470 = CARTESIAN_POINT ( 'NONE',  ( 0.9787284016396613495, -37.48834466450204417, -18.73392679723960086 ) ) ;
#5471 = CARTESIAN_POINT ( 'NONE',  ( 0.5806925824938499181, 5.237374507879953178, -46.60249210726582447 ) ) ;
#5472 = CARTESIAN_POINT ( 'NONE',  ( 4.549368137175248350, 18.79584381673534565, -38.59302160394733505 ) ) ;
#5473 = CARTESIAN_POINT ( 'NONE',  ( 4.833616638992208614, 35.06988470649527301, 30.15290813935915537 ) ) ;
#5474 = VECTOR ( 'NONE', #55797, 1000.000000000000000 ) ;
#5475 = VERTEX_POINT ( 'NONE', #23584 ) ;
#5476 = CARTESIAN_POINT ( 'NONE',  ( 0.5830082357119559244, -14.15480402886485400, 44.70876377001235369 ) ) ;
#5477 = CARTESIAN_POINT ( 'NONE',  ( -6.016761891674565099, 17.40752468084782834, 7.214149619366422961 ) ) ;
#5478 = CARTESIAN_POINT ( 'NONE',  ( 4.962356264823609031, 37.75702904547822669, -18.59145920903629090 ) ) ;
#5479 = LINE ( 'NONE', #39348, #8431 ) ;
#5480 = VERTEX_POINT ( 'NONE', #46182 ) ;
#5481 = CARTESIAN_POINT ( 'NONE',  ( 0.6029443199889047422, 4.715417708898021587, -48.88049179053964366 ) ) ;
#5482 = ORIENTED_EDGE ( 'NONE', *, *, #21945, .T. ) ;
#5483 = DIRECTION ( 'NONE',  ( -0.000000000000000000, 0.000000000000000000, 1.000000000000000000 ) ) ;
#5484 = CARTESIAN_POINT ( 'NONE',  ( 0.5839254288179547281, 24.02657516616565303, -41.43367229384560346 ) ) ;
#5485 = VERTEX_POINT ( 'NONE', #4444 ) ;
#5486 = CARTESIAN_POINT ( 'NONE',  ( 3.238931869106852712, -24.69728751010312706, 35.19033040238025478 ) ) ;
#5487 = CARTESIAN_POINT ( 'NONE',  ( 0.6009452777970413218, -47.63713033690757470, 6.711700115492742036 ) ) ;
#5488 = CARTESIAN_POINT ( 'NONE',  ( 0.9752132459055854463, 25.93579301218408162, -34.18286753639614517 ) ) ;
#5489 = LINE ( 'NONE', #54030, #6444 ) ;
#5490 = CARTESIAN_POINT ( 'NONE',  ( 0.6554360035617802227, -4.240386000424091861, -5.441324518471480687 ) ) ;
#5491 = CARTESIAN_POINT ( 'NONE',  ( 0.3622758884714600280, 10.35929834645864389, 41.85013935980105515 ) ) ;
#5492 = CARTESIAN_POINT ( 'NONE',  ( 0.5998501479064699549, 28.86886762351124958, -38.48283596222000114 ) ) ;
#5493 =( BOUNDED_SURFACE ( )  B_SPLINE_SURFACE ( 3, 1, ( 
 ( #6246, #58573 ),
 ( #29467, #25082 ),
 ( #38907, #44535 ),
 ( #44842, #57959 ) ),
 .UNSPECIFIED., .F., .F., .F. ) 
 B_SPLINE_SURFACE_WITH_KNOTS ( ( 4, 4 ),
 ( 2, 2 ),
 ( 0.000000000000000000, 1.000000000000000000 ),
 ( 0.000000000000000000, 1.000000000000000000 ),
 .UNSPECIFIED. ) 
 GEOMETRIC_REPRESENTATION_ITEM ( )  RATIONAL_B_SPLINE_SURFACE ( (
 ( 1.000000000000000000, 1.000000000000000000),
 ( 0.9953040768229013402, 0.8617119497784988535),
 ( 0.9953040768229013402, 0.8617119497784988535),
 ( 1.000000000000000000, 1.000000000000000000) ) ) 
 REPRESENTATION_ITEM ( '' )  SURFACE ( )  );
#5494 = PLANE ( 'NONE',  #4760 ) ;
#5495 = ORIENTED_EDGE ( 'NONE', *, *, #39561, .T. ) ;
#5497 = EDGE_CURVE ( 'NONE', #2691, #3325, #18968, .T. ) ;
#5496 = CARTESIAN_POINT ( 'NONE',  ( 0.9757787079277434605, 39.65734351318527473, -16.38386580718250229 ) ) ;
#5498 = CARTESIAN_POINT ( 'NONE',  ( -6.016761891674565099, 2.456125503350710115, 18.68243340030203470 ) ) ;
#5499 = CARTESIAN_POINT ( 'NONE',  ( 0.8557997880470606944, -24.73961900479280374, 41.02602466100771039 ) ) ;
#5500 = VERTEX_POINT ( 'NONE', #8870 ) ;
#5501 = EDGE_CURVE ( 'NONE', #13767, #6071, #36020, .T. ) ;
#5502 = CARTESIAN_POINT ( 'NONE',  ( -16.13875996306990146, -12.45778025494542618, 1.057258788294430429 ) ) ;
#5503 = FACE_OUTER_BOUND ( 'NONE', #35532, .T. ) ;
#5504 = CARTESIAN_POINT ( 'NONE',  ( 5.999999999999998224, 6.934333478519240412E-15, 0.000000000000000000 ) ) ;
#5505 = CARTESIAN_POINT ( 'NONE',  ( 1.227938101723756947, -22.18841447410693846, -36.73927144310534487 ) ) ;
#5506 = CARTESIAN_POINT ( 'NONE',  ( 0.6008123274975392114, -20.27530734412516367, 44.72657446373153078 ) ) ;
#5507 = CARTESIAN_POINT ( 'NONE',  ( 0.6025881611877910160, 38.29866377863839944, -29.11258673756373483 ) ) ;
#5508 = EDGE_CURVE ( 'NONE', #25496, #26613, #5344, .T. ) ;
#5509 = FACE_OUTER_BOUND ( 'NONE', #6763, .T. ) ;
#5510 = CARTESIAN_POINT ( 'NONE',  ( 0.9788927965476035276, -6.830870151262773859, 41.34822639011696310 ) ) ;
#5511 = B_SPLINE_CURVE_WITH_KNOTS ( 'NONE', 3,
 ( #13294, #17676, #22371, #8257, #3862, #46198 ),
 .UNSPECIFIED., .F., .F.,
 ( 4, 2, 4 ),
 ( 0.000000000000000000, 0.0002447195606305732282, 0.0004894391212611464564 ),
 .UNSPECIFIED. ) ;
#5512 = CARTESIAN_POINT ( 'NONE',  ( 5.958863334805807099, 19.82657410201442971, -5.311251202228647550 ) ) ;
#5513 = B_SPLINE_CURVE_WITH_KNOTS ( 'NONE', 3,
 ( #52802, #43439, #52490, #802, #9273, #29007, #479, #48418, #15228, #5481, #4550, #19939, #47200, #39050, #23688, #58106 ),
 .UNSPECIFIED., .F., .F.,
 ( 4, 3, 3, 3, 3, 4 ),
 ( 2.081781105835003463E-17, 0.0002612764279487753854, 0.0003919131003184801124, 0.0005225497727000663400, 0.0007837925190632469806, 0.001045051706266716084 ),
 .UNSPECIFIED. ) ;
#5515 = ORIENTED_EDGE ( 'NONE', *, *, #54374, .T. ) ;
#5514 = CARTESIAN_POINT ( 'NONE',  ( 0.5987334308729319599, 48.31411601509184806, 8.792559368578421797 ) ) ;
#5516 = EDGE_LOOP ( 'NONE', ( #27992, #47811, #4473, #16430 ) ) ;
#5517 = CARTESIAN_POINT ( 'NONE',  ( 0.5819845079324658110, -11.95724301473539519, 46.37938935563227005 ) ) ;
#5518 = VECTOR ( 'NONE', #57222, 1000.000000000000114 ) ;
#5519 = FACE_BOUND ( 'NONE', #54215, .T. ) ;
#5520 = CARTESIAN_POINT ( 'NONE',  ( -2.739355103387248747, 1.171460933655357417, -14.88204442379931614 ) ) ;
#5521 = EDGE_CURVE ( 'NONE', #51544, #14950, #46804, .T. ) ;
#5522 = AXIS2_PLACEMENT_3D ( 'NONE', #4487, #19250, #52119 ) ;
#5523 = DIRECTION ( 'NONE',  ( -1.000000000000000000, -1.836909530733580185E-16, 1.836909530733574022E-16 ) ) ;
#5524 = DIRECTION ( 'NONE',  ( 0.1024043820194936449, -0.4859385467930519842, 0.8679729669084529364 ) ) ;
#5525 = CARTESIAN_POINT ( 'NONE',  ( -5.995132425357893702, 18.68182899165014987, -2.468096378287932158 ) ) ;
#5526 = ORIENTED_EDGE ( 'NONE', *, *, #25097, .F. ) ;
#5527 = DIRECTION ( 'NONE',  ( 0.000000000000000000, -1.000000000000000000, 0.000000000000000000 ) ) ;
#5528 = CARTESIAN_POINT ( 'NONE',  ( -6.078726893082806448, -11.01388439747515235, 15.79520154185357050 ) ) ;
#5529 = CARTESIAN_POINT ( 'NONE',  ( 1.227938101723756947, -6.439911493064287562, -42.43379953535192328 ) ) ;
#5530 = VERTEX_POINT ( 'NONE', #52080 ) ;
#5531 = FACE_OUTER_BOUND ( 'NONE', #36176, .T. ) ;
#5532 = CARTESIAN_POINT ( 'NONE',  ( 5.999999999999995559, 15.72000000000000064, 0.000000000000000000 ) ) ;
#5533 = ORIENTED_EDGE ( 'NONE', *, *, #30909, .T. ) ;
#5534 = CARTESIAN_POINT ( 'NONE',  ( 4.975801465491694664, 45.55012473237754023, -14.85979367497125381 ) ) ;
#5535 = ORIENTED_EDGE ( 'NONE', *, *, #2746, .T. ) ;
#5536 = CARTESIAN_POINT ( 'NONE',  ( 52.88193763142881210, 15.45628894957374655, -1.174165929033795353 ) ) ;
#5537 = CARTESIAN_POINT ( 'NONE',  ( 3.678834586032787790, -15.69774311151756940, 46.39173666541442032 ) ) ;
#5538 = VERTEX_POINT ( 'NONE', #22356 ) ;
#5539 = CARTESIAN_POINT ( 'NONE',  ( -6.010958268070873523, -16.32616437357118500, 9.409153349053527293 ) ) ;
#5540 = CARTESIAN_POINT ( 'NONE',  ( -4.467300000000000715, 0.000000000000000000, 0.000000000000000000 ) ) ;
#5541 = CARTESIAN_POINT ( 'NONE',  ( 4.549368137175248350, 28.14399996863453168, 32.41327393324149853 ) ) ;
#5542 = DIRECTION ( 'NONE',  ( -1.000000000000000000, -0.000000000000000000, -0.000000000000000000 ) ) ;
#5543 = EDGE_CURVE ( 'NONE', #40624, #9646, #47989, .T. ) ;
#5544 = VERTEX_POINT ( 'NONE', #36789 ) ;
#5545 = EDGE_CURVE ( 'NONE', #39018, #48274, #4561, .T. ) ;
#5546 = CARTESIAN_POINT ( 'NONE',  ( 4.291220156522060236, -36.34793638197106702, -29.97026056072721545 ) ) ;
#5547 = CARTESIAN_POINT ( 'NONE',  ( 0.3676999524040366896, -0.5887207181726206162, 44.10900124961835900 ) ) ;
#5549 = ORIENTED_EDGE ( 'NONE', *, *, #43175, .T. ) ;
#5548 =( BOUNDED_SURFACE ( )  B_SPLINE_SURFACE ( 3, 1, ( 
 ( #54379, #11501 ),
 ( #1766, #1453 ),
 ( #20588, #44427 ),
 ( #39720, #30586 ) ),
 .UNSPECIFIED., .F., .F., .F. ) 
 B_SPLINE_SURFACE_WITH_KNOTS ( ( 4, 4 ),
 ( 2, 2 ),
 ( 0.000000000000000000, 1.000000000000000000 ),
 ( 0.000000000000000000, 1.000000000000000000 ),
 .UNSPECIFIED. ) 
 GEOMETRIC_REPRESENTATION_ITEM ( )  RATIONAL_B_SPLINE_SURFACE ( (
 ( 1.000000000000000000, 1.000000000000000000),
 ( 0.7269869731126817891, 0.9931720237060910339),
 ( 0.7269869731126817891, 0.9931720237060910339),
 ( 1.000000000000000000, 1.000000000000000000) ) ) 
 REPRESENTATION_ITEM ( '' )  SURFACE ( )  );
#5550 = CARTESIAN_POINT ( 'NONE',  ( 4.962356264823608143, 0.000000000000000000, 0.000000000000000000 ) ) ;
#5551 = ORIENTED_EDGE ( 'NONE', *, *, #55572, .T. ) ;
#5552 = CARTESIAN_POINT ( 'NONE',  ( 0.3676999524040323597, 39.37931578712994707, 19.88014264185084912 ) ) ;
#5553 = EDGE_CURVE ( 'NONE', #2462, #53003, #51616, .T. ) ;
#5554 = ORIENTED_EDGE ( 'NONE', *, *, #37422, .F. ) ;
#5555 = DIRECTION ( 'NONE',  ( -0.07439287786467650709, -0.7991213610169786152, -0.5965490341031348676 ) ) ;
#5556 = CARTESIAN_POINT ( 'NONE',  ( 5.974727161628367256, 17.78288073588488416, 10.24903993265015423 ) ) ;
#5557 = CARTESIAN_POINT ( 'NONE',  ( 3.238018933889920792, 9.507325605900359022, -9.434948446655354815 ) ) ;
#5558 = ORIENTED_EDGE ( 'NONE', *, *, #51071, .T. ) ;
#5559 = CARTESIAN_POINT ( 'NONE',  ( 4.975610109902397937, 0.000000000000000000, 0.000000000000000000 ) ) ;
#5560 = LINE ( 'NONE', #10606, #1014 ) ;
#5561 = CONICAL_SURFACE ( 'NONE', #51582, 43.92652462719577500, 1.486293639869522343 ) ;
#5562 = ORIENTED_EDGE ( 'NONE', *, *, #32687, .F. ) ;
#5563 = VERTEX_POINT ( 'NONE', #7946 ) ;
#5564 =( BOUNDED_SURFACE ( )  B_SPLINE_SURFACE ( 3, 1, ( 
 ( #8589, #61816 ),
 ( #42156, #52738 ),
 ( #4187, #33050 ),
 ( #52123, #32424 ) ),
 .UNSPECIFIED., .F., .F., .F. ) 
 B_SPLINE_SURFACE_WITH_KNOTS ( ( 4, 4 ),
 ( 2, 2 ),
 ( 0.000000000000000000, 1.000000000000000000 ),
 ( 0.000000000000000000, 1.000000000000000000 ),
 .UNSPECIFIED. ) 
 GEOMETRIC_REPRESENTATION_ITEM ( )  RATIONAL_B_SPLINE_SURFACE ( (
 ( 1.000000000000000000, 1.000000000000000000),
 ( 0.9754377213608244057, 0.9999580625633939235),
 ( 0.9754377213608244057, 0.9999580625633939235),
 ( 1.000000000000000000, 1.000000000000000000) ) ) 
 REPRESENTATION_ITEM ( '' )  SURFACE ( )  );
#5565 = CARTESIAN_POINT ( 'NONE',  ( 0.3676999524040323597, 37.41430475689418245, -23.36921870497780418 ) ) ;
#5566 = CARTESIAN_POINT ( 'NONE',  ( -6.077587904424778920, -18.90214787454608469, 3.674891443665150970 ) ) ;
#5567 = CARTESIAN_POINT ( 'NONE',  ( -6.078457390727109555, -12.94908628767718994, 14.25186567968553675 ) ) ;
#5568 = CARTESIAN_POINT ( 'NONE',  ( 0.5987334308729317378, -13.39119755867282180, 47.24657378598286073 ) ) ;
#5569 = CARTESIAN_POINT ( 'NONE',  ( 4.553261556744873317, 35.33793455049254106, 26.09156851415302825 ) ) ;
#5570 = ORIENTED_EDGE ( 'NONE', *, *, #52536, .T. ) ;
#5571 = EDGE_CURVE ( 'NONE', #37795, #1120, #28959, .T. ) ;
#5572 = AXIS2_PLACEMENT_3D ( 'NONE', #57813, #53719, #58124 ) ;
#5573 = CARTESIAN_POINT ( 'NONE',  ( 1.214306433183764966E-14, 4.618802153517020059, -5.599999999999999645 ) ) ;
#5574 = ORIENTED_EDGE ( 'NONE', *, *, #17839, .T. ) ;
#5575 = CARTESIAN_POINT ( 'NONE',  ( 0.1129192098497455998, -42.80154921430131054, 10.72283417016679508 ) ) ;
#5576 = CARTESIAN_POINT ( 'NONE',  ( 0.7762777257811882548, -38.54028505510738967, 28.45155622761415160 ) ) ;
#5577 = FACE_OUTER_BOUND ( 'NONE', #18295, .T. ) ;
#5578 = FACE_OUTER_BOUND ( 'NONE', #26849, .T. ) ;
#5579 = CARTESIAN_POINT ( 'NONE',  ( 0.8744876279028306332, -29.90976330662902427, 38.93271258621624042 ) ) ;
#5580 = EDGE_CURVE ( 'NONE', #7415, #12199, #21799, .T. ) ;
#5581 = DIRECTION ( 'NONE',  ( 0.09722883295013597105, -0.6146093961964005370, -0.7828166095262992785 ) ) ;
#5582 = CARTESIAN_POINT ( 'NONE',  ( 3.376099380956838925, -13.33697911751163012, -1.354020550481378704 ) ) ;
#5583 = CARTESIAN_POINT ( 'NONE',  ( 0.1156495703730067853, 29.76549459089011407, 32.57235461232057361 ) ) ;
#5584 = CARTESIAN_POINT ( 'NONE',  ( 1.231276596079887931, 5.037240371905710390, 41.61613846158375196 ) ) ;
#5585 = ADVANCED_FACE ( 'NONE', ( #13585 ), #32209, .F. ) ;
#5586 = CARTESIAN_POINT ( 'NONE',  ( 5.959547316686252039, 20.35048796920733238, 2.675599016784604434 ) ) ;
#5587 = ORIENTED_EDGE ( 'NONE', *, *, #35112, .F. ) ;
#5588 = CARTESIAN_POINT ( 'NONE',  ( 5.895596859100789899, 16.57987064389777743, -11.38578379577375088 ) ) ;
#5589 = CARTESIAN_POINT ( 'NONE',  ( 0.6028777368367060907, -47.47920655903965326, -12.54052526153192204 ) ) ;
#5590 = CARTESIAN_POINT ( 'NONE',  ( 1.479689385636123067, 40.19566492452400297, 18.05248920628627118 ) ) ;
#5591 = CARTESIAN_POINT ( 'NONE',  ( 0.1129192098497455998, 3.754263797494300725, 43.96427289429426821 ) ) ;
#5592 = AXIS2_PLACEMENT_3D ( 'NONE', #386, #19233, #28302 ) ;
#5593 = ORIENTED_EDGE ( 'NONE', *, *, #17929, .F. ) ;
#5594 = DIRECTION ( 'NONE',  ( -1.000000000000000000, -0.000000000000000000, -0.000000000000000000 ) ) ;
#5595 = CARTESIAN_POINT ( 'NONE',  ( 5.917102823773431552, -15.78915961314057270, -12.45761440896741767 ) ) ;
#5596 = DIRECTION ( 'NONE',  ( -2.341930812374879235E-31, 1.110223024625156540E-16, 1.000000000000000000 ) ) ;
#5597 = VERTEX_POINT ( 'NONE', #57683 ) ;
#5598 = CARTESIAN_POINT ( 'NONE',  ( 2.500000000000000000, 2.357898499370431722, -2.818925648462311528E-15 ) ) ;
#5599 = CARTESIAN_POINT ( 'NONE',  ( 0.8751705887134423323, 5.393078191592057813, 47.79200036674281904 ) ) ;
#5600 = ORIENTED_EDGE ( 'NONE', *, *, #21251, .F. ) ;
#5601 = CIRCLE ( 'NONE', #60664, 43.92652462719577500 ) ;
#5602 = CARTESIAN_POINT ( 'NONE',  ( 1.227938101723756947, -26.79402671879305231, -33.52879263017890565 ) ) ;
#5603 = ORIENTED_EDGE ( 'NONE', *, *, #43200, .F. ) ;
#5604 = FACE_OUTER_BOUND ( 'NONE', #18495, .T. ) ;
#5605 = VERTEX_POINT ( 'NONE', #19214 ) ;
#5606 = DIRECTION ( 'NONE',  ( 0.09722883295013597105, -0.5094590954038135111, -0.8549842011133788056 ) ) ;
#5607 = DIRECTION ( 'NONE',  ( -1.000000000000000000, -3.135800716341489291E-16, 1.298891185607901956E-16 ) ) ;
#5608 = EDGE_CURVE ( 'NONE', #6174, #52714, #38324, .T. ) ;
#5609 = ORIENTED_EDGE ( 'NONE', *, *, #29444, .F. ) ;
#5610 = CARTESIAN_POINT ( 'NONE',  ( 4.956653778116975495, -20.77844580450591394, 43.37017594958047084 ) ) ;
#5611 = ORIENTED_EDGE ( 'NONE', *, *, #14358, .F. ) ;
#5612 = EDGE_CURVE ( 'NONE', #10214, #23349, #33312, .T. ) ;
#5613 = DIRECTION ( 'NONE',  ( 1.000000000000000000, 1.836970198721029194E-16, -6.779273404243071298E-32 ) ) ;
#5614 = CARTESIAN_POINT ( 'NONE',  ( -6.079354080745853928, 17.84825706230203224, -7.227217658694646829 ) ) ;
#5615 = CARTESIAN_POINT ( 'NONE',  ( 0.5806925824938511393, 40.62497527030930655, 23.42720099863236882 ) ) ;
#5616 = EDGE_CURVE ( 'NONE', #60728, #13851, #13594, .T. ) ;
#5617 = ORIENTED_EDGE ( 'NONE', *, *, #60792, .T. ) ;
#5619 = ADVANCED_FACE ( 'NONE', ( #29818 ), #148, .F. ) ;
#5618 = CARTESIAN_POINT ( 'NONE',  ( 0.5804410086790514622, -7.261380058784011382, -46.33348909263462190 ) ) ;
#5620 = CARTESIAN_POINT ( 'NONE',  ( 0.5839879882012684043, 33.86754218494344570, -33.86758487442367027 ) ) ;
#5621 = CARTESIAN_POINT ( 'NONE',  ( 0.1103936448916694457, -6.269440624735986453E-17, 43.12443171339902648 ) ) ;
#5622 = CARTESIAN_POINT ( 'NONE',  ( 0.5997462898726536595, -34.91088276334701135, -34.53667463477266608 ) ) ;
#5624 = EDGE_CURVE ( 'NONE', #43366, #24074, #16582, .T. ) ;
#5623 = VERTEX_POINT ( 'NONE', #34233 ) ;
#5625 = CARTESIAN_POINT ( 'NONE',  ( 0.000000000000000000, 0.6959691356230525150, -1.199999999999999956 ) ) ;
#5626 = CARTESIAN_POINT ( 'NONE',  ( 0.1152809850208375564, -18.06278409025916432, 40.25768390504395455 ) ) ;
#5627 = ORIENTED_EDGE ( 'NONE', *, *, #10195, .F. ) ;
#5628 = CARTESIAN_POINT ( 'NONE',  ( 0.5834584762367741595, 43.24557549772239895, -18.13990597781544878 ) ) ;
#5629 = VERTEX_POINT ( 'NONE', #47707 ) ;
#5630 = DIRECTION ( 'NONE',  ( 1.000000000000000000, 0.000000000000000000, 0.000000000000000000 ) ) ;
#5631 = EDGE_CURVE ( 'NONE', #36040, #33551, #50961, .T. ) ;
#5632 = CARTESIAN_POINT ( 'NONE',  ( 0.1152339509894530906, 25.42708409640398415, 36.06114369802547515 ) ) ;
#5633 = ORIENTED_EDGE ( 'NONE', *, *, #13123, .T. ) ;
#5634 = DIRECTION ( 'NONE',  ( -0.07836865515943411409, -0.5052769534812628915, -0.8593913859058602833 ) ) ;
#5635 = CARTESIAN_POINT ( 'NONE',  ( 0.5806925824938494740, -38.35106547415225009, 26.98922265165951018 ) ) ;
#5636 = CARTESIAN_POINT ( 'NONE',  ( 0.5806925824938506953, -46.06186276235258958, -8.804950948515241294 ) ) ;
#5637 = DIRECTION ( 'NONE',  ( 1.000000000000000000, 0.000000000000000000, 0.000000000000000000 ) ) ;
#5638 = CIRCLE ( 'NONE', #29669, 2.698940690764988215 ) ;
#5639 = EDGE_CURVE ( 'NONE', #6245, #26600, #18811, .T. ) ;
#5640 =( BOUNDED_SURFACE ( )  B_SPLINE_SURFACE ( 3, 1, ( 
 ( #8997, #41925 ),
 ( #18100, #56292 ),
 ( #36919, #55985 ),
 ( #42536, #51907 ) ),
 .UNSPECIFIED., .F., .F., .F. ) 
 B_SPLINE_SURFACE_WITH_KNOTS ( ( 4, 4 ),
 ( 2, 2 ),
 ( 0.000000000000000000, 1.000000000000000000 ),
 ( 0.000000000000000000, 1.000000000000000000 ),
 .UNSPECIFIED. ) 
 GEOMETRIC_REPRESENTATION_ITEM ( )  RATIONAL_B_SPLINE_SURFACE ( (
 ( 1.000000000000000000, 1.000000000000000000),
 ( 0.7223157951917480446, 0.9931996967497186413),
 ( 0.7223157951917480446, 0.9931996967497186413),
 ( 1.000000000000000000, 1.000000000000000000) ) ) 
 REPRESENTATION_ITEM ( '' )  SURFACE ( )  );
#5641 = VERTEX_POINT ( 'NONE', #367 ) ;
#5642 = CARTESIAN_POINT ( 'NONE',  ( 0.6009452777970410997, 18.00606236585372955, -44.61081509289886071 ) ) ;
#5643 = CARTESIAN_POINT ( 'NONE',  ( 0.9787284016396619046, 41.50936080613161039, -5.771391894094023201 ) ) ;
#5644 = B_SPLINE_CURVE_WITH_KNOTS ( 'NONE', 3,
 ( #35319, #45343, #59400, #50020 ),
 .UNSPECIFIED., .F., .F.,
 ( 4, 4 ),
 ( 0.000000000000000000, 0.004447772540403806783 ),
 .UNSPECIFIED. ) ;
#5645 = DIRECTION ( 'NONE',  ( -2.280301054154487250E-31, 0.000000000000000000, 1.000000000000000000 ) ) ;
#5646 = CARTESIAN_POINT ( 'NONE',  ( 0.5809828226811617480, 46.40184912890855884, -11.86925843957117799 ) ) ;
#5647 = DIRECTION ( 'NONE',  ( 0.000000000000000000, 0.000000000000000000, -1.000000000000000000 ) ) ;
#5648 = FACE_OUTER_BOUND ( 'NONE', #23532, .T. ) ;
#5649 = CARTESIAN_POINT ( 'NONE',  ( 5.981074661064941900, -0.008585178657475886835, -20.52466374824937034 ) ) ;
#5650 = CARTESIAN_POINT ( 'NONE',  ( 3.660087539127337752, 45.87884541725766496, -14.24113226412002930 ) ) ;
#5651 =( BOUNDED_SURFACE ( )  B_SPLINE_SURFACE ( 3, 1, ( 
 ( #57482, #4253 ),
 ( #5179, #18081 ),
 ( #9913, #24308 ),
 ( #19314, #38133 ) ),
 .UNSPECIFIED., .F., .F., .F. ) 
 B_SPLINE_SURFACE_WITH_KNOTS ( ( 4, 4 ),
 ( 2, 2 ),
 ( 0.000000000000000000, 1.000000000000000000 ),
 ( 0.000000000000000000, 1.000000000000000000 ),
 .UNSPECIFIED. ) 
 GEOMETRIC_REPRESENTATION_ITEM ( )  RATIONAL_B_SPLINE_SURFACE ( (
 ( 1.000000000000000000, 1.000000000000000000),
 ( 0.9952954269826590483, 0.8620686068821339365),
 ( 0.9952954269826590483, 0.8620686068821339365),
 ( 1.000000000000000000, 1.000000000000000000) ) ) 
 REPRESENTATION_ITEM ( '' )  SURFACE ( )  );
#5652 = CARTESIAN_POINT ( 'NONE',  ( 4.291220156522060236, 13.00516750528111132, 45.27973736082483924 ) ) ;
#5653 = B_SPLINE_CURVE_WITH_KNOTS ( 'NONE', 3,
 ( #3032, #26223, #55644, #17768, #12158, #50340, #50956, #7409, #50642, #45365, #26539, #45065, #55962, #40988, #2411, #21534, #7729, #59738, #54718 ),
 .UNSPECIFIED., .F., .F.,
 ( 4, 3, 3, 3, 3, 3, 4 ),
 ( 8.674676106452504675E-19, 0.0002612768053151716548, 0.0003919133833142916844, 0.0005225499612322607535, 0.0006531865391693360669, 0.0008112755173415198574, 0.0009693688056799731152 ),
 .UNSPECIFIED. ) ;
#5654 = EDGE_CURVE ( 'NONE', #21051, #44755, #60963, .T. ) ;
#5655 = DIRECTION ( 'NONE',  ( 0.000000000000000000, 0.000000000000000000, -1.000000000000000000 ) ) ;
#5656 = CARTESIAN_POINT ( 'NONE',  ( 0.6041374136657476912, 44.51224464244974399, 18.24862627831550199 ) ) ;
#5657 = VECTOR ( 'NONE', #34746, 1000.000000000000114 ) ;
#5658 = CARTESIAN_POINT ( 'NONE',  ( 0.5832655196449137991, -1.794523853054427409, 46.86165668341387658 ) ) ;
#5659 = EDGE_CURVE ( 'NONE', #44157, #7098, #55389, .T. ) ;
#5660 = DIRECTION ( 'NONE',  ( 0.09722883295013598492, 0.7529176304110274387, 0.6508929219613607264 ) ) ;
#5661 = CARTESIAN_POINT ( 'NONE',  ( 0.8560838555295214869, 21.73747136795201129, -41.56747734237908531 ) ) ;
#5662 = EDGE_LOOP ( 'NONE', ( #16859, #52144, #6355, #16895 ) ) ;
#5663 = CARTESIAN_POINT ( 'NONE',  ( 1.827326673878743923, -1.232746109312476301, 43.03225468313000590 ) ) ;
#5664 = CARTESIAN_POINT ( 'NONE',  ( 0.9783242366443547500, -1.668301681818695759, 41.87542548685285482 ) ) ;
#5665 = CARTESIAN_POINT ( 'NONE',  ( 0.6001305935487422083, 24.50730504006456556, -41.40054608060269459 ) ) ;
#5666 = ORIENTED_EDGE ( 'NONE', *, *, #23767, .T. ) ;
#5667 = CARTESIAN_POINT ( 'NONE',  ( 0.9757402383260935785, 5.516496958497070224, 42.55239275983112179 ) ) ;
#5668 = CARTESIAN_POINT ( 'NONE',  ( 5.896278296736517710, -15.78795198421076940, -12.46064010228362484 ) ) ;
#5669 = EDGE_LOOP ( 'NONE', ( #31084, #25212, #60089, #35318 ) ) ;
#5670 = VERTEX_POINT ( 'NONE', #24822 ) ;
#5671 = CARTESIAN_POINT ( 'NONE',  ( 0.6252788684277227338, 37.83342009078897661, 31.30617599464285306 ) ) ;
#5672 = CIRCLE ( 'NONE', #40766, 47.09074272231896430 ) ;
#5673 = ORIENTED_EDGE ( 'NONE', *, *, #2755, .F. ) ;
#5674 = CARTESIAN_POINT ( 'NONE',  ( 1.157644175074337367, -41.87004051356380785, 1.975343735077094376 ) ) ;
#5675 = CIRCLE ( 'NONE', #20745, 43.12527911185304674 ) ;
#5676 = VERTEX_POINT ( 'NONE', #43962 ) ;
#5677 = ORIENTED_EDGE ( 'NONE', *, *, #1042, .T. ) ;
#5678 = DIRECTION ( 'NONE',  ( 0.000000000000000000, 0.000000000000000000, -1.000000000000000000 ) ) ;
#5679 = VERTEX_POINT ( 'NONE', #999 ) ;
#5680 = CARTESIAN_POINT ( 'NONE',  ( 0.6027935024548037868, -29.42425667880464957, 38.05972402498726126 ) ) ;
#5681 = CARTESIAN_POINT ( 'NONE',  ( 2.301430502907646503, 47.77346269870100315, -4.990893951996506317 ) ) ;
#5682 = FACE_OUTER_BOUND ( 'NONE', #48485, .T. ) ;
#5683 = EDGE_LOOP ( 'NONE', ( #45717, #23368, #43499, #25368 ) ) ;
#5684 = EDGE_CURVE ( 'NONE', #4853, #60714, #58300, .T. ) ;
#5685 = CARTESIAN_POINT ( 'NONE',  ( 0.2940133293163024186, 37.40612136450513248, -23.38851500292304308 ) ) ;
#5686 = CARTESIAN_POINT ( 'NONE',  ( 3.407937589446174087, -12.82481284928207010, 4.815089211105012978 ) ) ;
#5687 = VERTEX_POINT ( 'NONE', #58938 ) ;
#5688 = EDGE_CURVE ( 'NONE', #43133, #3989, #6290, .T. ) ;
#5689 = AXIS2_PLACEMENT_3D ( 'NONE', #15663, #57917, #14732 ) ;
#5690 = ORIENTED_EDGE ( 'NONE', *, *, #34450, .T. ) ;
#5691 = EDGE_CURVE ( 'NONE', #45083, #19517, #49236, .T. ) ;
#5692 = CARTESIAN_POINT ( 'NONE',  ( 5.895596859100789899, -9.662743138698242973, -17.63971593444825103 ) ) ;
#5693 = CARTESIAN_POINT ( 'NONE',  ( 4.967162193818130511, 0.000000000000000000, 0.000000000000000000 ) ) ;
#5694 = CARTESIAN_POINT ( 'NONE',  ( 0.8560838555295158248, -14.76796170096741534, 44.52280473286123907 ) ) ;
#5695 = FACE_OUTER_BOUND ( 'NONE', #40980, .T. ) ;
#5696 = ADVANCED_FACE ( 'NONE', ( #39559 ), #8579, .F. ) ;
#5697 = CARTESIAN_POINT ( 'NONE',  ( 0.1092565886968783623, 5.936467125236458031, 42.71401356099880786 ) ) ;
#5698 = VERTEX_POINT ( 'NONE', #59556 ) ;
#5699 = CARTESIAN_POINT ( 'NONE',  ( 0.1158516988532803799, -1.463449468457666436, -44.09989200084357464 ) ) ;
#5700 = CARTESIAN_POINT ( 'NONE',  ( 3.678834586032788678, 34.27179800835390466, -34.98651498653363490 ) ) ;
#5701 = CARTESIAN_POINT ( 'NONE',  ( 4.975610109902397937, -5.269241389991576874, 48.62802178077752302 ) ) ;
#5702 = CARTESIAN_POINT ( 'NONE',  ( 2.299746137290199943, 29.09984276079479315, 39.46492732773186418 ) ) ;
#5703 = ORIENTED_EDGE ( 'NONE', *, *, #50087, .F. ) ;
#5704 = CARTESIAN_POINT ( 'NONE',  ( 0.5809828226811617480, -46.11980934799329646, -12.92184523170252497 ) ) ;
#5705 = CARTESIAN_POINT ( 'NONE',  ( 1.231276596079881047, 32.36747132271556637, 26.63876069172986405 ) ) ;
#5706 = CARTESIAN_POINT ( 'NONE',  ( -6.078457390727109555, 9.985927120572254623, -16.46437883979007921 ) ) ;
#5707 = CARTESIAN_POINT ( 'NONE',  ( 0.6026777506516366456, -35.39729640274160971, -34.03788768436836421 ) ) ;
#5708 = ORIENTED_EDGE ( 'NONE', *, *, #59120, .F. ) ;
#5709 = ORIENTED_EDGE ( 'NONE', *, *, #8833, .T. ) ;
#5710 = PLANE ( 'NONE',  #57913 ) ;
#5711 = LINE ( 'NONE', #1329, #40712 ) ;
#5712 = CARTESIAN_POINT ( 'NONE',  ( 0.9790724872846757743, 15.10001979691015528, -39.09379250104007042 ) ) ;
#5713 = CARTESIAN_POINT ( 'NONE',  ( 2.881901170002227897, 8.474399077991585715E-12, -49.00591519830774700 ) ) ;
#5714 = CARTESIAN_POINT ( 'NONE',  ( 0.1073791018717578927, 34.50606437925546999, -25.86618856530675714 ) ) ;
#5715 = CARTESIAN_POINT ( 'NONE',  ( 0.1073791018717578927, -43.12183934961191056, -0.4849339620931655825 ) ) ;
#5716 = CARTESIAN_POINT ( 'NONE',  ( 0.7057020205115017708, 0.8412108057959468699, -47.89404687311022002 ) ) ;
#5717 = CARTESIAN_POINT ( 'NONE',  ( -1.200000000000006617, 6.873330160214519262E-16, 5.612499999999999822 ) ) ;
#5718 = LINE ( 'NONE', #57731, #19116 ) ;
#5719 = AXIS2_PLACEMENT_3D ( 'NONE', #43668, #42731, #38966 ) ;
#5720 = CARTESIAN_POINT ( 'NONE',  ( 0.1102144999581332607, 30.58258619461921413, -30.40435207217196734 ) ) ;
#5721 = CARTESIAN_POINT ( 'NONE',  ( 0.7246131072078552116, 38.65593150731050542, -28.62741613354252479 ) ) ;
#5722 = ORIENTED_EDGE ( 'NONE', *, *, #43935, .F. ) ;
#5723 = AXIS2_PLACEMENT_3D ( 'NONE', #18932, #33950, #38055 ) ;
#5724 = VECTOR ( 'NONE', #56583, 1000.000000000000227 ) ;
#5725 = CARTESIAN_POINT ( 'NONE',  ( 0.1158816050234198480, -7.047819867384492731, -43.55766610393698812 ) ) ;
#5726 = CARTESIAN_POINT ( 'NONE',  ( 1.227938101723757836, -15.63977281655870222, 39.96870412324331312 ) ) ;
#5727 = CARTESIAN_POINT ( 'NONE',  ( 0.3676999524040366896, 43.44964275340416293, 7.620966337964807380 ) ) ;
#5728 = CARTESIAN_POINT ( 'NONE',  ( 0.7048096507298579061, -0.8437160066910636136, 48.10291524268439645 ) ) ;
#5729 = CARTESIAN_POINT ( 'NONE',  ( 0.8751705887134423323, -34.63284514348608667, 33.37254303619495488 ) ) ;
#5730 = CARTESIAN_POINT ( 'NONE',  ( 0.5817217712918332229, -13.45862205245476773, -44.92327288229956395 ) ) ;
#5731 = DIRECTION ( 'NONE',  ( 0.000000000000000000, 0.000000000000000000, -1.000000000000000000 ) ) ;
#5732 = CARTESIAN_POINT ( 'NONE',  ( 4.975610109902397937, -17.43163075979710541, 45.70106843599904778 ) ) ;
#5733 =( BOUNDED_SURFACE ( )  B_SPLINE_SURFACE ( 3, 1, ( 
 ( #16778, #41519 ),
 ( #36506, #46217 ),
 ( #22388, #17088 ),
 ( #31165, #7651 ) ),
 .UNSPECIFIED., .F., .F., .F. ) 
 B_SPLINE_SURFACE_WITH_KNOTS ( ( 4, 4 ),
 ( 2, 2 ),
 ( 0.000000000000000000, 1.000000000000000000 ),
 ( 0.000000000000000000, 1.000000000000000000 ),
 .UNSPECIFIED. ) 
 GEOMETRIC_REPRESENTATION_ITEM ( )  RATIONAL_B_SPLINE_SURFACE ( (
 ( 1.000000000000000000, 1.000000000000000000),
 ( 0.9953040768229005630, 0.8617119497784937465),
 ( 0.9953040768229005630, 0.8617119497784937465),
 ( 1.000000000000000000, 1.000000000000000000) ) ) 
 REPRESENTATION_ITEM ( '' )  SURFACE ( )  );
#5734 = ADVANCED_FACE ( 'NONE', ( #26357 ), #9320, .F. ) ;
#5735 = FACE_OUTER_BOUND ( 'NONE', #38445, .T. ) ;
#5736 = CARTESIAN_POINT ( 'NONE',  ( 0.8744876279028263033, -34.64280934553510605, -34.78829991575325664 ) ) ;
#5737 = CARTESIAN_POINT ( 'NONE',  ( 0.6041374136657476912, -12.61972904329569012, -46.42299778158151469 ) ) ;
#5739 = VERTEX_POINT ( 'NONE', #40189 ) ;
#5738 = CARTESIAN_POINT ( 'NONE',  ( 1.154321713695928509, 10.30834583266730320, 41.66001467525142488 ) ) ;
#5741 = ORIENTED_EDGE ( 'NONE', *, *, #14855, .F. ) ;
#5740 = B_SPLINE_CURVE_WITH_KNOTS ( 'NONE', 3,
 ( #23702, #42832, #20546, #39061, #29317, #44079 ),
 .UNSPECIFIED., .F., .F.,
 ( 4, 2, 4 ),
 ( 7.040638946443416885E-18, 0.0002445244328975376734, 0.0004890488657950682995 ),
 .UNSPECIFIED. ) ;
#5742 = CARTESIAN_POINT ( 'NONE',  ( 0.1102847568649952675, -43.12433804869904463, 0.09217763870885797850 ) ) ;
#5743 = CARTESIAN_POINT ( 'NONE',  ( 0.3676999524040366896, -43.84864779214676389, -4.821480075983068048 ) ) ;
#5744 = CARTESIAN_POINT ( 'NONE',  ( 0.1155031312995260795, 41.82288736169277854, 14.06370240238919145 ) ) ;
#5745 = B_SPLINE_CURVE_WITH_KNOTS ( 'NONE', 3,
 ( #21031, #35452, #35767, #11967 ),
 .UNSPECIFIED., .F., .F.,
 ( 4, 4 ),
 ( 0.000000000000000000, 0.004446090762761352976 ),
 .UNSPECIFIED. ) ;
#5746 = ORIENTED_EDGE ( 'NONE', *, *, #9922, .T. ) ;
#5747 = CARTESIAN_POINT ( 'NONE',  ( 4.962356264823608143, 0.000000000000000000, 0.000000000000000000 ) ) ;
#5748 = DIRECTION ( 'NONE',  ( 0.000000000000000000, 0.000000000000000000, 1.000000000000000000 ) ) ;
#5749 = CARTESIAN_POINT ( 'NONE',  ( 0.6845945791218034371, 45.46290160446757511, -11.55556569002327194 ) ) ;
#5750 = VECTOR ( 'NONE', #23328, 1000.000000000000227 ) ;
#5751 = ORIENTED_EDGE ( 'NONE', *, *, #6356, .T. ) ;
#5752 = VERTEX_POINT ( 'NONE', #16985 ) ;
#5753 = CARTESIAN_POINT ( 'NONE',  ( 0.5549461598389366923, 28.99592290077940859, -33.23332891238644038 ) ) ;
#5754 = CARTESIAN_POINT ( 'NONE',  ( 4.960156602257177916, -45.62767441207045493, -8.553784487773349099 ) ) ;
#5755 = CIRCLE ( 'NONE', #22782, 5.612499999999999822 ) ;
#5756 = CARTESIAN_POINT ( 'NONE',  ( 1.227938101723748288, -39.32113113558953899, -17.20315230597885758 ) ) ;
#5757 = CARTESIAN_POINT ( 'NONE',  ( 0.6039202388192952409, 33.14386950699269363, -36.23599904725178078 ) ) ;
#5758 = CARTESIAN_POINT ( 'NONE',  ( 1.231276596079881935, 3.353048872156085825, 41.78556968953515849 ) ) ;
#5759 = CARTESIAN_POINT ( 'NONE',  ( 0.9730545539215883499, -10.61654491617534291, -41.57420493492396929 ) ) ;
#5760 = FACE_OUTER_BOUND ( 'NONE', #47572, .T. ) ;
#5761 = ADVANCED_FACE ( 'NONE', ( #25426 ), #47378, .F. ) ;
#5762 = B_SPLINE_CURVE_WITH_KNOTS ( 'NONE', 3,
 ( #986, #15110, #9780, #14805, #11029, #15732 ),
 .UNSPECIFIED., .F., .F.,
 ( 4, 2, 4 ),
 ( 0.000000000000000000, 0.0002447195606305748003, 0.0004894391212611496006 ),
 .UNSPECIFIED. ) ;
#5763 = CARTESIAN_POINT ( 'NONE',  ( 0.9757787079277435716, 42.53619983261577886, 5.639827755376784602 ) ) ;
#5764 = EDGE_CURVE ( 'NONE', #39035, #10587, #45012, .T. ) ;
#5765 = ORIENTED_EDGE ( 'NONE', *, *, #56317, .F. ) ;
#5766 = ORIENTED_EDGE ( 'NONE', *, *, #55692, .F. ) ;
#5767 = CARTESIAN_POINT ( 'NONE',  ( 1.157643937452369931, -30.52765900992394776, 28.72393270373265750 ) ) ;
#5768 = CARTESIAN_POINT ( 'NONE',  ( 0.9730545539215883499, -0.5054011016615761465, 42.90536227157002003 ) ) ;
#5769 = AXIS2_PLACEMENT_3D ( 'NONE', #42292, #13164, #32262 ) ;
#5770 = VERTEX_POINT ( 'NONE', #1923 ) ;
#5771 = CARTESIAN_POINT ( 'NONE',  ( -6.015611763856276717, -13.31979030221808458, 13.32857883366828666 ) ) ;
#5772 = CARTESIAN_POINT ( 'NONE',  ( 0.8560838555295158248, 5.603718208094640829, -46.57221463840858888 ) ) ;
#5773 = ADVANCED_FACE ( 'NONE', ( #16047 ), #2543, .F. ) ;
#5774 = CARTESIAN_POINT ( 'NONE',  ( 4.975610109902397937, -22.11219452748616021, 43.62912170003406942 ) ) ;
#5775 = CARTESIAN_POINT ( 'NONE',  ( 0.5809828226811617480, -11.86925843957133786, -46.40184912890851621 ) ) ;
#5776 = VERTEX_POINT ( 'NONE', #61092 ) ;
#5777 = CARTESIAN_POINT ( 'NONE',  ( 0.5834584762367771571, 46.50150427475632853, -6.070097956211762735 ) ) ;
#5778 = CARTESIAN_POINT ( 'NONE',  ( 1.227938101723756947, 10.28900963485438425, -41.66816631169181306 ) ) ;
#5779 = CARTESIAN_POINT ( 'NONE',  ( 0.7948884756798518803, 28.79738896807402071, -39.76693391778652398 ) ) ;
#5780 = CARTESIAN_POINT ( 'NONE',  ( 0.5838002273316424962, 29.04904228829611412, 38.08117724016815231 ) ) ;
#5781 = VERTEX_POINT ( 'NONE', #18512 ) ;
#5782 = CARTESIAN_POINT ( 'NONE',  ( 0.5807400328401574052, -47.89582301953904420, 0.5448834511088260779 ) ) ;
#5783 = ORIENTED_EDGE ( 'NONE', *, *, #54717, .T. ) ;
#5784 = CARTESIAN_POINT ( 'NONE',  ( 0.8557997880470690211, 47.89938907511594124, -0.9121262075947851322 ) ) ;
#5785 = CARTESIAN_POINT ( 'NONE',  ( 0.5819845901640494645, 24.34012668949545244, -41.25023214430176210 ) ) ;
#5786 = EDGE_CURVE ( 'NONE', #41582, #52129, #57955, .T. ) ;
#5787 = VECTOR ( 'NONE', #10845, 1000.000000000000114 ) ;
#5788 = ORIENTED_EDGE ( 'NONE', *, *, #38677, .F. ) ;
#5789 = CARTESIAN_POINT ( 'NONE',  ( -2.739355103387248747, 10.22927580983311913, 10.87241846864716699 ) ) ;
#5790 = FACE_OUTER_BOUND ( 'NONE', #16259, .T. ) ;
#5791 = B_SPLINE_CURVE_WITH_KNOTS ( 'NONE', 3,
 ( #24381, #556, #29385, #58184, #48489, #39744, #15311, #34413, #15920, #38819, #35037, #54095, #11217, #53484, #30306, #49415, #6469, #57873, #10598 ),
 .UNSPECIFIED., .F., .F.,
 ( 4, 3, 3, 3, 3, 3, 4 ),
 ( 1.250973872328959318E-17, 0.0002732106629380645461, 0.0004098138914053644816, 0.0005464171197651422444, 0.0006830203481512590186, 0.0008196235766963655845, 0.001011968216111138776 ),
 .UNSPECIFIED. ) ;
#5792 = EDGE_CURVE ( 'NONE', #27245, #44212, #53178, .T. ) ;
#5793 = CARTESIAN_POINT ( 'NONE',  ( 0.3622758884714730732, -22.26738722580142138, -36.91764744403313614 ) ) ;
#5794 = CARTESIAN_POINT ( 'NONE',  ( 4.975610109902397937, 2.142807115709817189, -48.86571174967818365 ) ) ;
#5795 = CARTESIAN_POINT ( 'NONE',  ( 2.282816707992307848, -18.57323074318924228, 43.14547561643301066 ) ) ;
#5796 = CARTESIAN_POINT ( 'NONE',  ( 0.6064515330803569304, 45.41333491424882851, 11.70313411028668860 ) ) ;
#5797 = CARTESIAN_POINT ( 'NONE',  ( 0.1119899015040010798, -7.595748810241286897, 43.46568656082891380 ) ) ;
#5798 = CARTESIAN_POINT ( 'NONE',  ( 0.5997462898726536595, 37.05192695178125462, 32.22896739432052016 ) ) ;
#5799 = VERTEX_POINT ( 'NONE', #27288 ) ;
#5800 = FACE_OUTER_BOUND ( 'NONE', #1304, .T. ) ;
#5801 = CARTESIAN_POINT ( 'NONE',  ( 0.9787284016396604613, 41.55927417454115869, 5.400252680583206732 ) ) ;
#5802 = CARTESIAN_POINT ( 'NONE',  ( 1.657374760986086049, -16.69403132851356730, 40.77008419484624113 ) ) ;
#5803 = VERTEX_POINT ( 'NONE', #32616 ) ;
#5804 = CARTESIAN_POINT ( 'NONE',  ( 1.227938101723748288, 42.43379953535185933, 6.439911493064710335 ) ) ;
#5805 = CARTESIAN_POINT ( 'NONE',  ( 0.1129192098497455998, -27.88830454350494392, 34.19348267541455044 ) ) ;
#5806 = CARTESIAN_POINT ( 'NONE',  ( 0.5997462898726536595, 10.41743419021343087, -47.98988117339822423 ) ) ;
#5807 = CARTESIAN_POINT ( 'NONE',  ( 4.834790513006555379, 29.09828987666571010, -37.22739404226293658 ) ) ;
#5808 = CARTESIAN_POINT ( 'NONE',  ( 0.5997462898726536595, -19.39900779840473888, 45.11352487427402025 ) ) ;
#5809 = CARTESIAN_POINT ( 'NONE',  ( -1.599999999999940359, -56.56854249492410247, 56.56854249492352693 ) ) ;
#5810 = CARTESIAN_POINT ( 'NONE',  ( 5.917102823773431552, 20.06644099299509776, 1.351911212464782075 ) ) ;
#5811 = EDGE_CURVE ( 'NONE', #57208, #58714, #27008, .T. ) ;
#5812 = CARTESIAN_POINT ( 'NONE',  ( 1.199999999999992628, 6.873330160214519262E-16, 5.612499999999999822 ) ) ;
#5813 = B_SPLINE_CURVE_WITH_KNOTS ( 'NONE', 3,
 ( #59306, #16412, #2288, #60537, #50840, #7931 ),
 .UNSPECIFIED., .F., .F.,
 ( 4, 2, 4 ),
 ( 1.964972962535902174E-17, 0.0002293319059085107401, 0.0004586638118170018020 ),
 .UNSPECIFIED. ) ;
#5814 = VECTOR ( 'NONE', #17909, 1000.000000000000114 ) ;
#5815 = CARTESIAN_POINT ( 'NONE',  ( 4.960156602257180580, -30.22163187094364645, -35.23783291257201711 ) ) ;
#5817 = EDGE_LOOP ( 'NONE', ( #32491, #52925, #29291, #12463 ) ) ;
#5816 = CARTESIAN_POINT ( 'NONE',  ( 1.827119703190779321, -37.88337895042280934, -20.44859290426024145 ) ) ;
#5818 = ORIENTED_EDGE ( 'NONE', *, *, #8838, .T. ) ;
#5819 = CARTESIAN_POINT ( 'NONE',  ( 0.5839879327111936469, -12.30864801674743525, 46.28746210677709882 ) ) ;
#5820 = CIRCLE ( 'NONE', #25831, 15.99999999999999645 ) ;
#5821 = DIRECTION ( 'NONE',  ( 1.836909530733573776E-16, -1.000000000000000000, 0.000000000000000000 ) ) ;
#5822 = CARTESIAN_POINT ( 'NONE',  ( 0.1102847568649952675, 16.58813073670652116, 39.80641842112251538 ) ) ;
#5823 = FACE_OUTER_BOUND ( 'NONE', #50170, .T. ) ;
#5824 = CARTESIAN_POINT ( 'NONE',  ( 0.9730545539215883499, 42.60426903087360984, -5.099196237954451760 ) ) ;
#5825 = CARTESIAN_POINT ( 'NONE',  ( -6.010958268070873523, 18.68034667844852237, -2.473955915502024983 ) ) ;
#5826 = ORIENTED_EDGE ( 'NONE', *, *, #43405, .F. ) ;
#5827 = EDGE_LOOP ( 'NONE', ( #13290, #11219, #21295, #29013 ) ) ;
#5828 = DIRECTION ( 'NONE',  ( 1.000000000000000000, 0.000000000000000000, 0.000000000000000000 ) ) ;
#5829 = AXIS2_PLACEMENT_3D ( 'NONE', #25402, #26031, #1578 ) ;
#5830 = CARTESIAN_POINT ( 'NONE',  ( 0.8751705887134553219, 19.22545746485597817, 44.08562551107088723 ) ) ;
#5831 = DIRECTION ( 'NONE',  ( -1.000000000000000000, -0.000000000000000000, -0.000000000000000000 ) ) ;
#5832 = ORIENTED_EDGE ( 'NONE', *, *, #45294, .F. ) ;
#5833 = CARTESIAN_POINT ( 'NONE',  ( 4.956445790443991584, 30.81386304088947625, 35.60960396630300551 ) ) ;
#5834 = CARTESIAN_POINT ( 'NONE',  ( 4.553261556744875094, 0.000000000000000000, 0.000000000000000000 ) ) ;
#5835 = ORIENTED_EDGE ( 'NONE', *, *, #15034, .F. ) ;
#5836 = AXIS2_PLACEMENT_3D ( 'NONE', #18723, #56911, #43468 ) ;
#5837 = CARTESIAN_POINT ( 'NONE',  ( 2.301529144917015213, 46.04684498357980971, -13.67115311794016463 ) ) ;
#5838 = EDGE_CURVE ( 'NONE', #61564, #15021, #37028, .T. ) ;
#5839 = ORIENTED_EDGE ( 'NONE', *, *, #7617, .F. ) ;
#5840 = CARTESIAN_POINT ( 'NONE',  ( 1.088313998177382169, -33.56520876252045582, -26.73848503423889156 ) ) ;
#5841 = CARTESIAN_POINT ( 'NONE',  ( 3.678748215320120085, 43.29174540921691516, -22.90060247511034675 ) ) ;
#5842 = ORIENTED_EDGE ( 'NONE', *, *, #39412, .T. ) ;
#5843 = CIRCLE ( 'NONE', #43791, 48.09070567114147110 ) ;
#5844 = CARTESIAN_POINT ( 'NONE',  ( 0.8557997880470690211, 0.9121262075946178216, 47.89938907511594124 ) ) ;
#5845 = FACE_OUTER_BOUND ( 'NONE', #2095, .T. ) ;
#5846 = ADVANCED_FACE ( 'NONE', ( #42338 ), #49385, .F. ) ;
#5847 = CARTESIAN_POINT ( 'NONE',  ( 4.956445790443988031, 0.000000000000000000, 0.000000000000000000 ) ) ;
#5848 = CARTESIAN_POINT ( 'NONE',  ( 0.8557997880470697982, -47.37054680076710866, 7.156447707085535903 ) ) ;
#5849 = EDGE_LOOP ( 'NONE', ( #53246, #30508, #35852, #21741 ) ) ;
#5850 = DIRECTION ( 'NONE',  ( 0.000000000000000000, 0.000000000000000000, 1.000000000000000000 ) ) ;
#5851 = CARTESIAN_POINT ( 'NONE',  ( 4.291220156522059348, 14.90393520085114254, 44.69073408252013024 ) ) ;
#5852 = VERTEX_POINT ( 'NONE', #41723 ) ;
#5853 = DIRECTION ( 'NONE',  ( 0.000000000000000000, 0.000000000000000000, -1.000000000000000000 ) ) ;
#5854 =( BOUNDED_SURFACE ( )  B_SPLINE_SURFACE ( 3, 1, ( 
 ( #46587, #18074 ),
 ( #9906, #57175 ),
 ( #14930, #28384 ),
 ( #24618, #61571 ) ),
 .UNSPECIFIED., .F., .F., .F. ) 
 B_SPLINE_SURFACE_WITH_KNOTS ( ( 4, 4 ),
 ( 2, 2 ),
 ( 0.000000000000000000, 1.000000000000000000 ),
 ( 0.000000000000000000, 1.000000000000000000 ),
 .UNSPECIFIED. ) 
 GEOMETRIC_REPRESENTATION_ITEM ( )  RATIONAL_B_SPLINE_SURFACE ( (
 ( 1.000000000000000000, 1.000000000000000000),
 ( 0.9751682680413298332, 0.9999560080971552356),
 ( 0.9751682680413298332, 0.9999560080971552356),
 ( 1.000000000000000000, 1.000000000000000000) ) ) 
 REPRESENTATION_ITEM ( '' )  SURFACE ( )  );
#5855 = VERTEX_POINT ( 'NONE', #41114 ) ;
#5856 = ORIENTED_EDGE ( 'NONE', *, *, #7952, .T. ) ;
#5857 = CARTESIAN_POINT ( 'NONE',  ( 1.000433927950261870, -31.52035191441499862, -27.62039269895128868 ) ) ;
#5858 = CARTESIAN_POINT ( 'NONE',  ( 0.5997462898726536595, -48.63480578518795738, -6.797594896826151256 ) ) ;
#5859 = AXIS2_PLACEMENT_3D ( 'NONE', #8779, #36697, #61079 ) ;
#5860 = VECTOR ( 'NONE', #19628, 999.9999999999998863 ) ;
#5861 = CARTESIAN_POINT ( 'NONE',  ( 0.6067375320500766334, 41.12099578548248502, 24.55990317723871641 ) ) ;
#5862 = ORIENTED_EDGE ( 'NONE', *, *, #42667, .T. ) ;
#5863 = CARTESIAN_POINT ( 'NONE',  ( 0.5839880159502333079, 6.206687493267690314, 47.49213420504721483 ) ) ;
#5864 = CARTESIAN_POINT ( 'NONE',  ( 0.5832366564991514624, -5.981458972434077204, 47.52097076201149406 ) ) ;
#5865 = EDGE_CURVE ( 'NONE', #25265, #27177, #52396, .T. ) ;
#5866 = CARTESIAN_POINT ( 'NONE',  ( 4.335381028904216727, -48.94118403004392093, 2.125406643849450550 ) ) ;
#5867 = VERTEX_POINT ( 'NONE', #32306 ) ;
#5868 = ORIENTED_EDGE ( 'NONE', *, *, #44516, .T. ) ;
#5869 = CARTESIAN_POINT ( 'NONE',  ( 0.9762797500689124330, -31.41867615533366376, -27.73430319715951242 ) ) ;
#5870 = LINE ( 'NONE', #55970, #28159 ) ;
#5871 = CARTESIAN_POINT ( 'NONE',  ( -6.078075953587585900, 7.799379819826266491, 17.60581860275808808 ) ) ;
#5872 = DIRECTION ( 'NONE',  ( -1.000000000000000000, -0.000000000000000000, -0.000000000000000000 ) ) ;
#5873 = CARTESIAN_POINT ( 'NONE',  ( 0.8751705887134553219, -13.30665218149330364, -46.21789262997752701 ) ) ;
#5874 = FACE_OUTER_BOUND ( 'NONE', #29230, .T. ) ;
#5875 = ORIENTED_EDGE ( 'NONE', *, *, #46846, .F. ) ;
#5876 = CARTESIAN_POINT ( 'NONE',  ( 3.661921753701996352, 41.39923634030784427, 22.33236114416415319 ) ) ;
#5877 = VECTOR ( 'NONE', #30955, 1000.000000000000114 ) ;
#5878 = ORIENTED_EDGE ( 'NONE', *, *, #46503, .F. ) ;
#5879 = CARTESIAN_POINT ( 'NONE',  ( 0.6017666602106490625, 12.78804974226035540, 46.37677619531716999 ) ) ;
#5880 = CARTESIAN_POINT ( 'NONE',  ( 2.788021980263895028, 5.971756191165462832E-15, 46.99417130740431503 ) ) ;
#5881 = LINE ( 'NONE', #49135, #60985 ) ;
#5882 = CARTESIAN_POINT ( 'NONE',  ( 5.960721111146673579, -18.96557324978281756, -7.848955554238449928 ) ) ;
#5883 = CARTESIAN_POINT ( 'NONE',  ( -6.077587904424778920, 19.09876248768967955, 2.456276212633274003 ) ) ;
#5884 = FACE_OUTER_BOUND ( 'NONE', #42609, .T. ) ;
#5885 = CARTESIAN_POINT ( 'NONE',  ( 4.958415959904820092, -11.02103540056541497, 44.06518730837441922 ) ) ;
#5886 = CARTESIAN_POINT ( 'NONE',  ( 0.9754292580325134576, -39.77696751020019406, 13.19546598633348644 ) ) ;
#5887 = CARTESIAN_POINT ( 'NONE',  ( 0.6845945791218023269, -41.46895371680806619, 21.92561055813899529 ) ) ;
#5888 = CARTESIAN_POINT ( 'NONE',  ( -6.015611763856276717, -18.20278301740940208, 4.870987357968111553 ) ) ;
#5889 = CARTESIAN_POINT ( 'NONE',  ( 3.678748215320119197, 2.858834614276290154, -48.89212491749258760 ) ) ;
#5890 = CARTESIAN_POINT ( 'NONE',  ( 2.879087469061463178, -19.38045785506447416, -39.50315848272703079 ) ) ;
#5891 = EDGE_CURVE ( 'NONE', #6804, #39984, #36794, .T. ) ;
#5892 = VECTOR ( 'NONE', #59160, 1000.000000000000000 ) ;
#5893 = ORIENTED_EDGE ( 'NONE', *, *, #54682, .F. ) ;
#5894 = EDGE_CURVE ( 'NONE', #6658, #45408, #26985, .T. ) ;
#5895 = PRESENTATION_STYLE_ASSIGNMENT (( #14727 ) ) ;
#5896 = AXIS2_PLACEMENT_3D ( 'NONE', #56429, #13544, #32650 ) ;
#5897 = CARTESIAN_POINT ( 'NONE',  ( 0.1102144999581333301, 37.28370465375326859, 21.67128446981392997 ) ) ;
#5898 = B_SPLINE_CURVE_WITH_KNOTS ( 'NONE', 3,
 ( #8427, #27553, #17858, #36983 ),
 .UNSPECIFIED., .F., .F.,
 ( 4, 4 ),
 ( 2.380113941701692686E-17, 0.004559932413162185935 ),
 .UNSPECIFIED. ) ;
#5899 = FACE_OUTER_BOUND ( 'NONE', #20816, .T. ) ;
#5900 = CARTESIAN_POINT ( 'NONE',  ( 0.1073791018717483448, -16.05399293000841254, 40.02496097243031414 ) ) ;
#5901 = CARTESIAN_POINT ( 'NONE',  ( 0.3676999524040323597, 5.056646555325726489, -43.82215089355327109 ) ) ;
#5902 = ORIENTED_EDGE ( 'NONE', *, *, #38511, .F. ) ;
#5903 = B_SPLINE_CURVE_WITH_KNOTS ( 'NONE', 3,
 ( #5848, #58473, #24998, #57546 ),
 .UNSPECIFIED., .F., .F.,
 ( 4, 4 ),
 ( 4.336808689942017736E-19, 0.004444878191957681718 ),
 .UNSPECIFIED. ) ;
#5904 = CARTESIAN_POINT ( 'NONE',  ( 7.839426360173755270, -8.264250432354510068, 2.910643653149725793E-16 ) ) ;
#5905 = CARTESIAN_POINT ( 'NONE',  ( 0.9749527285493306827, 16.68386601451091877, -39.53206838353028729 ) ) ;
#5906 =( BOUNDED_SURFACE ( )  B_SPLINE_SURFACE ( 3, 1, ( 
 ( #56028, #46658 ),
 ( #13146, #27533 ),
 ( #8728, #27843 ),
 ( #46975, #42576 ) ),
 .UNSPECIFIED., .F., .F., .F. ) 
 B_SPLINE_SURFACE_WITH_KNOTS ( ( 4, 4 ),
 ( 2, 2 ),
 ( 0.000000000000000000, 1.000000000000000000 ),
 ( 0.000000000000000000, 1.000000000000000000 ),
 .UNSPECIFIED. ) 
 GEOMETRIC_REPRESENTATION_ITEM ( )  RATIONAL_B_SPLINE_SURFACE ( (
 ( 1.000000000000000000, 1.000000000000000000),
 ( 0.9732289882329797637, 0.9999525324661233672),
 ( 0.9732289882329797637, 0.9999525324661233672),
 ( 1.000000000000000000, 1.000000000000000000) ) ) 
 REPRESENTATION_ITEM ( '' )  SURFACE ( )  );
#5907 = DIRECTION ( 'NONE',  ( -0.8660254037844348218, 0.5000000000000066613, 0.000000000000000000 ) ) ;
#5908 = VERTEX_POINT ( 'NONE', #55781 ) ;
#5909 = CARTESIAN_POINT ( 'NONE',  ( 0.2230388203127608437, -31.02270543585807161, -29.94794547692434605 ) ) ;
#5910 = CARTESIAN_POINT ( 'NONE',  ( 4.956445790444026223, 13.43466403631445338, -45.13366650706537797 ) ) ;
#5911 = EDGE_CURVE ( 'NONE', #8227, #45383, #61393, .T. ) ;
#5912 = ORIENTED_EDGE ( 'NONE', *, *, #55151, .T. ) ;
#5913 = CARTESIAN_POINT ( 'NONE',  ( 5.880360259849739535, -15.37531919565267735, 45.44137230084854906 ) ) ;
#5914 = AXIS2_PLACEMENT_3D ( 'NONE', #51156, #8238, #41179 ) ;
#5915 = EDGE_LOOP ( 'NONE', ( #46556, #34430, #13398, #58645 ) ) ;
#5916 = DIRECTION ( 'NONE',  ( 0.000000000000000000, 0.000000000000000000, -1.000000000000000000 ) ) ;
#5918 = ORIENTED_EDGE ( 'NONE', *, *, #2360, .F. ) ;
#5917 = EDGE_CURVE ( 'NONE', #56955, #40637, #1451, .T. ) ;
#5919 = CARTESIAN_POINT ( 'NONE',  ( 4.694002226626921015, 45.16857381419788453, 6.171281150417080141 ) ) ;
#5920 = CARTESIAN_POINT ( 'NONE',  ( -6.016761891674565099, -9.418621820384382559, -16.32039929810266798 ) ) ;
#5921 = ORIENTED_EDGE ( 'NONE', *, *, #43939, .T. ) ;
#5922 = CARTESIAN_POINT ( 'NONE',  ( 0.8560838555295223751, -46.85553835019177882, -2.220666565569921591 ) ) ;
#5923 = ORIENTED_EDGE ( 'NONE', *, *, #42959, .T. ) ;
#5924 = CARTESIAN_POINT ( 'NONE',  ( 0.9784957157296358954, 19.93608022797447532, -36.86306772551813538 ) ) ;
#5925 = ADVANCED_FACE ( 'NONE', ( #33239 ), #60173, .F. ) ;
#5926 = CARTESIAN_POINT ( 'NONE',  ( 5.958863334805807099, 5.311251202228851831, -19.82657410201437642 ) ) ;
#5927 =( BOUNDED_SURFACE ( )  B_SPLINE_SURFACE ( 3, 1, ( 
 ( #8942, #31510 ),
 ( #41551, #36541 ),
 ( #50917, #13658 ),
 ( #55607, #42179 ) ),
 .UNSPECIFIED., .F., .F., .F. ) 
 B_SPLINE_SURFACE_WITH_KNOTS ( ( 4, 4 ),
 ( 2, 2 ),
 ( 0.000000000000000000, 1.000000000000000000 ),
 ( 0.000000000000000000, 1.000000000000000000 ),
 .UNSPECIFIED. ) 
 GEOMETRIC_REPRESENTATION_ITEM ( )  RATIONAL_B_SPLINE_SURFACE ( (
 ( 1.000000000000000000, 1.000000000000000000),
 ( 0.9953485035131437453, 0.8621029689291515030),
 ( 0.9953485035131437453, 0.8621029689291515030),
 ( 1.000000000000000000, 1.000000000000000000) ) ) 
 REPRESENTATION_ITEM ( '' )  SURFACE ( )  );
#5928 = ORIENTED_EDGE ( 'NONE', *, *, #609, .F. ) ;
#5929 = CARTESIAN_POINT ( 'NONE',  ( 5.894904586330512508, 16.58261916749243881, 11.38183436918475167 ) ) ;
#5930 = FACE_OUTER_BOUND ( 'NONE', #51141, .T. ) ;
#5931 = CARTESIAN_POINT ( 'NONE',  ( -2.569797478183790229, 8.547745408040636761, 11.87678401312197529 ) ) ;
#5932 = CARTESIAN_POINT ( 'NONE',  ( -6.015611763856276717, -13.31979030221808458, 13.32857883366828666 ) ) ;
#5933 = EDGE_LOOP ( 'NONE', ( #25583, #3095, #57007, #56092 ) ) ;
#5934 = CARTESIAN_POINT ( 'NONE',  ( 0.6041374136657475802, -46.42299778158147205, -12.61972904329582867 ) ) ;
#5935 = EDGE_CURVE ( 'NONE', #12599, #35558, #31440, .T. ) ;
#5936 = CARTESIAN_POINT ( 'NONE',  ( 0.1152339509894530906, -17.65621462967984812, 40.43761584720249402 ) ) ;
#5937 = ORIENTED_EDGE ( 'NONE', *, *, #42970, .F. ) ;
#5938 = CARTESIAN_POINT ( 'NONE',  ( 0.5806925824938502512, -46.82446035038566379, -2.586943222941716858 ) ) ;
#5939 = VERTEX_POINT ( 'NONE', #4679 ) ;
#5940 = FACE_OUTER_BOUND ( 'NONE', #42713, .T. ) ;
#5941 = CARTESIAN_POINT ( 'NONE',  ( 0.1156495703730067576, 25.35586003454986681, 36.11126299562765496 ) ) ;
#5942 = ORIENTED_EDGE ( 'NONE', *, *, #61314, .T. ) ;
#5943 = DIRECTION ( 'NONE',  ( 0.07836865515943410021, -0.6993330359244864791, -0.7104869166657064028 ) ) ;
#5944 = DIRECTION ( 'NONE',  ( 1.000000000000000000, 0.000000000000000000, 0.000000000000000000 ) ) ;
#5945 = CARTESIAN_POINT ( 'NONE',  ( 52.49662775218939714, 12.37736723654698068, 1.751076765323000828 ) ) ;
#5946 = CARTESIAN_POINT ( 'NONE',  ( 0.9762797500689124330, -22.97506929404158171, -35.04955029839458547 ) ) ;
#5947 = CONICAL_SURFACE ( 'NONE', #26998, 47.09074272231896430, 0.04450589592586084303 ) ;
#5948 = VERTEX_POINT ( 'NONE', #5304 ) ;
#5949 = CARTESIAN_POINT ( 'NONE',  ( 0.6029303876144825880, 18.53079182983344708, -44.39523326884619081 ) ) ;
#5950 = CARTESIAN_POINT ( 'NONE',  ( 0.6067375320500720814, -5.548194933739853063, -47.57460111700608962 ) ) ;
#5951 = DIRECTION ( 'NONE',  ( 0.1024043820194936311, -0.3684880688409263305, 0.9239750460186089143 ) ) ;
#5952 = CARTESIAN_POINT ( 'NONE',  ( 5.901463166500146684, 17.94437285245843228, -9.083906278280815982 ) ) ;
#5953 = CARTESIAN_POINT ( 'NONE',  ( 4.390527457369401532, -9.463175119887736741, -42.90260660238439527 ) ) ;
#5954 = CARTESIAN_POINT ( 'NONE',  ( 1.227938101723748288, -42.65467462194921922, 4.762198645644287076 ) ) ;
#5955 = EDGE_CURVE ( 'NONE', #42350, #12019, #27665, .T. ) ;
#5956 = VECTOR ( 'NONE', #28723, 1000.000000000000000 ) ;
#5957 = CARTESIAN_POINT ( 'NONE',  ( -16.91888867401740981, -7.790380955814590891, -1.820995958802028580 ) ) ;
#5958 = CARTESIAN_POINT ( 'NONE',  ( 21.00000000000000355, 0.000000000000000000, 0.000000000000000000 ) ) ;
#5959 = EDGE_CURVE ( 'NONE', #12174, #21853, #56056, .T. ) ;
#5960 = FACE_OUTER_BOUND ( 'NONE', #32634, .T. ) ;
#5961 = CARTESIAN_POINT ( 'NONE',  ( 0.1155031312995260795, -43.74003612738039237, -5.809550077868878226 ) ) ;
#5962 = CARTESIAN_POINT ( 'NONE',  ( 0.1156867017252034557, 39.70013168197753117, 19.25726750369402396 ) ) ;
#5963 = CARTESIAN_POINT ( 'NONE',  ( 5.960221823109900008, 12.49951306783067828, 16.28072933292552094 ) ) ;
#5964 = EDGE_CURVE ( 'NONE', #21601, #29768, #59839, .T. ) ;
#5965 = ADVANCED_FACE ( 'NONE', ( #47946 ), #13361, .F. ) ;
#5966 = LINE ( 'NONE', #52988, #47262 ) ;
#5967 = CARTESIAN_POINT ( 'NONE',  ( 4.975610109902397937, 14.46773809681547718, 46.72401910687614190 ) ) ;
#5968 = VERTEX_POINT ( 'NONE', #57012 ) ;
#5969 = CARTESIAN_POINT ( 'NONE',  ( 3.661933894777872567, -39.81515357561435309, 25.04764880586393971 ) ) ;
#5970 = CARTESIAN_POINT ( 'NONE',  ( 3.050102900204245682, 18.72656562264871738, -39.80880542240235798 ) ) ;
#5971 = CARTESIAN_POINT ( 'NONE',  ( -6.016104459813371719, 9.416989654584535074, -16.32137543786072698 ) ) ;
#5972 = ORIENTED_EDGE ( 'NONE', *, *, #55071, .T. ) ;
#5973 = CARTESIAN_POINT ( 'NONE',  ( 0.3622758884714730732, -36.91764744403337062, 22.26738722580103413 ) ) ;
#5974 = CARTESIAN_POINT ( 'NONE',  ( 0.1064266379913939020, -39.62374453032509081, 17.02047542254779700 ) ) ;
#5975 = B_SPLINE_CURVE_WITH_KNOTS ( 'NONE', 3,
 ( #14426, #58532, #9704, #5294, #24421, #28814 ),
 .UNSPECIFIED., .F., .F.,
 ( 4, 2, 4 ),
 ( 0.000000000000000000, 0.0002450742804987318451, 0.0004901485609974636903 ),
 .UNSPECIFIED. ) ;
#5976 = PRODUCT_DEFINITION_CONTEXT ( 'detailed design', #10377, 'design' ) ;
#5977 = ORIENTED_EDGE ( 'NONE', *, *, #48509, .F. ) ;
#5978 = ORIENTED_EDGE ( 'NONE', *, *, #42470, .F. ) ;
#5979 = CARTESIAN_POINT ( 'NONE',  ( 5.960221823109900008, 5.307149561568086149, -19.82761049839337275 ) ) ;
#5980 = EDGE_CURVE ( 'NONE', #37398, #11505, #45657, .T. ) ;
#5981 = ORIENTED_EDGE ( 'NONE', *, *, #36796, .T. ) ;
#5982 = DIRECTION ( 'NONE',  ( -1.000000000000000000, -0.000000000000000000, -0.000000000000000000 ) ) ;
#5984 = ORIENTED_EDGE ( 'NONE', *, *, #38359, .T. ) ;
#5983 = EDGE_CURVE ( 'NONE', #32172, #32810, #59044, .T. ) ;
#5985 = ORIENTED_EDGE ( 'NONE', *, *, #18472, .T. ) ;
#5986 = CARTESIAN_POINT ( 'NONE',  ( 0.1087620492084205998, 10.81135549499722259, 41.74735017127134995 ) ) ;
#5987 = ORIENTED_EDGE ( 'NONE', *, *, #18436, .F. ) ;
#5988 = CARTESIAN_POINT ( 'NONE',  ( 0.3622758884714730732, -33.69533458712361806, 26.89560658783328861 ) ) ;
#5989 = B_SPLINE_CURVE_WITH_KNOTS ( 'NONE', 3,
 ( #21368, #59249, #39260, #11352 ),
 .UNSPECIFIED., .F., .F.,
 ( 4, 4 ),
 ( 0.000000000000000000, 0.004447772540403784232 ),
 .UNSPECIFIED. ) ;
#5990 = CARTESIAN_POINT ( 'NONE',  ( 0.8557997880470599172, 34.51495345639595058, -33.22501220301865033 ) ) ;
#5991 = ORIENTED_EDGE ( 'NONE', *, *, #26883, .F. ) ;
#5993 = B_SPLINE_CURVE_WITH_KNOTS ( 'NONE', 3,
 ( #48472, #34096, #28135, #28756 ),
 .UNSPECIFIED., .F., .F.,
 ( 4, 4 ),
 ( 0.000000000000000000, 0.004442905043737214836 ),
 .UNSPECIFIED. ) ;
#5992 = CARTESIAN_POINT ( 'NONE',  ( 0.1092565886968784317, 0.3103822814773909977, 43.12345370280014833 ) ) ;
#5994 = EDGE_CURVE ( 'NONE', #35714, #10097, #10474, .T. ) ;
#5995 = CIRCLE ( 'NONE', #41087, 48.09070567114147110 ) ;
#5996 = FACE_BOUND ( 'NONE', #46835, .T. ) ;
#5997 = EDGE_LOOP ( 'NONE', ( #8432, #36468, #1496, #44361, #29422 ) ) ;
#5998 = ORIENTED_EDGE ( 'NONE', *, *, #46695, .T. ) ;
#5999 = CARTESIAN_POINT ( 'NONE',  ( 0.6009453534118440743, -18.81239552213013511, 44.27682103112798728 ) ) ;
#6000 = AXIS2_PLACEMENT_3D ( 'NONE', #12570, #22266, #56373 ) ;
#6001 = CARTESIAN_POINT ( 'NONE',  ( 0.8554163680231708922, 16.00619315955180610, 44.10223637924653417 ) ) ;
#6002 = LINE ( 'NONE', #12300, #12269 ) ;
#6003 = CARTESIAN_POINT ( 'NONE',  ( 4.303969348037246512, 36.81598326424549583, 30.97035057417673443 ) ) ;
#6004 = EDGE_CURVE ( 'NONE', #2143, #26111, #19467, .T. ) ;
#6005 = B_SPLINE_CURVE_WITH_KNOTS ( 'NONE', 3,
 ( #1069, #53376, #38705, #20205 ),
 .UNSPECIFIED., .F., .F.,
 ( 4, 4 ),
 ( 0.000000000000000000, 0.004048833967417084755 ),
 .UNSPECIFIED. ) ;
#6006 = ORIENTED_EDGE ( 'NONE', *, *, #53242, .T. ) ;
#6007 = CARTESIAN_POINT ( 'NONE',  ( 0.6031356219577718170, -12.36679943215693456, 46.49081620741434051 ) ) ;
#6008 = CARTESIAN_POINT ( 'NONE',  ( 4.975801465491694664, -3.702618843597810905, 47.76942479135478692 ) ) ;
#6009 = EDGE_CURVE ( 'NONE', #694, #41370, #48628, .T. ) ;
#6010 = CARTESIAN_POINT ( 'NONE',  ( 5.880360259849752858, 43.00389496650585386, 21.25991003419967740 ) ) ;
#6011 = CARTESIAN_POINT ( 'NONE',  ( 3.238931869106853600, -31.66562935062918527, -29.07925862215120461 ) ) ;
#6012 = ORIENTED_EDGE ( 'NONE', *, *, #44282, .F. ) ;
#6013 = CARTESIAN_POINT ( 'NONE',  ( 2.009741617377216460, -42.92652007869518371, -9.839611351899232972 ) ) ;
#6014 = CARTESIAN_POINT ( 'NONE',  ( 2.282816707992305627, 45.63374358165494726, 11.13815124388837319 ) ) ;
#6015 = CARTESIAN_POINT ( 'NONE',  ( 4.956653778116966613, 0.000000000000000000, 0.000000000000000000 ) ) ;
#6016 = CARTESIAN_POINT ( 'NONE',  ( 4.956445790443988031, 0.000000000000000000, 0.000000000000000000 ) ) ;
#6017 = EDGE_LOOP ( 'NONE', ( #27373, #8176, #15895, #881 ) ) ;
#6018 = ORIENTED_EDGE ( 'NONE', *, *, #56776, .T. ) ;
#6019 = DIRECTION ( 'NONE',  ( 0.07906939808003035641, -0.9635513351855560238, 0.2555716235214582910 ) ) ;
#6020 = CARTESIAN_POINT ( 'NONE',  ( 13.51351822333067965, 12.53706398592619209, -3.269553361041724978E-15 ) ) ;
#6021 = CARTESIAN_POINT ( 'NONE',  ( 0.1100053167205930771, -39.77279469894225628, 16.66867746965576558 ) ) ;
#6022 = B_SPLINE_CURVE_WITH_KNOTS ( 'NONE', 3,
 ( #15491, #43711, #33682, #39618 ),
 .UNSPECIFIED., .F., .F.,
 ( 4, 4 ),
 ( 0.000000000000000000, 0.004444103432399267896 ),
 .UNSPECIFIED. ) ;
#6023 = CARTESIAN_POINT ( 'NONE',  ( 4.967162193818130511, 13.42934394584221280, -40.93989340068594629 ) ) ;
#6024 = CARTESIAN_POINT ( 'NONE',  ( 0.1101816497532063233, 34.13008584880293483, -26.36013219694235943 ) ) ;
#6025 = CARTESIAN_POINT ( 'NONE',  ( -6.001507490154111224, -2.475062734132568831, 18.68062548815624879 ) ) ;
#6026 = CARTESIAN_POINT ( 'NONE',  ( 4.303969348037258058, 47.36875205922783749, -8.413118729223581838 ) ) ;
#6027 =( BOUNDED_SURFACE ( )  B_SPLINE_SURFACE ( 3, 1, ( 
 ( #44216, #950 ),
 ( #15998, #44523 ),
 ( #35110, #1246 ),
 ( #58252, #15383 ) ),
 .UNSPECIFIED., .F., .F., .F. ) 
 B_SPLINE_SURFACE_WITH_KNOTS ( ( 4, 4 ),
 ( 2, 2 ),
 ( 0.000000000000000000, 1.000000000000000000 ),
 ( 0.000000000000000000, 1.000000000000000000 ),
 .UNSPECIFIED. ) 
 GEOMETRIC_REPRESENTATION_ITEM ( )  RATIONAL_B_SPLINE_SURFACE ( (
 ( 1.000000000000000000, 1.000000000000000000),
 ( 0.9953485035131437453, 0.8621029689291515030),
 ( 0.9953485035131437453, 0.8621029689291515030),
 ( 1.000000000000000000, 1.000000000000000000) ) ) 
 REPRESENTATION_ITEM ( '' )  SURFACE ( )  );
#6028 = CARTESIAN_POINT ( 'NONE',  ( 2.528100132419517365, 8.550405663958636993, -41.09920122841587187 ) ) ;
#6029 = CARTESIAN_POINT ( 'NONE',  ( 5.965394784446458765, 20.35165389555754700, 2.664747781316183506 ) ) ;
#6030 = CARTESIAN_POINT ( 'NONE',  ( 0.1104177457020373010, 30.49013195371455609, -30.49705356371274334 ) ) ;
#6031 = CARTESIAN_POINT ( 'NONE',  ( 5.981074661064941900, -2.687517936920148731, 20.34795181394743935 ) ) ;
#6032 = CARTESIAN_POINT ( 'NONE',  ( 0.1149546198390367369, -6.771702484218997675, -43.60149780097516015 ) ) ;
#6033 = CARTESIAN_POINT ( 'NONE',  ( 5.896782393890504181, -13.97772289704270676, -14.46199673252280249 ) ) ;
#6034 = ADVANCED_FACE ( 'NONE', ( #49473 ), #4536, .F. ) ;
#6035 = CARTESIAN_POINT ( 'NONE',  ( 0.1064266379913944016, -11.70292640078125324, -41.50637574965944054 ) ) ;
#6036 = CARTESIAN_POINT ( 'NONE',  ( 0.6025881611877910160, -24.24244696985837066, 41.55278713510040234 ) ) ;
#6037 = CARTESIAN_POINT ( 'NONE',  ( 0.5827359174754831450, -41.65957726278053030, 23.63273677570900233 ) ) ;
#6038 = DIRECTION ( 'NONE',  ( 1.000000000000000000, 0.000000000000000000, 0.000000000000000000 ) ) ;
#6040 = EDGE_CURVE ( 'NONE', #36635, #5101, #30647, .T. ) ;
#6039 = DIRECTION ( 'NONE',  ( 0.07439287786467665975, -0.9665813013808213228, 0.2453289374370035691 ) ) ;
#6041 = CONICAL_SURFACE ( 'NONE', #56099, 42.92674063221959813, 1.485477209440487556 ) ;
#6042 = CARTESIAN_POINT ( 'NONE',  ( 0.6008122571543325074, -30.27643937426860887, 38.66383024587132411 ) ) ;
#6043 = B_SPLINE_CURVE_WITH_KNOTS ( 'NONE', 3,
 ( #1728, #34661, #49058, #54043 ),
 .UNSPECIFIED., .F., .F.,
 ( 4, 4 ),
 ( 0.000000000000000000, 0.004041751736740996012 ),
 .UNSPECIFIED. ) ;
#6044 = EDGE_CURVE ( 'NONE', #16350, #16052, #44896, .T. ) ;
#6045 = CARTESIAN_POINT ( 'NONE',  ( 0.6254311100348657337, -47.60023274471275556, -6.960804577576654495 ) ) ;
#6046 = CARTESIAN_POINT ( 'NONE',  ( 5.960221823109900008, 10.25807604135597195, 17.77840967225723645 ) ) ;
#6047 = ADVANCED_FACE ( 'NONE', ( #30360 ), #10986, .F. ) ;
#6049 = ORIENTED_EDGE ( 'NONE', *, *, #36538, .T. ) ;
#6048 = DIRECTION ( 'NONE',  ( 1.000000000000000000, 1.836970198721027962E-16, -2.033782021272921061E-31 ) ) ;
#6050 = VERTEX_POINT ( 'NONE', #7153 ) ;
#6051 = CARTESIAN_POINT ( 'NONE',  ( 0.1073791018717578927, -37.58707531572220262, 21.14095454447495115 ) ) ;
#6052 = CARTESIAN_POINT ( 'NONE',  ( 2.533389852662419894, 43.79627363621963809, -4.397379596417775538 ) ) ;
#6053 = ADVANCED_FACE ( 'NONE', ( #49787 ), #52840, .F. ) ;
#6054 = DIRECTION ( 'NONE',  ( -0.1011922191286467460, 0.2953728085273335524, -0.9500079151093926422 ) ) ;
#6055 = ORIENTED_EDGE ( 'NONE', *, *, #13563, .T. ) ;
#6056 = VERTEX_POINT ( 'NONE', #59170 ) ;
#6057 = CARTESIAN_POINT ( 'NONE',  ( 0.5839879882104920261, 5.827794150371782279E-15, 47.89596766822081264 ) ) ;
#6058 = CARTESIAN_POINT ( 'NONE',  ( 3.660176727303411148, 25.63023984566702751, -40.62966184289462745 ) ) ;
#6059 = CARTESIAN_POINT ( 'NONE',  ( 0.5832366564991500191, -41.61464700196760447, -23.71163571971566597 ) ) ;
#6060 = EDGE_LOOP ( 'NONE', ( #18084, #18729, #4539, #27927 ) ) ;
#6061 = ORIENTED_EDGE ( 'NONE', *, *, #8274, .T. ) ;
#6062 = EDGE_CURVE ( 'NONE', #14241, #8188, #44199, .T. ) ;
#6063 = CARTESIAN_POINT ( 'NONE',  ( 0.6009452777970413218, -24.43074291040877455, -41.44251326863921037 ) ) ;
#6064 = CARTESIAN_POINT ( 'NONE',  ( -4.000000000000000000, -0.7779732554280792689, -0.03354435108167819896 ) ) ;
#6065 = CARTESIAN_POINT ( 'NONE',  ( 0.6252788684277197362, -0.8874023922525490216, 49.09844038427176116 ) ) ;
#6066 = CARTESIAN_POINT ( 'NONE',  ( 0.8753041380234530822, 49.05142151719380195, 2.257515230415335417 ) ) ;
#6067 = CARTESIAN_POINT ( 'NONE',  ( 0.9769922540276041456, -40.97853790617248393, -8.780147274306424166 ) ) ;
#6068 = B_SPLINE_CURVE_WITH_KNOTS ( 'NONE', 3,
 ( #34915, #7284, #25484, #11719 ),
 .UNSPECIFIED., .F., .F.,
 ( 4, 4 ),
 ( 0.000000000000000000, 0.005004948556313800964 ),
 .UNSPECIFIED. ) ;
#6069 = CARTESIAN_POINT ( 'NONE',  ( 0.6000166863083090663, -13.47152005829796373, -47.22649287240509608 ) ) ;
#6070 = CARTESIAN_POINT ( 'NONE',  ( 0.8760168074886965917, 19.22870327415304814, -44.09317760313732748 ) ) ;
#6071 = VERTEX_POINT ( 'NONE', #16588 ) ;
#6072 = VERTEX_POINT ( 'NONE', #40415 ) ;
#6073 = CARTESIAN_POINT ( 'NONE',  ( 0.5980271706414734822, -19.23780022038743809, 45.18801041783234496 ) ) ;
#6074 = CARTESIAN_POINT ( 'NONE',  ( 2.301529144917015213, 44.85388898587000028, 17.18548816179638905 ) ) ;
#6075 = ORIENTED_EDGE ( 'NONE', *, *, #31773, .T. ) ;
#6076 = CARTESIAN_POINT ( 'NONE',  ( 2.526464513654346433, 20.43088802552616912, -37.81242626108676319 ) ) ;
#6077 = FACE_OUTER_BOUND ( 'NONE', #53310, .T. ) ;
#6078 = CARTESIAN_POINT ( 'NONE',  ( 5.895881250540457863, 8.462078741123386649, -18.24612027219289700 ) ) ;
#6079 = CARTESIAN_POINT ( 'NONE',  ( 0.1152809850208375564, -40.81594088468489900, -16.76318144588499592 ) ) ;
#6080 = B_SPLINE_CURVE_WITH_KNOTS ( 'NONE', 3,
 ( #30503, #39327, #1684, #11124 ),
 .UNSPECIFIED., .F., .F.,
 ( 4, 4 ),
 ( 0.000000000000000000, 0.004444878191957688657 ),
 .UNSPECIFIED. ) ;
#6081 = ORIENTED_EDGE ( 'NONE', *, *, #17734, .F. ) ;
#6082 = CARTESIAN_POINT ( 'NONE',  ( 5.860006189529234355, -45.67886430272019993, -15.48781697582095163 ) ) ;
#6083 = CARTESIAN_POINT ( 'NONE',  ( 0.6016118706126977189, -35.51781829556208692, 33.91217536973064739 ) ) ;
#6084 = CARTESIAN_POINT ( 'NONE',  ( 6.999999999999992895, 72.00000000000002842, -1.348150961071066192E-31 ) ) ;
#6085 = CIRCLE ( 'NONE', #37136, 42.08604991992415023 ) ;
#6086 = EDGE_CURVE ( 'NONE', #10506, #18533, #27848, .T. ) ;
#6087 = LINE ( 'NONE', #49333, #40486 ) ;
#6088 = VERTEX_POINT ( 'NONE', #34778 ) ;
#6089 = FACE_OUTER_BOUND ( 'NONE', #38846, .T. ) ;
#6090 = VERTEX_POINT ( 'NONE', #59479 ) ;
#6091 = CARTESIAN_POINT ( 'NONE',  ( 0.2230388203127621483, -26.84831060237819145, -33.74101226470655490 ) ) ;
#6092 = DIRECTION ( 'NONE',  ( -0.1024043820194934645, -0.9946559125373959365, -0.01315135725336883353 ) ) ;
#6093 = B_SPLINE_CURVE_WITH_KNOTS ( 'NONE', 3,
 ( #10318, #29413, #48522, #59143 ),
 .UNSPECIFIED., .F., .F.,
 ( 4, 4 ),
 ( 1.907487264466063683E-17, 0.004444306975806115029 ),
 .UNSPECIFIED. ) ;
#6094 = EDGE_LOOP ( 'NONE', ( #55324, #38272, #54863, #25909 ) ) ;
#6095 = CARTESIAN_POINT ( 'NONE',  ( 0.3622758884714600280, 39.50828911766974016, 17.25816669465007891 ) ) ;
#6096 = LINE ( 'NONE', #30234, #57643 ) ;
#6097 = PRODUCT_RELATED_PRODUCT_CATEGORY ( 'part', '', ( #34426 ) ) ;
#6098 = CARTESIAN_POINT ( 'NONE',  ( 5.960721111146673579, -20.34914600876577140, 2.685391721745692628 ) ) ;
#6099 = B_SPLINE_CURVE_WITH_KNOTS ( 'NONE', 3,
 ( #441, #9869, #23656, #61837 ),
 .UNSPECIFIED., .F., .F.,
 ( 4, 4 ),
 ( 0.000000000000000000, 0.004442905043737215703 ),
 .UNSPECIFIED. ) ;
#6100 = CARTESIAN_POINT ( 'NONE',  ( -5.995132425357893702, 18.84415457712583475, 0.008513469642873375265 ) ) ;
#6101 =( BOUNDED_SURFACE ( )  B_SPLINE_SURFACE ( 3, 1, ( 
 ( #45370, #2415 ),
 ( #16227, #50344 ),
 ( #44155, #44753 ),
 ( #20924, #35660 ) ),
 .UNSPECIFIED., .F., .F., .F. ) 
 B_SPLINE_SURFACE_WITH_KNOTS ( ( 4, 4 ),
 ( 2, 2 ),
 ( 0.000000000000000000, 1.000000000000000000 ),
 ( 0.000000000000000000, 1.000000000000000000 ),
 .UNSPECIFIED. ) 
 GEOMETRIC_REPRESENTATION_ITEM ( )  RATIONAL_B_SPLINE_SURFACE ( (
 ( 1.000000000000000000, 1.000000000000000000),
 ( 0.9729067724841187204, 0.9999501103223794596),
 ( 0.9729067724841187204, 0.9999501103223794596),
 ( 1.000000000000000000, 1.000000000000000000) ) ) 
 REPRESENTATION_ITEM ( '' )  SURFACE ( )  );
#6102 = CARTESIAN_POINT ( 'NONE',  ( 0.1158403557922069033, 33.62268606590009057, -28.57368175258040566 ) ) ;
#6103 = CARTESIAN_POINT ( 'NONE',  ( 3.390910168358336918, 22.06791622149280840, 38.04082294292292943 ) ) ;
#6104 = CARTESIAN_POINT ( 'NONE',  ( 0.2940135542859010354, -41.18723742143126287, -15.80670814186408535 ) ) ;
#6105 = CARTESIAN_POINT ( 'NONE',  ( 1.227938101723748288, 34.55893248994541267, -25.45152231597022308 ) ) ;
#6106 = ORIENTED_EDGE ( 'NONE', *, *, #9476, .F. ) ;
#6107 = CARTESIAN_POINT ( 'NONE',  ( 0.000000000000000000, 0.000000000000000000, 0.000000000000000000 ) ) ;
#6108 = DIRECTION ( 'NONE',  ( 0.000000000000000000, 0.000000000000000000, 1.000000000000000000 ) ) ;
#6109 = CARTESIAN_POINT ( 'NONE',  ( 0.5830081025819913165, 27.59732473080532245, -37.91595577174246046 ) ) ;
#6110 = VERTEX_POINT ( 'NONE', #35401 ) ;
#6111 = CARTESIAN_POINT ( 'NONE',  ( 0.8551540677456715978, -5.348818140991227210, 47.61725548905988603 ) ) ;
#6112 = CARTESIAN_POINT ( 'NONE',  ( 30.00000000000000711, 16.00000000000000000, -1.502225356622044316E-30 ) ) ;
#6113 = LINE ( 'NONE', #15556, #14850 ) ;
#6114 = CARTESIAN_POINT ( 'NONE',  ( 0.8560838555295223751, -44.60403252362528548, -14.52078223489045072 ) ) ;
#6115 = B_SPLINE_CURVE_WITH_KNOTS ( 'NONE', 3,
 ( #7330, #12384, #16769, #12085 ),
 .UNSPECIFIED., .F., .F.,
 ( 4, 4 ),
 ( 9.054276140135500350E-17, 0.005004741218457489996 ),
 .UNSPECIFIED. ) ;
#6116 = DIRECTION ( 'NONE',  ( 0.000000000000000000, 0.000000000000000000, 1.000000000000000000 ) ) ;
#6117 = CARTESIAN_POINT ( 'NONE',  ( 15.00000000000000355, 7.834225141937060168E-14, -80.00000000000001421 ) ) ;
#6119 = EDGE_CURVE ( 'NONE', #24949, #36033, #38874, .T. ) ;
#6118 = CARTESIAN_POINT ( 'NONE',  ( 0.7246131072078504376, 17.64706930304232202, 44.74808308960857062 ) ) ;
#6120 = CARTESIAN_POINT ( 'NONE',  ( 4.975801465491695552, 0.000000000000000000, 0.000000000000000000 ) ) ;
#6121 = EDGE_CURVE ( 'NONE', #40624, #26674, #35716, .T. ) ;
#6122 = CARTESIAN_POINT ( 'NONE',  ( 0.5804410086790514622, -20.23572001627558947, -42.30881098870896295 ) ) ;
#6123 = EDGE_CURVE ( 'NONE', #21383, #497, #50098, .T. ) ;
#6125 = ORIENTED_EDGE ( 'NONE', *, *, #3367, .T. ) ;
#6124 = CARTESIAN_POINT ( 'NONE',  ( -79.49999999999975842, 5.000000000000006217, -1.500000000000003109 ) ) ;
#6126 = VERTEX_POINT ( 'NONE', #45725 ) ;
#6127 = CARTESIAN_POINT ( 'NONE',  ( 0.5827359174754828119, -12.74690115177639704, 46.16863801597760641 ) ) ;
#6128 = CARTESIAN_POINT ( 'NONE',  ( 0.8560838555295214869, 21.73747136795201129, -41.56747734237908531 ) ) ;
#6129 = ADVANCED_FACE ( 'NONE', ( #12517 ), #56146, .F. ) ;
#6130 = CARTESIAN_POINT ( 'NONE',  ( 0.1103744047535531458, 16.46720136312925220, 39.85659247569267194 ) ) ;
#6131 = CARTESIAN_POINT ( 'NONE',  ( 1.227938101723756947, -25.45152231597080927, 34.55893248994497924 ) ) ;
#6132 = FACE_OUTER_BOUND ( 'NONE', #2777, .T. ) ;
#6133 = CARTESIAN_POINT ( 'NONE',  ( 0.8760168074886960365, -47.80016357497252955, 5.394043284318696507 ) ) ;
#6134 = VECTOR ( 'NONE', #37824, 1000.000000000000114 ) ;
#6135 = AXIS2_PLACEMENT_3D ( 'NONE', #35539, #54601, #49302 ) ;
#6136 = ORIENTED_EDGE ( 'NONE', *, *, #51257, .T. ) ;
#6137 = VERTEX_POINT ( 'NONE', #22824 ) ;
#6138 = CARTESIAN_POINT ( 'NONE',  ( 0.6064515330803585957, -38.25723792261539558, 27.12412362767662799 ) ) ;
#6139 = EDGE_CURVE ( 'NONE', #9802, #4518, #46962, .T. ) ;
#6140 = CARTESIAN_POINT ( 'NONE',  ( -6.077587904424778920, -11.01164173315302008, 15.79682777441765751 ) ) ;
#6141 = CARTESIAN_POINT ( 'NONE',  ( 0.6008123274975391004, 37.10904484800355618, 32.16322965168950532 ) ) ;
#6142 = VERTEX_POINT ( 'NONE', #18133 ) ;
#6143 = EDGE_CURVE ( 'NONE', #58875, #58301, #23234, .T. ) ;
#6144 = CARTESIAN_POINT ( 'NONE',  ( 5.959547316686252039, -0.003562808152765507049, -20.52562247508876681 ) ) ;
#6145 = ORIENTED_EDGE ( 'NONE', *, *, #28499, .T. ) ;
#6146 = CARTESIAN_POINT ( 'NONE',  ( 4.549368137175248350, 0.000000000000000000, 0.000000000000000000 ) ) ;
#6147 = EDGE_LOOP ( 'NONE', ( #47093, #8250, #48798, #1356 ) ) ;
#6148 = CARTESIAN_POINT ( 'NONE',  ( 4.962356264823608143, 17.31942680647409460, 38.35717733303029320 ) ) ;
#6149 = CARTESIAN_POINT ( 'NONE',  ( 0.5807400328401574052, 0.5448834511096651845, -47.89582301953902999 ) ) ;
#6150 = EDGE_LOOP ( 'NONE', ( #35718, #16587, #20888, #785 ) ) ;
#6151 = CARTESIAN_POINT ( 'NONE',  ( 6.999999999999995559, 56.56854249492450037, -56.56854249492312192 ) ) ;
#6152 = CARTESIAN_POINT ( 'NONE',  ( 4.956653778116966613, 0.000000000000000000, 0.000000000000000000 ) ) ;
#6153 = CARTESIAN_POINT ( 'NONE',  ( 0.5997462898726536595, -48.63480578518795738, -6.797594896826151256 ) ) ;
#6154 = LINE ( 'NONE', #43824, #49365 ) ;
#6155 = ORIENTED_EDGE ( 'NONE', *, *, #90, .F. ) ;
#6156 = B_SPLINE_CURVE_WITH_KNOTS ( 'NONE', 3,
 ( #38992, #57123, #58047, #14255 ),
 .UNSPECIFIED., .F., .F.,
 ( 4, 4 ),
 ( 4.848699518061080308E-18, 0.004050076154993002484 ),
 .UNSPECIFIED. ) ;
#6157 = CARTESIAN_POINT ( 'NONE',  ( -6.063463321072276813, 9.969191071288641126, -16.47530521306384088 ) ) ;
#6158 = CARTESIAN_POINT ( 'NONE',  ( 0.8744876279028263033, -45.83369275826233036, 17.59609782084381280 ) ) ;
#6159 = ORIENTED_EDGE ( 'NONE', *, *, #47421, .T. ) ;
#6160 = CARTESIAN_POINT ( 'NONE',  ( 1.091591847532193960, 40.62362772340473782, -10.31890796286426415 ) ) ;
#6161 = EDGE_CURVE ( 'NONE', #33929, #20064, #41040, .T. ) ;
#6162 = VERTEX_POINT ( 'NONE', #27520 ) ;
#6163 = CARTESIAN_POINT ( 'NONE',  ( 0.9787464366903556590, 4.018689650996690510, 41.71551421688862149 ) ) ;
#6164 = ORIENTED_EDGE ( 'NONE', *, *, #24913, .F. ) ;
#6165 = CARTESIAN_POINT ( 'NONE',  ( 4.549368137175248350, 38.40568845698250300, 19.17571786012337753 ) ) ;
#6166 = CARTESIAN_POINT ( 'NONE',  ( 4.303969348037246512, -40.54345935592760952, -25.89994482339412230 ) ) ;
#6167 = CARTESIAN_POINT ( 'NONE',  ( 1.227938101723748288, -41.66816631169199070, 10.28900963485366127 ) ) ;
#6168 = ORIENTED_EDGE ( 'NONE', *, *, #45409, .F. ) ;
#6169 = CARTESIAN_POINT ( 'NONE',  ( 0.1368894036331278208, 41.67016667612794834, -14.50718908359056947 ) ) ;
#6170 = DIRECTION ( 'NONE',  ( 0.000000000000000000, 0.000000000000000000, 1.000000000000000000 ) ) ;
#6171 = CARTESIAN_POINT ( 'NONE',  ( -2.569797478183790229, -0.4487456364279838184, 14.62602397812940502 ) ) ;
#6172 = ORIENTED_EDGE ( 'NONE', *, *, #25234, .F. ) ;
#6173 = PRESENTATION_LAYER_ASSIGNMENT (  '', '', ( #60208 ) ) ;
#6174 = VERTEX_POINT ( 'NONE', #36331 ) ;
#6175 = AXIS2_PLACEMENT_3D ( 'NONE', #12324, #26708, #31730 ) ;
#6176 = CARTESIAN_POINT ( 'NONE',  ( 4.833616638992205949, 45.44786513329597710, -8.578242093415260783 ) ) ;
#6177 = CARTESIAN_POINT ( 'NONE',  ( 4.390527457369401532, 31.33584375699295066, 30.79367195814660718 ) ) ;
#6178 = CARTESIAN_POINT ( 'NONE',  ( -6.078457390727109555, -18.90176508385434317, 3.676654423833250807 ) ) ;
#6179 = CARTESIAN_POINT ( 'NONE',  ( 0.1310142868023705109, 41.81449350725030456, -10.54463319394690224 ) ) ;
#6180 = CARTESIAN_POINT ( 'NONE',  ( 0.2885697896453104927, 29.91358794843018742, 31.05173034173381907 ) ) ;
#6181 = CARTESIAN_POINT ( 'NONE',  ( -6.010958268070873523, -2.473955915502089820, -18.68034667844851526 ) ) ;
#6182 = ORIENTED_EDGE ( 'NONE', *, *, #43419, .F. ) ;
#6183 = CARTESIAN_POINT ( 'NONE',  ( 4.960386119450144626, -40.46376651419608095, -16.64692356433961606 ) ) ;
#6184 = ORIENTED_EDGE ( 'NONE', *, *, #56927, .T. ) ;
#6185 = CARTESIAN_POINT ( 'NONE',  ( 0.5806925824938502512, 37.13995815321093374, 28.63295078613632683 ) ) ;
#6186 = CARTESIAN_POINT ( 'NONE',  ( 5.896278296736517710, 0.6775463355846830238, 20.10144051001120147 ) ) ;
#6187 = CARTESIAN_POINT ( 'NONE',  ( 4.833616638992208614, -20.86133030530261578, -41.27831852777636357 ) ) ;
#6188 = CARTESIAN_POINT ( 'NONE',  ( 1.827119703190779321, 33.38937793923687991, -27.17434071502568216 ) ) ;
#6189 =( NAMED_UNIT ( * ) SI_UNIT ( $, .STERADIAN. ) SOLID_ANGLE_UNIT ( ) );
#6190 = CARTESIAN_POINT ( 'NONE',  ( 5.981074661064941900, -19.82308078259094586, 5.320466518160593239 ) ) ;
#6191 = CARTESIAN_POINT ( 'NONE',  ( 0.9747592971366227932, -39.51726118357604634, 16.71904224817891915 ) ) ;
#6192 = CARTESIAN_POINT ( 'NONE',  ( -6.016104459813374383, 18.20253432612973299, -4.871830707672867078 ) ) ;
#6193 = EDGE_CURVE ( 'NONE', #46370, #10577, #53802, .T. ) ;
#6194 = CARTESIAN_POINT ( 'NONE',  ( 0.9754292580325141238, 10.28092798196799507, -40.62794588375828653 ) ) ;
#6195 = CARTESIAN_POINT ( 'NONE',  ( 2.282816707992309624, -37.96808949008106282, 27.65720786487965910 ) ) ;
#6196 = FACE_OUTER_BOUND ( 'NONE', #10720, .T. ) ;
#6197 = EDGE_CURVE ( 'NONE', #50125, #14535, #38901, .T. ) ;
#6198 = CARTESIAN_POINT ( 'NONE',  ( 0.5819845901640494645, -23.55368560422314417, -41.70428411658551227 ) ) ;
#6199 = CARTESIAN_POINT ( 'NONE',  ( 0.7242486021783856032, 27.41642097787600463, 40.73513622338652596 ) ) ;
#6200 = CARTESIAN_POINT ( 'NONE',  ( 0.8560838555295158248, -42.27062166135473120, 20.33635607586422012 ) ) ;
#6201 = CARTESIAN_POINT ( 'NONE',  ( 0.8560838555295223751, -39.18289055412714106, -25.78902716088815694 ) ) ;
#6202 = ORIENTED_EDGE ( 'NONE', *, *, #50208, .F. ) ;
#6203 = SURFACE_STYLE_FILL_AREA ( #19735 ) ;
#6204 = ADVANCED_FACE ( 'NONE', ( #7787 ), #19767, .F. ) ;
#6205 = CARTESIAN_POINT ( 'NONE',  ( 0.09136607875274982415, 0.000000000000000000, 0.000000000000000000 ) ) ;
#6206 = CARTESIAN_POINT ( 'NONE',  ( -6.017396004339687465, -4.875835690939052114, -18.20140164570674202 ) ) ;
#6207 = CARTESIAN_POINT ( 'NONE',  ( 5.838029081930955932, -32.82243551873101950, -33.96693664096990517 ) ) ;
#6208 = CARTESIAN_POINT ( 'NONE',  ( 0.1129192098497455998, 4.719118110135312349, -43.87119455916086963 ) ) ;
#6209 = ORIENTED_EDGE ( 'NONE', *, *, #32067, .F. ) ;
#6210 = EDGE_CURVE ( 'NONE', #50555, #49238, #25827, .T. ) ;
#6211 = CARTESIAN_POINT ( 'NONE',  ( 2.281351352603290472, -30.23585463601401813, 37.24546109640808567 ) ) ;
#6212 = CARTESIAN_POINT ( 'NONE',  ( 0.6008122571543325074, 27.73703307328602108, -40.52420939089070373 ) ) ;
#6213 = VECTOR ( 'NONE', #23881, 1000.000000000000114 ) ;
#6214 = CARTESIAN_POINT ( 'NONE',  ( 0.6029442701453591180, -13.88890752606295464, 47.10247841558604165 ) ) ;
#6215 = CIRCLE ( 'NONE', #55238, 9.500000000000000000 ) ;
#6216 = ORIENTED_EDGE ( 'NONE', *, *, #15658, .T. ) ;
#6217 = CARTESIAN_POINT ( 'NONE',  ( 5.895881250540457863, 12.98890680526542951, 15.35630103939195301 ) ) ;
#6218 = CARTESIAN_POINT ( 'NONE',  ( 1.830465331921977246, 8.594330631025679068, 43.20316582014567786 ) ) ;
#6219 = ORIENTED_EDGE ( 'NONE', *, *, #33268, .F. ) ;
#6220 = CARTESIAN_POINT ( 'NONE',  ( 4.958415959904820092, -26.53498967168953371, 36.86595010230943359 ) ) ;
#6221 = VERTEX_POINT ( 'NONE', #32233 ) ;
#6222 = CARTESIAN_POINT ( 'NONE',  ( 0.5988103622719990193, -46.62176011478430127, 11.86435782853352805 ) ) ;
#6223 = EDGE_LOOP ( 'NONE', ( #51618, #46364 ) ) ;
#6224 = CARTESIAN_POINT ( 'NONE',  ( 4.834790513006553603, 46.80118606150055882, 6.499101796493775396 ) ) ;
#6225 = DIRECTION ( 'NONE',  ( -1.000000000000000000, -3.135800716341471541E-16, -1.298891185607920445E-16 ) ) ;
#6226 = ORIENTED_EDGE ( 'NONE', *, *, #8217, .T. ) ;
#6227 = ORIENTED_EDGE ( 'NONE', *, *, #58180, .T. ) ;
#6228 = CARTESIAN_POINT ( 'NONE',  ( 0.9780106845699483298, 20.41499038561383017, -36.59999199468128239 ) ) ;
#6229 = CARTESIAN_POINT ( 'NONE',  ( -6.078726893082806448, 17.84743921491362073, -7.229312189875575889 ) ) ;
#6230 = B_SPLINE_CURVE_WITH_KNOTS ( 'NONE', 3,
 ( #56521, #21792, #60912, #17100 ),
 .UNSPECIFIED., .F., .F.,
 ( 4, 4 ),
 ( 5.818439421673295599E-18, 0.004042984057420976295 ),
 .UNSPECIFIED. ) ;
#6231 = ADVANCED_FACE ( 'NONE', ( #55091 ), #26155, .F. ) ;
#6232 = ORIENTED_EDGE ( 'NONE', *, *, #4432, .T. ) ;
#6233 = FACE_OUTER_BOUND ( 'NONE', #24152, .T. ) ;
#6234 = CARTESIAN_POINT ( 'NONE',  ( 1.199999999999992628, 8.239576745513314221E-16, 6.728125000000023448 ) ) ;
#6235 = CARTESIAN_POINT ( 'NONE',  ( 0.5835226383429288344, 32.47062518953475774, -33.83638536171847733 ) ) ;
#6236 = CARTESIAN_POINT ( 'NONE',  ( 0.6027935024548037868, 44.37842839362948411, 18.57106801640314586 ) ) ;
#6237 = ORIENTED_EDGE ( 'NONE', *, *, #28089, .T. ) ;
#6238 = CARTESIAN_POINT ( 'NONE',  ( -4.482327238996802521, -10.94462134745707793, 2.754595595722048466E-16 ) ) ;
#6239 = CARTESIAN_POINT ( 'NONE',  ( 2.648799415243696664, -38.45353011080844396, -30.42767630475167095 ) ) ;
#6240 = EDGE_LOOP ( 'NONE', ( #6155, #7105, #23019, #36101 ) ) ;
#6241 = CARTESIAN_POINT ( 'NONE',  ( 0.6067099128993237445, 47.38952184036240567, -6.954009037735675136 ) ) ;
#6242 = ORIENTED_EDGE ( 'NONE', *, *, #24454, .F. ) ;
#6243 = CARTESIAN_POINT ( 'NONE',  ( 0.8560838555295158248, 31.94705745926175311, 34.34761059777461867 ) ) ;
#6244 = CARTESIAN_POINT ( 'NONE',  ( 0.1149546198390367369, 25.01907401799166308, 36.34546051854996307 ) ) ;
#6245 = VERTEX_POINT ( 'NONE', #50398 ) ;
#6246 = CARTESIAN_POINT ( 'NONE',  ( -6.016761891674564211, -4.873659902332494909, 18.20201388312094082 ) ) ;
#6247 = CARTESIAN_POINT ( 'NONE',  ( -6.078075953587585900, 5.473785299353282063, 18.46165888385222331 ) ) ;
#6248 = FACE_OUTER_BOUND ( 'NONE', #1936, .T. ) ;
#6249 = CARTESIAN_POINT ( 'NONE',  ( -17.97369999999976642, -12.32233744059949210, -2.099999999999997424 ) ) ;
#6250 = VERTEX_POINT ( 'NONE', #26590 ) ;
#6251 = CARTESIAN_POINT ( 'NONE',  ( 0.5998501479064699549, 17.92509395669108585, -44.64337787626229925 ) ) ;
#6252 = CARTESIAN_POINT ( 'NONE',  ( 0.5807400328401574052, -34.25275203086258813, 33.48217046439099676 ) ) ;
#6253 = CARTESIAN_POINT ( 'NONE',  ( 4.975610109902397937, 48.90928568712960356, 0.5754830253899292369 ) ) ;
#6254 = AXIS2_PLACEMENT_3D ( 'NONE', #32974, #28550, #42678 ) ;
#6255 = FILL_AREA_STYLE ('',( #7199 ) ) ;
#6256 = CARTESIAN_POINT ( 'NONE',  ( 0.8753041380234465318, 46.31375555491744223, 16.31485134079786192 ) ) ;
#6257 = DIRECTION ( 'NONE',  ( 1.000000000000000000, 0.000000000000000000, 0.000000000000000000 ) ) ;
#6258 = EDGE_CURVE ( 'NONE', #29973, #45131, #5993, .T. ) ;
#6259 = CARTESIAN_POINT ( 'NONE',  ( 58.00000000000000000, 15.50000000000000888, 1.598617315530390651E-15 ) ) ;
#6260 = B_SPLINE_CURVE_WITH_KNOTS ( 'NONE', 3,
 ( #4966, #48220, #33824, #10009, #581, #28477, #47601, #57271, #43226, #24403, #262, #42606, #4644, #9372, #15026, #28794, #43856, #19410, #52904 ),
 .UNSPECIFIED., .F., .F.,
 ( 4, 3, 3, 3, 3, 3, 4 ),
 ( 3.469446951953614189E-18, 0.0002724573126191867601, 0.0004086839781548543861, 0.0005449106435901867988, 0.0006811373090491506990, 0.0008459866663933788070, 0.001010840725717216185 ),
 .UNSPECIFIED. ) ;
#6261 = CARTESIAN_POINT ( 'NONE',  ( 4.975610109902397937, 19.27143522741655701, 44.95621415792550124 ) ) ;
#6262 = EDGE_CURVE ( 'NONE', #29773, #12923, #17251, .T. ) ;
#6263 = CARTESIAN_POINT ( 'NONE',  ( 2.301430502907647391, -17.18551536142221181, -44.85388302506900260 ) ) ;
#6264 = CARTESIAN_POINT ( 'NONE',  ( -6.015611763856276717, 9.427003116184401676, -16.31561949997065852 ) ) ;
#6265 = CARTESIAN_POINT ( 'NONE',  ( 3.678748215320120529, -44.67004451351987626, 20.07983907952543490 ) ) ;
#6266 = CIRCLE ( 'NONE', #17360, 10.00000000000000711 ) ;
#6267 = DIRECTION ( 'NONE',  ( 0.09835009131224567436, 0.6981896185982624514, 0.7091251765524093642 ) ) ;
#6268 = B_SPLINE_CURVE_WITH_KNOTS ( 'NONE', 3,
 ( #12091, #27392, #50272, #3880 ),
 .UNSPECIFIED., .F., .F.,
 ( 4, 4 ),
 ( 0.000000000000000000, 0.004444103432399266161 ),
 .UNSPECIFIED. ) ;
#6269 = EDGE_CURVE ( 'NONE', #44917, #41784, #52278, .T. ) ;
#6270 =( BOUNDED_SURFACE ( )  B_SPLINE_SURFACE ( 3, 1, ( 
 ( #15236, #58723 ),
 ( #53114, #52810 ),
 ( #15850, #10219 ),
 ( #54027, #20246 ) ),
 .UNSPECIFIED., .F., .F., .F. ) 
 B_SPLINE_SURFACE_WITH_KNOTS ( ( 4, 4 ),
 ( 2, 2 ),
 ( 0.000000000000000000, 1.000000000000000000 ),
 ( 0.000000000000000000, 1.000000000000000000 ),
 .UNSPECIFIED. ) 
 GEOMETRIC_REPRESENTATION_ITEM ( )  RATIONAL_B_SPLINE_SURFACE ( (
 ( 1.000000000000000000, 1.000000000000000000),
 ( 0.9953040768229013402, 0.8617119497784988535),
 ( 0.9953040768229013402, 0.8617119497784988535),
 ( 1.000000000000000000, 1.000000000000000000) ) ) 
 REPRESENTATION_ITEM ( '' )  SURFACE ( )  );
#6271 = CIRCLE ( 'NONE', #5263, 47.91270532121795611 ) ;
#6272 = B_SPLINE_CURVE_WITH_KNOTS ( 'NONE', 3,
 ( #4512, #61832, #33376, #43087 ),
 .UNSPECIFIED., .F., .F.,
 ( 4, 4 ),
 ( 0.000000000000000000, 0.005004741218457417137 ),
 .UNSPECIFIED. ) ;
#6273 = CARTESIAN_POINT ( 'NONE',  ( 4.553261556744875094, 0.000000000000000000, 0.000000000000000000 ) ) ;
#6274 = CARTESIAN_POINT ( 'NONE',  ( 0.6024113833632039894, -45.59977004659592126, 18.22643247589719095 ) ) ;
#6275 = EDGE_LOOP ( 'NONE', ( #27054, #24858, #45071, #19511 ) ) ;
#6276 = B_SPLINE_CURVE_WITH_KNOTS ( 'NONE', 3,
 ( #26521, #3013, #55626, #36876 ),
 .UNSPECIFIED., .F., .F.,
 ( 4, 4 ),
 ( 4.336808689942017736E-18, 0.004042984057420974560 ),
 .UNSPECIFIED. ) ;
#6277 = CARTESIAN_POINT ( 'NONE',  ( 4.963659409799330291, -8.262218268420191691, -43.98510776953418855 ) ) ;
#6278 = CARTESIAN_POINT ( 'NONE',  ( 4.553261556744875094, 17.98701270972463817, -40.07501640179128799 ) ) ;
#6279 = CARTESIAN_POINT ( 'NONE',  ( 5.895596859100789899, -20.11288567981415909, -0.003583743010673907416 ) ) ;
#6280 = VERTEX_POINT ( 'NONE', #53169 ) ;
#6281 = ADVANCED_FACE ( 'NONE', ( #42565 ), #27806, .F. ) ;
#6282 = CARTESIAN_POINT ( 'NONE',  ( 1.827326673878744145, 39.28486782721041237, 17.60663982372551217 ) ) ;
#6283 = FACE_BOUND ( 'NONE', #18002, .T. ) ;
#6284 = CARTESIAN_POINT ( 'NONE',  ( 4.956445790443988031, 0.000000000000000000, 0.000000000000000000 ) ) ;
#6285 =( BOUNDED_SURFACE ( )  B_SPLINE_SURFACE ( 3, 1, ( 
 ( #49557, #49250 ),
 ( #6613, #45209 ),
 ( #1016, #44902 ),
 ( #53620, #35488 ) ),
 .UNSPECIFIED., .F., .F., .F. ) 
 B_SPLINE_SURFACE_WITH_KNOTS ( ( 4, 4 ),
 ( 2, 2 ),
 ( 0.000000000000000000, 1.000000000000000000 ),
 ( 0.000000000000000000, 1.000000000000000000 ),
 .UNSPECIFIED. ) 
 GEOMETRIC_REPRESENTATION_ITEM ( )  RATIONAL_B_SPLINE_SURFACE ( (
 ( 1.000000000000000000, 1.000000000000000000),
 ( 0.9732289882329797637, 0.9999525324661233672),
 ( 0.9732289882329797637, 0.9999525324661233672),
 ( 1.000000000000000000, 1.000000000000000000) ) ) 
 REPRESENTATION_ITEM ( '' )  SURFACE ( )  );
#6286 = ORIENTED_EDGE ( 'NONE', *, *, #26117, .T. ) ;
#6287 = ORIENTED_EDGE ( 'NONE', *, *, #15288, .F. ) ;
#6288 = CARTESIAN_POINT ( 'NONE',  ( 0.6000166863083090663, 22.25084548767559767, -43.78039923061506755 ) ) ;
#6289 = ORIENTED_EDGE ( 'NONE', *, *, #21493, .F. ) ;
#6290 = LINE ( 'NONE', #53917, #14982 ) ;
#6291 = ORIENTED_EDGE ( 'NONE', *, *, #26434, .T. ) ;
#6292 = EDGE_LOOP ( 'NONE', ( #56120, #17153, #23354, #43883 ) ) ;
#6293 = CARTESIAN_POINT ( 'NONE',  ( 4.975610109902397937, 0.000000000000000000, 0.000000000000000000 ) ) ;
#6294 = ORIENTED_EDGE ( 'NONE', *, *, #58114, .T. ) ;
#6295 = CARTESIAN_POINT ( 'NONE',  ( 0.2940133293163019190, -11.77874402649793240, -42.51472378760423965 ) ) ;
#6296 = AXIS2_PLACEMENT_3D ( 'NONE', #35588, #29623, #54647 ) ;
#6297 = B_SPLINE_CURVE_WITH_KNOTS ( 'NONE', 3,
 ( #53332, #38352, #61798, #18933, #5093, #57103, #52105, #33953, #57401, #9203, #5403, #10131, #38056, #24222, #43053, #15147 ),
 .UNSPECIFIED., .F., .F.,
 ( 4, 3, 3, 3, 3, 4 ),
 ( 9.813676791237319219E-18, 0.0002732102107931898912, 0.0004098135523333789319, 0.0005464168938824946970, 0.0008195847345945537436, 0.001092771384553115890 ),
 .UNSPECIFIED. ) ;
#6298 = CARTESIAN_POINT ( 'NONE',  ( 4.962356264823608143, -38.57439820587617163, -16.83007429920747811 ) ) ;
#6299 = ORIENTED_EDGE ( 'NONE', *, *, #28873, .T. ) ;
#6300 = LINE ( 'NONE', #7240, #44785 ) ;
#6301 = CARTESIAN_POINT ( 'NONE',  ( 0.8744876279028306332, 3.827863332835647281, -48.94586308039347955 ) ) ;
#6302 = ORIENTED_EDGE ( 'NONE', *, *, #9063, .F. ) ;
#6303 = DIRECTION ( 'NONE',  ( 0.9848077530122079093, 0.1736481776669314414, -5.551115123125783935E-17 ) ) ;
#6304 = CARTESIAN_POINT ( 'NONE',  ( 5.896278296736517710, -7.233829247026186238, -18.76695750619295922 ) ) ;
#6305 = CARTESIAN_POINT ( 'NONE',  ( 5.896782393890504181, -4.656380635072850716, 19.56640504178861306 ) ) ;
#6306 = CARTESIAN_POINT ( 'NONE',  ( 0.9787464366903567692, 35.96771654815888297, 21.50947138359660116 ) ) ;
#6307 = ORIENTED_EDGE ( 'NONE', *, *, #14591, .T. ) ;
#6308 = EDGE_CURVE ( 'NONE', #5144, #46408, #24667, .T. ) ;
#6309 = B_SPLINE_CURVE_WITH_KNOTS ( 'NONE', 3,
 ( #36127, #10759, #3489, #22940 ),
 .UNSPECIFIED., .F., .F.,
 ( 4, 4 ),
 ( 0.000000000000000000, 0.005004741218457367698 ),
 .UNSPECIFIED. ) ;
#6310 = AXIS2_PLACEMENT_3D ( 'NONE', #31501, #7053, #60603 ) ;
#6311 = ORIENTED_EDGE ( 'NONE', *, *, #28635, .F. ) ;
#6312 = CARTESIAN_POINT ( 'NONE',  ( 0.7762777257811898091, -37.45705273430986892, -29.86325207275917393 ) ) ;
#6313 = EDGE_CURVE ( 'NONE', #28193, #57844, #29365, .T. ) ;
#6314 = CARTESIAN_POINT ( 'NONE',  ( 0.5998501479064699549, 5.759754759340783181, -47.76154736470751772 ) ) ;
#6315 = ORIENTED_EDGE ( 'NONE', *, *, #24116, .T. ) ;
#6316 = CARTESIAN_POINT ( 'NONE',  ( 5.974727161628367256, -17.78288073588495877, -10.24903993265002633 ) ) ;
#6317 = CARTESIAN_POINT ( 'NONE',  ( -31.75000000000000000, 0.000000000000000000, 0.000000000000000000 ) ) ;
#6318 = ADVANCED_FACE ( 'NONE', ( #52547 ), #43011, .F. ) ;
#6319 = CARTESIAN_POINT ( 'NONE',  ( 0.8744876279028263033, 46.30617036199606673, 16.31222353896886545 ) ) ;
#6320 = FACE_OUTER_BOUND ( 'NONE', #15017, .T. ) ;
#6321 = ORIENTED_EDGE ( 'NONE', *, *, #58986, .F. ) ;
#6322 = EDGE_LOOP ( 'NONE', ( #24751, #1008, #16187, #49375 ) ) ;
#6323 = CARTESIAN_POINT ( 'NONE',  ( 0.9722240750034578660, 39.41582016107722097, -16.95645446544443047 ) ) ;
#6324 = CARTESIAN_POINT ( 'NONE',  ( 0.1097557419366048670, 34.34829179474800043, 26.07515889977830170 ) ) ;
#6325 = CARTESIAN_POINT ( 'NONE',  ( 0.7048096507298635682, -19.18768066167092456, -44.11842270945967215 ) ) ;
#6326 = CARTESIAN_POINT ( 'NONE',  ( 0.7948878604505665857, -49.09120187693520876, 0.8674938480527389917 ) ) ;
#6327 = LINE ( 'NONE', #44608, #13607 ) ;
#6328 = CARTESIAN_POINT ( 'NONE',  ( -6.078726893082806448, -6.653559303940109082, -18.06998035022927596 ) ) ;
#6329 = CARTESIAN_POINT ( 'NONE',  ( 2.533389852662419894, -14.03271582234461334, -41.71970060274805547 ) ) ;
#6330 = EDGE_CURVE ( 'NONE', #3214, #55302, #35889, .T. ) ;
#6331 = FACE_OUTER_BOUND ( 'NONE', #8732, .T. ) ;
#6332 = CARTESIAN_POINT ( 'NONE',  ( 5.958863334805807099, -14.51469124124469978, -14.51296551801798174 ) ) ;
#6333 = EDGE_CURVE ( 'NONE', #2450, #30431, #28431, .T. ) ;
#6334 = CARTESIAN_POINT ( 'NONE',  ( 0.1135584504625008206, -6.615454642350983683, -43.62554082198006000 ) ) ;
#6335 = LINE ( 'NONE', #54266, #37437 ) ;
#6336 = CARTESIAN_POINT ( 'NONE',  ( 4.956653778116970166, -27.17045123668450657, -39.67974989265067620 ) ) ;
#6337 = B_SPLINE_CURVE_WITH_KNOTS ( 'NONE', 3,
 ( #58639, #6011, #10132, #15452 ),
 .UNSPECIFIED., .F., .F.,
 ( 4, 4 ),
 ( 6.992893892674702526E-18, 0.004566006591234645501 ),
 .UNSPECIFIED. ) ;
#6338 = CARTESIAN_POINT ( 'NONE',  ( 5.896278296736517710, 14.92041660055668295, -13.48733287496887634 ) ) ;
#6339 = CIRCLE ( 'NONE', #58401, 43.08621763946400307 ) ;
#6340 = CARTESIAN_POINT ( 'NONE',  ( 1.321505333908968627, -3.855830693249186147, -0.03421028094655685636 ) ) ;
#6341 = CARTESIAN_POINT ( 'NONE',  ( 0.5806925824938494740, -19.24316026636509136, 42.76591101925167493 ) ) ;
#6342 = CONTEXT_DEPENDENT_SHAPE_REPRESENTATION ( #12393, #4796 ) ;
#6343 = CARTESIAN_POINT ( 'NONE',  ( 0.3622758884714600280, 10.35929834645864389, 41.85013935980105515 ) ) ;
#6344 = ADVANCED_FACE ( 'NONE', ( #25593 ), #6541, .F. ) ;
#6345 = B_SPLINE_CURVE_WITH_KNOTS ( 'NONE', 3,
 ( #56967, #47904, #42911, #18465 ),
 .UNSPECIFIED., .F., .F.,
 ( 4, 4 ),
 ( 2.033478910116247305E-17, 0.004444306975806115029 ),
 .UNSPECIFIED. ) ;
#6346 = DIRECTION ( 'NONE',  ( 0.000000000000000000, 0.000000000000000000, -1.000000000000000000 ) ) ;
#6347 = DIRECTION ( 'NONE',  ( 1.000000000000000000, -0.000000000000000000, -0.000000000000000000 ) ) ;
#6348 = CARTESIAN_POINT ( 'NONE',  ( 0.6027444965799114707, 49.01471672440227678, -3.015967558519589531 ) ) ;
#6350 = VERTEX_POINT ( 'NONE', #16511 ) ;
#6349 = CARTESIAN_POINT ( 'NONE',  ( 0.5800708119828335008, 41.16171018093194078, -24.48933355903722386 ) ) ;
#6351 = ORIENTED_EDGE ( 'NONE', *, *, #50228, .F. ) ;
#6352 = CARTESIAN_POINT ( 'NONE',  ( 1.231276596079881047, 36.49189576017899839, -20.63051901543672884 ) ) ;
#6353 = CARTESIAN_POINT ( 'NONE',  ( 0.8744876279028306332, 49.04340454744548339, 2.257104511336577968 ) ) ;
#6354 = CARTESIAN_POINT ( 'NONE',  ( 0.1158516988532803105, 41.89178036391317761, 13.85716048743228335 ) ) ;
#6355 = ORIENTED_EDGE ( 'NONE', *, *, #14726, .F. ) ;
#6356 = EDGE_CURVE ( 'NONE', #9789, #59695, #14849, .T. ) ;
#6357 = ORIENTED_EDGE ( 'NONE', *, *, #37311, .T. ) ;
#6358 = CARTESIAN_POINT ( 'NONE',  ( 0.1081432562775998113, -11.56998286599564807, 41.54352569227142311 ) ) ;
#6360 = CARTESIAN_POINT ( 'NONE',  ( 0.5980894510889457338, -28.72954109785633037, 38.59343625445397663 ) ) ;
#6359 = AXIS2_PLACEMENT_3D ( 'NONE', #20298, #5542, #24682 ) ;
#6361 = CARTESIAN_POINT ( 'NONE',  ( 0.1100053167205930632, -37.25683392728348053, 21.71746606919042932 ) ) ;
#6362 = ORIENTED_EDGE ( 'NONE', *, *, #31765, .F. ) ;
#6363 = EDGE_LOOP ( 'NONE', ( #27773, #60605, #46866, #11752 ) ) ;
#6364 = CARTESIAN_POINT ( 'NONE',  ( 0.5998501479064699549, -24.50586714782575726, -41.39809967730479201 ) ) ;
#6365 =( BOUNDED_CURVE ( )  B_SPLINE_CURVE ( 3, ( #9106, #3467, #14445, #61399 ),
 .UNSPECIFIED., .F., .F. ) 
 B_SPLINE_CURVE_WITH_KNOTS ( ( 4, 4 ),
 ( 3.141592653589793116, 6.283185307179586232 ),
 .UNSPECIFIED. ) 
 CURVE ( )  GEOMETRIC_REPRESENTATION_ITEM ( )  RATIONAL_B_SPLINE_CURVE ( ( 1.000000000000000000, 0.3333333333333333703, 0.3333333333333333703, 1.000000000000000000 ) ) 
 REPRESENTATION_ITEM ( '' )  );
#6366 = CARTESIAN_POINT ( 'NONE',  ( 0.5830081025819940921, -38.81694609819070507, -26.31495259339077109 ) ) ;
#6367 = CARTESIAN_POINT ( 'NONE',  ( 3.050102900204245682, -10.77143531111902597, 42.65444209594632952 ) ) ;
#6368 = ORIENTED_EDGE ( 'NONE', *, *, #3335, .F. ) ;
#6369 = CARTESIAN_POINT ( 'NONE',  ( 0.1119899015040013157, -1.975119189439954681, 44.08015667372350777 ) ) ;
#6370 = CARTESIAN_POINT ( 'NONE',  ( -2.601141883200662974, -12.22474371604796417, -8.564523836520885780 ) ) ;
#6371 = DIRECTION ( 'NONE',  ( -0.1024043820194934645, 0.3684880688409138960, 0.9239750460186137992 ) ) ;
#6372 = ORIENTED_EDGE ( 'NONE', *, *, #7058, .F. ) ;
#6373 = EDGE_LOOP ( 'NONE', ( #10883, #4933, #41070, #51838 ) ) ;
#6374 = CARTESIAN_POINT ( 'NONE',  ( 0.6254311100348631802, 44.70341307176154544, -17.77188277739572797 ) ) ;
#6375 = ORIENTED_EDGE ( 'NONE', *, *, #4893, .F. ) ;
#6376 = CARTESIAN_POINT ( 'NONE',  ( 0.5827359174754830340, 44.38786494726119969, -17.99288944686844616 ) ) ;
#6377 = CARTESIAN_POINT ( 'NONE',  ( 4.956445790443995136, 19.33052208089553758, 42.94029536716820417 ) ) ;
#6378 = CARTESIAN_POINT ( 'NONE',  ( 0.7242486021783836048, -8.644155275603129240, 48.33518430651980680 ) ) ;
#6379 = EDGE_CURVE ( 'NONE', #15970, #33742, #7446, .T. ) ;
#6380 = AXIS2_PLACEMENT_3D ( 'NONE', #36457, #27343, #36768 ) ;
#6381 = VERTEX_POINT ( 'NONE', #30911 ) ;
#6382 = CARTESIAN_POINT ( 'NONE',  ( 4.303969348037246512, -45.86537346639047996, -14.52400616872417061 ) ) ;
#6383 = CARTESIAN_POINT ( 'NONE',  ( 0.6017666602106489515, 18.73203020817298636, 44.31084100715259666 ) ) ;
#6384 = EDGE_CURVE ( 'NONE', #21245, #34877, #49845, .T. ) ;
#6385 = CARTESIAN_POINT ( 'NONE',  ( 4.549368137175248350, -28.14399996863474129, -32.41327393324131378 ) ) ;
#6386 = FACE_OUTER_BOUND ( 'NONE', #22664, .T. ) ;
#6387 = ORIENTED_EDGE ( 'NONE', *, *, #37375, .F. ) ;
#6388 = CARTESIAN_POINT ( 'NONE',  ( 0.5809828226811617480, -46.40184912890847357, 11.86925843957150128 ) ) ;
#6389 = CARTESIAN_POINT ( 'NONE',  ( 0.5806925824938511393, 5.237374507879287044, 46.60249210726590263 ) ) ;
#6391 = ORIENTED_EDGE ( 'NONE', *, *, #26437, .F. ) ;
#6390 = EDGE_CURVE ( 'NONE', #59975, #5739, #40343, .T. ) ;
#6392 = CARTESIAN_POINT ( 'NONE',  ( 0.7954190325252773475, 42.08256085583540340, 23.29293489839749753 ) ) ;
#6393 = CARTESIAN_POINT ( 'NONE',  ( 0.1158403557922069033, 9.781626696134630095, 43.02627204814850614 ) ) ;
#6394 = EDGE_CURVE ( 'NONE', #57497, #1853, #26822, .T. ) ;
#6395 = ORIENTED_EDGE ( 'NONE', *, *, #59282, .F. ) ;
#6396 = CARTESIAN_POINT ( 'NONE',  ( -90.00000000000000000, 6.873330160214519262E-16, 5.612499999999999822 ) ) ;
#6397 = EDGE_CURVE ( 'NONE', #30001, #15923, #26893, .T. ) ;
#6398 = DIRECTION ( 'NONE',  ( 0.000000000000000000, 0.000000000000000000, -1.000000000000000000 ) ) ;
#6399 = CARTESIAN_POINT ( 'NONE',  ( 1.088313998177381947, -39.93881167962110368, 15.69908095455140362 ) ) ;
#6400 = VECTOR ( 'NONE', #40749, 1000.000000000000114 ) ;
#6401 = LINE ( 'NONE', #48736, #37492 ) ;
#6402 = CARTESIAN_POINT ( 'NONE',  ( 0.2285344041767094769, -31.15968535845325604, 31.23419886370790266 ) ) ;
#6403 = EDGE_CURVE ( 'NONE', #59315, #30302, #39672, .T. ) ;
#6404 = CARTESIAN_POINT ( 'NONE',  ( 2.301529144917015213, -1.287519423136938679, -48.01619158420458433 ) ) ;
#6405 = CARTESIAN_POINT ( 'NONE',  ( 39.99999999999998579, 72.00000000000004263, -4.333342374871279794E-31 ) ) ;
#6406 = CARTESIAN_POINT ( 'NONE',  ( 0.9754292589017190540, 29.55040399309918087, 29.71701685465599141 ) ) ;
#6407 = CARTESIAN_POINT ( 'NONE',  ( 0.9752570700956805227, 39.72995844664877296, -16.20701641182873587 ) ) ;
#6408 = EDGE_CURVE ( 'NONE', #3997, #22756, #37458, .T. ) ;
#6409 = CARTESIAN_POINT ( 'NONE',  ( 3.238931869106854933, -40.38337734129193990, -14.74782013370832878 ) ) ;
#6410 = CARTESIAN_POINT ( 'NONE',  ( 0.9784957157296353403, 15.27927399397425567, 39.02405467412931017 ) ) ;
#6411 = ORIENTED_EDGE ( 'NONE', *, *, #40389, .T. ) ;
#6412 = CARTESIAN_POINT ( 'NONE',  ( -16.58512404506131688, -12.39995699298779286, 1.581313323489840661 ) ) ;
#6413 = FACE_OUTER_BOUND ( 'NONE', #59888, .T. ) ;
#6414 = DIRECTION ( 'NONE',  ( 1.000000000000000000, 1.836909530733573776E-16, 0.000000000000000000 ) ) ;
#6415 = CARTESIAN_POINT ( 'NONE',  ( 1.827119703190779765, -39.28489939038900047, 17.60659059422107475 ) ) ;
#6416 = B_SPLINE_CURVE_WITH_KNOTS ( 'NONE', 3,
 ( #48052, #19864, #9831, #20463, #6323, #30157 ),
 .UNSPECIFIED., .F., .F.,
 ( 4, 2, 4 ),
 ( 9.948699630566629781E-18, 0.0002291978881530141272, 0.0004583957763060183340 ),
 .UNSPECIFIED. ) ;
#6417 = DIRECTION ( 'NONE',  ( 0.09835009131224552170, -0.1375559175655225452, -0.9855991218957026456 ) ) ;
#6418 = CARTESIAN_POINT ( 'NONE',  ( 0.2230388203127603441, -0.7599700551097323675, -43.11276071378621566 ) ) ;
#6419 = DIRECTION ( 'NONE',  ( 1.311418906110681266E-16, -0.7099284060911114080, -0.7042738517259704567 ) ) ;
#6420 = CARTESIAN_POINT ( 'NONE',  ( 5.901463166500145796, -9.653076390470529233, -17.64471554149788801 ) ) ;
#6421 = AXIS2_PLACEMENT_3D ( 'NONE', #54757, #11891, #30970 ) ;
#6422 = CARTESIAN_POINT ( 'NONE',  ( 0.6009453534118438522, -0.4363813339961392646, 48.10564080474284054 ) ) ;
#6423 = CARTESIAN_POINT ( 'NONE',  ( 4.963659409799330291, 19.36487359954752918, -40.34793212403946683 ) ) ;
#6425 = ORIENTED_EDGE ( 'NONE', *, *, #16646, .T. ) ;
#6424 = CARTESIAN_POINT ( 'NONE',  ( 4.691466044806103852, -36.88741755356086571, 25.04870410140726733 ) ) ;
#6426 = ORIENTED_EDGE ( 'NONE', *, *, #30182, .T. ) ;
#6427 = CARTESIAN_POINT ( 'NONE',  ( 3.680974057930773924, 1.849713332883747841, -47.94008194857089222 ) ) ;
#6428 = FACE_OUTER_BOUND ( 'NONE', #2931, .T. ) ;
#6429 = CARTESIAN_POINT ( 'NONE',  ( 0.5850706913938534814, 38.10903744847141894, 29.01314519953811555 ) ) ;
#6430 = EDGE_CURVE ( 'NONE', #14715, #58555, #25436, .T. ) ;
#6431 = CARTESIAN_POINT ( 'NONE',  ( -2.569797478183783568, -10.65947181927832865, -10.02484965418637586 ) ) ;
#6432 = CARTESIAN_POINT ( 'NONE',  ( 4.291220156522059348, -5.703517857940158642, -46.76386298574845313 ) ) ;
#6433 = CARTESIAN_POINT ( 'NONE',  ( 0.1092565886968784455, 41.57372480460685438, -11.46097737058320298 ) ) ;
#6435 = ADVANCED_FACE ( 'NONE', ( #12756 ), #13013, .F. ) ;
#6434 = VERTEX_POINT ( 'NONE', #53763 ) ;
#6436 = VERTEX_POINT ( 'NONE', #2699 ) ;
#6437 = CIRCLE ( 'NONE', #24447, 43.08621763946400307 ) ;
#6438 = DIRECTION ( 'NONE',  ( 0.000000000000000000, 0.000000000000000000, 1.000000000000000000 ) ) ;
#6440 = CARTESIAN_POINT ( 'NONE',  ( 0.6000166863083106206, 48.10206967781414278, -9.900220927795848169 ) ) ;
#6439 = CONICAL_SURFACE ( 'NONE', #25470, 42.08604991992415023, 1.569615340895231137 ) ;
#6441 = B_SPLINE_CURVE_WITH_KNOTS ( 'NONE', 3,
 ( #17471, #59439, #46005, #21552, #16546, #40378 ),
 .UNSPECIFIED., .F., .F.,
 ( 4, 2, 4 ),
 ( 1.497543825688427252E-16, 0.0002445252820015178345, 0.0004890505640028859407 ),
 .UNSPECIFIED. ) ;
#6442 = FACE_OUTER_BOUND ( 'NONE', #21551, .T. ) ;
#6443 = ORIENTED_EDGE ( 'NONE', *, *, #26369, .F. ) ;
#6444 = VECTOR ( 'NONE', #19948, 1000.000000000000000 ) ;
#6445 = CARTESIAN_POINT ( 'NONE',  ( 0.1103310638050661735, -0.08238894504425745002, 43.12437788119554227 ) ) ;
#6446 = CARTESIAN_POINT ( 'NONE',  ( 4.967162193818130511, 42.34252806656603241, -7.970725651239366272 ) ) ;
#6447 = VERTEX_POINT ( 'NONE', #17435 ) ;
#6448 = CARTESIAN_POINT ( 'NONE',  ( 0.9757892942422814464, 41.43309903783670478, -11.15510465568958409 ) ) ;
#6449 = ORIENTED_EDGE ( 'NONE', *, *, #26889, .F. ) ;
#6450 = CARTESIAN_POINT ( 'NONE',  ( 4.956445790443995136, 19.33052208089553758, 42.94029536716820417 ) ) ;
#6451 = CARTESIAN_POINT ( 'NONE',  ( 0.6039202388192952409, -39.45949250020272814, 29.23204003273524521 ) ) ;
#6452 = ORIENTED_EDGE ( 'NONE', *, *, #54819, .T. ) ;
#6453 = DIRECTION ( 'NONE',  ( -0.07906939808003035641, -0.1578407582592981639, 0.9842938206244065125 ) ) ;
#6454 = CARTESIAN_POINT ( 'NONE',  ( -6.079354080745853928, -18.27537090945901710, -6.066611358069764037 ) ) ;
#6455 = CARTESIAN_POINT ( 'NONE',  ( 0.5837374860065643878, 41.38807031854345553, -24.10515569139005621 ) ) ;
#6456 = CARTESIAN_POINT ( 'NONE',  ( 0.3622758884714600280, 43.10531414739104150, 0.8252992914329575491 ) ) ;
#6457 = B_SPLINE_CURVE_WITH_KNOTS ( 'NONE', 3,
 ( #7594, #17327, #12643, #17954, #27335, #46157 ),
 .UNSPECIFIED., .F., .F.,
 ( 4, 2, 4 ),
 ( 8.344835848757739736E-18, 0.0002291472222819933150, 0.0004582944445639782816 ),
 .UNSPECIFIED. ) ;
#6458 = ORIENTED_EDGE ( 'NONE', *, *, #59686, .T. ) ;
#6459 = CARTESIAN_POINT ( 'NONE',  ( 0.5797568665920715958, -19.16764089848626185, 42.79984638977747124 ) ) ;
#6460 = ADVANCED_FACE ( 'NONE', ( #60029 ), #23783, .F. ) ;
#6461 = ORIENTED_EDGE ( 'NONE', *, *, #22632, .T. ) ;
#6462 = CARTESIAN_POINT ( 'NONE',  ( 3.376099380956842921, 12.80002687883565748, -3.983427611134879864 ) ) ;
#6463 =( BOUNDED_SURFACE ( )  B_SPLINE_SURFACE ( 3, 1, ( 
 ( #34924, #48087 ),
 ( #58683, #24895 ),
 ( #53074, #5140 ),
 ( #44334, #39625 ) ),
 .UNSPECIFIED., .F., .F., .F. ) 
 B_SPLINE_SURFACE_WITH_KNOTS ( ( 4, 4 ),
 ( 2, 2 ),
 ( 0.000000000000000000, 1.000000000000000000 ),
 ( 0.000000000000000000, 1.000000000000000000 ),
 .UNSPECIFIED. ) 
 GEOMETRIC_REPRESENTATION_ITEM ( )  RATIONAL_B_SPLINE_SURFACE ( (
 ( 1.000000000000000000, 1.000000000000000000),
 ( 0.9953485035131437453, 0.8621029689291515030),
 ( 0.9953485035131437453, 0.8621029689291515030),
 ( 1.000000000000000000, 1.000000000000000000) ) ) 
 REPRESENTATION_ITEM ( '' )  SURFACE ( )  );
#6464 = VECTOR ( 'NONE', #57841, 1000.000000000000227 ) ;
#6465 = VERTEX_POINT ( 'NONE', #26518 ) ;
#6466 = CARTESIAN_POINT ( 'NONE',  ( 0.9790724872846784388, 4.154643925904573543, 41.70220790114591836 ) ) ;
#6467 = ORIENTED_EDGE ( 'NONE', *, *, #37077, .F. ) ;
#6468 = CARTESIAN_POINT ( 'NONE',  ( 0.5987334363312686314, 10.33658596697176257, 48.00747751152395182 ) ) ;
#6469 = CARTESIAN_POINT ( 'NONE',  ( 0.9775691876210979014, 36.24929767012833537, -21.03145566556006330 ) ) ;
#6470 = EDGE_CURVE ( 'NONE', #33914, #42943, #44776, .T. ) ;
#6471 = CARTESIAN_POINT ( 'NONE',  ( 0.8744876279028306332, 48.92939099258504143, -4.032957658373305776 ) ) ;
#6472 = EDGE_LOOP ( 'NONE', ( #12224, #55308, #22603, #6736 ) ) ;
#6473 = CARTESIAN_POINT ( 'NONE',  ( 0.2285344041767100043, 41.62591743292807678, -14.62135999702185707 ) ) ;
#6474 = ADVANCED_FACE ( 'NONE', ( #60950 ), #4914, .F. ) ;
#6475 = CARTESIAN_POINT ( 'NONE',  ( 0.8560838555295223751, -44.60403252362528548, -14.52078223489045072 ) ) ;
#6476 = CARTESIAN_POINT ( 'NONE',  ( -5.995132425357893702, -14.94489030678143493, -11.47834865841111451 ) ) ;
#6477 = ORIENTED_EDGE ( 'NONE', *, *, #28715, .T. ) ;
#6478 = ORIENTED_EDGE ( 'NONE', *, *, #26678, .F. ) ;
#6479 = CARTESIAN_POINT ( 'NONE',  ( 0.9762797500689124330, -30.73989051779308568, -28.48480149377557424 ) ) ;
#6480 = CARTESIAN_POINT ( 'NONE',  ( 2.009741617377216460, 30.60835445554638312, 31.66437612122933487 ) ) ;
#6481 = CARTESIAN_POINT ( 'NONE',  ( 4.549368137175248350, 24.02461520945271900, -35.57418903283089406 ) ) ;
#6482 = DIRECTION ( 'NONE',  ( 0.07500201931887538753, 0.01982172072487804054, 0.9969863572213993885 ) ) ;
#6483 = CARTESIAN_POINT ( 'NONE',  ( 0.1073791018717578927, 30.14884492832347718, 30.83464511437148659 ) ) ;
#6485 = VECTOR ( 'NONE', #41593, 1000.000000000000114 ) ;
#6484 = DIRECTION ( 'NONE',  ( -0.07836865515943411409, 0.2656332009267315386, 0.9608836331491552585 ) ) ;
#6486 = VERTEX_POINT ( 'NONE', #12436 ) ;
#6487 = CARTESIAN_POINT ( 'NONE',  ( 4.956445790443991584, 41.78282513192503700, 21.71942849465911252 ) ) ;
#6488 = CARTESIAN_POINT ( 'NONE',  ( 0.8557997880470606944, -28.43566216844945771, -38.55640757422467857 ) ) ;
#6489 = EDGE_LOOP ( 'NONE', ( #15221, #26737, #59392, #23914 ) ) ;
#6490 = VECTOR ( 'NONE', #52929, 1000.000000000000000 ) ;
#6491 = CARTESIAN_POINT ( 'NONE',  ( -6.016104459813371719, 11.47525878590916193, 14.94608397322088678 ) ) ;
#6492 = CARTESIAN_POINT ( 'NONE',  ( 0.6008123274975392114, -19.47899178227436323, -45.07907974110103311 ) ) ;
#6493 = VECTOR ( 'NONE', #1396, 1000.000000000000000 ) ;
#6494 = CARTESIAN_POINT ( 'NONE',  ( 0.1149546198390367646, -42.74978084130992073, 10.92715896485409210 ) ) ;
#6495 = LINE ( 'NONE', #58825, #34730 ) ;
#6496 = CARTESIAN_POINT ( 'NONE',  ( 4.956445790444035104, 39.12691469764034480, -26.20348443209818967 ) ) ;
#6497 = CARTESIAN_POINT ( 'NONE',  ( 0.5782707292762423457, 40.71812376972668801, 23.27596937574968905 ) ) ;
#6498 = CARTESIAN_POINT ( 'NONE',  ( 0.1155031312995260795, 20.55835925191953351, -39.04222710605559854 ) ) ;
#6499 = CARTESIAN_POINT ( 'NONE',  ( -6.015611763856276717, 18.20278301740943405, -4.870987357967985432 ) ) ;
#6500 = CARTESIAN_POINT ( 'NONE',  ( 0.1154773475650540532, 29.79763058674064169, 32.54296915559886827 ) ) ;
#6501 = CARTESIAN_POINT ( 'NONE',  ( 0.1368894036331280706, -2.051263853491218647, -44.07554472183745276 ) ) ;
#6502 =( NAMED_UNIT ( * ) SI_UNIT ( $, .STERADIAN. ) SOLID_ANGLE_UNIT ( ) );
#6503 = CARTESIAN_POINT ( 'NONE',  ( 1.834102595619085507, -21.70983406038687491, 38.32598139549919836 ) ) ;
#6504 = DIRECTION ( 'NONE',  ( 0.000000000000000000, 0.000000000000000000, 1.000000000000000000 ) ) ;
#6505 = CARTESIAN_POINT ( 'NONE',  ( 5.959547316686252039, -20.52562247508876681, -0.003562808152834123603 ) ) ;
#6506 = DIRECTION ( 'NONE',  ( -0.07836865515943412797, -0.1379401902675499447, -0.9873352307081186829 ) ) ;
#6507 = ADVANCED_FACE ( 'NONE', ( #21514 ), #46267, .F. ) ;
#6508 = ORIENTED_EDGE ( 'NONE', *, *, #20731, .F. ) ;
#6509 = FACE_OUTER_BOUND ( 'NONE', #7401, .T. ) ;
#6510 = PLANE ( 'NONE',  #44955 ) ;
#6511 = CARTESIAN_POINT ( 'NONE',  ( 0.9736507210033074067, -25.76216842460672751, -34.31386771842686301 ) ) ;
#6512 = CARTESIAN_POINT ( 'NONE',  ( 5.895596859100789899, -13.98490190264574196, 14.45512718677573538 ) ) ;
#6513 = CARTESIAN_POINT ( 'NONE',  ( 0.1103744047535531458, -41.66501489234570954, 11.12399292196364442 ) ) ;
#6514 = ORIENTED_EDGE ( 'NONE', *, *, #10630, .T. ) ;
#6515 = CARTESIAN_POINT ( 'NONE',  ( 5.974727161628369032, 20.52494643607030156, 0.01551142186656635953 ) ) ;
#6516 = CARTESIAN_POINT ( 'NONE',  ( 5.965394784446458765, 10.27521535480962100, 17.76824826579358430 ) ) ;
#6517 = B_SPLINE_CURVE_WITH_KNOTS ( 'NONE', 3,
 ( #45244, #17032, #40243, #41463, #59296, #12645 ),
 .UNSPECIFIED., .F., .F.,
 ( 4, 2, 4 ),
 ( 3.511543213478341086E-18, 0.0002450742804987343930, 0.0004901485609974652081 ),
 .UNSPECIFIED. ) ;
#6518 = CARTESIAN_POINT ( 'NONE',  ( 4.962356264823608143, 0.000000000000000000, 0.000000000000000000 ) ) ;
#6519 = VERTEX_POINT ( 'NONE', #7707 ) ;
#6520 = CARTESIAN_POINT ( 'NONE',  ( 3.221118495291109163, -43.94535254261806045, 1.888758737044896163 ) ) ;
#6521 = CIRCLE ( 'NONE', #8514, 42.08604991992415023 ) ;
#6522 = CARTESIAN_POINT ( 'NONE',  ( 1.827326673878743923, 41.24690799101790617, 12.32830836993835177 ) ) ;
#6523 = EDGE_LOOP ( 'NONE', ( #53541, #22587, #14587, #14213 ) ) ;
#6524 = CARTESIAN_POINT ( 'NONE',  ( 0.8760168074886960365, -13.30888447662112561, 46.22580377597762435 ) ) ;
#6525 = AXIS2_PLACEMENT_3D ( 'NONE', #24205, #52704, #5075 ) ;
#6526 = EDGE_LOOP ( 'NONE', ( #20989, #13168, #30900, #45280 ) ) ;
#6527 = FACE_OUTER_BOUND ( 'NONE', #2100, .T. ) ;
#6528 = VERTEX_POINT ( 'NONE', #59716 ) ;
#6529 = CARTESIAN_POINT ( 'NONE',  ( 4.962356264823609031, -35.98698831890617100, -21.82137185415387037 ) ) ;
#6530 = CARTESIAN_POINT ( 'NONE',  ( -2.569797478183783568, -10.02484965418648599, 10.65947181927822207 ) ) ;
#6531 = ORIENTED_EDGE ( 'NONE', *, *, #27579, .T. ) ;
#6532 = EDGE_CURVE ( 'NONE', #15927, #29824, #6650, .T. ) ;
#6533 = CIRCLE ( 'NONE', #49577, 48.09070567114147110 ) ;
#6534 = B_SPLINE_CURVE_WITH_KNOTS ( 'NONE', 3,
 ( #48341, #14536, #29224, #58634 ),
 .UNSPECIFIED., .F., .F.,
 ( 4, 4 ),
 ( 2.318063799052743651E-17, 0.004564976165746187711 ),
 .UNSPECIFIED. ) ;
#6535 = ORIENTED_EDGE ( 'NONE', *, *, #18753, .T. ) ;
#6536 = CARTESIAN_POINT ( 'NONE',  ( 4.963659409799331179, -14.83726297270249006, -42.22332985082326928 ) ) ;
#6537 = EDGE_CURVE ( 'NONE', #26600, #24124, #58930, .T. ) ;
#6538 = DIRECTION ( 'NONE',  ( 0.09835009131224552170, 0.5042575517176567379, 0.8579344853044360564 ) ) ;
#6540 = EDGE_CURVE ( 'NONE', #4994, #55598, #8321, .T. ) ;
#6539 = ORIENTED_EDGE ( 'NONE', *, *, #41623, .T. ) ;
#6541 =( BOUNDED_SURFACE ( )  B_SPLINE_SURFACE ( 3, 1, ( 
 ( #49397, #44730 ),
 ( #7080, #25910 ),
 ( #11506, #35017 ),
 ( #45044, #49708 ) ),
 .UNSPECIFIED., .F., .F., .F. ) 
 B_SPLINE_SURFACE_WITH_KNOTS ( ( 4, 4 ),
 ( 2, 2 ),
 ( 0.000000000000000000, 1.000000000000000000 ),
 ( 0.000000000000000000, 1.000000000000000000 ),
 .UNSPECIFIED. ) 
 GEOMETRIC_REPRESENTATION_ITEM ( )  RATIONAL_B_SPLINE_SURFACE ( (
 ( 1.000000000000000000, 1.000000000000000000),
 ( 0.7269869731126817891, 0.9931720237060910339),
 ( 0.7269869731126817891, 0.9931720237060910339),
 ( 1.000000000000000000, 1.000000000000000000) ) ) 
 REPRESENTATION_ITEM ( '' )  SURFACE ( )  );
#6542 = VERTEX_POINT ( 'NONE', #13362 ) ;
#6543 = CARTESIAN_POINT ( 'NONE',  ( 1.399999999999999467, 0.000000000000000000, 0.000000000000000000 ) ) ;
#6544 = CARTESIAN_POINT ( 'NONE',  ( 0.6031356219577718170, 24.12932366310808519, 41.61861914321219302 ) ) ;
#6545 = CARTESIAN_POINT ( 'NONE',  ( 5.960221823109900008, -7.859839668735083329, -18.96108896995712101 ) ) ;
#6546 = EDGE_LOOP ( 'NONE', ( #24452, #48553, #3046, #47023 ) ) ;
#6547 = EDGE_CURVE ( 'NONE', #59254, #34686, #13357, .T. ) ;
#6548 = CARTESIAN_POINT ( 'NONE',  ( -6.078457390727109555, -18.27366031693659210, -6.071890122418616365 ) ) ;
#6549 = DIRECTION ( 'NONE',  ( 0.000000000000000000, 0.000000000000000000, 1.000000000000000000 ) ) ;
#6550 = B_SPLINE_CURVE_WITH_KNOTS ( 'NONE', 3,
 ( #19772, #15071, #38893, #42353 ),
 .UNSPECIFIED., .F., .F.,
 ( 4, 4 ),
 ( 1.734723475976807094E-18, 0.004042984057420972825 ),
 .UNSPECIFIED. ) ;
#6551 = ORIENTED_EDGE ( 'NONE', *, *, #33289, .T. ) ;
#6552 = FACE_OUTER_BOUND ( 'NONE', #8235, .T. ) ;
#6553 = VERTEX_POINT ( 'NONE', #38411 ) ;
#6554 = CARTESIAN_POINT ( 'NONE',  ( -6.001507490154110336, 13.33564355450108430, 13.31361390284164692 ) ) ;
#6555 = CARTESIAN_POINT ( 'NONE',  ( 1.227938101723747621, 20.72293514920750468, 37.58536632582787007 ) ) ;
#6556 = ORIENTED_EDGE ( 'NONE', *, *, #31470, .T. ) ;
#6557 = LINE ( 'NONE', #645, #50562 ) ;
#6558 = CARTESIAN_POINT ( 'NONE',  ( 3.680974057930773924, -45.82782223000864974, -14.19449211152921997 ) ) ;
#6559 = CARTESIAN_POINT ( 'NONE',  ( 51.18761205055119490, 12.23403309190988075, -2.565078866171123906 ) ) ;
#6560 = CARTESIAN_POINT ( 'NONE',  ( 3.680882792899936362, -16.63701193714018700, 44.99870212802612457 ) ) ;
#6561 = EDGE_CURVE ( 'NONE', #16220, #6447, #22842, .T. ) ;
#6562 = ORIENTED_EDGE ( 'NONE', *, *, #36899, .F. ) ;
#6563 = CARTESIAN_POINT ( 'NONE',  ( 4.322998006666179727, -32.40067585697823205, 35.39923696758956595 ) ) ;
#6564 = VERTEX_POINT ( 'NONE', #32781 ) ;
#6565 = EDGE_CURVE ( 'NONE', #3838, #3952, #2904, .T. ) ;
#6566 = CARTESIAN_POINT ( 'NONE',  ( 0.1129192098497455998, 39.54191224844618802, 19.58032082273768637 ) ) ;
#6567 = LINE ( 'NONE', #25397, #12808 ) ;
#6568 = CARTESIAN_POINT ( 'NONE',  ( 0.5806925824938499181, 17.36345040154836994, -43.56297685531297503 ) ) ;
#6569 = DIRECTION ( 'NONE',  ( 1.000000000000000000, -0.000000000000000000, -0.000000000000000000 ) ) ;
#6570 = FACE_OUTER_BOUND ( 'NONE', #20810, .T. ) ;
#6571 = VECTOR ( 'NONE', #43666, 999.9999999999998863 ) ;
#6572 = CARTESIAN_POINT ( 'NONE',  ( 0.8744876279028306332, 36.80052600666260787, -32.49725120702428427 ) ) ;
#6573 = DIRECTION ( 'NONE',  ( -0.07439287786467650709, 0.2708295585865068689, 0.9597484305373201741 ) ) ;
#6574 = CARTESIAN_POINT ( 'NONE',  ( 0.1119898979215349089, -27.07006246863960541, 34.84498566789457641 ) ) ;
#6575 = CIRCLE ( 'NONE', #54567, 47.91270532121795611 ) ;
#6576 = CARTESIAN_POINT ( 'NONE',  ( 10.00000000000001599, -56.56854249492331377, -56.56854249492430142 ) ) ;
#6577 = CARTESIAN_POINT ( 'NONE',  ( -6.016104459813371719, -11.47525878590906423, -14.94608397322096138 ) ) ;
#6578 = EDGE_CURVE ( 'NONE', #50243, #226, #4537, .T. ) ;
#6579 = FACE_OUTER_BOUND ( 'NONE', #4559, .T. ) ;
#6580 = CARTESIAN_POINT ( 'NONE',  ( 0.6029443199889047422, -45.51847136150880857, 18.42841302895899247 ) ) ;
#6581 = CIRCLE ( 'NONE', #60618, 47.91270532121795611 ) ;
#6582 = ORIENTED_EDGE ( 'NONE', *, *, #61154, .T. ) ;
#6583 = CARTESIAN_POINT ( 'NONE',  ( 2.359973842542475886, -2.918503669880030849, -43.92742003534235806 ) ) ;
#6584 = CARTESIAN_POINT ( 'NONE',  ( 0.7048096507298635682, -47.58126109679107429, 7.115188260603041215 ) ) ;
#6585 = CARTESIAN_POINT ( 'NONE',  ( 0.8744876279028263033, -45.16590161814997373, -19.24555484778471026 ) ) ;
#6586 = ORIENTED_EDGE ( 'NONE', *, *, #28861, .T. ) ;
#6587 = EDGE_CURVE ( 'NONE', #45047, #33819, #55826, .T. ) ;
#6588 = CARTESIAN_POINT ( 'NONE',  ( 2.526552050251863690, -15.32056541070812905, -40.15571433620802111 ) ) ;
#6589 = CARTESIAN_POINT ( 'NONE',  ( 0.1147471544378676350, 4.545905012546410440, 43.88948548445461029 ) ) ;
#6590 = DIRECTION ( 'NONE',  ( 0.000000000000000000, 0.000000000000000000, 1.000000000000000000 ) ) ;
#6591 = PRODUCT_DEFINITION_CONTEXT ( 'detailed design', #4407, 'design' ) ;
#6592 = ORIENTED_EDGE ( 'NONE', *, *, #60446, .F. ) ;
#6593 = CARTESIAN_POINT ( 'NONE',  ( 0.6253024248130486518, -45.25541762693965353, -19.06282777630130809 ) ) ;
#6594 = CARTESIAN_POINT ( 'NONE',  ( 4.694002226626921015, -43.15593359350852154, -14.69184015427673273 ) ) ;
#6595 = ORIENTED_EDGE ( 'NONE', *, *, #20872, .F. ) ;
#6596 = CARTESIAN_POINT ( 'NONE',  ( 0.6008122571543325074, 11.35154853257121843, 47.77757733893585623 ) ) ;
#6597 = ORIENTED_EDGE ( 'NONE', *, *, #47552, .T. ) ;
#6598 = ORIENTED_EDGE ( 'NONE', *, *, #13975, .F. ) ;
#6599 = CARTESIAN_POINT ( 'NONE',  ( 0.7948884756798505480, -48.79909643092307903, 5.417271649605749140 ) ) ;
#6600 = ORIENTED_EDGE ( 'NONE', *, *, #12325, .T. ) ;
#6601 = DIRECTION ( 'NONE',  ( -0.07500201931887529039, -0.1525301372901670394, 0.9854487578338784193 ) ) ;
#6602 = B_SPLINE_CURVE_WITH_KNOTS ( 'NONE', 3,
 ( #12924, #40827, #13221, #32020 ),
 .UNSPECIFIED., .F., .F.,
 ( 4, 4 ),
 ( 2.380737581618737539E-07, 0.002336974151641576809 ),
 .UNSPECIFIED. ) ;
#6603 = CARTESIAN_POINT ( 'NONE',  ( -6.016761891674565099, 16.31696541414272161, 9.424569481870310739 ) ) ;
#6604 = ORIENTED_EDGE ( 'NONE', *, *, #44026, .T. ) ;
#6605 = CARTESIAN_POINT ( 'NONE',  ( 0.2279481005628805901, 37.38452800950467747, -23.42862677536759719 ) ) ;
#6606 = CARTESIAN_POINT ( 'NONE',  ( 2.526552050251863246, 41.81191169914609418, -9.948123361606407755 ) ) ;
#6607 = EDGE_CURVE ( 'NONE', #38419, #33924, #43329, .T. ) ;
#6608 = VECTOR ( 'NONE', #3036, 1000.000000000000114 ) ;
#6609 = ORIENTED_EDGE ( 'NONE', *, *, #46006, .T. ) ;
#6610 = CARTESIAN_POINT ( 'NONE',  ( 0.6030672727741701600, -18.49051564326162023, 44.41203814406376438 ) ) ;
#6611 = VECTOR ( 'NONE', #40481, 999.9999999999998863 ) ;
#6612 = FACE_OUTER_BOUND ( 'NONE', #26292, .T. ) ;
#6613 = CARTESIAN_POINT ( 'NONE',  ( 5.958863334805807099, -14.51469124124489873, 14.51296551801777923 ) ) ;
#6614 = CIRCLE ( 'NONE', #60655, 47.09074272231896430 ) ;
#6615 = CARTESIAN_POINT ( 'NONE',  ( 0.8751705887134553219, 13.30665218149297857, 46.21789262997761938 ) ) ;
#6616 = ORIENTED_EDGE ( 'NONE', *, *, #7104, .T. ) ;
#6617 = EDGE_CURVE ( 'NONE', #57884, #23449, #38784, .T. ) ;
#6618 = ORIENTED_EDGE ( 'NONE', *, *, #48321, .T. ) ;
#6619 = CARTESIAN_POINT ( 'NONE',  ( 0.5807400328401574052, -23.47602859900744576, 41.75144119563878320 ) ) ;
#6620 = CARTESIAN_POINT ( 'NONE',  ( -6.078726893082806448, -18.90156862012328887, -3.677600436084754509 ) ) ;
#6621 = CARTESIAN_POINT ( 'NONE',  ( 0.8557997880470606944, -17.48760788519184217, -44.60232077416704755 ) ) ;
#6622 = VERTEX_POINT ( 'NONE', #46889 ) ;
#6623 = CARTESIAN_POINT ( 'NONE',  ( -4.908599999999998964, 12.80000000000000071, 3.000000000000000000 ) ) ;
#6624 = CARTESIAN_POINT ( 'NONE',  ( 0.8554163680231738898, 5.604726001789477330, -46.58103175710779453 ) ) ;
#6625 = DIRECTION ( 'NONE',  ( -3.273063162220391312E-16, 1.000000000000000000, 1.047380211910525220E-14 ) ) ;
#6626 = CIRCLE ( 'NONE', #41706, 10.00000000000000711 ) ;
#6627 = ORIENTED_EDGE ( 'NONE', *, *, #33888, .T. ) ;
#6628 = ORIENTED_EDGE ( 'NONE', *, *, #33756, .T. ) ;
#6629 = CARTESIAN_POINT ( 'NONE',  ( 0.9790850452238856194, -39.60641447000896420, -13.69924315767353740 ) ) ;
#6630 = CARTESIAN_POINT ( 'NONE',  ( 0.1100247026804066219, 34.10937070541709204, 26.38690693952968758 ) ) ;
#6631 = CARTESIAN_POINT ( 'NONE',  ( 3.661921753702025661, 2.831104162483613518, -46.95333825251623949 ) ) ;
#6632 = EDGE_CURVE ( 'NONE', #38290, #59505, #13991, .T. ) ;
#6633 = CARTESIAN_POINT ( 'NONE',  ( 0.6000166863083106206, 32.62822748873707468, 36.70452632376116497 ) ) ;
#6634 = CARTESIAN_POINT ( 'NONE',  ( 0.7762777257811892540, -17.50713318242604899, -44.59086130178268803 ) ) ;
#6635 =( BOUNDED_SURFACE ( )  B_SPLINE_SURFACE ( 3, 1, ( 
 ( #6885, #54820 ),
 ( #39846, #40454 ),
 ( #31030, #50138 ),
 ( #45459, #55127 ) ),
 .UNSPECIFIED., .F., .F., .F. ) 
 B_SPLINE_SURFACE_WITH_KNOTS ( ( 4, 4 ),
 ( 2, 2 ),
 ( 0.000000000000000000, 1.000000000000000000 ),
 ( 0.000000000000000000, 1.000000000000000000 ),
 .UNSPECIFIED. ) 
 GEOMETRIC_REPRESENTATION_ITEM ( )  RATIONAL_B_SPLINE_SURFACE ( (
 ( 1.000000000000000000, 1.000000000000000000),
 ( 0.9953485035131437453, 0.8621029689291515030),
 ( 0.9953485035131437453, 0.8621029689291515030),
 ( 1.000000000000000000, 1.000000000000000000) ) ) 
 REPRESENTATION_ITEM ( '' )  SURFACE ( )  );
#6636 = B_SPLINE_CURVE_WITH_KNOTS ( 'NONE', 3,
 ( #31421, #31110, #21097, #36449, #30174, #50520 ),
 .UNSPECIFIED., .F., .F.,
 ( 4, 2, 4 ),
 ( 8.148123767742043513E-18, 0.0002291978881530167564, 0.0004583957763060253271 ),
 .UNSPECIFIED. ) ;
#6637 = CARTESIAN_POINT ( 'NONE',  ( 4.226256110419179812, -41.57058058356821562, -14.23776948585163815 ) ) ;
#6638 = CARTESIAN_POINT ( 'NONE',  ( 4.060580049360325461, -14.70525263353195378, -41.41525370371659420 ) ) ;
#6639 = CARTESIAN_POINT ( 'NONE',  ( 0.6064782688330875304, -24.63250656785344717, -39.90706787780114695 ) ) ;
#6640 = CARTESIAN_POINT ( 'NONE',  ( 5.880360259849752858, 47.04104239318753855, 9.405269135695407456 ) ) ;
#6641 = CARTESIAN_POINT ( 'NONE',  ( 0.6023143664670691511, -6.538774821499543144, 47.66103278671578636 ) ) ;
#6642 = CARTESIAN_POINT ( 'NONE',  ( 0.7762777257811878107, -28.45155622761403436, -38.54028505510749625 ) ) ;
#6643 = CARTESIAN_POINT ( 'NONE',  ( 0.7762783648524373969, -41.03453896757959285, 24.71864151483699601 ) ) ;
#6644 = CARTESIAN_POINT ( 'NONE',  ( 5.896278296736517710, 14.92041660055649821, 13.48733287496908062 ) ) ;
#6645 = CARTESIAN_POINT ( 'NONE',  ( 1.834102595619085285, 41.37485482074667686, -15.11023273877077422 ) ) ;
#6646 = B_SPLINE_CURVE_WITH_KNOTS ( 'NONE', 3,
 ( #19008, #61566, #27768, #14000, #57169, #23683, #4244, #46900, #56873, #51247, #23379, #8644, #61868, #42815, #3623, #22759, #51869, #33103, #42206 ),
 .UNSPECIFIED., .F., .F.,
 ( 4, 3, 3, 3, 3, 3, 4 ),
 ( 1.355320476548679676E-18, 0.0002612768053151710043, 0.0003919133833142910339, 0.0005225499612322606451, 0.0006531865391693356332, 0.0008112755173415187732, 0.0009693688056799720310 ),
 .UNSPECIFIED. ) ;
#6647 = DIRECTION ( 'NONE',  ( -1.000000000000000000, -0.000000000000000000, -0.000000000000000000 ) ) ;
#6648 = DIRECTION ( 'NONE',  ( 0.07906939808003035641, -0.4861426559824300053, 0.8702949777642121632 ) ) ;
#6649 = CARTESIAN_POINT ( 'NONE',  ( 0.6023142530420679819, -6.538792732869529445, -47.66103033449096671 ) ) ;
#6650 = B_SPLINE_CURVE_WITH_KNOTS ( 'NONE', 3,
 ( #55011, #37178, #22136, #27441, #60321, #41566 ),
 .UNSPECIFIED., .F., .F.,
 ( 4, 2, 4 ),
 ( 0.000000000000000000, 0.0002447195606305735535, 0.0004894391212611471070 ),
 .UNSPECIFIED. ) ;
#6651 =( BOUNDED_SURFACE ( )  B_SPLINE_SURFACE ( 3, 1, ( 
 ( #60734, #45751 ),
 ( #60130, #27552 ),
 ( #3115, #22244 ),
 ( #41366, #31326 ) ),
 .UNSPECIFIED., .F., .F., .F. ) 
 B_SPLINE_SURFACE_WITH_KNOTS ( ( 4, 4 ),
 ( 2, 2 ),
 ( 0.000000000000000000, 1.000000000000000000 ),
 ( 0.000000000000000000, 1.000000000000000000 ),
 .UNSPECIFIED. ) 
 GEOMETRIC_REPRESENTATION_ITEM ( )  RATIONAL_B_SPLINE_SURFACE ( (
 ( 1.000000000000000000, 1.000000000000000000),
 ( 0.9953485035131437453, 0.8621029689291523912),
 ( 0.9953485035131437453, 0.8621029689291523912),
 ( 1.000000000000000000, 1.000000000000000000) ) ) 
 REPRESENTATION_ITEM ( '' )  SURFACE ( )  );
#6652 = CARTESIAN_POINT ( 'NONE',  ( 0.3676999524040366896, -34.85286720109691316, 27.04123205746257241 ) ) ;
#6653 = VECTOR ( 'NONE', #61284, 1000.000000000000000 ) ;
#6654 = CARTESIAN_POINT ( 'NONE',  ( 0.5997462898726536595, 23.17609050332868037, 43.29457771044576475 ) ) ;
#6655 = CARTESIAN_POINT ( 'NONE',  ( 0.6016117650947689910, 48.98309729621151831, -3.493885160444671012 ) ) ;
#6657 = ORIENTED_EDGE ( 'NONE', *, *, #627, .T. ) ;
#6656 = CARTESIAN_POINT ( 'NONE',  ( -15.25000000000000711, -2.688986455804108555, -9.952330921218299798E-16 ) ) ;
#6658 = VERTEX_POINT ( 'NONE', #14602 ) ;
#6659 =( GEOMETRIC_REPRESENTATION_CONTEXT ( 3 ) GLOBAL_UNCERTAINTY_ASSIGNED_CONTEXT ( ( #4140 ) ) GLOBAL_UNIT_ASSIGNED_CONTEXT ( ( #18478, #51047, #17252 ) ) REPRESENTATION_CONTEXT ( 'NONE', 'WORKASPACE' ) );
#6660 = CARTESIAN_POINT ( 'NONE',  ( -6.015611763856276717, -18.19956619163654565, -4.882992715191491584 ) ) ;
#6661 = CARTESIAN_POINT ( 'NONE',  ( 0.3622758884714600280, 11.95365414648497193, -41.42293301073613776 ) ) ;
#6662 = AXIS2_PLACEMENT_3D ( 'NONE', #56785, #9183, #10115 ) ;
#6663 = CARTESIAN_POINT ( 'NONE',  ( 7.999999999999996447, -2.650000000000270806, 80.00000000000000000 ) ) ;
#6664 = EDGE_CURVE ( 'NONE', #23991, #14306, #24553, .T. ) ;
#6665 = ORIENTED_EDGE ( 'NONE', *, *, #57751, .T. ) ;
#6666 = VERTEX_POINT ( 'NONE', #37808 ) ;
#6667 = CARTESIAN_POINT ( 'NONE',  ( 1.092182651088182910, -23.20727262041672745, -34.90248819158799876 ) ) ;
#6668 = CARTESIAN_POINT ( 'NONE',  ( 0.6028618097248864549, 6.452328974162978348, 47.67286800277445735 ) ) ;
#6669 = B_SPLINE_CURVE_WITH_KNOTS ( 'NONE', 3,
 ( #13346, #23051, #8615, #4519, #46872, #42178, #42479, #61537, #47471, #61237, #37469, #32762, #8941, #28050, #47170, #4212 ),
 .UNSPECIFIED., .F., .F.,
 ( 4, 3, 3, 3, 3, 4 ),
 ( 2.194378057379452319E-17, 0.0002612764279487761443, 0.0003919131003184802209, 0.0005225497727000647137, 0.0007837925190632471974, 0.001045051706266716951 ),
 .UNSPECIFIED. ) ;
#6670 = EDGE_CURVE ( 'NONE', #31157, #2500, #39553, .T. ) ;
#6671 = VERTEX_POINT ( 'NONE', #24290 ) ;
#6672 = ORIENTED_EDGE ( 'NONE', *, *, #2563, .F. ) ;
#6673 = CARTESIAN_POINT ( 'NONE',  ( 2.648799415243696664, 47.84750745855099296, 10.73002764644649787 ) ) ;
#6674 = EDGE_CURVE ( 'NONE', #29292, #28734, #59707, .T. ) ;
#6675 = AXIS2_PLACEMENT_3D ( 'NONE', #41405, #55456, #40477 ) ;
#6676 = DIRECTION ( 'NONE',  ( 1.000000000000000000, 0.000000000000000000, 0.000000000000000000 ) ) ;
#6678 = FACE_OUTER_BOUND ( 'NONE', #18161, .T. ) ;
#6677 = B_SPLINE_CURVE_WITH_KNOTS ( 'NONE', 3,
 ( #25462, #6957, #2263, #21393, #6326, #53956 ),
 .UNSPECIFIED., .F., .F.,
 ( 4, 2, 4 ),
 ( 0.000000000000000000, 0.0002447195606305751798, 0.0004894391212611503596 ),
 .UNSPECIFIED. ) ;
#6679 = EDGE_LOOP ( 'NONE', ( #19130, #54704, #54097, #48412 ) ) ;
#6680 = B_SPLINE_CURVE_WITH_KNOTS ( 'NONE', 3,
 ( #18376, #37490, #56567, #13681 ),
 .UNSPECIFIED., .F., .F.,
 ( 4, 4 ),
 ( 0.000000000000000000, 0.005014147105413704723 ),
 .UNSPECIFIED. ) ;
#6681 = CARTESIAN_POINT ( 'NONE',  ( 0.9787284016396615716, -41.10577017155041091, -8.164046639535335714 ) ) ;
#6682 = CARTESIAN_POINT ( 'NONE',  ( -6.016761891674565099, 18.84319130225482297, 0.003433883959850178927 ) ) ;
#6683 = DIRECTION ( 'NONE',  ( 0.000000000000000000, 0.000000000000000000, -1.000000000000000000 ) ) ;
#6684 = ORIENTED_EDGE ( 'NONE', *, *, #11551, .T. ) ;
#6685 = EDGE_CURVE ( 'NONE', #8457, #243, #58819, .T. ) ;
#6686 = ORIENTED_EDGE ( 'NONE', *, *, #37009, .F. ) ;
#6687 = CARTESIAN_POINT ( 'NONE',  ( 0.5998501479064708430, 44.64337787626247689, -17.92509395669061689 ) ) ;
#6688 = CARTESIAN_POINT ( 'NONE',  ( -5.995132425357893702, 9.429450169548182714, -16.31525984181023148 ) ) ;
#6689 = ORIENTED_EDGE ( 'NONE', *, *, #17053, .T. ) ;
#6690 = CARTESIAN_POINT ( 'NONE',  ( -5.995132425357893702, -18.20425902871271262, 4.869002713216508127 ) ) ;
#6691 = CARTESIAN_POINT ( 'NONE',  ( 0.6021447746440204973, -7.579515948152010019, 48.51898676889489082 ) ) ;
#6692 = CARTESIAN_POINT ( 'NONE',  ( 5.895596859100789899, -11.92767122914683675, -16.19440774656085935 ) ) ;
#6693 = CARTESIAN_POINT ( 'NONE',  ( 0.5834872094924161701, 12.61552836343356354, -46.20467604622288604 ) ) ;
#6694 = ADVANCED_FACE ( 'NONE', ( #14914 ), #30168, .F. ) ;
#6695 = ORIENTED_EDGE ( 'NONE', *, *, #17492, .T. ) ;
#6696 = CARTESIAN_POINT ( 'NONE',  ( 0.6009453534118438522, 18.00606795643212621, 44.61081284455538309 ) ) ;
#6697 = EDGE_CURVE ( 'NONE', #15210, #26085, #10869, .T. ) ;
#6698 = CARTESIAN_POINT ( 'NONE',  ( 4.967162193818130511, 0.000000000000000000, 0.000000000000000000 ) ) ;
#6699 = ORIENTED_EDGE ( 'NONE', *, *, #23148, .F. ) ;
#6700 = CARTESIAN_POINT ( 'NONE',  ( 9.500000000000000000, 0.000000000000000000, -1.199999999999999956 ) ) ;
#6701 = AXIS2_PLACEMENT_3D ( 'NONE', #8405, #32866, #4307 ) ;
#6702 = CARTESIAN_POINT ( 'NONE',  ( -6.057079549204054558, 18.62933071312873068, 4.876399110062378028 ) ) ;
#6703 = EDGE_LOOP ( 'NONE', ( #32876, #36871, #29626, #13580 ) ) ;
#6704 = CARTESIAN_POINT ( 'NONE',  ( 0.5997462898726536595, -48.63480578518805686, 6.797594896825438049 ) ) ;
#6705 = AXIS2_PLACEMENT_3D ( 'NONE', #39833, #37873, #29663 ) ;
#6706 = ORIENTED_EDGE ( 'NONE', *, *, #61784, .T. ) ;
#6707 = CARTESIAN_POINT ( 'NONE',  ( 0.1073791018717578927, 39.65380858626191696, 16.95003405440326816 ) ) ;
#6708 = VECTOR ( 'NONE', #22834, 1000.000000000000114 ) ;
#6709 = DIRECTION ( 'NONE',  ( 1.836766033387207149E-16, -1.000000000000000000, 0.000000000000000000 ) ) ;
#6710 = CARTESIAN_POINT ( 'NONE',  ( 5.860006189529234355, 48.12869875779313134, -3.171667470662035804 ) ) ;
#6711 = EDGE_CURVE ( 'NONE', #31302, #27767, #31324, .T. ) ;
#6712 = PRODUCT ( 'straight bevel gear(output)_iso_ISO - Straight bevel gear 2M 47GT 48PT 20PA 5FW ---47O25H120MD16.0N', 'straight bevel gear(output)_iso_ISO - Straight bevel gear 2M 47GT 48PT 20PA 5FW ---47O25H120MD16.0N', '', ( #45612 ) ) ;
#6713 = DIRECTION ( 'NONE',  ( 0.09835009131224550782, 0.1375559175655161059, 0.9855991218957035338 ) ) ;
#6714 = CARTESIAN_POINT ( 'NONE',  ( 4.226256110419178924, 22.42442410584029844, 37.78852277489284006 ) ) ;
#6715 = CARTESIAN_POINT ( 'NONE',  ( 5.895596859100789899, -7.232071727010249695, 18.76766692340490295 ) ) ;
#6716 = CARTESIAN_POINT ( 'NONE',  ( 0.7413678028165010536, -32.31867156292732091, -29.99982600246001851 ) ) ;
#6717 = FACE_OUTER_BOUND ( 'NONE', #36250, .T. ) ;
#6718 = CARTESIAN_POINT ( 'NONE',  ( 0.5819845079324672543, 38.27312975753810065, 28.79567599618773244 ) ) ;
#6719 = CARTESIAN_POINT ( 'NONE',  ( 4.956445790444040433, 44.65954324082233029, -14.93530206124928128 ) ) ;
#6720 = ORIENTED_EDGE ( 'NONE', *, *, #42025, .F. ) ;
#6721 = CARTESIAN_POINT ( 'NONE',  ( 5.965394784446458765, -14.50338846149142924, 14.52385693118977450 ) ) ;
#6722 = DIRECTION ( 'NONE',  ( 1.000000000000000000, 0.000000000000000000, 0.000000000000000000 ) ) ;
#6723 = CARTESIAN_POINT ( 'NONE',  ( -4.000000000000000000, 2.309401076758531346, -5.242734410091827613 ) ) ;
#6724 = CARTESIAN_POINT ( 'NONE',  ( 4.967162193818130511, 0.000000000000000000, 0.000000000000000000 ) ) ;
#6725 = CARTESIAN_POINT ( 'NONE',  ( 3.238741278300274917, -31.66556122967977771, 29.07934833201312941 ) ) ;
#6726 = CIRCLE ( 'NONE', #60762, 12.50000000000000000 ) ;
#6727 = CARTESIAN_POINT ( 'NONE',  ( 0.9787284016396591291, -30.95573971909037425, 28.25027747426143421 ) ) ;
#6728 = CARTESIAN_POINT ( 'NONE',  ( 15.00000000000000355, 4.858054913877314581E-13, 80.00000000000001421 ) ) ;
#6729 = CARTESIAN_POINT ( 'NONE',  ( 4.975801465491695552, -32.01766832630288206, -35.64402118370946937 ) ) ;
#6730 = CARTESIAN_POINT ( 'NONE',  ( 0.9268187852002115479, 36.39936320882078746, -24.87650881657170387 ) ) ;
#6731 = AXIS2_PLACEMENT_3D ( 'NONE', #54676, #11805, #30884 ) ;
#6732 = CARTESIAN_POINT ( 'NONE',  ( -2.601141883200665639, 12.74835759521969791, -7.763685084661332780 ) ) ;
#6733 = EDGE_CURVE ( 'NONE', #40756, #17512, #16339, .T. ) ;
#6735 = VERTEX_POINT ( 'NONE', #34320 ) ;
#6734 = CARTESIAN_POINT ( 'NONE',  ( 4.553261556744873317, -15.38244134641770167, -41.14510984366982171 ) ) ;
#6736 = ORIENTED_EDGE ( 'NONE', *, *, #53649, .F. ) ;
#6737 = CARTESIAN_POINT ( 'NONE',  ( 0.1073791018717578927, -34.50606437925563341, 25.86618856530653687 ) ) ;
#6738 = CARTESIAN_POINT ( 'NONE',  ( 5.965394784446460541, -14.52385693119012799, 14.50338846149107930 ) ) ;
#6739 = CARTESIAN_POINT ( 'NONE',  ( 0.1087620492084205998, 16.16798550313366434, 39.97903073778071814 ) ) ;
#6740 = EDGE_CURVE ( 'NONE', #61467, #43662, #8128, .T. ) ;
#6741 = VERTEX_POINT ( 'NONE', #20221 ) ;
#6742 = DIRECTION ( 'NONE',  ( 0.000000000000000000, 1.000000000000000000, 0.000000000000000000 ) ) ;
#6743 = CARTESIAN_POINT ( 'NONE',  ( 0.8751705887134553219, 0.8911681664081729792, 48.08707113907595243 ) ) ;
#6745 = B_SPLINE_CURVE_WITH_KNOTS ( 'NONE', 3,
 ( #18332, #52124, #42758, #3574, #37763, #51501 ),
 .UNSPECIFIED., .F., .F.,
 ( 4, 2, 4 ),
 ( 0.000000000000000000, 0.0002450742804987321162, 0.0004901485609974642324 ),
 .UNSPECIFIED. ) ;
#6744 = CARTESIAN_POINT ( 'NONE',  ( -6.016761891674564211, -14.94721834528423088, 11.47373234755497862 ) ) ;
#6746 = EDGE_CURVE ( 'NONE', #49329, #33083, #41777, .T. ) ;
#6747 = VERTEX_POINT ( 'NONE', #35560 ) ;
#6748 = ORIENTED_EDGE ( 'NONE', *, *, #44945, .T. ) ;
#6749 = DIRECTION ( 'NONE',  ( -1.000000000000000000, -0.000000000000000000, -0.000000000000000000 ) ) ;
#6750 = EDGE_CURVE ( 'NONE', #59272, #4442, #14146, .T. ) ;
#6751 = ADVANCED_FACE ( 'NONE', ( #49022 ), #34961, .F. ) ;
#6752 = AXIS2_PLACEMENT_3D ( 'NONE', #21935, #59825, #26941 ) ;
#6753 = CARTESIAN_POINT ( 'NONE',  ( 4.553261556744875094, 27.56395660609745235, -34.20186927699732138 ) ) ;
#6754 = CARTESIAN_POINT ( 'NONE',  ( 0.6021447746440204973, 37.56149566485957081, 31.63345037309751007 ) ) ;
#6755 = ORIENTED_EDGE ( 'NONE', *, *, #47460, .F. ) ;
#6756 = ORIENTED_EDGE ( 'NONE', *, *, #44992, .T. ) ;
#6757 = CARTESIAN_POINT ( 'NONE',  ( 0.3622758884714730732, -10.35929834645951964, 41.85013935980084199 ) ) ;
#6758 = CARTESIAN_POINT ( 'NONE',  ( -2.601141883200662974, 9.698805021789313585, -11.34586306186986526 ) ) ;
#6759 = VERTEX_POINT ( 'NONE', #15214 ) ;
#6760 = SHAPE_REPRESENTATION ( 'housing left', ( #14677 ), #24835 ) ;
#6761 = CARTESIAN_POINT ( 'NONE',  ( 0.8753041380234530822, 28.81806460335451803, 39.75748332565663645 ) ) ;
#6762 = CARTESIAN_POINT ( 'NONE',  ( 4.549368137175248350, -35.80950303116117794, 23.67244292351576718 ) ) ;
#6763 = EDGE_LOOP ( 'NONE', ( #13672, #23227, #40995, #58881 ) ) ;
#6764 = EDGE_CURVE ( 'NONE', #28331, #12754, #12703, .T. ) ;
#6765 = CARTESIAN_POINT ( 'NONE',  ( 0.2885697896453111033, -36.93108635218683844, -22.25146201964130555 ) ) ;
#6766 = CARTESIAN_POINT ( 'NONE',  ( -6.079354080745853928, 15.43270669589069222, -11.51627193525633075 ) ) ;
#6767 = ORIENTED_EDGE ( 'NONE', *, *, #9901, .F. ) ;
#6768 = CARTESIAN_POINT ( 'NONE',  ( -6.079354080745853928, 3.072100940895722943, 19.00934378291659144 ) ) ;
#6769 = FACE_OUTER_BOUND ( 'NONE', #30520, .T. ) ;
#6770 = DIRECTION ( 'NONE',  ( 0.07906939808003035641, 0.4269277467251280100, -0.9008222518141226764 ) ) ;
#6771 = CARTESIAN_POINT ( 'NONE',  ( -6.015611763856276717, 16.32183393015609951, -9.416239407363130809 ) ) ;
#6772 = VECTOR ( 'NONE', #38678, 1000.000000000000114 ) ;
#6773 = ORIENTED_EDGE ( 'NONE', *, *, #58185, .T. ) ;
#6774 = CARTESIAN_POINT ( 'NONE',  ( 5.896782393890504181, -15.78847575145224447, 12.45994062280461634 ) ) ;
#6775 = CARTESIAN_POINT ( 'NONE',  ( 0.9730545539215883499, 16.88610103448558064, 39.44597740938066721 ) ) ;
#6776 = ORIENTED_EDGE ( 'NONE', *, *, #49614, .F. ) ;
#6777 = EDGE_CURVE ( 'NONE', #14733, #33003, #19354, .T. ) ;
#6778 = CARTESIAN_POINT ( 'NONE',  ( 4.962356264823608143, 0.000000000000000000, 0.000000000000000000 ) ) ;
#6779 = ORIENTED_EDGE ( 'NONE', *, *, #48651, .F. ) ;
#6780 = CARTESIAN_POINT ( 'NONE',  ( 0.5834872094924176134, -18.53852119651595842, 44.16273175734635004 ) ) ;
#6781 = CIRCLE ( 'NONE', #9807, 8.000000000000000000 ) ;
#6782 = ORIENTED_EDGE ( 'NONE', *, *, #30805, .F. ) ;
#6783 = CARTESIAN_POINT ( 'NONE',  ( 0.2885697896453112699, 41.43179225254749554, 11.93479333319038993 ) ) ;
#6784 = DIRECTION ( 'NONE',  ( 0.1011922191286468431, 0.2338987173090816551, 0.9669806227784434327 ) ) ;
#6785 = CARTESIAN_POINT ( 'NONE',  ( 0.1129192098497455998, 10.29049805561888498, -42.90754522869442411 ) ) ;
#6786 = VERTEX_POINT ( 'NONE', #39336 ) ;
#6787 = CARTESIAN_POINT ( 'NONE',  ( 0.1139756605157202368, 43.38486962273822911, 8.044147407465196409 ) ) ;
#6788 = CARTESIAN_POINT ( 'NONE',  ( 5.860006189529234355, 48.13093674595585014, 3.137522369585681759 ) ) ;
#6789 = FACE_OUTER_BOUND ( 'NONE', #55397, .T. ) ;
#6791 = ORIENTED_EDGE ( 'NONE', *, *, #55460, .T. ) ;
#6790 = EDGE_CURVE ( 'NONE', #11251, #13823, #49287, .T. ) ;
#6792 = ORIENTED_EDGE ( 'NONE', *, *, #18019, .T. ) ;
#6793 = CARTESIAN_POINT ( 'NONE',  ( 0.5809828226811553087, 18.83114015454698631, 44.03860873105701046 ) ) ;
#6794 = CARTESIAN_POINT ( 'NONE',  ( -2.708315649062910779, 2.171184472130682774, -14.47261168455367653 ) ) ;
#6796 = EDGE_CURVE ( 'NONE', #55475, #11923, #14926, .T. ) ;
#6795 = CARTESIAN_POINT ( 'NONE',  ( 0.9789889208857700531, 38.54554747982771801, -16.44918440296411077 ) ) ;
#6797 = CARTESIAN_POINT ( 'NONE',  ( 0.1100247026804066219, -5.460606496326611214, -42.77732815928598598 ) ) ;
#6798 = CARTESIAN_POINT ( 'NONE',  ( 0.5837800005270544768, -30.27739104966287087, -35.81221648917557587 ) ) ;
#6799 = CARTESIAN_POINT ( 'NONE',  ( 0.8760168074886960365, 5.394043284318862597, 47.80016357497251533 ) ) ;
#6800 = ORIENTED_EDGE ( 'NONE', *, *, #46870, .F. ) ;
#6801 = CARTESIAN_POINT ( 'NONE',  ( 4.962356264823603702, -20.60668162140254722, -36.69605251817282010 ) ) ;
#6802 = AXIS2_PLACEMENT_3D ( 'NONE', #35948, #32463, #17138 ) ;
#6803 = CARTESIAN_POINT ( 'NONE',  ( 5.719999999999999751, -15.71999999999998820, 1.925144768259638627E-15 ) ) ;
#6804 = VERTEX_POINT ( 'NONE', #40277 ) ;
#6805 = CONICAL_SURFACE ( 'NONE', #11873, 42.08604991992415023, 1.569615340895231137 ) ;
#6806 = B_SPLINE_CURVE_WITH_KNOTS ( 'NONE', 3,
 ( #35492, #39582, #16684, #30765, #1944, #31087, #54243, #44907, #15764, #21380, #58635, #40511, #34558, #45513, #20764, #34871, #2565, #16369, #25767 ),
 .UNSPECIFIED., .F., .F.,
 ( 4, 3, 3, 3, 3, 3, 4 ),
 ( 1.161276725443423652E-16, 0.0002618519381806260794, 0.0003927759815485985773, 0.0005237000248299448395, 0.0006546240681325003188, 0.0007855481115631321671, 0.0009699050456655092071 ),
 .UNSPECIFIED. ) ;
#6807 = CARTESIAN_POINT ( 'NONE',  ( 0.5837800005270558090, 36.80397537723558798, 29.06376876927043895 ) ) ;
#6808 = B_SPLINE_CURVE_WITH_KNOTS ( 'NONE', 3,
 ( #30063, #44204, #49172, #15680 ),
 .UNSPECIFIED., .F., .F.,
 ( 4, 4 ),
 ( 0.000000000000000000, 0.005014147105413699519 ),
 .UNSPECIFIED. ) ;
#6809 = CARTESIAN_POINT ( 'NONE',  ( 0.8551540677456715978, 43.91216198251539993, 19.17641535420869658 ) ) ;
#6810 = CARTESIAN_POINT ( 'NONE',  ( 0.1158403557922069033, -42.69064927979727742, 11.15566095097745425 ) ) ;
#6811 = CARTESIAN_POINT ( 'NONE',  ( 0.5850706913938533704, 44.31965802246131858, -18.16120156791832585 ) ) ;
#6812 = CARTESIAN_POINT ( 'NONE',  ( 4.553261556744875094, 31.39705178283641018, 30.72075365562384519 ) ) ;
#6813 = CARTESIAN_POINT ( 'NONE',  ( 0.1129192098497455998, 20.83764143887614040, -38.89401608281131928 ) ) ;
#6814 = CARTESIAN_POINT ( 'NONE',  ( 0.6001305935487315502, 44.64600790884055215, -17.92615948558493599 ) ) ;
#6815 = CARTESIAN_POINT ( 'NONE',  ( 2.528100132419517365, 19.10482268222866864, -37.37993484361196295 ) ) ;
#6816 = CARTESIAN_POINT ( 'NONE',  ( 0.9754292589017219406, 4.774020992617491466, 41.63575615330319835 ) ) ;
#6817 = VECTOR ( 'NONE', #52597, 1000.000000000000000 ) ;
#6818 = B_SPLINE_CURVE_WITH_KNOTS ( 'NONE', 3,
 ( #61751, #56755, #51434, #8222, #9155, #27340, #46467, #18890, #56143, #57061, #38010, #13881, #28261, #52061, #22964, #8528, #14190, #3512, #33295 ),
 .UNSPECIFIED., .F., .F.,
 ( 4, 3, 3, 3, 3, 3, 4 ),
 ( 0.000000000000000000, 0.0002724573126191728281, 0.0004086839781548461462, 0.0005449106435901787757, 0.0006811373090491435432, 0.0008459866663933707839, 0.001010840725717218570 ),
 .UNSPECIFIED. ) ;
#6819 = CARTESIAN_POINT ( 'NONE',  ( 0.9783242366443560822, 9.454269318224707064, 40.82831470762658910 ) ) ;
#6820 = EDGE_CURVE ( 'NONE', #4388, #2051, #24604, .T. ) ;
#6821 = CARTESIAN_POINT ( 'NONE',  ( 4.962356264823608143, 0.000000000000000000, 0.000000000000000000 ) ) ;
#6822 = CARTESIAN_POINT ( 'NONE',  ( 0.8744876279028306332, -8.712669995481570950, -48.31603700562917680 ) ) ;
#6823 = B_SPLINE_CURVE_WITH_KNOTS ( 'NONE', 3,
 ( #12983, #17355, #45880, #60238 ),
 .UNSPECIFIED., .F., .F.,
 ( 4, 4 ),
 ( 2.385244779468109755E-18, 0.004444878191957686922 ),
 .UNSPECIFIED. ) ;
#6824 = EDGE_CURVE ( 'NONE', #27931, #16986, #5107, .T. ) ;
#6825 = VERTEX_POINT ( 'NONE', #8480 ) ;
#6826 = B_SPLINE_CURVE_WITH_KNOTS ( 'NONE', 3,
 ( #11390, #10465, #44928, #34586, #20791, #15790 ),
 .UNSPECIFIED., .F., .F.,
 ( 4, 2, 4 ),
 ( 0.000000000000000000, 0.0002291459268755689880, 0.0004582918537511379759 ),
 .UNSPECIFIED. ) ;
#6827 = FACE_OUTER_BOUND ( 'NONE', #40406, .T. ) ;
#6828 = ADVANCED_FACE ( 'NONE', ( #12068 ), #41373, .F. ) ;
#6830 = EDGE_CURVE ( 'NONE', #4631, #25125, #56711, .T. ) ;
#6829 = B_SPLINE_CURVE_WITH_KNOTS ( 'NONE', 3,
 ( #55733, #12865, #31958, #51039 ),
 .UNSPECIFIED., .F., .F.,
 ( 4, 4 ),
 ( 0.000000000000000000, 0.005013413432710142441 ),
 .UNSPECIFIED. ) ;
#6831 = FACE_OUTER_BOUND ( 'NONE', #12213, .T. ) ;
#6832 = CARTESIAN_POINT ( 'NONE',  ( 0.9756008150404590351, -39.69644259322195978, -16.28894658522374073 ) ) ;
#6833 = CARTESIAN_POINT ( 'NONE',  ( 0.6021448801613057400, -45.41983169298476497, -18.67029800533144268 ) ) ;
#6834 = CARTESIAN_POINT ( 'NONE',  ( 0.1098349054025745952, -41.70974743324821787, 10.95525583467203745 ) ) ;
#6835 = EDGE_CURVE ( 'NONE', #53201, #2091, #28322, .T. ) ;
#6836 = ORIENTED_EDGE ( 'NONE', *, *, #56353, .T. ) ;
#6837 = CARTESIAN_POINT ( 'NONE',  ( 4.975801465491695552, 31.15993731089124097, -36.39623109580435312 ) ) ;
#6838 = CARTESIAN_POINT ( 'NONE',  ( 0.9756354156337460060, 16.54067710771413857, -39.59221474545846320 ) ) ;
#6839 = CARTESIAN_POINT ( 'NONE',  ( 0.5263152470540364281, 0.000000000000000000, 0.000000000000000000 ) ) ;
#6840 =( BOUNDED_SURFACE ( )  B_SPLINE_SURFACE ( 3, 1, ( 
 ( #18990, #33390 ),
 ( #38106, #4224 ),
 ( #56853, #33701 ),
 ( #28359, #57151 ) ),
 .UNSPECIFIED., .F., .F., .F. ) 
 B_SPLINE_SURFACE_WITH_KNOTS ( ( 4, 4 ),
 ( 2, 2 ),
 ( 0.000000000000000000, 1.000000000000000000 ),
 ( 0.000000000000000000, 1.000000000000000000 ),
 .UNSPECIFIED. ) 
 GEOMETRIC_REPRESENTATION_ITEM ( )  RATIONAL_B_SPLINE_SURFACE ( (
 ( 1.000000000000000000, 1.000000000000000000),
 ( 0.9953390228620291325, 0.8624445117761032620),
 ( 0.9953390228620291325, 0.8624445117761032620),
 ( 1.000000000000000000, 1.000000000000000000) ) ) 
 REPRESENTATION_ITEM ( '' )  SURFACE ( )  );
#6841 = ORIENTED_EDGE ( 'NONE', *, *, #21236, .T. ) ;
#6842 = EDGE_CURVE ( 'NONE', #22443, #10591, #50723, .T. ) ;
#6843 = CARTESIAN_POINT ( 'NONE',  ( 4.549368137175248350, 18.79584381673477012, 38.59302160394760506 ) ) ;
#6844 = ORIENTED_EDGE ( 'NONE', *, *, #45787, .T. ) ;
#6845 = AXIS2_PLACEMENT_3D ( 'NONE', #32994, #52067, #27966 ) ;
#6846 = CARTESIAN_POINT ( 'NONE',  ( 2.624215991343620935, -1.411420423865143325, -47.98682984381862582 ) ) ;
#6848 = CARTESIAN_POINT ( 'NONE',  ( 9.500000000000000000, 0.000000000000000000, -1.199999999999999956 ) ) ;
#6847 = AXIS2_PLACEMENT_3D ( 'NONE', #61578, #33732, #14010 ) ;
#6849 = ORIENTED_EDGE ( 'NONE', *, *, #50669, .T. ) ;
#6850 = DIRECTION ( 'NONE',  ( 1.000000000000000000, 0.000000000000000000, 0.000000000000000000 ) ) ;
#6851 = ORIENTED_EDGE ( 'NONE', *, *, #50571, .T. ) ;
#6852 = CARTESIAN_POINT ( 'NONE',  ( 4.553261556744873317, 1.182159483579998449, -43.91061448874312845 ) ) ;
#6853 = ORIENTED_EDGE ( 'NONE', *, *, #54148, .T. ) ;
#6854 = ORIENTED_EDGE ( 'NONE', *, *, #6578, .F. ) ;
#6855 = CARTESIAN_POINT ( 'NONE',  ( 0.9787464366903548818, 20.29559929315806954, -36.66636936242839084 ) ) ;
#6856 = B_SPLINE_CURVE_WITH_KNOTS ( 'NONE', 3,
 ( #39896, #1017, #29527, #39578, #53622, #58955 ),
 .UNSPECIFIED., .F., .F.,
 ( 4, 2, 4 ),
 ( 1.807478856737577690E-17, 0.0002293319059085094391, 0.0004586638118170007720 ),
 .UNSPECIFIED. ) ;
#6857 = CARTESIAN_POINT ( 'NONE',  ( 0.1158816050234199174, -1.408571594206387889, 44.10167760266219972 ) ) ;
#6858 = ORIENTED_EDGE ( 'NONE', *, *, #11690, .T. ) ;
#6859 = ORIENTED_EDGE ( 'NONE', *, *, #15356, .T. ) ;
#6860 = CARTESIAN_POINT ( 'NONE',  ( 2.618530812446115519, 37.74802994993038396, 28.01451452546264065 ) ) ;
#6861 = CARTESIAN_POINT ( 'NONE',  ( 0.5848930533535030563, -7.979791871079970456, -46.21250917318604223 ) ) ;
#6862 = CARTESIAN_POINT ( 'NONE',  ( 0.6024113833632039894, -25.27052062982265923, -42.10632560790092782 ) ) ;
#6863 = AXIS2_PLACEMENT_3D ( 'NONE', #23333, #47761, #37770 ) ;
#6864 = CARTESIAN_POINT ( 'NONE',  ( 0.1129192098497447394, -32.03190746134960420, -30.34647742609823595 ) ) ;
#6865 = CARTESIAN_POINT ( 'NONE',  ( 4.956445790444011124, -11.44166143951963122, -45.67960632101645757 ) ) ;
#6866 = EDGE_LOOP ( 'NONE', ( #52081, #37292, #53664, #26364 ) ) ;
#6867 = CARTESIAN_POINT ( 'NONE',  ( 3.238018933889920792, -8.855909537851408331, -10.04889837868039137 ) ) ;
#6868 = CARTESIAN_POINT ( 'NONE',  ( 5.901764892641307547, -48.86589420182298937, -3.180542610297919737 ) ) ;
#6869 = EDGE_LOOP ( 'NONE', ( #39580, #48031, #41890, #43013 ) ) ;
#6870 = CARTESIAN_POINT ( 'NONE',  ( 0.5835871038041854364, -46.78195124289987916, -3.268560969056623744 ) ) ;
#6871 = ORIENTED_EDGE ( 'NONE', *, *, #31573, .T. ) ;
#6872 = MECHANICAL_DESIGN_GEOMETRIC_PRESENTATION_REPRESENTATION (  '', ( #35892 ), #28889 ) ;
#6873 = DIRECTION ( 'NONE',  ( -1.000000000000000000, 0.000000000000000000, 0.000000000000000000 ) ) ;
#6875 = EDGE_CURVE ( 'NONE', #13708, #10594, #34331, .T. ) ;
#6874 = CARTESIAN_POINT ( 'NONE',  ( -6.078726893082806448, 13.83016815118539000, -13.39852567182887455 ) ) ;
#6876 = CARTESIAN_POINT ( 'NONE',  ( 0.5832655196449147983, -44.37535523958005257, 15.16782879433973541 ) ) ;
#6877 = ORIENTED_EDGE ( 'NONE', *, *, #42124, .F. ) ;
#6878 = CARTESIAN_POINT ( 'NONE',  ( 0.1104177457020373010, -42.75615561261997755, -5.624018123398488278 ) ) ;
#6879 = CARTESIAN_POINT ( 'NONE',  ( 0.6000166863083090663, 37.05402083933981316, -32.23077754796219807 ) ) ;
#6880 = LINE ( 'NONE', #53569, #57685 ) ;
#6881 = CARTESIAN_POINT ( 'NONE',  ( -20.07378285010853602, -12.50001391881583501, 0.1374748271822699153 ) ) ;
#6882 = ORIENTED_EDGE ( 'NONE', *, *, #58747, .T. ) ;
#6883 = DIRECTION ( 'NONE',  ( 0.9848077530122079093, 0.1736481776669314414, -5.551115123125783935E-17 ) ) ;
#6884 = ORIENTED_EDGE ( 'NONE', *, *, #33125, .F. ) ;
#6885 = CARTESIAN_POINT ( 'NONE',  ( -6.077587904424778920, 18.62786028128800098, -4.878405757493267103 ) ) ;
#6886 = CARTESIAN_POINT ( 'NONE',  ( 0.5997462898726536595, -25.90236585764231947, -41.72072714036939090 ) ) ;
#6887 = B_SPLINE_CURVE_WITH_KNOTS ( 'NONE', 3,
 ( #19195, #44787, #1511, #33910, #30339, #16565 ),
 .UNSPECIFIED., .F., .F.,
 ( 4, 2, 4 ),
 ( 1.029992063861229212E-18, 0.0002293801035737093720, 0.0004587602071474177140 ),
 .UNSPECIFIED. ) ;
#6888 = SURFACE_STYLE_FILL_AREA ( #2510 ) ;
#6889 = CARTESIAN_POINT ( 'NONE',  ( 2.624215991343608501, 17.05978231157404323, 44.87417713512093798 ) ) ;
#6890 = B_SPLINE_CURVE_WITH_KNOTS ( 'NONE', 3,
 ( #43322, #5969, #14804, #43951 ),
 .UNSPECIFIED., .F., .F.,
 ( 4, 4 ),
 ( 0.000000000000000000, 0.004447772540403797242 ),
 .UNSPECIFIED. ) ;
#6891 = VERTEX_POINT ( 'NONE', #56405 ) ;
#6892 = CARTESIAN_POINT ( 'NONE',  ( 4.956445790443998689, -23.10347171912865250, 41.03373788314999615 ) ) ;
#6893 = CARTESIAN_POINT ( 'NONE',  ( 0.7764139734771222656, 43.52296024007050335, -17.48692090815614364 ) ) ;
#6894 = CARTESIAN_POINT ( 'NONE',  ( -6.000000000000003553, 15.14599999999999902, 0.000000000000000000 ) ) ;
#6895 = CARTESIAN_POINT ( 'NONE',  ( 5.960221823109900008, 20.35070456576734443, -2.673723662181125338 ) ) ;
#6896 = CARTESIAN_POINT ( 'NONE',  ( 4.694002226626920127, 23.92658369670189700, 38.80468224391037069 ) ) ;
#6897 = EDGE_CURVE ( 'NONE', #22282, #48887, #3778, .T. ) ;
#6898 = CARTESIAN_POINT ( 'NONE',  ( 5.894904586330512508, 5.960138742492302022, -19.20953300400311647 ) ) ;
#6899 = DIRECTION ( 'NONE',  ( -1.000000000000000000, -0.000000000000000000, -0.000000000000000000 ) ) ;
#6900 = ADVANCED_FACE ( 'NONE', ( #37038 ), #19403, .F. ) ;
#6901 = EDGE_CURVE ( 'NONE', #8188, #28286, #45543, .T. ) ;
#6902 = LINE ( 'NONE', #22579, #49253 ) ;
#6903 = LINE ( 'NONE', #20725, #29183 ) ;
#6904 = ORIENTED_EDGE ( 'NONE', *, *, #59662, .F. ) ;
#6905 = ADVANCED_FACE ( 'NONE', ( #47043 ), #18830, .T. ) ;
#6906 = CIRCLE ( 'NONE', #31942, 2.649999999999997691 ) ;
#6907 = CARTESIAN_POINT ( 'NONE',  ( 3.238741278300272697, -41.01623499586005295, -12.88350628398725917 ) ) ;
#6908 = CARTESIAN_POINT ( 'NONE',  ( 0.5819845901640492425, 46.14435291605029477, 12.83441129068549813 ) ) ;
#6909 = LINE ( 'NONE', #59544, #31718 ) ;
#6910 = ADVANCED_FACE ( 'NONE', ( #28217 ), #4381, .T. ) ;
#6911 = ORIENTED_EDGE ( 'NONE', *, *, #19731, .T. ) ;
#6912 = CARTESIAN_POINT ( 'NONE',  ( -6.077587904424778920, -18.89978312007031391, -3.687033958107209131 ) ) ;
#6913 = PLANE ( 'NONE',  #53928 ) ;
#6914 = FACE_OUTER_BOUND ( 'NONE', #40112, .T. ) ;
#6915 = ORIENTED_EDGE ( 'NONE', *, *, #33643, .F. ) ;
#6916 = CARTESIAN_POINT ( 'NONE',  ( 5.860006189529234355, -26.81109398084681317, -40.09484204000627017 ) ) ;
#6917 = CARTESIAN_POINT ( 'NONE',  ( -2.569797478183783568, -14.44232325624828306, 2.353985772484507244 ) ) ;
#6919 = ORIENTED_EDGE ( 'NONE', *, *, #21014, .F. ) ;
#6918 =( BOUNDED_SURFACE ( )  B_SPLINE_SURFACE ( 3, 1, ( 
 ( #58691, #18747 ),
 ( #23130, #19917 ),
 ( #39028, #58083 ),
 ( #61319, #15818 ) ),
 .UNSPECIFIED., .F., .F., .F. ) 
 B_SPLINE_SURFACE_WITH_KNOTS ( ( 4, 4 ),
 ( 2, 2 ),
 ( 0.000000000000000000, 1.000000000000000000 ),
 ( 0.000000000000000000, 1.000000000000000000 ),
 .UNSPECIFIED. ) 
 GEOMETRIC_REPRESENTATION_ITEM ( )  RATIONAL_B_SPLINE_SURFACE ( (
 ( 1.000000000000000000, 1.000000000000000000),
 ( 0.7223157951917476005, 0.9931996967497186413),
 ( 0.7223157951917476005, 0.9931996967497186413),
 ( 1.000000000000000000, 1.000000000000000000) ) ) 
 REPRESENTATION_ITEM ( '' )  SURFACE ( )  );
#6920 = ADVANCED_FACE ( 'NONE', ( #58246 ), #3814, .F. ) ;
#6921 = CARTESIAN_POINT ( 'NONE',  ( 5.959547316686252039, 12.49238070347954555, 16.28624005235103311 ) ) ;
#6922 = B_SPLINE_CURVE_WITH_KNOTS ( 'NONE', 3,
 ( #17600, #7241, #41123, #18222 ),
 .UNSPECIFIED., .F., .F.,
 ( 4, 4 ),
 ( 2.122407100861210359E-17, 0.004444306975806114161 ),
 .UNSPECIFIED. ) ;
#6923 = EDGE_LOOP ( 'NONE', ( #41248, #16299, #14838, #40828 ) ) ;
#6924 = EDGE_LOOP ( 'NONE', ( #32609, #61839, #7403, #56997 ) ) ;
#6925 = CARTESIAN_POINT ( 'NONE',  ( 0.1129192098497455998, 43.99990943031669843, 3.310552508129313232 ) ) ;
#6927 = ORIENTED_EDGE ( 'NONE', *, *, #38793, .F. ) ;
#6926 = EDGE_CURVE ( 'NONE', #25242, #8101, #56710, .T. ) ;
#6928 = CARTESIAN_POINT ( 'NONE',  ( 4.335381028904216727, 20.75278752742130450, -44.37430176922282499 ) ) ;
#6929 = CARTESIAN_POINT ( 'NONE',  ( 0.9762797500689124330, -17.18051571332090788, -38.22505284509149703 ) ) ;
#6930 = ORIENTED_EDGE ( 'NONE', *, *, #12981, .F. ) ;
#6931 = CARTESIAN_POINT ( 'NONE',  ( 0.1100053167205930910, 0.1794603581038460294, 43.12409768020066281 ) ) ;
#6932 = VECTOR ( 'NONE', #7544, 1000.000000000000000 ) ;
#6933 = FACE_OUTER_BOUND ( 'NONE', #1255, .T. ) ;
#6934 = EDGE_LOOP ( 'NONE', ( #37729, #6720, #9035, #33413 ) ) ;
#6935 = CARTESIAN_POINT ( 'NONE',  ( 0.1157991065609915715, 43.32597169134096760, -8.354791591585023269 ) ) ;
#6936 = VECTOR ( 'NONE', #18674, 999.9999999999998863 ) ;
#6937 = LINE ( 'NONE', #45508, #52531 ) ;
#6938 = CARTESIAN_POINT ( 'NONE',  ( 0.1103878639767399694, -30.45925431905134317, 30.52789484587400892 ) ) ;
#6939 = CARTESIAN_POINT ( 'NONE',  ( 0.9789889208857709413, 36.10718377573707016, 21.27454295225910741 ) ) ;
#6940 = ORIENTED_EDGE ( 'NONE', *, *, #12526, .F. ) ;
#6941 = ORIENTED_EDGE ( 'NONE', *, *, #28990, .T. ) ;
#6942 = CARTESIAN_POINT ( 'NONE',  ( 5.959547316686252039, 10.25972575517530139, -17.77749189599207114 ) ) ;
#6943 = CARTESIAN_POINT ( 'NONE',  ( -6.010958268070873523, -16.31164801516935370, -9.434296419346379636 ) ) ;
#6944 = EDGE_CURVE ( 'NONE', #14392, #41383, #25331, .T. ) ;
#6945 = CARTESIAN_POINT ( 'NONE',  ( 0.8751705887134553219, 0.8911681664081729792, 48.08707113907595243 ) ) ;
#6946 = EDGE_LOOP ( 'NONE', ( #22828, #2607, #48957, #16108 ) ) ;
#6947 = CARTESIAN_POINT ( 'NONE',  ( 0.3676999524040366896, -42.87209381266877983, -10.38913641457107673 ) ) ;
#6948 = DIRECTION ( 'NONE',  ( 0.09722883295013594329, 0.7627152102960286228, 0.6393841271303498663 ) ) ;
#6949 = DIRECTION ( 'NONE',  ( -1.000000000000000000, -0.000000000000000000, -0.000000000000000000 ) ) ;
#6950 = CARTESIAN_POINT ( 'NONE',  ( 0.7057020205115069889, 29.82342581815259308, -37.48480537461301054 ) ) ;
#6951 = VECTOR ( 'NONE', #24331, 1000.000000000000114 ) ;
#6952 = ORIENTED_EDGE ( 'NONE', *, *, #42667, .F. ) ;
#6953 = ORIENTED_EDGE ( 'NONE', *, *, #35792, .F. ) ;
#6954 = CARTESIAN_POINT ( 'NONE',  ( 4.975801465491694664, 26.14269827151623105, 40.15204426031542795 ) ) ;
#6955 = FACE_OUTER_BOUND ( 'NONE', #18450, .T. ) ;
#6956 = CARTESIAN_POINT ( 'NONE',  ( 0.1081432562775997558, -40.00205417854824219, 16.11101151263754616 ) ) ;
#6957 = CARTESIAN_POINT ( 'NONE',  ( 0.5987334308729319599, -49.10393657821489910, 0.6052430027486100927 ) ) ;
#6958 = CARTESIAN_POINT ( 'NONE',  ( 4.390527457369401532, -41.59349320486530388, -14.14802670500178827 ) ) ;
#6959 = CARTESIAN_POINT ( 'NONE',  ( 0.5850706913938533704, -44.18063951072207374, -18.49682194438010896 ) ) ;
#6960 = DIRECTION ( 'NONE',  ( 0.000000000000000000, 0.000000000000000000, -1.000000000000000000 ) ) ;
#6961 = CARTESIAN_POINT ( 'NONE',  ( 4.967162193818131399, -42.34252806656588319, -7.970725651240238463 ) ) ;
#6962 = FACE_OUTER_BOUND ( 'NONE', #60959, .T. ) ;
#6963 = CARTESIAN_POINT ( 'NONE',  ( 0.5809828226811553087, 0.5448590168532381206, 47.89273459658653564 ) ) ;
#6964 = CARTESIAN_POINT ( 'NONE',  ( 4.549368137175248350, -42.06008734272402450, 8.582197505783685898 ) ) ;
#6965 = CARTESIAN_POINT ( 'NONE',  ( 0.1073791018717483448, -11.62916352156123168, -41.52698815987163528 ) ) ;
#6966 = CARTESIAN_POINT ( 'NONE',  ( 0.7413678028165010536, 41.54644801266331200, -14.77764356388756006 ) ) ;
#6967 = CARTESIAN_POINT ( 'NONE',  ( 4.553261556744873317, -24.94552653848474222, 36.15605442441679429 ) ) ;
#6968 = DIRECTION ( 'NONE',  ( 0.09835009131224552170, 0.9876177374393958486, 0.1222230102475044128 ) ) ;
#6969 = CARTESIAN_POINT ( 'NONE',  ( 0.6017666602106490625, -6.625262199740747704, -47.64919188470826583 ) ) ;
#6970 = B_SPLINE_CURVE_WITH_KNOTS ( 'NONE', 3,
 ( #36634, #61629, #41643, #8106, #56325, #4003, #51628, #47257, #23141, #60708, #32237, #60396, #42270, #4306, #12835, #23444, #61028, #8720, #27524 ),
 .UNSPECIFIED., .F., .F.,
 ( 4, 3, 3, 3, 3, 3, 4 ),
 ( 1.165802754517233128E-16, 0.0002618519381806274889, 0.0003927759815485978726, 0.0005237000248299410448, 0.0006546240681324946810, 0.0007855481115631296734, 0.0009699050456655074724 ),
 .UNSPECIFIED. ) ;
#6971 = DIRECTION ( 'NONE',  ( -1.000000000000000000, -0.000000000000000000, -0.000000000000000000 ) ) ;
#6972 = ADVANCED_FACE ( 'NONE', ( #34174 ), #38614, .F. ) ;
#6973 = CARTESIAN_POINT ( 'NONE',  ( 0.5997462898726536595, 17.44942740672405534, 45.90282249842351803 ) ) ;
#6974 = FACE_OUTER_BOUND ( 'NONE', #43433, .T. ) ;
#6976 = VERTEX_POINT ( 'NONE', #48265 ) ;
#6975 = CARTESIAN_POINT ( 'NONE',  ( 0.3622758884714730732, 43.10531414739106282, -0.8252992914323589169 ) ) ;
#6977 = ORIENTED_EDGE ( 'NONE', *, *, #33888, .F. ) ;
#6978 = CARTESIAN_POINT ( 'NONE',  ( 3.660176727303405375, -46.85282580473587899, 10.60619300811855403 ) ) ;
#6979 = CARTESIAN_POINT ( 'NONE',  ( 2.533389852662419894, 2.648867642851640003, -43.93670483712077157 ) ) ;
#6980 = CARTESIAN_POINT ( 'NONE',  ( 5.880360259849752858, 36.03610316515339917, 31.66572319753574405 ) ) ;
#6981 = EDGE_CURVE ( 'NONE', #47520, #46817, #20077, .T. ) ;
#6982 = ORIENTED_EDGE ( 'NONE', *, *, #21171, .T. ) ;
#6983 = VERTEX_POINT ( 'NONE', #57941 ) ;
#6984 = CARTESIAN_POINT ( 'NONE',  ( 0.3676999524040366896, -7.853951980431815194, -43.40813312746713848 ) ) ;
#6985 = CARTESIAN_POINT ( 'NONE',  ( 4.975610109902397937, 48.58133226360775581, 5.683622315980952244 ) ) ;
#6986 = CARTESIAN_POINT ( 'NONE',  ( 0.5786265663353153954, -13.09387673186302870, -46.07681357296498703 ) ) ;
#6988 = VERTEX_POINT ( 'NONE', #52321 ) ;
#6987 = AXIS2_PLACEMENT_3D ( 'NONE', #39483, #24122, #48251 ) ;
#6989 = ORIENTED_EDGE ( 'NONE', *, *, #1739, .F. ) ;
#6990 = B_SPLINE_CURVE_WITH_KNOTS ( 'NONE', 3,
 ( #18780, #33188, #47901, #52889, #42907, #52263, #34119, #53191, #9359, #58191, #14086, #37907, #56964, #28461, #10295, #47588, #29696, #4626, #39131 ),
 .UNSPECIFIED., .F., .F.,
 ( 4, 3, 3, 3, 3, 3, 4 ),
 ( 0.000000000000000000, 0.0002612768053151736064, 0.0003919133833142934733, 0.0005225499612322633556, 0.0006531865391693374764, 0.0008112755173415215921, 0.0009693688056799695373 ),
 .UNSPECIFIED. ) ;
#6991 = CARTESIAN_POINT ( 'NONE',  ( 4.960386119450149955, -37.40422633003205988, -22.70154878690168587 ) ) ;
#6992 = AXIS2_PLACEMENT_3D ( 'NONE', #54101, #59743, #11222 ) ;
#6993 = CARTESIAN_POINT ( 'NONE',  ( 4.967162193818131399, -3.259922920618036901, 42.96271701169384016 ) ) ;
#6994 = CARTESIAN_POINT ( 'NONE',  ( -6.016761891674565099, 2.456125503350710115, 18.68243340030203470 ) ) ;
#6995 = VERTEX_POINT ( 'NONE', #19451 ) ;
#6996 = EDGE_CURVE ( 'NONE', #219, #61755, #53252, .T. ) ;
#6997 = DIRECTION ( 'NONE',  ( -0.5000000000000051070, 0.000000000000000000, 0.8660254037844355990 ) ) ;
#6998 = B_SPLINE_CURVE_WITH_KNOTS ( 'NONE', 3,
 ( #43788, #19965, #6118, #34365, #53135, #34991 ),
 .UNSPECIFIED., .F., .F.,
 ( 4, 2, 4 ),
 ( 1.272149902321906704E-16, 0.0002450741128632372211, 0.0004901482257263471568 ),
 .UNSPECIFIED. ) ;
#6999 = CARTESIAN_POINT ( 'NONE',  ( -6.016489644550737204, 18.84320342686341121, 0.004404229197842324944 ) ) ;
#7000 = CARTESIAN_POINT ( 'NONE',  ( 0.9736507210033064075, 42.48017254354723349, 6.046964561328082688 ) ) ;
#7001 = VERTEX_POINT ( 'NONE', #47958 ) ;
#7002 = EDGE_LOOP ( 'NONE', ( #50884, #51629, #32003, #21627 ) ) ;
#7003 = CARTESIAN_POINT ( 'NONE',  ( -2.601141883200665639, -3.815535891687811709, -14.43042318605489527 ) ) ;
#7004 = CARTESIAN_POINT ( 'NONE',  ( -2.708315649062910779, -14.06540004355479923, -4.041664582652747306 ) ) ;
#7005 = ORIENTED_EDGE ( 'NONE', *, *, #15232, .F. ) ;
#7006 = CARTESIAN_POINT ( 'NONE',  ( 4.962356264823608143, 0.000000000000000000, 0.000000000000000000 ) ) ;
#7007 = CARTESIAN_POINT ( 'NONE',  ( 4.956445790443996913, 2.113652668516264654, 47.04328350079860854 ) ) ;
#7008 = CARTESIAN_POINT ( 'NONE',  ( 0.5848930533535030563, 27.96442382265459514, 37.64656800632039335 ) ) ;
#7009 = CARTESIAN_POINT ( 'NONE',  ( 3.727782113643637096, -43.82423448898260432, -3.494888747963610598 ) ) ;
#7010 = VERTEX_POINT ( 'NONE', #15066 ) ;
#7011 = CARTESIAN_POINT ( 'NONE',  ( 0.9757787079277437936, -30.31292661677473887, -30.36877398309933440 ) ) ;
#7012 = CARTESIAN_POINT ( 'NONE',  ( 0.6026112563231247332, -35.39723702811621564, 34.03787016955622136 ) ) ;
#7013 = B_SPLINE_CURVE_WITH_KNOTS ( 'NONE', 3,
 ( #20025, #1487, #39757, #25622, #39137, #35356, #58810, #44759, #10611, #11227, #30316, #54412, #49737, #1799, #40073, #6793 ),
 .UNSPECIFIED., .F., .F.,
 ( 4, 3, 3, 3, 3, 4 ),
 ( 1.250973872328959318E-17, 0.0002724568934985550049, 0.0004086836638483800927, 0.0005449104342063564293, 0.0008173270854453635291, 0.001089761613562688575 ),
 .UNSPECIFIED. ) ;
#7014 =( BOUNDED_SURFACE ( )  B_SPLINE_SURFACE ( 3, 1, ( 
 ( #39085, #14341 ),
 ( #5512, #33449 ),
 ( #14651, #47537 ),
 ( #38459, #9618 ) ),
 .UNSPECIFIED., .F., .F., .F. ) 
 B_SPLINE_SURFACE_WITH_KNOTS ( ( 4, 4 ),
 ( 2, 2 ),
 ( 0.000000000000000000, 1.000000000000000000 ),
 ( 0.000000000000000000, 1.000000000000000000 ),
 .UNSPECIFIED. ) 
 GEOMETRIC_REPRESENTATION_ITEM ( )  RATIONAL_B_SPLINE_SURFACE ( (
 ( 1.000000000000000000, 1.000000000000000000),
 ( 0.9732289882329797637, 0.9999525324661233672),
 ( 0.9732289882329797637, 0.9999525324661233672),
 ( 1.000000000000000000, 1.000000000000000000) ) ) 
 REPRESENTATION_ITEM ( '' )  SURFACE ( )  );
#7015 = CARTESIAN_POINT ( 'NONE',  ( 4.967162193818130511, 19.45289607368822615, 38.44485641567079881 ) ) ;
#7016 = CARTESIAN_POINT ( 'NONE',  ( 0.8554163680231816613, 44.99993935735625428, -13.27444654010398573 ) ) ;
#7017 = B_SPLINE_CURVE_WITH_KNOTS ( 'NONE', 3,
 ( #38996, #58052, #4501, #32743 ),
 .UNSPECIFIED., .F., .F.,
 ( 4, 4 ),
 ( 7.589415207398531038E-19, 0.004444878191957689524 ),
 .UNSPECIFIED. ) ;
#7018 = EDGE_CURVE ( 'NONE', #25568, #20738, #34214, .T. ) ;
#7019 = VERTEX_POINT ( 'NONE', #37864 ) ;
#7020 = FACE_OUTER_BOUND ( 'NONE', #56354, .T. ) ;
#7021 = CARTESIAN_POINT ( 'NONE',  ( 4.975801465491695552, 47.84403947906839960, 2.564218696447662982 ) ) ;
#7022 = CARTESIAN_POINT ( 'NONE',  ( 0.6067375320500720814, 33.36326114377818897, 34.36594163291719894 ) ) ;
#7023 = CARTESIAN_POINT ( 'NONE',  ( -6.015611763856276717, -4.882992715191428523, 18.19956619163656697 ) ) ;
#7024 = CONICAL_SURFACE ( 'NONE', #50073, 43.08621763946400307, 1.568696531533066763 ) ;
#7025 = ORIENTED_EDGE ( 'NONE', *, *, #60749, .F. ) ;
#7026 = CARTESIAN_POINT ( 'NONE',  ( 0.2285344041767103374, -11.82284706221704695, 42.50554619857131655 ) ) ;
#7027 = CARTESIAN_POINT ( 'NONE',  ( 0.1100053167205930910, -42.73174076921948483, 5.806749312984397449 ) ) ;
#7028 = CARTESIAN_POINT ( 'NONE',  ( 0.1064266379913941657, -22.04679939086809171, -37.06314005629904784 ) ) ;
#7029 = EDGE_CURVE ( 'NONE', #16747, #40146, #12849, .T. ) ;
#7030 = CARTESIAN_POINT ( 'NONE',  ( 0.6023142530420679819, -41.53076277789759274, 24.28014345169096799 ) ) ;
#7031 = DIRECTION ( 'NONE',  ( 0.000000000000000000, 0.000000000000000000, -1.000000000000000000 ) ) ;
#7032 =( BOUNDED_SURFACE ( )  B_SPLINE_SURFACE ( 3, 1, ( 
 ( #39574, #58627 ),
 ( #30137, #49249 ),
 ( #30441, #25136 ),
 ( #5692, #44278 ) ),
 .UNSPECIFIED., .F., .F., .F. ) 
 B_SPLINE_SURFACE_WITH_KNOTS ( ( 4, 4 ),
 ( 2, 2 ),
 ( 0.000000000000000000, 1.000000000000000000 ),
 ( 0.000000000000000000, 1.000000000000000000 ),
 .UNSPECIFIED. ) 
 GEOMETRIC_REPRESENTATION_ITEM ( )  RATIONAL_B_SPLINE_SURFACE ( (
 ( 1.000000000000000000, 1.000000000000000000),
 ( 0.9952954269826590483, 0.8620686068821307169),
 ( 0.9952954269826590483, 0.8620686068821307169),
 ( 1.000000000000000000, 1.000000000000000000) ) ) 
 REPRESENTATION_ITEM ( '' )  SURFACE ( )  );
#7033 = VECTOR ( 'NONE', #16353, 1000.000000000000000 ) ;
#7034 = CARTESIAN_POINT ( 'NONE',  ( 0.9740398440564311811, 42.90647580953695694, -0.4145941695174525932 ) ) ;
#7035 = CARTESIAN_POINT ( 'NONE',  ( 4.335381028904216727, 47.11764506933879915, 13.40463989759361674 ) ) ;
#7036 = CARTESIAN_POINT ( 'NONE',  ( 4.967162193818130511, 36.06913038482799294, 23.56777426397191277 ) ) ;
#7037 = EDGE_CURVE ( 'NONE', #32714, #17539, #42433, .T. ) ;
#7038 = CARTESIAN_POINT ( 'NONE',  ( 0.1073791018717483448, 21.98088480513615295, 37.10214135362896570 ) ) ;
#7039 = CARTESIAN_POINT ( 'NONE',  ( -2.569797478183783568, 7.701637110048508816, 12.44213550320655948 ) ) ;
#7040 = ORIENTED_EDGE ( 'NONE', *, *, #38708, .T. ) ;
#7041 = CARTESIAN_POINT ( 'NONE',  ( 0.8560838555295158248, -46.73345513967312570, -4.044379407262746362 ) ) ;
#7042 = CARTESIAN_POINT ( 'NONE',  ( 0.5806925824938490299, 46.40146083665128174, 6.791670970260652140 ) ) ;
#7043 = CARTESIAN_POINT ( 'NONE',  ( 1.231276596079881047, -35.03243822710529543, 23.02183839058294623 ) ) ;
#7044 = CARTESIAN_POINT ( 'NONE',  ( 0.1147471544378677460, 44.01263920499553706, -3.136842151612880603 ) ) ;
#7045 = CARTESIAN_POINT ( 'NONE',  ( 5.959547316686252039, -17.77749189599224877, 10.25972575517499052 ) ) ;
#7046 = B_SPLINE_CURVE_WITH_KNOTS ( 'NONE', 3,
 ( #59499, #60123, #36653, #8417 ),
 .UNSPECIFIED., .F., .F.,
 ( 4, 4 ),
 ( 0.000000000000000000, 0.005014147105413698652 ),
 .UNSPECIFIED. ) ;
#7047 = CARTESIAN_POINT ( 'NONE',  ( 2.618530812446115519, -46.32565728282589390, -7.978738403554839209 ) ) ;
#7048 = DIRECTION ( 'NONE',  ( -1.286342699658459486E-16, 0.7042738517259728992, -0.7099284060911089655 ) ) ;
#7049 = LINE ( 'NONE', #32128, #11900 ) ;
#7050 = FACE_OUTER_BOUND ( 'NONE', #53319, .T. ) ;
#7051 = EDGE_CURVE ( 'NONE', #55688, #53648, #4286, .T. ) ;
#7052 = CARTESIAN_POINT ( 'NONE',  ( 0.3622758884714600280, -6.444611261694905835, 42.62881903538198713 ) ) ;
#7054 = ORIENTED_EDGE ( 'NONE', *, *, #41406, .F. ) ;
#7053 = DIRECTION ( 'NONE',  ( -1.000000000000000000, -0.000000000000000000, -0.000000000000000000 ) ) ;
#7055 = ORIENTED_EDGE ( 'NONE', *, *, #24347, .F. ) ;
#7056 = CARTESIAN_POINT ( 'NONE',  ( 0.2885697896453132127, -34.69058521462552847, 25.60460893337419108 ) ) ;
#7057 = CARTESIAN_POINT ( 'NONE',  ( 0.1129192098497455998, 41.72114954716776936, 14.36305915353748297 ) ) ;
#7058 = EDGE_CURVE ( 'NONE', #26555, #48631, #44866, .T. ) ;
#7059 = ORIENTED_EDGE ( 'NONE', *, *, #29923, .F. ) ;
#7060 = LINE ( 'NONE', #45950, #28487 ) ;
#7061 = CARTESIAN_POINT ( 'NONE',  ( 0.5819845079324663661, -47.42480735454290652, 6.701571823032553610 ) ) ;
#7062 = CARTESIAN_POINT ( 'NONE',  ( 4.967162193818130511, 0.000000000000000000, 0.000000000000000000 ) ) ;
#7063 = EDGE_CURVE ( 'NONE', #8350, #28177, #54367, .T. ) ;
#7064 = ORIENTED_EDGE ( 'NONE', *, *, #41694, .F. ) ;
#7065 = EDGE_LOOP ( 'NONE', ( #18356, #4618, #54164, #30424 ) ) ;
#7066 = CARTESIAN_POINT ( 'NONE',  ( 0.1073791018717578927, -25.86618856530687793, -34.50606437925538472 ) ) ;
#7067 = B_SPLINE_CURVE_WITH_KNOTS ( 'NONE', 3,
 ( #46820, #48035, #14224, #27997, #47119, #52715, #18925, #9496, #28602, #9812, #5084, #57392, #8564, #47417, #19231, #3859 ),
 .UNSPECIFIED., .F., .F.,
 ( 4, 3, 3, 3, 3, 4 ),
 ( 2.194378057379452319E-17, 0.0002612764279487727833, 0.0003919131003184789198, 0.0005225497727000618948, 0.0007837925190632441617, 0.001045051706266715216 ),
 .UNSPECIFIED. ) ;
#7068 = LINE ( 'NONE', #40641, #35246 ) ;
#7069 = CARTESIAN_POINT ( 'NONE',  ( 5.981074661064941900, 7.862380442164140781, -18.95903134304781190 ) ) ;
#7070 = ORIENTED_EDGE ( 'NONE', *, *, #44702, .T. ) ;
#7071 = ADVANCED_FACE ( 'NONE', ( #55998 ), #61006, .T. ) ;
#7072 = ORIENTED_EDGE ( 'NONE', *, *, #49993, .T. ) ;
#7073 = CARTESIAN_POINT ( 'NONE',  ( 4.962356264823608143, 0.9708976703217077064, 42.07484944210865052 ) ) ;
#7074 = CARTESIAN_POINT ( 'NONE',  ( 0.8751705887134423323, 0.8911681664088411114, -48.08707113907595243 ) ) ;
#7075 = EDGE_LOOP ( 'NONE', ( #36120, #35842, #58112, #6391 ) ) ;
#7076 = VECTOR ( 'NONE', #13958, 1000.000000000000000 ) ;
#7077 = CARTESIAN_POINT ( 'NONE',  ( 42.00000000000000711, 1.592040838891559293E-15, -13.00000000000000178 ) ) ;
#7078 = CARTESIAN_POINT ( 'NONE',  ( 0.9749527285493314599, 41.51939261707898510, -10.82939760924460515 ) ) ;
#7079 = ORIENTED_EDGE ( 'NONE', *, *, #52702, .T. ) ;
#7080 = CARTESIAN_POINT ( 'NONE',  ( 5.974727161628369032, -5.297264154380800782, -19.82959049719573841 ) ) ;
#7081 = CARTESIAN_POINT ( 'NONE',  ( 5.958863334805807099, -0.001220270596312466932, 20.52565293643016275 ) ) ;
#7082 = VERTEX_POINT ( 'NONE', #56306 ) ;
#7083 = CARTESIAN_POINT ( 'NONE',  ( -6.057079549204054558, -11.02420820863788187, 15.78917554758130848 ) ) ;
#7084 = CARTESIAN_POINT ( 'NONE',  ( 0.5824935313925952984, -19.40916258553593821, 42.69101292757142119 ) ) ;
#7085 = CARTESIAN_POINT ( 'NONE',  ( 3.783278058412225864, 31.62921638229668275, 29.18720354295055230 ) ) ;
#7086 = ORIENTED_EDGE ( 'NONE', *, *, #43887, .F. ) ;
#7087 = CARTESIAN_POINT ( 'NONE',  ( 0.7762783648524406166, -33.23866576554864594, 34.49689442177335508 ) ) ;
#7088 = CARTESIAN_POINT ( 'NONE',  ( 0.1156495703730067437, 39.69517360536710271, -19.26748934528932722 ) ) ;
#7089 = VERTEX_POINT ( 'NONE', #56617 ) ;
#7090 = CARTESIAN_POINT ( 'NONE',  ( 0.2885697896453108813, -31.05173034173391855, 29.91358794843008440 ) ) ;
#7091 = B_SPLINE_CURVE_WITH_KNOTS ( 'NONE', 3,
 ( #42490, #52163, #48099, #18994 ),
 .UNSPECIFIED., .F., .F.,
 ( 4, 4 ),
 ( 1.226634733346699156E-18, 0.004042984057420973693 ),
 .UNSPECIFIED. ) ;
#7092 = EDGE_LOOP ( 'NONE', ( #8178, #2722, #52249, #42094 ) ) ;
#7093 = CARTESIAN_POINT ( 'NONE',  ( 5.960721111146673579, -14.50930005615026808, 14.51823969584074625 ) ) ;
#7094 = EDGE_LOOP ( 'NONE', ( #11073, #38148, #13086, #24967 ) ) ;
#7095 = CARTESIAN_POINT ( 'NONE',  ( 4.958415959904818315, -22.27126879049734143, -39.58780797523473893 ) ) ;
#7096 = CARTESIAN_POINT ( 'NONE',  ( 0.9789889208857696090, 24.93672124877021901, 33.68226286049529250 ) ) ;
#7097 = DIRECTION ( 'NONE',  ( 0.1305261922200468827, -0.9914448613738110483, 0.000000000000000000 ) ) ;
#7098 = VERTEX_POINT ( 'NONE', #23734 ) ;
#7099 = CARTESIAN_POINT ( 'NONE',  ( 0.1149546198390367091, -27.29633129785849022, -34.66780729582952603 ) ) ;
#7100 = EDGE_CURVE ( 'NONE', #61755, #46275, #19545, .T. ) ;
#7101 = CARTESIAN_POINT ( 'NONE',  ( 1.399999999999999467, 0.000000000000000000, 0.000000000000000000 ) ) ;
#7102 = CARTESIAN_POINT ( 'NONE',  ( -6.015611763856276717, -14.94556629257417590, -11.47596948473826650 ) ) ;
#7103 = EDGE_LOOP ( 'NONE', ( #32035, #49413, #2186, #46245 ) ) ;
#7104 = EDGE_CURVE ( 'NONE', #41282, #21198, #40231, .T. ) ;
#7105 = ORIENTED_EDGE ( 'NONE', *, *, #29261, .F. ) ;
#7106 = CARTESIAN_POINT ( 'NONE',  ( 0.3676999524040323597, 29.04098611012938136, 33.20499524279608750 ) ) ;
#7107 = CARTESIAN_POINT ( 'NONE',  ( 3.390910168358337806, 30.99541111418804107, 31.19906451155395644 ) ) ;
#7108 = CARTESIAN_POINT ( 'NONE',  ( 0.6016117650947689910, 33.27209104220542457, 36.11812580857002786 ) ) ;
#7109 = CARTESIAN_POINT ( 'NONE',  ( 0.2224561200757624035, 41.84032767736802327, -10.42482236669260054 ) ) ;
#7110 = CARTESIAN_POINT ( 'NONE',  ( -2.000000000000009770, 3.464101615137749057, 0.000000000000000000 ) ) ;
#7111 = CARTESIAN_POINT ( 'NONE',  ( 5.959547316686252039, -19.82530672674365846, 5.315863417545987346 ) ) ;
#7112 = EDGE_LOOP ( 'NONE', ( #37948, #58035, #21921, #45166 ) ) ;
#7113 = ADVANCED_FACE ( 'NONE', ( #32845 ), #45032, .F. ) ;
#7114 = CARTESIAN_POINT ( 'NONE',  ( 0.5782707292762423457, 28.40044722094901886, 37.32493739254906728 ) ) ;
#7115 = CARTESIAN_POINT ( 'NONE',  ( 2.281351352603284699, -28.15073776031340813, -38.84542754822352606 ) ) ;
#7116 = VERTEX_POINT ( 'NONE', #15272 ) ;
#7117 = CARTESIAN_POINT ( 'NONE',  ( 5.960721111146673579, -17.77250458025985225, -10.26825948882919626 ) ) ;
#7118 = CARTESIAN_POINT ( 'NONE',  ( 4.956653778116982600, -47.94889704119054130, 3.690426056929806631 ) ) ;
#7119 = CARTESIAN_POINT ( 'NONE',  ( 5.917102823773431552, 16.57624106732485814, -11.38937882984295236 ) ) ;
#7120 = FACE_OUTER_BOUND ( 'NONE', #52594, .T. ) ;
#7121 = CARTESIAN_POINT ( 'NONE',  ( 2.648799415243708655, 12.25810282899282200, 47.47900987092545222 ) ) ;
#7122 = CARTESIAN_POINT ( 'NONE',  ( 5.901764892641307547, -22.68842833057569308, 43.39615982236225733 ) ) ;
#7123 = FACE_BOUND ( 'NONE', #19230, .T. ) ;
#7124 = CARTESIAN_POINT ( 'NONE',  ( 0.6027935024548037868, 38.05972402498736784, 29.42425667880449325 ) ) ;
#7125 = CIRCLE ( 'NONE', #18162, 2.649999999999997691 ) ;
#7126 = CIRCLE ( 'NONE', #42193, 48.91267123290010943 ) ;
#7127 = CARTESIAN_POINT ( 'NONE',  ( 4.956653778116994147, 39.67974989265076857, -27.17045123668430406 ) ) ;
#7128 = CARTESIAN_POINT ( 'NONE',  ( 5.958863334805807099, -2.677925489610497589, -20.35021240744034188 ) ) ;
#7129 = EDGE_CURVE ( 'NONE', #1309, #54294, #17021, .T. ) ;
#7130 = CARTESIAN_POINT ( 'NONE',  ( 0.8751705887134553219, 11.58504748649199811, -46.67919521768876479 ) ) ;
#7131 = DIRECTION ( 'NONE',  ( -1.000000000000000000, -3.135800716341471541E-16, -1.298891185607920445E-16 ) ) ;
#7132 = EDGE_CURVE ( 'NONE', #15054, #28479, #15578, .T. ) ;
#7133 = CARTESIAN_POINT ( 'NONE',  ( 4.833616638992205949, 43.64812679991096900, 15.29495699393742036 ) ) ;
#7134 = B_SPLINE_CURVE_WITH_KNOTS ( 'NONE', 3,
 ( #16688, #31090, #50192, #7255, #31399, #26384 ),
 .UNSPECIFIED., .F., .F.,
 ( 4, 2, 4 ),
 ( 1.269611854458016711E-16, 0.0002450741128632349442, 0.0004901482257263429284 ),
 .UNSPECIFIED. ) ;
#7135 = CARTESIAN_POINT ( 'NONE',  ( 0.8744876279028263033, 40.65405044375290800, 27.52450240960382644 ) ) ;
#7136 = CARTESIAN_POINT ( 'NONE',  ( -99.49999999999975842, 2.999999999999993339, -1.278713541334263340E-16 ) ) ;
#7137 = EDGE_CURVE ( 'NONE', #54529, #461, #35004, .T. ) ;
#7138 =( BOUNDED_SURFACE ( )  B_SPLINE_SURFACE ( 3, 1, ( 
 ( #24818, #55466 ),
 ( #60469, #21355 ),
 ( #45488, #54528 ),
 ( #2221, #31683 ) ),
 .UNSPECIFIED., .F., .F., .F. ) 
 B_SPLINE_SURFACE_WITH_KNOTS ( ( 4, 4 ),
 ( 2, 2 ),
 ( 0.000000000000000000, 1.000000000000000000 ),
 ( 0.000000000000000000, 1.000000000000000000 ),
 .UNSPECIFIED. ) 
 GEOMETRIC_REPRESENTATION_ITEM ( )  RATIONAL_B_SPLINE_SURFACE ( (
 ( 1.000000000000000000, 1.000000000000000000),
 ( 0.9953040768229005630, 0.8617119497784937465),
 ( 0.9953040768229005630, 0.8617119497784937465),
 ( 1.000000000000000000, 1.000000000000000000) ) ) 
 REPRESENTATION_ITEM ( '' )  SURFACE ( )  );
#7139 = EDGE_LOOP ( 'NONE', ( #53543, #26603, #26286, #55709 ) ) ;
#7140 = CARTESIAN_POINT ( 'NONE',  ( 0.1081432562775998946, 37.13343246403895392, 21.92800090985282679 ) ) ;
#7141 = CARTESIAN_POINT ( 'NONE',  ( 0.1154773475650540532, -38.53416957546567545, -21.49561362639775908 ) ) ;
#7142 = CARTESIAN_POINT ( 'NONE',  ( -6.057079549204054558, -12.95277456599841592, 14.24980217905367930 ) ) ;
#7143 = CARTESIAN_POINT ( 'NONE',  ( 0.9740398440564319582, 39.48175649279257726, -16.80263250099845251 ) ) ;
#7144 = ORIENTED_EDGE ( 'NONE', *, *, #60795, .F. ) ;
#7145 = CARTESIAN_POINT ( 'NONE',  ( 4.549368137175248350, 13.59764261105751793, -40.71620287708331176 ) ) ;
#7146 = CARTESIAN_POINT ( 'NONE',  ( 5.895596859100789899, -4.666058297670421240, -19.56415301451173150 ) ) ;
#7147 = EDGE_CURVE ( 'NONE', #31029, #51225, #23010, .T. ) ;
#7148 = CARTESIAN_POINT ( 'NONE',  ( 0.5997462898726536595, -14.47257175146309649, 46.92649887902422279 ) ) ;
#7149 = VERTEX_POINT ( 'NONE', #28740 ) ;
#7150 = EDGE_CURVE ( 'NONE', #3346, #9975, #47862, .T. ) ;
#7151 = LINE ( 'NONE', #12514, #53981 ) ;
#7152 = ORIENTED_EDGE ( 'NONE', *, *, #42796, .T. ) ;
#7153 = CARTESIAN_POINT ( 'NONE',  ( 0.8751705887134423323, -24.81530984069236823, 41.19904111682465242 ) ) ;
#7154 = CARTESIAN_POINT ( 'NONE',  ( 0.6041374136657475802, 33.89363087703001298, 34.14050483116148627 ) ) ;
#7155 = ORIENTED_EDGE ( 'NONE', *, *, #4843, .F. ) ;
#7156 = CARTESIAN_POINT ( 'NONE',  ( 0.3676999524040323597, -28.14442808720941969, 33.96824621564581292 ) ) ;
#7157 = ORIENTED_EDGE ( 'NONE', *, *, #6835, .T. ) ;
#7158 = CARTESIAN_POINT ( 'NONE',  ( 2.788021980277358036, 6.069845295522647588E-12, -46.99417130740492610 ) ) ;
#7159 = CARTESIAN_POINT ( 'NONE',  ( 0.1104177457020373010, -26.25638621857967792, -34.20994892372200979 ) ) ;
#7160 = EDGE_LOOP ( 'NONE', ( #28295, #38709, #37095, #61409 ) ) ;
#7161 = CIRCLE ( 'NONE', #42237, 8.000000000000000000 ) ;
#7162 = EDGE_LOOP ( 'NONE', ( #25861, #37858, #1239, #31853 ) ) ;
#7163 = CARTESIAN_POINT ( 'NONE',  ( -6.010958268070873523, 9.409153349053815063, -16.32616437357102157 ) ) ;
#7164 = ORIENTED_EDGE ( 'NONE', *, *, #480, .F. ) ;
#7165 = CARTESIAN_POINT ( 'NONE',  ( -6.010958268070873523, -0.01451635840176482631, 18.84344976839986785 ) ) ;
#7166 = CIRCLE ( 'NONE', #44250, 75.00000000000001421 ) ;
#7167 = ORIENTED_EDGE ( 'NONE', *, *, #3667, .T. ) ;
#7168 = EDGE_LOOP ( 'NONE', ( #321, #1851, #40585, #12227 ) ) ;
#7169 = CARTESIAN_POINT ( 'NONE',  ( -6.072942160501519915, -4.270762779174508417, 18.77670758075115742 ) ) ;
#7170 = CARTESIAN_POINT ( 'NONE',  ( 0.6067375320500711933, 43.97491060910887484, 18.98242280073580801 ) ) ;
#7171 = CARTESIAN_POINT ( 'NONE',  ( 4.956445790443989807, 46.03642002599014660, 9.908889005849758291 ) ) ;
#7172 = CARTESIAN_POINT ( 'NONE',  ( 4.967162193818131399, -38.83676580803778933, 18.65818244221244981 ) ) ;
#7173 = CARTESIAN_POINT ( 'NONE',  ( 0.5980894510889448457, 41.31170365136853917, 24.66136644716835491 ) ) ;
#7174 = EDGE_LOOP ( 'NONE', ( #44984, #46257, #4077, #44569 ) ) ;
#7175 = CARTESIAN_POINT ( 'NONE',  ( 0.1154773475650540393, -1.594008704965688805, -44.09538259607931110 ) ) ;
#7176 = ADVANCED_FACE ( 'NONE', ( #29050 ), #28522, .F. ) ;
#7177 = CARTESIAN_POINT ( 'NONE',  ( 0.5819845901640493535, -44.42187107932956280, 17.90867915372037444 ) ) ;
#7178 = ORIENTED_EDGE ( 'NONE', *, *, #49712, .F. ) ;
#7179 = ADVANCED_FACE ( 'NONE', ( #48456 ), #21399, .F. ) ;
#7180 = ORIENTED_EDGE ( 'NONE', *, *, #44702, .F. ) ;
#7181 = CARTESIAN_POINT ( 'NONE',  ( 0.9756008150404602564, 33.95486284030262425, -26.23365443298883193 ) ) ;
#7182 = FACE_OUTER_BOUND ( 'NONE', #39196, .T. ) ;
#7183 = CARTESIAN_POINT ( 'NONE',  ( 1.157643937452369709, 40.20129499413059904, -11.86836784859839788 ) ) ;
#7184 = VERTEX_POINT ( 'NONE', #14518 ) ;
#7185 = CARTESIAN_POINT ( 'NONE',  ( 0.1081432562775997003, -42.69830087850308331, -6.048481838665884958 ) ) ;
#7186 = B_SPLINE_CURVE_WITH_KNOTS ( 'NONE', 3,
 ( #13637, #61823, #52436, #61521, #32744, #37145, #51203, #28638, #22716, #28334, #38079, #8285, #18641, #32431, #42164, #13029, #41846, #33061, #32124 ),
 .UNSPECIFIED., .F., .F.,
 ( 4, 3, 3, 3, 3, 3, 4 ),
 ( 3.469685171791681197E-18, 0.0002612768053151709501, 0.0003919133833142916844, 0.0005225499612322625966, 0.0006531865391693322722, 0.0008112755173415197489, 0.0009693688056799745247 ),
 .UNSPECIFIED. ) ;
#7187 = CARTESIAN_POINT ( 'NONE',  ( 0.9762797500689124330, -27.44172181261391330, -31.67454323498310842 ) ) ;
#7188 = CARTESIAN_POINT ( 'NONE',  ( 4.549368137175248350, 0.000000000000000000, 0.000000000000000000 ) ) ;
#7189 = EDGE_CURVE ( 'NONE', #461, #26377, #2784, .T. ) ;
#7190 = EDGE_CURVE ( 'NONE', #30308, #9806, #28200, .T. ) ;
#7191 = B_SPLINE_CURVE_WITH_KNOTS ( 'NONE', 3,
 ( #5715, #1335, #33970, #39600, #11081, #39291 ),
 .UNSPECIFIED., .F., .F.,
 ( 4, 2, 4 ),
 ( 1.807478856737577690E-17, 0.0002293319059085093307, 0.0004586638118170005551 ),
 .UNSPECIFIED. ) ;
#7192 = ORIENTED_EDGE ( 'NONE', *, *, #42796, .F. ) ;
#7193 = CARTESIAN_POINT ( 'NONE',  ( 4.553261556744873317, -41.61700166486752295, 14.05577241741092998 ) ) ;
#7194 = VERTEX_POINT ( 'NONE', #47713 ) ;
#7195 = EDGE_CURVE ( 'NONE', #61919, #48474, #33318, .T. ) ;
#7196 = CARTESIAN_POINT ( 'NONE',  ( 5.959547316686252039, 14.51632612601528827, -14.51128755440526241 ) ) ;
#7197 = CARTESIAN_POINT ( 'NONE',  ( 4.967162193818130511, -18.65818244221228284, -38.83676580803786749 ) ) ;
#7198 = DIRECTION ( 'NONE',  ( 0.000000000000000000, 0.000000000000000000, 1.000000000000000000 ) ) ;
#7199 = FILL_AREA_STYLE_COLOUR ( '', #30707 ) ;
#7200 = CARTESIAN_POINT ( 'NONE',  ( 0.5998501479064708430, -5.759754759340450114, -47.76154736470756745 ) ) ;
#7201 = EDGE_CURVE ( 'NONE', #60883, #52075, #45429, .T. ) ;
#7202 = VERTEX_POINT ( 'NONE', #56780 ) ;
#7203 = CARTESIAN_POINT ( 'NONE',  ( 0.9758171775293931205, 21.44911662810702779, -37.16279804060109626 ) ) ;
#7204 = FACE_OUTER_BOUND ( 'NONE', #32068, .T. ) ;
#7205 = CARTESIAN_POINT ( 'NONE',  ( 4.975801465491695552, -3.702618843597113685, -47.76942479135485087 ) ) ;
#7206 = CARTESIAN_POINT ( 'NONE',  ( 0.1119899015040009965, 9.270611153904185997, 43.13950714861741176 ) ) ;
#7207 = CARTESIAN_POINT ( 'NONE',  ( 0.8560838555295223751, -0.6537497281626496459, 46.90357604036880446 ) ) ;
#7208 = CARTESIAN_POINT ( 'NONE',  ( 0.5830082357119554803, 32.40480661380604488, 33.89927054171182164 ) ) ;
#7209 = CARTESIAN_POINT ( 'NONE',  ( 1.088313998177382613, -37.54798835078475605, 20.77783415101614395 ) ) ;
#7210 = DIRECTION ( 'NONE',  ( 0.000000000000000000, 0.000000000000000000, 1.000000000000000000 ) ) ;
#7211 = CARTESIAN_POINT ( 'NONE',  ( 1.227938101723748288, 26.79402671879374864, -33.52879263017835143 ) ) ;
#7212 = B_SPLINE_CURVE_WITH_KNOTS ( 'NONE', 3,
 ( #44900, #35486, #10434, #54542, #1937, #20148, #15443, #40205, #11672, #49876, #6935, #26069, #50185, #12918, #7559, #51091, #31080, #26682, #41429 ),
 .UNSPECIFIED., .F., .F.,
 ( 4, 3, 3, 3, 3, 3, 4 ),
 ( 1.734776414728241573E-18, 0.0002612768053151702454, 0.0003919133833142904918, 0.0005225499612322580430, 0.0006531865391693332480, 0.0008112755173415176890, 0.0009693688056799727899 ),
 .UNSPECIFIED. ) ;
#7213 =( BOUNDED_SURFACE ( )  B_SPLINE_SURFACE ( 3, 1, ( 
 ( #32509, #22180 ),
 ( #32200, #41307 ),
 ( #51584, #36918 ),
 ( #27799, #40695 ) ),
 .UNSPECIFIED., .F., .F., .F. ) 
 B_SPLINE_SURFACE_WITH_KNOTS ( ( 4, 4 ),
 ( 2, 2 ),
 ( 0.000000000000000000, 1.000000000000000000 ),
 ( 0.000000000000000000, 1.000000000000000000 ),
 .UNSPECIFIED. ) 
 GEOMETRIC_REPRESENTATION_ITEM ( )  RATIONAL_B_SPLINE_SURFACE ( (
 ( 1.000000000000000000, 1.000000000000000000),
 ( 0.9953390228620291325, 0.8624445117761032620),
 ( 0.9953390228620291325, 0.8624445117761032620),
 ( 1.000000000000000000, 1.000000000000000000) ) ) 
 REPRESENTATION_ITEM ( '' )  SURFACE ( )  );
#7214 = CIRCLE ( 'NONE', #2249, 4.000000000000000888 ) ;
#7215 = CARTESIAN_POINT ( 'NONE',  ( 4.553261556744875094, 0.000000000000000000, 0.000000000000000000 ) ) ;
#7216 = LINE ( 'NONE', #60456, #16191 ) ;
#7217 = ORIENTED_EDGE ( 'NONE', *, *, #9358, .T. ) ;
#7218 = LINE ( 'NONE', #12274, #4836 ) ;
#7219 = FACE_OUTER_BOUND ( 'NONE', #61459, .T. ) ;
#7220 = CARTESIAN_POINT ( 'NONE',  ( 1.112077966505211402, -42.35976605652983551, 12.19346319814910728 ) ) ;
#7221 = ORIENTED_EDGE ( 'NONE', *, *, #24978, .T. ) ;
#7222 = DIRECTION ( 'NONE',  ( 0.000000000000000000, 0.000000000000000000, 1.000000000000000000 ) ) ;
#7223 = B_SPLINE_CURVE_WITH_KNOTS ( 'NONE', 3,
 ( #23768, #23156, #19090, #28151, #13774, #32881 ),
 .UNSPECIFIED., .F., .F.,
 ( 4, 2, 4 ),
 ( 7.040638946443416885E-18, 0.0002445244328975369145, 0.0004890488657950667816 ),
 .UNSPECIFIED. ) ;
#7224 = EDGE_CURVE ( 'NONE', #17384, #40739, #27986, .T. ) ;
#7225 = CARTESIAN_POINT ( 'NONE',  ( 45.00000000000001421, 0.000000000000000000, 0.000000000000000000 ) ) ;
#7226 = ORIENTED_EDGE ( 'NONE', *, *, #4134, .F. ) ;
#7227 = CARTESIAN_POINT ( 'NONE',  ( 3.238741278300274029, 38.11287256318061623, -19.89284324544654226 ) ) ;
#7228 = EDGE_CURVE ( 'NONE', #9581, #6735, #38007, .T. ) ;
#7229 = CARTESIAN_POINT ( 'NONE',  ( 0.9730545539215883499, -41.31259007387222226, -11.59290486963550393 ) ) ;
#7230 = ORIENTED_EDGE ( 'NONE', *, *, #44211, .F. ) ;
#7232 = CARTESIAN_POINT ( 'NONE',  ( 5.959547316686252039, 20.35048796920736791, -2.675599016784323769 ) ) ;
#7231 = B_SPLINE_CURVE_WITH_KNOTS ( 'NONE', 3,
 ( #504, #5198, #1730, #34062 ),
 .UNSPECIFIED., .F., .F.,
 ( 4, 4 ),
 ( 4.164239746139790209E-17, 0.005004948556313859077 ),
 .UNSPECIFIED. ) ;
#7233 = ORIENTED_EDGE ( 'NONE', *, *, #42224, .F. ) ;
#7234 = ORIENTED_EDGE ( 'NONE', *, *, #55075, .T. ) ;
#7235 = CARTESIAN_POINT ( 'NONE',  ( 0.9740398440564311811, -5.189371650077155174, 42.59352035928885982 ) ) ;
#7236 = VERTEX_POINT ( 'NONE', #4758 ) ;
#7237 = CARTESIAN_POINT ( 'NONE',  ( 4.975610109902397937, 30.04451009524531102, -38.59762713269398660 ) ) ;
#7238 = PRODUCT_DEFINITION_SHAPE ( 'NONE', 'NONE',  #61975 ) ;
#7239 = EDGE_LOOP ( 'NONE', ( #4013, #45371, #9473, #45138, #17668, #60804, #13702 ) ) ;
#7240 = CARTESIAN_POINT ( 'NONE',  ( 3.407937589446178528, 13.69123696618924413, -0.4592810312472460077 ) ) ;
#7241 = CARTESIAN_POINT ( 'NONE',  ( 2.301529144917015213, 17.18548816179623628, -44.85388898587007134 ) ) ;
#7242 = ORIENTED_EDGE ( 'NONE', *, *, #25967, .F. ) ;
#7243 = DIRECTION ( 'NONE',  ( 0.000000000000000000, 0.000000000000000000, 1.000000000000000000 ) ) ;
#7244 = CARTESIAN_POINT ( 'NONE',  ( 2.282803330402968456, -6.514475874215432505, -46.51944229611155635 ) ) ;
#7245 = CARTESIAN_POINT ( 'NONE',  ( 0.5809828226811617480, 18.83114015454759738, -44.03860873105676177 ) ) ;
#7246 = EDGE_LOOP ( 'NONE', ( #40911, #30741 ) ) ;
#7247 = B_SPLINE_CURVE_WITH_KNOTS ( 'NONE', 3,
 ( #7669, #20867, #44396, #11472 ),
 .UNSPECIFIED., .F., .F.,
 ( 4, 4 ),
 ( 0.000000000000000000, 0.004048833967417086489 ),
 .UNSPECIFIED. ) ;
#7248 = ORIENTED_EDGE ( 'NONE', *, *, #9104, .F. ) ;
#7249 = COLOUR_RGB ( '', 0.08235294, 0.09019608, 0.10196078) ;
#7250 = CARTESIAN_POINT ( 'NONE',  ( 4.691466044806102076, -3.249105306918757652, 44.46979273209129246 ) ) ;
#7251 = ADVANCED_FACE ( 'NONE', ( #57690 ), #15019, .F. ) ;
#7252 = AXIS2_PLACEMENT_3D ( 'NONE', #46444, #18538, #41751 ) ;
#7253 = CARTESIAN_POINT ( 'NONE',  ( 0.1158816050234199174, -12.54909674931304941, 42.30203555482339084 ) ) ;
#7254 = B_SPLINE_CURVE_WITH_KNOTS ( 'NONE', 3,
 ( #34086, #48169, #33772, #527, #208, #19982 ),
 .UNSPECIFIED., .F., .F.,
 ( 4, 2, 4 ),
 ( 1.553642821798679850E-17, 0.0002293755540694301259, 0.0004587511081388447477 ),
 .UNSPECIFIED. ) ;
#7255 = CARTESIAN_POINT ( 'NONE',  ( 0.6254311100348668440, -47.77988293940239117, 5.596225872411223712 ) ) ;
#7256 = ORIENTED_EDGE ( 'NONE', *, *, #942, .F. ) ;
#7257 = CARTESIAN_POINT ( 'NONE',  ( 4.967162193818130511, -28.74031574030035685, 32.10009971360062764 ) ) ;
#7258 = CARTESIAN_POINT ( 'NONE',  ( -1.139999999999999680, 6.866799999999992465, 0.000000000000000000 ) ) ;
#7259 = EDGE_CURVE ( 'NONE', #10228, #61052, #14588, .T. ) ;
#7260 = CARTESIAN_POINT ( 'NONE',  ( 3.390910168358336918, 7.855615995994031486, -43.27108080296954995 ) ) ;
#7261 = EDGE_CURVE ( 'NONE', #50174, #32675, #28553, .T. ) ;
#7262 = ORIENTED_EDGE ( 'NONE', *, *, #10072, .T. ) ;
#7263 = ORIENTED_EDGE ( 'NONE', *, *, #56554, .T. ) ;
#7264 = CARTESIAN_POINT ( 'NONE',  ( 9.999999999999991118, 80.00000000000001421, 2.649999999999992806 ) ) ;
#7265 = EDGE_CURVE ( 'NONE', #42991, #51963, #14797, .T. ) ;
#7266 = CARTESIAN_POINT ( 'NONE',  ( 2.009741617377216460, 42.20789687549766001, 12.56970639953054558 ) ) ;
#7267 = DIRECTION ( 'NONE',  ( -0.1011922191286467460, -0.9400526519483206611, -0.3256703031483669242 ) ) ;
#7268 = DIRECTION ( 'NONE',  ( 0.000000000000000000, 0.000000000000000000, 1.000000000000000000 ) ) ;
#7269 = CIRCLE ( 'NONE', #9306, 4.000000000000000000 ) ;
#7270 = CARTESIAN_POINT ( 'NONE',  ( 5.958863334805807099, 18.96369761673808441, 7.853699934219964263 ) ) ;
#7271 = CYLINDRICAL_SURFACE ( 'NONE', #38250, 5.000000000000000888 ) ;
#7272 = CARTESIAN_POINT ( 'NONE',  ( 4.322998006666179727, 46.85697641700694049, 10.36018990813329310 ) ) ;
#7273 = DIRECTION ( 'NONE',  ( -1.000000000000000000, -0.000000000000000000, -0.000000000000000000 ) ) ;
#7274 = CARTESIAN_POINT ( 'NONE',  ( 0.1064266379913944155, -15.98292486309362737, 40.05351204369879525 ) ) ;
#7275 = CARTESIAN_POINT ( 'NONE',  ( 0.5804410086790514622, -34.41390132670949242, -31.86225427258559151 ) ) ;
#7276 = B_SPLINE_CURVE_WITH_KNOTS ( 'NONE', 3,
 ( #23699, #170, #13084, #14315, #32178, #33421, #37201, #52497, #8346, #27466, #46594, #60974, #8658, #27780, #46914, #3950, #23089, #42218, #33734 ),
 .UNSPECIFIED., .F., .F.,
 ( 4, 3, 3, 3, 3, 3, 4 ),
 ( 1.355252715606880543E-20, 0.0002612768053151697033, 0.0003919133833142910339, 0.0005225499612322614040, 0.0006531865391693344406, 0.0008112755173415172553, 0.0009693688056799748499 ),
 .UNSPECIFIED. ) ;
#7277 = CARTESIAN_POINT ( 'NONE',  ( 4.553261556744875094, 40.80044851610500700, -16.27461110774390818 ) ) ;
#7278 = CARTESIAN_POINT ( 'NONE',  ( 0.8744876279028263033, 17.78802839418742110, -45.75954650373051891 ) ) ;
#7279 = CARTESIAN_POINT ( 'NONE',  ( 4.975801465491695552, 0.000000000000000000, 0.000000000000000000 ) ) ;
#7280 = CARTESIAN_POINT ( 'NONE',  ( 0.9789233960466690032, -22.66104764199909027, 35.25356218312401779 ) ) ;
#7281 = CARTESIAN_POINT ( 'NONE',  ( 4.956445790443988031, 0.000000000000000000, 0.000000000000000000 ) ) ;
#7283 =( BOUNDED_SURFACE ( )  B_SPLINE_SURFACE ( 3, 1, ( 
 ( #5588, #595 ),
 ( #279, #15043 ),
 ( #34149, #14729 ),
 ( #24733, #29732 ) ),
 .UNSPECIFIED., .F., .F., .F. ) 
 B_SPLINE_SURFACE_WITH_KNOTS ( ( 4, 4 ),
 ( 2, 2 ),
 ( 0.000000000000000000, 1.000000000000000000 ),
 ( 0.000000000000000000, 1.000000000000000000 ),
 .UNSPECIFIED. ) 
 GEOMETRIC_REPRESENTATION_ITEM ( )  RATIONAL_B_SPLINE_SURFACE ( (
 ( 1.000000000000000000, 1.000000000000000000),
 ( 0.9952954269826590483, 0.8620686068821339365),
 ( 0.9952954269826590483, 0.8620686068821339365),
 ( 1.000000000000000000, 1.000000000000000000) ) ) 
 REPRESENTATION_ITEM ( '' )  SURFACE ( )  );
#7282 = CARTESIAN_POINT ( 'NONE',  ( -6.010958268070873523, -4.891065400978257038, -18.19761767765835359 ) ) ;
#7284 = CARTESIAN_POINT ( 'NONE',  ( 4.960386119450141074, -20.61356833094631824, 38.59426466896017871 ) ) ;
#7286 = ORIENTED_EDGE ( 'NONE', *, *, #36924, .F. ) ;
#7285 = CARTESIAN_POINT ( 'NONE',  ( 3.238931869106854489, 42.95312220797017488, -1.828840280768938120 ) ) ;
#7287 = VERTEX_POINT ( 'NONE', #33622 ) ;
#7288 = CARTESIAN_POINT ( 'NONE',  ( 7.000000000000006217, 1.285836671513502038E-15, -1.348150961071066192E-31 ) ) ;
#7289 = CARTESIAN_POINT ( 'NONE',  ( 0.8557997880470606944, -13.27832040216671317, 46.03118133706021808 ) ) ;
#7290 = CARTESIAN_POINT ( 'NONE',  ( 4.322998006666179727, 35.39923696758967964, 32.40067585697811126 ) ) ;
#7291 = ORIENTED_EDGE ( 'NONE', *, *, #55562, .F. ) ;
#7292 = ORIENTED_EDGE ( 'NONE', *, *, #12343, .F. ) ;
#7293 = CARTESIAN_POINT ( 'NONE',  ( 4.553261556744873317, -15.38244134641770167, -41.14510984366982171 ) ) ;
#7295 = B_SPLINE_CURVE_WITH_KNOTS ( 'NONE', 3,
 ( #16982, #54216, #9095, #41718 ),
 .UNSPECIFIED., .F., .F.,
 ( 4, 4 ),
 ( 0.000000000000000000, 0.004041751736741000349 ),
 .UNSPECIFIED. ) ;
#7294 = CARTESIAN_POINT ( 'NONE',  ( 0.1073791018717578927, -37.58707531572220262, 21.14095454447495115 ) ) ;
#7296 = AXIS2_PLACEMENT_3D ( 'NONE', #30275, #45335, #6438 ) ;
#7297 = ORIENTED_EDGE ( 'NONE', *, *, #1057, .T. ) ;
#7298 = ORIENTED_EDGE ( 'NONE', *, *, #25716, .T. ) ;
#7299 = ADVANCED_FACE ( 'NONE', ( #48022 ), #47755, .F. ) ;
#7300 = CYLINDRICAL_SURFACE ( 'NONE', #35562, 18.99999999999999645 ) ;
#7301 =( BOUNDED_SURFACE ( )  B_SPLINE_SURFACE ( 3, 1, ( 
 ( #28483, #19123 ),
 ( #28800, #61674 ),
 ( #38535, #52912 ),
 ( #8768, #13802 ) ),
 .UNSPECIFIED., .F., .F., .F. ) 
 B_SPLINE_SURFACE_WITH_KNOTS ( ( 4, 4 ),
 ( 2, 2 ),
 ( 0.000000000000000000, 1.000000000000000000 ),
 ( 0.000000000000000000, 1.000000000000000000 ),
 .UNSPECIFIED. ) 
 GEOMETRIC_REPRESENTATION_ITEM ( )  RATIONAL_B_SPLINE_SURFACE ( (
 ( 1.000000000000000000, 1.000000000000000000),
 ( 0.9732289882329797637, 0.9999525324661233672),
 ( 0.9732289882329797637, 0.9999525324661233672),
 ( 1.000000000000000000, 1.000000000000000000) ) ) 
 REPRESENTATION_ITEM ( '' )  SURFACE ( )  );
#7302 = CARTESIAN_POINT ( 'NONE',  ( 0.3676999524040323597, 43.13409918076290950, 9.241215893319909114 ) ) ;
#7303 = CARTESIAN_POINT ( 'NONE',  ( 0.5817217712918331118, -38.40351169400030074, -26.91477742016745012 ) ) ;
#7304 =( BOUNDED_SURFACE ( )  B_SPLINE_SURFACE ( 3, 1, ( 
 ( #57010, #13826 ),
 ( #33237, #37025 ),
 ( #51380, #18828 ),
 ( #37955, #1 ) ),
 .UNSPECIFIED., .F., .F., .F. ) 
 B_SPLINE_SURFACE_WITH_KNOTS ( ( 4, 4 ),
 ( 2, 2 ),
 ( 0.000000000000000000, 1.000000000000000000 ),
 ( 0.000000000000000000, 1.000000000000000000 ),
 .UNSPECIFIED. ) 
 GEOMETRIC_REPRESENTATION_ITEM ( )  RATIONAL_B_SPLINE_SURFACE ( (
 ( 1.000000000000000000, 1.000000000000000000),
 ( 0.9953485035131437453, 0.8621029689291515030),
 ( 0.9953485035131437453, 0.8621029689291515030),
 ( 1.000000000000000000, 1.000000000000000000) ) ) 
 REPRESENTATION_ITEM ( '' )  SURFACE ( )  );
#7305 = ORIENTED_EDGE ( 'NONE', *, *, #43973, .T. ) ;
#7306 = CARTESIAN_POINT ( 'NONE',  ( 4.975610109902397937, 20.32389311291233724, -44.49032227207044343 ) ) ;
#7307 = AXIS2_PLACEMENT_3D ( 'NONE', #2284, #11402, #55526 ) ;
#7308 = CARTESIAN_POINT ( 'NONE',  ( 4.956445790444003130, -40.78973928653796577, 23.53157918788916803 ) ) ;
#7309 = B_SPLINE_CURVE_WITH_KNOTS ( 'NONE', 3,
 ( #52450, #3907, #9545, #28655 ),
 .UNSPECIFIED., .F., .F.,
 ( 4, 4 ),
 ( 1.734723475976807094E-18, 0.004048833967417083887 ),
 .UNSPECIFIED. ) ;
#7310 = CARTESIAN_POINT ( 'NONE',  ( 0.1156495703730067576, 15.11094602997547298, -41.45602806963348286 ) ) ;
#7311 = VERTEX_POINT ( 'NONE', #16589 ) ;
#7312 = EDGE_LOOP ( 'NONE', ( #38320, #11191, #54982, #8762 ) ) ;
#7313 = CARTESIAN_POINT ( 'NONE',  ( 0.5800708119828338338, 13.00144522946658476, 46.09746484493482654 ) ) ;
#7314 = CARTESIAN_POINT ( 'NONE',  ( 4.956445790443987143, 47.01859095792193699, -2.605792484304513934 ) ) ;
#7315 = ORIENTED_EDGE ( 'NONE', *, *, #26378, .F. ) ;
#7316 = CARTESIAN_POINT ( 'NONE',  ( 0.5804410086790514622, -35.14691939471192939, 31.05179397260356211 ) ) ;
#7317 = CARTESIAN_POINT ( 'NONE',  ( 0.6024113833632039894, -8.052380081654970212, 48.44276049237319626 ) ) ;
#7318 = FACE_OUTER_BOUND ( 'NONE', #43411, .T. ) ;
#7319 = CARTESIAN_POINT ( 'NONE',  ( 2.533389852662419894, -43.82923048324839499, -4.055747400899961441 ) ) ;
#7320 = ORIENTED_EDGE ( 'NONE', *, *, #32748, .F. ) ;
#7321 = CARTESIAN_POINT ( 'NONE',  ( 0.9756354156337444516, -30.24859376089802510, -30.43287766742280098 ) ) ;
#7322 = CARTESIAN_POINT ( 'NONE',  ( 0.5782707292762423457, -13.20261929688047076, 45.00474638756736567 ) ) ;
#7323 = EDGE_CURVE ( 'NONE', #15612, #55623, #24534, .T. ) ;
#7324 = DIRECTION ( 'NONE',  ( 1.000000000000000000, 0.000000000000000000, 0.000000000000000000 ) ) ;
#7325 = DIRECTION ( 'NONE',  ( -1.000000000000000000, -0.000000000000000000, -0.000000000000000000 ) ) ;
#7326 = ORIENTED_EDGE ( 'NONE', *, *, #30256, .T. ) ;
#7327 = CARTESIAN_POINT ( 'NONE',  ( 4.975801465491695552, 0.000000000000000000, 0.000000000000000000 ) ) ;
#7328 = EDGE_CURVE ( 'NONE', #41448, #50438, #17794, .T. ) ;
#7329 = CARTESIAN_POINT ( 'NONE',  ( 0.1073791018717483448, -5.147744207007177053, 42.81622261970985477 ) ) ;
#7330 = CARTESIAN_POINT ( 'NONE',  ( 4.956653778116987041, -47.94889704119048446, -3.690426056930470988 ) ) ;
#7331 = CARTESIAN_POINT ( 'NONE',  ( 0.7954196712028466232, 7.138712347928183988, -47.56618050291067590 ) ) ;
#7332 = EDGE_LOOP ( 'NONE', ( #7478, #31542, #47567, #58626 ) ) ;
#7333 = CARTESIAN_POINT ( 'NONE',  ( 1.157643937452368821, -41.75974212862475810, 3.623011447058365864 ) ) ;
#7334 = EDGE_CURVE ( 'NONE', #43245, #53393, #46557, .T. ) ;
#7335 = CARTESIAN_POINT ( 'NONE',  ( 4.956653778116971054, 42.88673967249130925, 21.75875759808722876 ) ) ;
#7336 = CARTESIAN_POINT ( 'NONE',  ( 3.783278058412225864, 38.10568111914503930, 20.00643011788468328 ) ) ;
#7337 = B_SPLINE_CURVE_WITH_KNOTS ( 'NONE', 3,
 ( #12278, #9090, #13820, #51375, #4361, #9393 ),
 .UNSPECIFIED., .F., .F.,
 ( 4, 2, 4 ),
 ( 8.805430561888389713E-18, 0.0002445244328975372397, 0.0004890488657950656974 ),
 .UNSPECIFIED. ) ;
#7338 = COLOUR_RGB ( '', 0.31764706, 0.68627451, 0.89019608) ;
#7339 = CARTESIAN_POINT ( 'NONE',  ( 4.956445790444031552, 34.56007374686835476, -31.98654955994249960 ) ) ;
#7340 = CARTESIAN_POINT ( 'NONE',  ( 4.956653778116990594, -20.77844580450529577, -43.37017594958076927 ) ) ;
#7341 = CARTESIAN_POINT ( 'NONE',  ( 0.5819845901640493535, 46.37938751183699537, -11.95725023767309203 ) ) ;
#7342 = CARTESIAN_POINT ( 'NONE',  ( 4.553261556744875094, -25.31600221269659201, 35.89762663172006540 ) ) ;
#7343 = CARTESIAN_POINT ( 'NONE',  ( 1.157643937452369043, 29.72797324181601653, 29.55080170703706699 ) ) ;
#7344 = CARTESIAN_POINT ( 'NONE',  ( 0.6041374136657476912, -6.452348380035592967, -47.67304777898696955 ) ) ;
#7345 = LINE ( 'NONE', #7039, #27821 ) ;
#7347 = ORIENTED_EDGE ( 'NONE', *, *, #9134, .T. ) ;
#7346 = ADVANCED_FACE ( 'NONE', ( #30669 ), #54123, .F. ) ;
#7348 = CARTESIAN_POINT ( 'NONE',  ( 0.1129192098497447394, -1.898585089631814826, -44.08341142019957459 ) ) ;
#7349 = DIRECTION ( 'NONE',  ( 0.000000000000000000, 0.000000000000000000, 1.000000000000000000 ) ) ;
#7350 = B_SPLINE_CURVE_WITH_KNOTS ( 'NONE', 3,
 ( #11436, #2320, #54624, #30837, #49955, #7009, #31148, #26142, #21446, #40582, #59645, #16757, #7319, #26448, #45579, #3245, #42134, #51794, #8258, #60566, #13295, #27377, #50870, #52099, #18308 ),
 .UNSPECIFIED., .F., .F.,
 ( 4, 3, 3, 3, 3, 3, 3, 3, 4 ),
 ( 5.057544569639794935E-18, 0.0005656085177311395316, 0.001131215744874499622, 0.001696821861372766133, 0.002262427090022498151, 0.002828031679238745925, 0.003393635864401604862, 0.003977030878808131623, 0.004561030005651158133 ),
 .UNSPECIFIED. ) ;
#7352 = EDGE_CURVE ( 'NONE', #41987, #41115, #50606, .T. ) ;
#7351 = CARTESIAN_POINT ( 'NONE',  ( 3.680882792899937250, 1.849662971457552540, 47.94008871805920080 ) ) ;
#7353 = CARTESIAN_POINT ( 'NONE',  ( -6.078457390727109555, -1.844660340667949816, -19.16746564533440633 ) ) ;
#7354 = VECTOR ( 'NONE', #38808, 1000.000000000000114 ) ;
#7355 = CARTESIAN_POINT ( 'NONE',  ( 5.910764540655178756, -11.91768246006627763, 16.20092846876966775 ) ) ;
#7356 = CARTESIAN_POINT ( 'NONE',  ( 5.910764540655177868, 19.70610972188033827, 4.021253299454832231 ) ) ;
#7357 = PRODUCT_CONTEXT ( 'NONE', #13962, 'mechanical' ) ;
#7358 = CARTESIAN_POINT ( 'NONE',  ( 0.6030672727741701600, -44.47882233696937249, 18.32928433899675014 ) ) ;
#7359 = LINE ( 'NONE', #41232, #23487 ) ;
#7360 = CARTESIAN_POINT ( 'NONE',  ( 0.7954190325252783467, -29.96539637359188646, -37.62416463577099535 ) ) ;
#7362 = EDGE_LOOP ( 'NONE', ( #28161, #35366 ) ) ;
#7361 = CARTESIAN_POINT ( 'NONE',  ( 0.9730545539215883499, -41.31259007387222226, -11.59290486963550393 ) ) ;
#7363 = ORIENTED_EDGE ( 'NONE', *, *, #38549, .T. ) ;
#7364 = CARTESIAN_POINT ( 'NONE',  ( 0.8753041380234471980, -2.462982411634902835, 49.04153388213869391 ) ) ;
#7365 = CARTESIAN_POINT ( 'NONE',  ( 0.5837800304671212359, -7.845051310127922228, 46.23518683990537426 ) ) ;
#7366 = CARTESIAN_POINT ( 'NONE',  ( 4.999999999999997335, 9.184547653667864935E-16, -9.629649721936170507E-32 ) ) ;
#7367 = VERTEX_POINT ( 'NONE', #26283 ) ;
#7368 = DIRECTION ( 'NONE',  ( 0.07500201931887537365, 0.8296863770785113390, -0.5531683403706553204 ) ) ;
#7369 = CARTESIAN_POINT ( 'NONE',  ( 0.7764139734771244861, 31.96094574548908440, 34.32984733378186348 ) ) ;
#7370 = CARTESIAN_POINT ( 'NONE',  ( 0.5998501479064708430, 41.39809967730453621, 24.50586714782619424 ) ) ;
#7371 = VERTEX_POINT ( 'NONE', #15434 ) ;
#7372 = ORIENTED_EDGE ( 'NONE', *, *, #61197, .T. ) ;
#7373 = ADVANCED_FACE ( 'NONE', ( #21909 ), #58516, .F. ) ;
#7374 = B_SPLINE_CURVE_WITH_KNOTS ( 'NONE', 3,
 ( #36150, #7599, #55524, #55215, #12338, #41161, #12649, #50833, #3211, #22337, #60529, #36767, #31427, #26724, #60221, #17334 ),
 .UNSPECIFIED., .F., .F.,
 ( 4, 3, 3, 3, 3, 4 ),
 ( 2.194378057379452319E-17, 0.0002612764279487740844, 0.0003919131003184779440, 0.0005225497727000652558, 0.0007837925190632489322, 0.001045051706266716734 ),
 .UNSPECIFIED. ) ;
#7375 = CARTESIAN_POINT ( 'NONE',  ( 0.7048096507298579061, -17.62869676200378066, -44.76417498422306807 ) ) ;
#7376 = B_SPLINE_CURVE_WITH_KNOTS ( 'NONE', 3,
 ( #60916, #13332, #6340, #34591, #10471, #29873 ),
 .UNSPECIFIED., .F., .F.,
 ( 4, 2, 4 ),
 ( 0.002336974151641521731, 0.003500975885716455828, 0.004664977619791389925 ),
 .UNSPECIFIED. ) ;
#7377 = FACE_OUTER_BOUND ( 'NONE', #27359, .T. ) ;
#7378 = CARTESIAN_POINT ( 'NONE',  ( 1.827326673878743923, -4.394636550976340317, -42.82501343454093501 ) ) ;
#7379 = ORIENTED_EDGE ( 'NONE', *, *, #8627, .T. ) ;
#7380 = AXIS2_PLACEMENT_3D ( 'NONE', #20792, #59291, #25172 ) ;
#7381 = ORIENTED_EDGE ( 'NONE', *, *, #56045, .T. ) ;
#7382 = CARTESIAN_POINT ( 'NONE',  ( 5.894904586330512508, -18.51743364446320328, 7.850736480391183214 ) ) ;
#7383 = CARTESIAN_POINT ( 'NONE',  ( 1.227938101723756947, -33.52879263017882039, 26.79402671879314823 ) ) ;
#7384 =( BOUNDED_SURFACE ( )  B_SPLINE_SURFACE ( 3, 1, ( 
 ( #39616, #53976 ),
 ( #58363, #16405 ),
 ( #54276, #30482 ),
 ( #58671, #11717 ) ),
 .UNSPECIFIED., .F., .F., .F. ) 
 B_SPLINE_SURFACE_WITH_KNOTS ( ( 4, 4 ),
 ( 2, 2 ),
 ( 0.000000000000000000, 1.000000000000000000 ),
 ( 0.000000000000000000, 1.000000000000000000 ),
 .UNSPECIFIED. ) 
 GEOMETRIC_REPRESENTATION_ITEM ( )  RATIONAL_B_SPLINE_SURFACE ( (
 ( 1.000000000000000000, 1.000000000000000000),
 ( 0.9729067724841187204, 0.9999501103223794596),
 ( 0.9729067724841187204, 0.9999501103223794596),
 ( 1.000000000000000000, 1.000000000000000000) ) ) 
 REPRESENTATION_ITEM ( '' )  SURFACE ( )  );
#7385 = VERTEX_POINT ( 'NONE', #6848 ) ;
#7386 = CARTESIAN_POINT ( 'NONE',  ( -6.078075953587585900, -11.01234782890426445, -15.79630873154748549 ) ) ;
#7387 = LINE ( 'NONE', #40650, #44030 ) ;
#7388 = EDGE_LOOP ( 'NONE', ( #37494, #6556, #11509, #54224 ) ) ;
#7389 =( BOUNDED_SURFACE ( )  B_SPLINE_SURFACE ( 3, 1, ( 
 ( #5337, #24468 ),
 ( #23856, #47980 ),
 ( #43926, #44231 ),
 ( #20396, #1259 ) ),
 .UNSPECIFIED., .F., .F., .F. ) 
 B_SPLINE_SURFACE_WITH_KNOTS ( ( 4, 4 ),
 ( 2, 2 ),
 ( 0.000000000000000000, 1.000000000000000000 ),
 ( 0.000000000000000000, 1.000000000000000000 ),
 .UNSPECIFIED. ) 
 GEOMETRIC_REPRESENTATION_ITEM ( )  RATIONAL_B_SPLINE_SURFACE ( (
 ( 1.000000000000000000, 1.000000000000000000),
 ( 0.7211978278499968642, 0.9934217856018975334),
 ( 0.7211978278499968642, 0.9934217856018975334),
 ( 1.000000000000000000, 1.000000000000000000) ) ) 
 REPRESENTATION_ITEM ( '' )  SURFACE ( )  );
#7390 = CARTESIAN_POINT ( 'NONE',  ( -6.078726893082806448, -4.288195875146701752, 18.77246434022701749 ) ) ;
#7391 = CARTESIAN_POINT ( 'NONE',  ( 0.5797568599927133137, -46.82898596429171789, 2.504272794081084275 ) ) ;
#7392 = VERTEX_POINT ( 'NONE', #36029 ) ;
#7393 = CARTESIAN_POINT ( 'NONE',  ( 0.6017666602106489515, -47.74032907933394654, -5.933006478840522568 ) ) ;
#7394 = CARTESIAN_POINT ( 'NONE',  ( 0.7056759521544994085, 46.89390201348435028, 0.8430795138737422478 ) ) ;
#7395 = CARTESIAN_POINT ( 'NONE',  ( -4.000000000000000000, -2.309401076758531346, -5.242734410091827613 ) ) ;
#7396 = PRESENTATION_LAYER_ASSIGNMENT (  '', '', ( #54392 ) ) ;
#7397 = B_SPLINE_CURVE_WITH_KNOTS ( 'NONE', 3,
 ( #35735, #8124, #21308, #50719, #31947, #60126, #7811, #26935, #41362, #55111, #8420, #3109, #17232, #54802, #59820, #17536, #27544, #36656, #56038 ),
 .UNSPECIFIED., .F., .F.,
 ( 4, 3, 3, 3, 3, 3, 4 ),
 ( 9.813676791237320760E-18, 0.0002732106629380670940, 0.0004098138914053731010, 0.0005464171197651472318, 0.0006830203481512563081, 0.0008196235766963549593, 0.001011968216111140510 ),
 .UNSPECIFIED. ) ;
#7398 = ORIENTED_EDGE ( 'NONE', *, *, #11110, .T. ) ;
#7399 = CARTESIAN_POINT ( 'NONE',  ( 0.09136607875274982415, 0.000000000000000000, 0.000000000000000000 ) ) ;
#7400 = CARTESIAN_POINT ( 'NONE',  ( 0.2224561200757621260, -42.84309024201780147, 4.874377913225771408 ) ) ;
#7401 = EDGE_LOOP ( 'NONE', ( #58328, #35295, #21517, #50860 ) ) ;
#7402 = FACE_OUTER_BOUND ( 'NONE', #24816, .T. ) ;
#7403 = ORIENTED_EDGE ( 'NONE', *, *, #53516, .T. ) ;
#7404 = CARTESIAN_POINT ( 'NONE',  ( 0.9730545539215883499, -36.90443313492315980, -21.89037132892475057 ) ) ;
#7405 = ADVANCED_FACE ( 'NONE', ( #17211 ), #52563, .T. ) ;
#7406 = VERTEX_POINT ( 'NONE', #21288 ) ;
#7407 = CARTESIAN_POINT ( 'NONE',  ( -6.017396004339687465, 0.001173774849245718494, -18.84316306185412415 ) ) ;
#7408 = CARTESIAN_POINT ( 'NONE',  ( 0.7245667037590747261, 44.12005358974304414, -19.16327388244015495 ) ) ;
#7409 = CARTESIAN_POINT ( 'NONE',  ( 0.1158516988532803244, -43.75558653473088810, 5.691292105881863073 ) ) ;
#7410 = ORIENTED_EDGE ( 'NONE', *, *, #49220, .F. ) ;
#7411 = CARTESIAN_POINT ( 'NONE',  ( 0.1140933569871965259, -27.21347274398934246, -34.73293611683375559 ) ) ;
#7412 = EDGE_CURVE ( 'NONE', #3302, #8164, #10359, .T. ) ;
#7413 = CARTESIAN_POINT ( 'NONE',  ( 4.975801465491695552, 0.000000000000000000, 0.000000000000000000 ) ) ;
#7414 = CARTESIAN_POINT ( 'NONE',  ( 1.000433927950262314, -41.85488811441339863, -2.141732612345590425 ) ) ;
#7415 = VERTEX_POINT ( 'NONE', #43649 ) ;
#7416 = EDGE_CURVE ( 'NONE', #49781, #10248, #29757, .T. ) ;
#7417 = ORIENTED_EDGE ( 'NONE', *, *, #20767, .F. ) ;
#7418 = CARTESIAN_POINT ( 'NONE',  ( 8.000000000000007105, -56.56854249492331377, -56.56854249492430142 ) ) ;
#7419 = CARTESIAN_POINT ( 'NONE',  ( 5.838029081930955932, -28.00222738077721729, -38.03866874468887715 ) ) ;
#7420 = CARTESIAN_POINT ( 'NONE',  ( 0.9787284016396634589, 38.50972377290732140, -16.53291183860855895 ) ) ;
#7421 = CARTESIAN_POINT ( 'NONE',  ( 0.1092355843206037486, 30.28032287551036816, 30.70542469027335031 ) ) ;
#7422 = CARTESIAN_POINT ( 'NONE',  ( 5.895596859100789899, 12.98270243688433645, -15.36156309259591701 ) ) ;
#7423 = CARTESIAN_POINT ( 'NONE',  ( 4.549368137175248350, 35.80950303116100741, -23.67244292351601942 ) ) ;
#7424 = ORIENTED_EDGE ( 'NONE', *, *, #9041, .F. ) ;
#7425 = CARTESIAN_POINT ( 'NONE',  ( 4.956653778116990594, -32.11725092155016625, -35.79382859084151391 ) ) ;
#7426 = CARTESIAN_POINT ( 'NONE',  ( 0.5998501479064708430, 6.798102206414135651, -47.62484632993681544 ) ) ;
#7427 = ORIENTED_EDGE ( 'NONE', *, *, #23305, .F. ) ;
#7428 = CARTESIAN_POINT ( 'NONE',  ( 5.965394784446460541, 19.82223131420046869, 5.326334832595717828 ) ) ;
#7429 = CARTESIAN_POINT ( 'NONE',  ( 0.5824935313925939662, 37.02861770305457156, 28.77706809344680750 ) ) ;
#7431 = EDGE_CURVE ( 'NONE', #29097, #56408, #49563, .T. ) ;
#7430 = CARTESIAN_POINT ( 'NONE',  ( 0.8554163680231708922, 3.785871848716424903, 46.76401017296224438 ) ) ;
#7432 = CARTESIAN_POINT ( 'NONE',  ( -6.017396004339687465, -14.94857180791985130, -11.47192209077602776 ) ) ;
#7433 = CARTESIAN_POINT ( 'NONE',  ( 0.8557997880470697982, -47.37054680076710866, 7.156447707085535903 ) ) ;
#7434 = CARTESIAN_POINT ( 'NONE',  ( 2.281351352603289584, -19.56575819747254741, 43.80196780981711413 ) ) ;
#7435 = CARTESIAN_POINT ( 'NONE',  ( 4.962356264823608143, 0.000000000000000000, 0.000000000000000000 ) ) ;
#7436 = CARTESIAN_POINT ( 'NONE',  ( 0.1135584504625007929, -12.13985218845071579, -42.42141017196176023 ) ) ;
#7437 = CARTESIAN_POINT ( 'NONE',  ( 4.553261556744875094, -41.61700166486733110, -14.05577241741153216 ) ) ;
#7438 = CIRCLE ( 'NONE', #57421, 43.08621763946400307 ) ;
#7439 = CARTESIAN_POINT ( 'NONE',  ( 0.6253024248130485407, 4.031273609322430396, 48.94070964447109162 ) ) ;
#7440 = FACE_OUTER_BOUND ( 'NONE', #38323, .T. ) ;
#7441 =( NAMED_UNIT ( * ) PLANE_ANGLE_UNIT ( ) SI_UNIT ( $, .RADIAN. ) );
#7442 = CARTESIAN_POINT ( 'NONE',  ( 0.5848930533535030563, -38.76613696830708733, 26.39052305169438029 ) ) ;
#7443 = LINE ( 'NONE', #12813, #42522 ) ;
#7444 = CARTESIAN_POINT ( 'NONE',  ( 1.092182651088188017, 38.88600182739025968, 15.64097331761952425 ) ) ;
#7445 = B_SPLINE_CURVE_WITH_KNOTS ( 'NONE', 3,
 ( #11995, #24834, #43972, #48944, #58310, #25132 ),
 .UNSPECIFIED., .F., .F.,
 ( 4, 2, 4 ),
 ( 3.471140604459641645E-18, 0.0002291459268755755203, 0.0004582918537511475711 ),
 .UNSPECIFIED. ) ;
#7446 = B_SPLINE_CURVE_WITH_KNOTS ( 'NONE', 3,
 ( #1459, #54696, #10580, #30591, #21207, #39413 ),
 .UNSPECIFIED., .F., .F.,
 ( 4, 2, 4 ),
 ( 8.673617379884034509E-19, 0.0002291459268755708311, 0.0004582918537511407949 ),
 .UNSPECIFIED. ) ;
#7447 = ORIENTED_EDGE ( 'NONE', *, *, #56084, .F. ) ;
#7448 = CARTESIAN_POINT ( 'NONE',  ( 5.895596859100789899, -2.016778947468235828, 20.01151633159107845 ) ) ;
#7449 = CARTESIAN_POINT ( 'NONE',  ( 0.1101816497532063094, 43.12424935764384060, -0.1358190954551057039 ) ) ;
#7450 = CARTESIAN_POINT ( 'NONE',  ( 0.1145239942831223490, -38.28493031833373550, -21.93648994768771132 ) ) ;
#7451 = CARTESIAN_POINT ( 'NONE',  ( 0.9972139404380313543, -25.59643345733252318, 34.43899251299762199 ) ) ;
#7452 = ORIENTED_EDGE ( 'NONE', *, *, #34318, .F. ) ;
#7453 = ADVANCED_FACE ( 'NONE', ( #56321 ), #32579, .F. ) ;
#7454 = CARTESIAN_POINT ( 'NONE',  ( 0.6067099128993201917, 17.67241243535543305, -44.51753430581923254 ) ) ;
#7455 = CARTESIAN_POINT ( 'NONE',  ( 4.303969348037246512, -22.16169334783807443, -42.70173985163840058 ) ) ;
#7456 = B_SPLINE_CURVE_WITH_KNOTS ( 'NONE', 3,
 ( #57213, #9626, #203, #51922, #32843, #4588 ),
 .UNSPECIFIED., .F., .F.,
 ( 4, 2, 4 ),
 ( 0.002336974151641604130, 0.003500975885716476211, 0.004664977619791348291 ),
 .UNSPECIFIED. ) ;
#7457 = EDGE_CURVE ( 'NONE', #30599, #28421, #18565, .T. ) ;
#7458 = LINE ( 'NONE', #10967, #8517 ) ;
#7459 = ORIENTED_EDGE ( 'NONE', *, *, #9120, .F. ) ;
#7460 = VECTOR ( 'NONE', #50221, 1000.000000000000000 ) ;
#7461 = EDGE_CURVE ( 'NONE', #11438, #18533, #46989, .T. ) ;
#7462 = FACE_OUTER_BOUND ( 'NONE', #48271, .T. ) ;
#7463 = VERTEX_POINT ( 'NONE', #42267 ) ;
#7464 = CARTESIAN_POINT ( 'NONE',  ( 0.5839879882074149320, -2.012401402563926455E-05, -47.89596766821756546 ) ) ;
#7465 = CARTESIAN_POINT ( 'NONE',  ( 0.6009452777970409887, -28.93864923253926946, 38.43042656245023636 ) ) ;
#7466 = B_SPLINE_CURVE_WITH_KNOTS ( 'NONE', 3,
 ( #54486, #46368, #51036, #17543 ),
 .UNSPECIFIED., .F., .F.,
 ( 4, 4 ),
 ( 8.673617379884035472E-19, 0.004041751736740989941 ),
 .UNSPECIFIED. ) ;
#7467 = ORIENTED_EDGE ( 'NONE', *, *, #33673, .F. ) ;
#7468 = CARTESIAN_POINT ( 'NONE',  ( 4.956653778116989706, -42.88673967249116004, -21.75875759808752008 ) ) ;
#7469 = ORIENTED_EDGE ( 'NONE', *, *, #60436, .F. ) ;
#7470 = LINE ( 'NONE', #26918, #13736 ) ;
#7471 = CARTESIAN_POINT ( 'NONE',  ( 5.000000000000013323, -85.00000000000001421, -9.629649721936174886E-32 ) ) ;
#7472 = B_SPLINE_CURVE_WITH_KNOTS ( 'NONE', 3,
 ( #28374, #47495, #32789, #19004, #9572, #18684 ),
 .UNSPECIFIED., .F., .F.,
 ( 4, 2, 4 ),
 ( 3.476216610979977084E-18, 0.0002291966416970803253, 0.0004583932833941571812 ),
 .UNSPECIFIED. ) ;
#7473 = ORIENTED_EDGE ( 'NONE', *, *, #23305, .T. ) ;
#7474 = CARTESIAN_POINT ( 'NONE',  ( 0.1129192098497447394, 36.71339784380064231, -24.47607416535520741 ) ) ;
#7475 = ORIENTED_EDGE ( 'NONE', *, *, #37879, .T. ) ;
#7476 = CARTESIAN_POINT ( 'NONE',  ( 0.5837374860065643878, -38.10878877974126056, -29.01294733976400408 ) ) ;
#7477 = CONICAL_SURFACE ( 'NONE', #37537, 4.000000000000000000, 1.047197551196595855 ) ;
#7478 = ORIENTED_EDGE ( 'NONE', *, *, #34956, .F. ) ;
#7479 = EDGE_CURVE ( 'NONE', #11294, #2547, #61025, .T. ) ;
#7480 = ORIENTED_EDGE ( 'NONE', *, *, #257, .F. ) ;
#7481 = CARTESIAN_POINT ( 'NONE',  ( -6.016761891674564211, -9.424569481870138432, -16.31696541414282109 ) ) ;
#7482 = CARTESIAN_POINT ( 'NONE',  ( 3.270143674763207553, -9.482922169188032768, 9.870732238228487887 ) ) ;
#7483 = CARTESIAN_POINT ( 'NONE',  ( 1.157643937452369709, -37.77649500668685079, -18.16421480836746483 ) ) ;
#7484 = VECTOR ( 'NONE', #19976, 1000.000000000000000 ) ;
#7485 = CARTESIAN_POINT ( 'NONE',  ( 5.838029081930955932, -43.49392513872165011, 18.42127938499921314 ) ) ;
#7486 = CARTESIAN_POINT ( 'NONE',  ( 0.6031356219577718170, 44.47888959008672316, 18.32926896140846296 ) ) ;
#7487 = EDGE_LOOP ( 'NONE', ( #36785, #12533, #57073, #23756 ) ) ;
#7488 = CARTESIAN_POINT ( 'NONE',  ( 4.956653778116975495, -39.67974989265057673, 27.17045123668458828 ) ) ;
#7489 = EDGE_CURVE ( 'NONE', #26742, #14506, #31203, .T. ) ;
#7490 = CARTESIAN_POINT ( 'NONE',  ( 4.303969348037258058, -4.133486515473634881, 47.93217632892346813 ) ) ;
#7491 = CARTESIAN_POINT ( 'NONE',  ( 4.335381028904216727, -48.81116855472415494, -4.150502618557639245 ) ) ;
#7492 = VECTOR ( 'NONE', #43754, 1000.000000000000000 ) ;
#7493 = EDGE_LOOP ( 'NONE', ( #55188, #46058, #60252, #24923 ) ) ;
#7494 = EDGE_CURVE ( 'NONE', #14527, #19512, #20565, .T. ) ;
#7495 = ORIENTED_EDGE ( 'NONE', *, *, #47385, .F. ) ;
#7496 = CARTESIAN_POINT ( 'NONE',  ( 0.1073791018717483448, -21.98088480513640874, -37.10214135362880228 ) ) ;
#7497 = CARTESIAN_POINT ( 'NONE',  ( -6.057079549204054558, -8.899553672604694654, -17.07715361318058811 ) ) ;
#7498 = ORIENTED_EDGE ( 'NONE', *, *, #47425, .F. ) ;
#7499 = CARTESIAN_POINT ( 'NONE',  ( 0.1102847568649952675, -42.76743495471826151, -5.537466591275519434 ) ) ;
#7500 = B_SPLINE_CURVE_WITH_KNOTS ( 'NONE', 3,
 ( #10704, #342, #48595, #24168, #1273, #24482 ),
 .UNSPECIFIED., .F., .F.,
 ( 4, 2, 4 ),
 ( 8.770652787438942800E-18, 0.0002448709889506568314, 0.0004897419779013048808 ),
 .UNSPECIFIED. ) ;
#7501 = CARTESIAN_POINT ( 'NONE',  ( 1.112077966505210957, -34.68817258157839234, 27.19854790387139332 ) ) ;
#7502 = ORIENTED_EDGE ( 'NONE', *, *, #24386, .F. ) ;
#7503 = CARTESIAN_POINT ( 'NONE',  ( -6.015611763856276717, 13.32857883366851937, -13.31979030221785365 ) ) ;
#7504 = ORIENTED_EDGE ( 'NONE', *, *, #22869, .F. ) ;
#7505 = DIRECTION ( 'NONE',  ( -0.07836865515943411409, 0.2503967164834599024, -0.9649662368512192945 ) ) ;
#7507 = EDGE_CURVE ( 'NONE', #21289, #35184, #28136, .T. ) ;
#7506 = DIRECTION ( 'NONE',  ( 0.000000000000000000, 1.224646799147353207E-16, 1.000000000000000000 ) ) ;
#7508 = CARTESIAN_POINT ( 'NONE',  ( 0.9787464366903567692, 9.887393718638527673, -40.72558702269483177 ) ) ;
#7509 = SHAPE_REPRESENTATION_RELATIONSHIP ( 'NONE' , 'NONE' ,  #42491, #32490 ) ;
#7510 = CARTESIAN_POINT ( 'NONE',  ( 0.8751705887134423323, -5.393078191592370452, -47.79200036674278351 ) ) ;
#7511 =( BOUNDED_SURFACE ( )  B_SPLINE_SURFACE ( 3, 1, ( 
 ( #50540, #26745 ),
 ( #36787, #59627 ),
 ( #3530, #17353 ),
 ( #41798, #7615 ) ),
 .UNSPECIFIED., .F., .F., .F. ) 
 B_SPLINE_SURFACE_WITH_KNOTS ( ( 4, 4 ),
 ( 2, 2 ),
 ( 0.000000000000000000, 1.000000000000000000 ),
 ( 0.000000000000000000, 1.000000000000000000 ),
 .UNSPECIFIED. ) 
 GEOMETRIC_REPRESENTATION_ITEM ( )  RATIONAL_B_SPLINE_SURFACE ( (
 ( 1.000000000000000000, 1.000000000000000000),
 ( 0.9952954269826590483, 0.8620686068821307169),
 ( 0.9952954269826590483, 0.8620686068821307169),
 ( 1.000000000000000000, 1.000000000000000000) ) ) 
 REPRESENTATION_ITEM ( '' )  SURFACE ( )  );
#7512 = ORIENTED_EDGE ( 'NONE', *, *, #46999, .T. ) ;
#7513 = CARTESIAN_POINT ( 'NONE',  ( 1.000433927950264756, 10.35500712260046896, 40.61025123221650546 ) ) ;
#7514 = DIRECTION ( 'NONE',  ( -1.000000000000000000, -0.000000000000000000, -0.000000000000000000 ) ) ;
#7515 = CARTESIAN_POINT ( 'NONE',  ( 4.967162193818130511, 36.06913038482799294, 23.56777426397191277 ) ) ;
#7516 = CARTESIAN_POINT ( 'NONE',  ( 0.1100053167205930632, 21.40663161100993506, -37.43629428538741877 ) ) ;
#7517 = CARTESIAN_POINT ( 'NONE',  ( 5.959547316686252039, -5.308980600728594013, 19.82715097195153220 ) ) ;
#7518 = CARTESIAN_POINT ( 'NONE',  ( 0.8560838555295223751, 31.94705745926225404, -34.34761059777416392 ) ) ;
#7519 = CARTESIAN_POINT ( 'NONE',  ( 1.140000000000009006, 0.000000000000000000, 0.000000000000000000 ) ) ;
#7520 = CARTESIAN_POINT ( 'NONE',  ( 0.5807400328401637335, 46.40483864045145168, 11.87003418057259374 ) ) ;
#7521 = B_SPLINE_CURVE_WITH_KNOTS ( 'NONE', 3,
 ( #55346, #17464, #8056, #32185, #27170, #32495 ),
 .UNSPECIFIED., .F., .F.,
 ( 4, 2, 4 ),
 ( 1.275615807185303638E-16, 0.0002450741128632383595, 0.0004901482257263492168 ),
 .UNSPECIFIED. ) ;
#7522 = CARTESIAN_POINT ( 'NONE',  ( 0.3622758884714600280, -0.8252992914331080954, 43.10531414739104150 ) ) ;
#7523 = VECTOR ( 'NONE', #54936, 1000.000000000000227 ) ;
#7524 = DIRECTION ( 'NONE',  ( 1.000000000000000000, 0.000000000000000000, 0.000000000000000000 ) ) ;
#7525 = CARTESIAN_POINT ( 'NONE',  ( 0.6039202388192953519, 27.95228209933789998, -40.37615185091348735 ) ) ;
#7526 = EDGE_LOOP ( 'NONE', ( #18611, #43041, #56619, #35940 ) ) ;
#7527 = CARTESIAN_POINT ( 'NONE',  ( 0.6064782688330876415, -46.09361631204276222, 8.643667144039953953 ) ) ;
#7528 = AXIS2_PLACEMENT_3D ( 'NONE', #7540, #2541, #40804 ) ;
#7529 = FACE_OUTER_BOUND ( 'NONE', #1003, .T. ) ;
#7530 = CARTESIAN_POINT ( 'NONE',  ( 3.727782113643637096, -41.93293375853455274, 13.20631827226376309 ) ) ;
#7531 = VERTEX_POINT ( 'NONE', #8717 ) ;
#7532 = EDGE_CURVE ( 'NONE', #3952, #55732, #6521, .T. ) ;
#7533 = CARTESIAN_POINT ( 'NONE',  ( 0.8751705887134553219, 47.79200036674271956, 5.393078191592866055 ) ) ;
#7534 = CIRCLE ( 'NONE', #33593, 42.08604991992415023 ) ;
#7535 = CARTESIAN_POINT ( 'NONE',  ( 0.1129192098497455998, 3.754263797494300725, 43.96427289429426821 ) ) ;
#7536 = EDGE_CURVE ( 'NONE', #46801, #6622, #55156, .T. ) ;
#7537 = FACE_OUTER_BOUND ( 'NONE', #45126, .T. ) ;
#7538 = ORIENTED_EDGE ( 'NONE', *, *, #20951, .T. ) ;
#7539 = CARTESIAN_POINT ( 'NONE',  ( -11.40403086437694569, 0.6959691356230539583, -1.199999999999999956 ) ) ;
#7540 = CARTESIAN_POINT ( 'NONE',  ( 4.553261556744875094, 0.000000000000000000, 0.000000000000000000 ) ) ;
#7541 = ADVANCED_FACE ( 'NONE', ( #12832 ), #2908, .F. ) ;
#7542 = CARTESIAN_POINT ( 'NONE',  ( 3.894904216938898323, -10.35809250500306611, 42.71807875050094339 ) ) ;
#7543 = ORIENTED_EDGE ( 'NONE', *, *, #38102, .T. ) ;
#7544 = DIRECTION ( 'NONE',  ( 0.09722883295013591554, -0.7096678276952463893, 0.6977951908529210767 ) ) ;
#7545 = EDGE_CURVE ( 'NONE', #14372, #5781, #39585, .T. ) ;
#7546 = ORIENTED_EDGE ( 'NONE', *, *, #25338, .F. ) ;
#7547 = ORIENTED_EDGE ( 'NONE', *, *, #50417, .T. ) ;
#7548 = CARTESIAN_POINT ( 'NONE',  ( 0.5797568599927126476, 21.98355117866222130, 41.42401219396963796 ) ) ;
#7549 = ORIENTED_EDGE ( 'NONE', *, *, #51958, .T. ) ;
#7550 = CARTESIAN_POINT ( 'NONE',  ( -6.078457390727109555, 19.25602481922002340, -0.004381676659706296682 ) ) ;
#7551 = B_SPLINE_CURVE_WITH_KNOTS ( 'NONE', 3,
 ( #21728, #26115, #41475, #40868, #55530, #50842 ),
 .UNSPECIFIED., .F., .F.,
 ( 4, 2, 4 ),
 ( 0.000000000000000000, 0.0002291966416970789701, 0.0004583932833941579401 ),
 .UNSPECIFIED. ) ;
#7552 = ORIENTED_EDGE ( 'NONE', *, *, #43108, .T. ) ;
#7553 = CARTESIAN_POINT ( 'NONE',  ( 0.6039202388192953519, -42.87364092186805209, -23.94607748571178973 ) ) ;
#7554 = B_SPLINE_CURVE_WITH_KNOTS ( 'NONE', 3,
 ( #58529, #45404, #58845, #1837, #25652, #2453 ),
 .UNSPECIFIED., .F., .F.,
 ( 4, 2, 4 ),
 ( 1.500335247250105340E-16, 0.0002445252820015200571, 0.0004890505640028900607 ),
 .UNSPECIFIED. ) ;
#7555 = EDGE_CURVE ( 'NONE', #43681, #17235, #20782, .T. ) ;
#7556 = CARTESIAN_POINT ( 'NONE',  ( 4.975801465491695552, -35.64402118370979622, 32.01766832630250548 ) ) ;
#7557 = ADVANCED_FACE ( 'NONE', ( #19074 ), #47566, .F. ) ;
#7558 = ORIENTED_EDGE ( 'NONE', *, *, #4186, .T. ) ;
#7559 = CARTESIAN_POINT ( 'NONE',  ( 0.1149546198390367924, 43.36205231031419061, -8.165720082196996188 ) ) ;
#7560 = CARTESIAN_POINT ( 'NONE',  ( 4.956445790444005794, -36.61936279692559992, -29.60676136437043127 ) ) ;
#7561 = CARTESIAN_POINT ( 'NONE',  ( 0.9268187852002115479, -37.91842020551887060, 22.49328215326355718 ) ) ;
#7562 = CARTESIAN_POINT ( 'NONE',  ( 0.5980271706414711508, -7.146479349117414337, -48.58988655836006387 ) ) ;
#7563 = VERTEX_POINT ( 'NONE', #24369 ) ;
#7564 = CARTESIAN_POINT ( 'NONE',  ( 3.678834586032788234, 2.858786927004010270, 48.89212315838150857 ) ) ;
#7565 = ORIENTED_EDGE ( 'NONE', *, *, #46023, .T. ) ;
#7566 = CARTESIAN_POINT ( 'NONE',  ( 0.9745511491811745808, -42.90705396078544709, -0.3405614984925067756 ) ) ;
#7567 =( BOUNDED_SURFACE ( )  B_SPLINE_SURFACE ( 3, 1, ( 
 ( #9750, #28856 ),
 ( #57641, #14776 ),
 ( #33889, #52965 ),
 ( #29166, #39524 ) ),
 .UNSPECIFIED., .F., .F., .F. ) 
 B_SPLINE_SURFACE_WITH_KNOTS ( ( 4, 4 ),
 ( 2, 2 ),
 ( 0.000000000000000000, 1.000000000000000000 ),
 ( 0.000000000000000000, 1.000000000000000000 ),
 .UNSPECIFIED. ) 
 GEOMETRIC_REPRESENTATION_ITEM ( )  RATIONAL_B_SPLINE_SURFACE ( (
 ( 1.000000000000000000, 1.000000000000000000),
 ( 0.9751682680413298332, 0.9999560080971552356),
 ( 0.9751682680413298332, 0.9999560080971552356),
 ( 1.000000000000000000, 1.000000000000000000) ) ) 
 REPRESENTATION_ITEM ( '' )  SURFACE ( )  );
#7568 = CARTESIAN_POINT ( 'NONE',  ( 0.9754642270333685472, 25.98138239028857654, 34.14824330022339183 ) ) ;
#7569 = B_SPLINE_CURVE_WITH_KNOTS ( 'NONE', 3,
 ( #60295, #42471, #8002, #41857 ),
 .UNSPECIFIED., .F., .F.,
 ( 4, 4 ),
 ( 0.000000000000000000, 0.004446090762761378996 ),
 .UNSPECIFIED. ) ;
#7570 = CARTESIAN_POINT ( 'NONE',  ( 0.3622758884714600280, 17.25816669464994746, -39.50828911766980411 ) ) ;
#7571 = VERTEX_POINT ( 'NONE', #541 ) ;
#7572 = DIRECTION ( 'NONE',  ( -1.000000000000000000, -0.000000000000000000, -0.000000000000000000 ) ) ;
#7573 = CARTESIAN_POINT ( 'NONE',  ( 0.6000166863083106206, -2.096232480232000039, 49.06556115135416007 ) ) ;
#7574 = CARTESIAN_POINT ( 'NONE',  ( 0.6008122571543325074, 28.45128890504206609, 40.02597544229430326 ) ) ;
#7575 = CARTESIAN_POINT ( 'NONE',  ( 0.6017667736363749853, -41.48674115080387281, -24.35549005323402127 ) ) ;
#7577 = ORIENTED_EDGE ( 'NONE', *, *, #57264, .F. ) ;
#7576 = AXIS2_PLACEMENT_3D ( 'NONE', #24361, #534, #19669 ) ;
#7578 = EDGE_LOOP ( 'NONE', ( #18913, #10567, #36025, #18361 ) ) ;
#7579 = LINE ( 'NONE', #27946, #32967 ) ;
#7580 = CARTESIAN_POINT ( 'NONE',  ( 4.956445790444010235, -22.15545010017738647, -41.55326799420456751 ) ) ;
#7581 = CARTESIAN_POINT ( 'NONE',  ( 0.9736507210033072957, -16.83559693395292101, 39.46762617149627772 ) ) ;
#7582 = AXIS2_PLACEMENT_3D ( 'NONE', #48912, #19807, #20412 ) ;
#7584 = ADVANCED_FACE ( 'NONE', ( #43818 ), #15740, .F. ) ;
#7583 = CARTESIAN_POINT ( 'NONE',  ( 0.6017667736363752073, 6.625250263233628978, -47.64919355032682091 ) ) ;
#7585 =( BOUNDED_SURFACE ( )  B_SPLINE_SURFACE ( 3, 1, ( 
 ( #1212, #44182 ),
 ( #16567, #35381 ),
 ( #39789, #52675 ),
 ( #40101, #20958 ) ),
 .UNSPECIFIED., .F., .F., .F. ) 
 B_SPLINE_SURFACE_WITH_KNOTS ( ( 4, 4 ),
 ( 2, 2 ),
 ( 0.000000000000000000, 1.000000000000000000 ),
 ( 0.000000000000000000, 1.000000000000000000 ),
 .UNSPECIFIED. ) 
 GEOMETRIC_REPRESENTATION_ITEM ( )  RATIONAL_B_SPLINE_SURFACE ( (
 ( 1.000000000000000000, 1.000000000000000000),
 ( 0.9953040768229013402, 0.8617119497784988535),
 ( 0.9953040768229013402, 0.8617119497784988535),
 ( 1.000000000000000000, 1.000000000000000000) ) ) 
 REPRESENTATION_ITEM ( '' )  SURFACE ( )  );
#7586 = ADVANCED_FACE ( 'NONE', ( #52867 ), #60530, .F. ) ;
#7587 = CARTESIAN_POINT ( 'NONE',  ( -6.016489644550737204, -14.95199950534956201, 11.46752133529379414 ) ) ;
#7588 = CARTESIAN_POINT ( 'NONE',  ( 3.270143674763207553, 12.53844339339234715, 5.490410281242826152 ) ) ;
#7589 = LINE ( 'NONE', #49584, #52739 ) ;
#7590 = AXIS2_PLACEMENT_3D ( 'NONE', #27190, #17183, #27489 ) ;
#7591 = CARTESIAN_POINT ( 'NONE',  ( 0.8554163680231816613, 36.24698750680841641, -29.78861141095861242 ) ) ;
#7592 = CARTESIAN_POINT ( 'NONE',  ( 0.000000000000000000, 5.051668046482832750E-16, -4.000000000000000000 ) ) ;
#7593 = CARTESIAN_POINT ( 'NONE',  ( 0.9784957157296348962, 33.03361919771707278, 25.78978595670369600 ) ) ;
#7594 = CARTESIAN_POINT ( 'NONE',  ( 1.231276596079887264, 35.62927148397050559, -22.08691432816256395 ) ) ;
#7595 = CARTESIAN_POINT ( 'NONE',  ( 0.1073791018717578927, -16.95003405440338895, 39.65380858626186722 ) ) ;
#7596 = DIRECTION ( 'NONE',  ( 0.000000000000000000, 1.000000000000000000, -1.224646799147353207E-16 ) ) ;
#7597 = CARTESIAN_POINT ( 'NONE',  ( 0.6029303876144825880, -6.149480157546260983, -47.71279573267356966 ) ) ;
#7598 = CARTESIAN_POINT ( 'NONE',  ( 0.3622758884714730732, -40.13994584881772454, -15.73321244754840720 ) ) ;
#7599 = CARTESIAN_POINT ( 'NONE',  ( 0.6008123274975391004, 16.55074354900158440, 46.23448322554973799 ) ) ;
#7600 = CARTESIAN_POINT ( 'NONE',  ( 4.975801465491695552, -26.14269827151708370, 40.15204426031488794 ) ) ;
#7602 = VERTEX_POINT ( 'NONE', #33474 ) ;
#7601 = FACE_OUTER_BOUND ( 'NONE', #19359, .T. ) ;
#7603 = ORIENTED_EDGE ( 'NONE', *, *, #45100, .F. ) ;
#7604 = CARTESIAN_POINT ( 'NONE',  ( 0.6029443199889047422, 16.95996013332177554, -46.08576129490039364 ) ) ;
#7605 = CARTESIAN_POINT ( 'NONE',  ( 3.221118495291109163, 2.339734729467391805, -43.92365036125158184 ) ) ;
#7606 = CARTESIAN_POINT ( 'NONE',  ( 4.967162193818130511, 0.000000000000000000, 0.000000000000000000 ) ) ;
#7607 = VERTEX_POINT ( 'NONE', #19998 ) ;
#7608 = ORIENTED_EDGE ( 'NONE', *, *, #37077, .T. ) ;
#7609 = DIRECTION ( 'NONE',  ( -1.000000000000000000, -0.000000000000000000, -0.000000000000000000 ) ) ;
#7610 = CARTESIAN_POINT ( 'NONE',  ( 0.8753041380234530822, -39.87785955339003863, -28.65125905284232743 ) ) ;
#7611 = B_SPLINE_CURVE_WITH_KNOTS ( 'NONE', 3,
 ( #47176, #19288, #18668, #18364, #51849, #14286 ),
 .UNSPECIFIED., .F., .F.,
 ( 4, 2, 4 ),
 ( 0.000000000000000000, 0.0002447195606305755050, 0.0004894391212611510101 ),
 .UNSPECIFIED. ) ;
#7612 = EDGE_CURVE ( 'NONE', #19850, #41574, #31995, .T. ) ;
#7613 = VERTEX_POINT ( 'NONE', #9644 ) ;
#7614 = ORIENTED_EDGE ( 'NONE', *, *, #32151, .F. ) ;
#7615 = CARTESIAN_POINT ( 'NONE',  ( 0.5804410086790514622, 45.37396088368706870, 11.86269470150153005 ) ) ;
#7616 = AXIS2_PLACEMENT_3D ( 'NONE', #40144, #1872, #11607 ) ;
#7617 = EDGE_CURVE ( 'NONE', #9846, #40367, #11811, .T. ) ;
#7618 = EDGE_CURVE ( 'NONE', #41383, #58552, #38657, .T. ) ;
#7619 = CARTESIAN_POINT ( 'NONE',  ( -6.016489644550737204, 13.32727118274456579, -13.32104266208085619 ) ) ;
#7620 = TOROIDAL_SURFACE ( 'NONE', #50641, 5.633200000000004870, 0.02570000000000154800 ) ;
#7621 = CARTESIAN_POINT ( 'NONE',  ( 4.291220156522060236, 26.18147253908353989, -39.16528428328985711 ) ) ;
#7622 = CIRCLE ( 'NONE', #56637, 15.43999999999999240 ) ;
#7623 = ADVANCED_FACE ( 'NONE', ( #54385 ), #34583, .F. ) ;
#7624 = VERTEX_POINT ( 'NONE', #30288 ) ;
#7625 = DIRECTION ( 'NONE',  ( 0.000000000000000000, 0.000000000000000000, 1.000000000000000000 ) ) ;
#7626 = FACE_OUTER_BOUND ( 'NONE', #23273, .T. ) ;
#7627 = ADVANCED_FACE ( 'NONE', ( #34701, #15596 ), #40653, .F. ) ;
#7628 = DIRECTION ( 'NONE',  ( -1.000000000000000000, 0.000000000000000000, 0.000000000000000000 ) ) ;
#7629 = EDGE_LOOP ( 'NONE', ( #39308, #58785, #53524, #20887 ) ) ;
#7630 = ORIENTED_EDGE ( 'NONE', *, *, #41755, .T. ) ;
#7631 = CARTESIAN_POINT ( 'NONE',  ( 1.227938101723748288, -0.8460948827228147451, 42.91134962331487657 ) ) ;
#7632 = EDGE_LOOP ( 'NONE', ( #29744, #25347, #28080, #48019 ) ) ;
#7633 = CARTESIAN_POINT ( 'NONE',  ( 0.6846871229502899947, -33.25969555998767646, 34.48177377577824387 ) ) ;
#7634 = CARTESIAN_POINT ( 'NONE',  ( 0.5980271706414711508, -24.85837266090859998, -42.35694218771055830 ) ) ;
#7635 = DIRECTION ( 'NONE',  ( -1.000000000000000000, -0.000000000000000000, -0.000000000000000000 ) ) ;
#7636 = CARTESIAN_POINT ( 'NONE',  ( 0.5830081025819929819, -38.50771568613562579, 26.76542297476333232 ) ) ;
#7637 = LINE ( 'NONE', #25836, #10390 ) ;
#7638 = VERTEX_POINT ( 'NONE', #58776 ) ;
#7639 = CARTESIAN_POINT ( 'NONE',  ( 0.9752132459055852243, -30.50512806189389892, -30.17566824627277100 ) ) ;
#7640 = CARTESIAN_POINT ( 'NONE',  ( 4.335381028904201628, -47.87967504119353634, 10.35826074271415287 ) ) ;
#7641 = B_SPLINE_CURVE_WITH_KNOTS ( 'NONE', 3,
 ( #24294, #43428, #19610, #57785, #44357, #35566 ),
 .UNSPECIFIED., .F., .F.,
 ( 4, 2, 4 ),
 ( 8.492412771929966223E-17, 0.0002293366620881466381, 0.0004586733241762083833 ),
 .UNSPECIFIED. ) ;
#7642 = CARTESIAN_POINT ( 'NONE',  ( 0.9736507210033050752, -21.06291100879414913, -37.38294557109060179 ) ) ;
#7643 = EDGE_LOOP ( 'NONE', ( #12045, #43094, #54229, #46907 ) ) ;
#7644 = CARTESIAN_POINT ( 'NONE',  ( 0.1073791018717483448, 42.68962945260953035, -6.109314776652274404 ) ) ;
#7645 = CARTESIAN_POINT ( 'NONE',  ( 0.5782707292762423457, -29.72436028066441338, 36.27945368404655113 ) ) ;
#7646 = CARTESIAN_POINT ( 'NONE',  ( 4.956445790443988031, 0.000000000000000000, 0.000000000000000000 ) ) ;
#7647 = CARTESIAN_POINT ( 'NONE',  ( 5.910764540655178756, -19.93069368583282142, 2.696050383554946084 ) ) ;
#7648 = ORIENTED_EDGE ( 'NONE', *, *, #42294, .F. ) ;
#7649 = CARTESIAN_POINT ( 'NONE',  ( 2.648799415243696664, -40.11112523584315426, 28.20664984722760948 ) ) ;
#7650 = CARTESIAN_POINT ( 'NONE',  ( 0.3622758884714600280, 34.70015533914828865, -25.58609868863731407 ) ) ;
#7651 = CARTESIAN_POINT ( 'NONE',  ( 0.6001305935487315502, -0.5236757026886070809, -48.10757715638248300 ) ) ;
#7652 = LINE ( 'NONE', #11777, #21462 ) ;
#7653 = CARTESIAN_POINT ( 'NONE',  ( -6.015611763856276717, -16.32183393015590056, -9.416239407363475422 ) ) ;
#7654 = CARTESIAN_POINT ( 'NONE',  ( 0.5850706913938533704, -29.30134895053080868, 37.88789093229795668 ) ) ;
#7655 = EDGE_CURVE ( 'NONE', #4461, #11343, #11542, .T. ) ;
#7656 = CARTESIAN_POINT ( 'NONE',  ( 0.5800708119828335008, -47.56394195701282968, -5.628966929618236748 ) ) ;
#7657 = CARTESIAN_POINT ( 'NONE',  ( 4.962356264823598373, -19.84272732133986139, 37.11471096901200895 ) ) ;
#7658 = VECTOR ( 'NONE', #27391, 1000.000000000000000 ) ;
#7659 = CARTESIAN_POINT ( 'NONE',  ( 0.6016117650947689910, 40.96537808716857398, -27.08115308512227060 ) ) ;
#7660 =( BOUNDED_SURFACE ( )  B_SPLINE_SURFACE ( 3, 1, ( 
 ( #29864, #28946 ),
 ( #33974, #24242 ),
 ( #48062, #38073 ),
 ( #5113, #413 ) ),
 .UNSPECIFIED., .F., .F., .F. ) 
 B_SPLINE_SURFACE_WITH_KNOTS ( ( 4, 4 ),
 ( 2, 2 ),
 ( 0.000000000000000000, 1.000000000000000000 ),
 ( 0.000000000000000000, 1.000000000000000000 ),
 .UNSPECIFIED. ) 
 GEOMETRIC_REPRESENTATION_ITEM ( )  RATIONAL_B_SPLINE_SURFACE ( (
 ( 1.000000000000000000, 1.000000000000000000),
 ( 0.7211978278499968642, 0.9934217856018975334),
 ( 0.7211978278499968642, 0.9934217856018975334),
 ( 1.000000000000000000, 1.000000000000000000) ) ) 
 REPRESENTATION_ITEM ( '' )  SURFACE ( )  );
#7661 = CARTESIAN_POINT ( 'NONE',  ( 0.5800708057587371513, -18.90714313908690869, 44.00606528161381448 ) ) ;
#7662 = ORIENTED_EDGE ( 'NONE', *, *, #5553, .F. ) ;
#7663 = CONICAL_SURFACE ( 'NONE', #35701, 43.92652462719577500, 1.486293639869522343 ) ;
#7664 = B_SPLINE_CURVE_WITH_KNOTS ( 'NONE', 3,
 ( #47925, #9378, #52911, #4651, #42928, #14719 ),
 .UNSPECIFIED., .F., .F.,
 ( 4, 2, 4 ),
 ( 7.040638946443416885E-18, 0.0002445244328975378903, 0.0004890488657950687332 ),
 .UNSPECIFIED. ) ;
#7665 = CIRCLE ( 'NONE', #42710, 4.250000000000000000 ) ;
#7666 = CARTESIAN_POINT ( 'NONE',  ( 0.5809828226811553087, 11.86925843957232729, -46.40184912890826752 ) ) ;
#7667 = CARTESIAN_POINT ( 'NONE',  ( 4.553261556744875094, 0.000000000000000000, 0.000000000000000000 ) ) ;
#7668 = CARTESIAN_POINT ( 'NONE',  ( 0.6067099128993221901, -13.08009036336170539, -46.07641759122979863 ) ) ;
#7669 = CARTESIAN_POINT ( 'NONE',  ( 1.227938101723748288, -4.762198645644156514, -42.65467462194923343 ) ) ;
#7670 = CARTESIAN_POINT ( 'NONE',  ( 0.6254087463353884546, -28.73645667569980233, 38.58044986685640509 ) ) ;
#7671 = CARTESIAN_POINT ( 'NONE',  ( 0.6846871229502932144, -47.60345020167355301, 5.395516691087021144 ) ) ;
#7672 = APPLICATION_PROTOCOL_DEFINITION ( 'draft international standard', 'automotive_design', 1998, #57535 ) ;
#7673 = CARTESIAN_POINT ( 'NONE',  ( 0.6023143664670691511, -44.54505257464873580, 18.16777128831313348 ) ) ;
#7674 = B_SPLINE_CURVE_WITH_KNOTS ( 'NONE', 3,
 ( #3519, #27657, #41786, #13889 ),
 .UNSPECIFIED., .F., .F.,
 ( 4, 4 ),
 ( 7.757919228897728493E-18, 0.005004741218457420607 ),
 .UNSPECIFIED. ) ;
#7675 = CARTESIAN_POINT ( 'NONE',  ( 0.6031356219577718170, 41.61861914321211486, -24.12932366310823440 ) ) ;
#7676 = CARTESIAN_POINT ( 'NONE',  ( 1.231276596079887931, -41.87427716283724521, -1.954912557623687652 ) ) ;
#7677 =( BOUNDED_SURFACE ( )  B_SPLINE_SURFACE ( 3, 1, ( 
 ( #26180, #35915 ),
 ( #60296, #16482 ),
 ( #17722, #17409 ),
 ( #40319, #59374 ) ),
 .UNSPECIFIED., .F., .F., .F. ) 
 B_SPLINE_SURFACE_WITH_KNOTS ( ( 4, 4 ),
 ( 2, 2 ),
 ( 0.000000000000000000, 1.000000000000000000 ),
 ( 0.000000000000000000, 1.000000000000000000 ),
 .UNSPECIFIED. ) 
 GEOMETRIC_REPRESENTATION_ITEM ( )  RATIONAL_B_SPLINE_SURFACE ( (
 ( 1.000000000000000000, 1.000000000000000000),
 ( 0.7282232189291693025, 0.9929344683865674037),
 ( 0.7282232189291693025, 0.9929344683865674037),
 ( 1.000000000000000000, 1.000000000000000000) ) ) 
 REPRESENTATION_ITEM ( '' )  SURFACE ( )  );
#7679 = EDGE_LOOP ( 'NONE', ( #1480, #38792, #47540, #22144 ) ) ;
#7678 = CARTESIAN_POINT ( 'NONE',  ( 0.5998501479064699549, 41.92175333043586960, 23.59887241503369282 ) ) ;
#7680 = ORIENTED_EDGE ( 'NONE', *, *, #61314, .F. ) ;
#7681 = DIRECTION ( 'NONE',  ( -1.000000000000000000, -0.000000000000000000, -0.000000000000000000 ) ) ;
#7682 = CARTESIAN_POINT ( 'NONE',  ( 0.5835226383429290564, -7.620528918417245556, 46.27277832105536959 ) ) ;
#7683 = CARTESIAN_POINT ( 'NONE',  ( 0.5848930533535030563, 22.69711449001842851, -41.03795896745540261 ) ) ;
#7684 =( BOUNDED_SURFACE ( )  B_SPLINE_SURFACE ( 3, 1, ( 
 ( #23320, #46516 ),
 ( #43059, #9513 ),
 ( #18624, #23020 ),
 ( #37433, #9210 ) ),
 .UNSPECIFIED., .F., .F., .F. ) 
 B_SPLINE_SURFACE_WITH_KNOTS ( ( 4, 4 ),
 ( 2, 2 ),
 ( 0.000000000000000000, 1.000000000000000000 ),
 ( 0.000000000000000000, 1.000000000000000000 ),
 .UNSPECIFIED. ) 
 GEOMETRIC_REPRESENTATION_ITEM ( )  RATIONAL_B_SPLINE_SURFACE ( (
 ( 1.000000000000000000, 1.000000000000000000),
 ( 0.7211978278499970862, 0.9934217856018976445),
 ( 0.7211978278499970862, 0.9934217856018976445),
 ( 1.000000000000000000, 1.000000000000000000) ) ) 
 REPRESENTATION_ITEM ( '' )  SURFACE ( )  );
#7685 = ORIENTED_EDGE ( 'NONE', *, *, #56701, .F. ) ;
#7686 = DIRECTION ( 'NONE',  ( -1.836909530733573776E-16, 1.000000000000000000, 0.000000000000000000 ) ) ;
#7687 = CYLINDRICAL_SURFACE ( 'NONE', #19196, 6.887500000000022382 ) ;
#7688 = DIRECTION ( 'NONE',  ( 1.000000000000000000, 0.000000000000000000, 0.000000000000000000 ) ) ;
#7689 = VECTOR ( 'NONE', #46690, 999.9999999999998863 ) ;
#7690 = EDGE_CURVE ( 'NONE', #52454, #3847, #47627, .T. ) ;
#7691 = VERTEX_POINT ( 'NONE', #39727 ) ;
#7692 = ORIENTED_EDGE ( 'NONE', *, *, #11259, .T. ) ;
#7693 = B_SPLINE_CURVE_WITH_KNOTS ( 'NONE', 3,
 ( #50451, #59531, #23416, #40465 ),
 .UNSPECIFIED., .F., .F.,
 ( 4, 4 ),
 ( 0.000000000000000000, 0.005004741218457412801 ),
 .UNSPECIFIED. ) ;
#7694 = EDGE_CURVE ( 'NONE', #7082, #38640, #58807, .T. ) ;
#7695 = FACE_OUTER_BOUND ( 'NONE', #23082, .T. ) ;
#7696 = EDGE_CURVE ( 'NONE', #34095, #11994, #2391, .T. ) ;
#7697 = CARTESIAN_POINT ( 'NONE',  ( 0.1073791018717578927, -10.69234304550026593, -41.77800844988510676 ) ) ;
#7698 = DIRECTION ( 'NONE',  ( -1.000000000000000000, -0.000000000000000000, -0.000000000000000000 ) ) ;
#7699 = ORIENTED_EDGE ( 'NONE', *, *, #60245, .T. ) ;
#7700 = ADVANCED_FACE ( 'NONE', ( #58469 ), #11340, .F. ) ;
#7701 = CARTESIAN_POINT ( 'NONE',  ( 2.706805983486679779, -43.97766765339521555, 1.655554616215038077 ) ) ;
#7702 = CARTESIAN_POINT ( 'NONE',  ( 0.1152809850208375564, -42.62447063833258909, -11.40612928611975896 ) ) ;
#7703 = CARTESIAN_POINT ( 'NONE',  ( 4.833616638992205949, -9.466882727842460099, 45.27110352095230184 ) ) ;
#7704 = CARTESIAN_POINT ( 'NONE',  ( 0.1158816050234199035, 33.60184995524097928, 28.59821184778224179 ) ) ;
#7705 = CONICAL_SURFACE ( 'NONE', #60739, 43.92652462719577500, 1.486293639869522343 ) ;
#7706 = ORIENTED_EDGE ( 'NONE', *, *, #6394, .T. ) ;
#7707 = CARTESIAN_POINT ( 'NONE',  ( 4.553261556744873317, 12.28162544311275006, -42.17465165592624032 ) ) ;
#7708 = EDGE_CURVE ( 'NONE', #59248, #21575, #49065, .T. ) ;
#7709 = SURFACE_STYLE_USAGE ( .BOTH. , #3310 ) ;
#7710 = PRESENTATION_LAYER_ASSIGNMENT (  '', '', ( #34752 ) ) ;
#7711 = AXIS2_PLACEMENT_3D ( 'NONE', #12927, #41744, #51405 ) ;
#7712 = VERTEX_POINT ( 'NONE', #49098 ) ;
#7713 = CARTESIAN_POINT ( 'NONE',  ( 0.6000166863083106206, -7.321729200002761395, -48.56146376737711279 ) ) ;
#7714 = CARTESIAN_POINT ( 'NONE',  ( 0.2885700199627498352, 34.69058524452978531, 25.60460887553389853 ) ) ;
#7715 = CARTESIAN_POINT ( 'NONE',  ( 2.526464513654347321, 31.23609615087176294, 29.52129845577943001 ) ) ;
#7716 =( NAMED_UNIT ( * ) SI_UNIT ( $, .STERADIAN. ) SOLID_ANGLE_UNIT ( ) );
#7717 = ADVANCED_FACE ( 'NONE', ( #59405 ), #22134, .F. ) ;
#7718 = ORIENTED_EDGE ( 'NONE', *, *, #39459, .F. ) ;
#7719 = ORIENTED_EDGE ( 'NONE', *, *, #40009, .F. ) ;
#7720 = CARTESIAN_POINT ( 'NONE',  ( 4.975801465491695552, 0.000000000000000000, 0.000000000000000000 ) ) ;
#7721 = CARTESIAN_POINT ( 'NONE',  ( 0.6031356219577719280, 44.41207482560206188, -18.49057407199411074 ) ) ;
#7722 = EDGE_LOOP ( 'NONE', ( #58392, #56760, #41324, #59807 ) ) ;
#7723 = DIRECTION ( 'NONE',  ( 1.000000000000000000, 0.000000000000000000, 0.000000000000000000 ) ) ;
#7724 = ORIENTED_EDGE ( 'NONE', *, *, #13980, .F. ) ;
#7725 = CARTESIAN_POINT ( 'NONE',  ( -6.016761891674564211, 7.214149619366359900, 17.40752468084784965 ) ) ;
#7726 = ORIENTED_EDGE ( 'NONE', *, *, #30854, .F. ) ;
#7727 = LINE ( 'NONE', #40360, #35705 ) ;
#7728 = CARTESIAN_POINT ( 'NONE',  ( 0.6026112563231247332, -48.68169479572535607, -6.452409373253833458 ) ) ;
#7729 = CARTESIAN_POINT ( 'NONE',  ( 0.1140933569871965675, -43.80888098664257058, 5.266108314694333714 ) ) ;
#7730 = EDGE_LOOP ( 'NONE', ( #48614, #32134, #34996, #379 ) ) ;
#7731 = CARTESIAN_POINT ( 'NONE',  ( 5.901463166500145796, 14.92627229327890426, -13.48051429907372878 ) ) ;
#7732 = CARTESIAN_POINT ( 'NONE',  ( 1.092182651088186018, -0.6199217264839108621, 41.90915033134549361 ) ) ;
#7733 = CARTESIAN_POINT ( 'NONE',  ( 0.8744876279028263033, 44.61213666265857825, -20.49651952824592982 ) ) ;
#7734 = ORIENTED_EDGE ( 'NONE', *, *, #28591, .T. ) ;
#7735 = ORIENTED_EDGE ( 'NONE', *, *, #34684, .T. ) ;
#7736 = CARTESIAN_POINT ( 'NONE',  ( 0.5987334363312686314, -38.99056171795593428, -29.85463118831556883 ) ) ;
#7737 = CARTESIAN_POINT ( 'NONE',  ( 0.5998501479064708430, -18.89267974119696447, 44.24259072156053918 ) ) ;
#7738 = CARTESIAN_POINT ( 'NONE',  ( 0.9769922540276056999, 38.75350856957730628, -15.95296613905461669 ) ) ;
#7739 = CARTESIAN_POINT ( 'NONE',  ( 3.999999999999990674, -2.309401076758548221, -0.3572655899081733644 ) ) ;
#7740 = ADVANCED_FACE ( 'NONE', ( #13363 ), #10549, .T. ) ;
#7741 = CARTESIAN_POINT ( 'NONE',  ( 0.3622758884714730732, 36.91764744403321430, -22.26738722580129348 ) ) ;
#7742 = VERTEX_POINT ( 'NONE', #31530 ) ;
#7743 = CIRCLE ( 'NONE', #43832, 6.728125000000022560 ) ;
#7744 = CARTESIAN_POINT ( 'NONE',  ( 5.838029081930955932, -46.81536740852278200, 6.275861100912162982 ) ) ;
#7745 = DIRECTION ( 'NONE',  ( -1.000000000000000000, -0.000000000000000000, -0.000000000000000000 ) ) ;
#7746 = EDGE_LOOP ( 'NONE', ( #3545, #35986, #21379, #59545 ) ) ;
#7748 = MANIFOLD_SOLID_BREP ( 'EndChamfer', #59047 ) ;
#7747 = CARTESIAN_POINT ( 'NONE',  ( 0.9756354156337455619, -30.43287766742269085, 30.24859376089808904 ) ) ;
#7749 = CARTESIAN_POINT ( 'NONE',  ( 0.9783242366443560822, -27.26157242999075692, 31.82987839830509103 ) ) ;
#7750 = CARTESIAN_POINT ( 'NONE',  ( 0.5806925824938511393, -42.09901922557415332, -20.66143612114853312 ) ) ;
#7751 = CARTESIAN_POINT ( 'NONE',  ( 0.5834584762367752697, 45.18130578213499859, 12.56525355233251062 ) ) ;
#7752 = CARTESIAN_POINT ( 'NONE',  ( 4.833616638992205949, -34.47248434257890182, -30.83411269743551841 ) ) ;
#7753 = CARTESIAN_POINT ( 'NONE',  ( 3.407937589446178528, 7.970324840162117397, -11.14158115674364957 ) ) ;
#7754 = DIRECTION ( 'NONE',  ( -1.000000000000000000, -1.836909530733573776E-16, 1.925929944387235853E-32 ) ) ;
#7755 = CARTESIAN_POINT ( 'NONE',  ( 0.1139756605157203201, -12.93522790580227877, -42.18572150289689660 ) ) ;
#7756 = CARTESIAN_POINT ( 'NONE',  ( 0.9757892942422816684, -39.62259979733192239, 16.46777583825590341 ) ) ;
#7757 = DIRECTION ( 'NONE',  ( -0.07836865515943412797, -0.7860872967108227805, 0.6131273243286198271 ) ) ;
#7758 = CARTESIAN_POINT ( 'NONE',  ( 0.6024113833632039894, 22.90686952850539626, -43.43750910796909181 ) ) ;
#7759 = CARTESIAN_POINT ( 'NONE',  ( 4.549368137175248350, 19.17571786012324608, -38.40568845698256695 ) ) ;
#7760 = AXIS2_PLACEMENT_3D ( 'NONE', #13943, #26089, #29547 ) ;
#7761 = VECTOR ( 'NONE', #48882, 1000.000000000000114 ) ;
#7762 = DIRECTION ( 'NONE',  ( -1.000000000000000000, -0.000000000000000000, -0.000000000000000000 ) ) ;
#7763 = CARTESIAN_POINT ( 'NONE',  ( -6.001507490154110336, -14.94036486426021249, 11.48377994779695754 ) ) ;
#7764 = CARTESIAN_POINT ( 'NONE',  ( 0.7413678028165011646, 16.10168025133689440, 41.05145533174129469 ) ) ;
#7765 = PRODUCT ( 'housing right', 'housing right', '', ( #12722 ) ) ;
#7766 = CARTESIAN_POINT ( 'NONE',  ( 0.5809828226811617480, -28.72298383114462439, -38.32755012159175578 ) ) ;
#7767 = CARTESIAN_POINT ( 'NONE',  ( 0.8557997880470697982, -47.89938907511594834, 0.9121262075944505110 ) ) ;
#7768 =( BOUNDED_SURFACE ( )  B_SPLINE_SURFACE ( 3, 1, ( 
 ( #20404, #33896 ),
 ( #5345, #15094 ),
 ( #9757, #34203 ),
 ( #53278, #15403 ) ),
 .UNSPECIFIED., .F., .F., .F. ) 
 B_SPLINE_SURFACE_WITH_KNOTS ( ( 4, 4 ),
 ( 2, 2 ),
 ( 0.000000000000000000, 1.000000000000000000 ),
 ( 0.000000000000000000, 1.000000000000000000 ),
 .UNSPECIFIED. ) 
 GEOMETRIC_REPRESENTATION_ITEM ( )  RATIONAL_B_SPLINE_SURFACE ( (
 ( 1.000000000000000000, 1.000000000000000000),
 ( 0.9953040768229013402, 0.8617119497784988535),
 ( 0.9953040768229013402, 0.8617119497784988535),
 ( 1.000000000000000000, 1.000000000000000000) ) ) 
 REPRESENTATION_ITEM ( '' )  SURFACE ( )  );
#7769 = B_SPLINE_CURVE_WITH_KNOTS ( 'NONE', 3,
 ( #48326, #52393, #47108, #4155, #43342, #57693 ),
 .UNSPECIFIED., .F., .F.,
 ( 4, 2, 4 ),
 ( 5.421010862427522170E-19, 0.0002293801035737099412, 0.0004587602071474193403 ),
 .UNSPECIFIED. ) ;
#7770 = ORIENTED_EDGE ( 'NONE', *, *, #16211, .F. ) ;
#7771 = ADVANCED_FACE ( 'NONE', ( #50933 ), #17744, .F. ) ;
#7772 = CARTESIAN_POINT ( 'NONE',  ( 1.154321485836933281, 37.57248783354771859, 20.73950273457856142 ) ) ;
#7773 = CARTESIAN_POINT ( 'NONE',  ( 2.706805983486679779, -32.74306943570211814, -29.40522942009712182 ) ) ;
#7775 = CONICAL_SURFACE ( 'NONE', #44846, 43.92652462719577500, 1.486293639869522343 ) ;
#7774 = CARTESIAN_POINT ( 'NONE',  ( 0.1135584504625007790, -38.23248975848313336, -22.02790909284708576 ) ) ;
#7776 = CARTESIAN_POINT ( 'NONE',  ( -4.000000000000000000, 1.557668341133497059, -0.1596965656957516910 ) ) ;
#7777 = ORIENTED_EDGE ( 'NONE', *, *, #15784, .T. ) ;
#7778 = EDGE_CURVE ( 'NONE', #11923, #58971, #36559, .T. ) ;
#7779 = CARTESIAN_POINT ( 'NONE',  ( 2.009741617377216460, -40.28707309596673980, 17.78920512511105301 ) ) ;
#7780 = CARTESIAN_POINT ( 'NONE',  ( -6.078726893082806448, 13.83016815118519638, 13.39852567182907350 ) ) ;
#7781 = AXIS2_PLACEMENT_3D ( 'NONE', #58344, #5419, #16088 ) ;
#7782 = CARTESIAN_POINT ( 'NONE',  ( 5.901463166500146684, 16.58986915973321530, 11.37075686150967790 ) ) ;
#7783 = VERTEX_POINT ( 'NONE', #22137 ) ;
#7784 = CARTESIAN_POINT ( 'NONE',  ( 4.549368137175248350, 40.71620287708324781, 13.59764261105765826 ) ) ;
#7785 = CONICAL_SURFACE ( 'NONE', #40878, 42.08604991992415023, 1.569615340895231137 ) ;
#7786 = VERTEX_POINT ( 'NONE', #3926 ) ;
#7787 = FACE_OUTER_BOUND ( 'NONE', #46509, .T. ) ;
#7788 = CARTESIAN_POINT ( 'NONE',  ( -1.129531546211723025, 0.000000000000000000, 0.000000000000000000 ) ) ;
#7789 = VERTEX_POINT ( 'NONE', #60322 ) ;
#7790 = CARTESIAN_POINT ( 'NONE',  ( -6.063463321072278589, -1.864608017455489097, 19.16621218239824032 ) ) ;
#7791 = ORIENTED_EDGE ( 'NONE', *, *, #40509, .T. ) ;
#7792 = CARTESIAN_POINT ( 'NONE',  ( 0.7056759521544989644, 42.84373637420357994, 19.08305747553924903 ) ) ;
#7793 = CARTESIAN_POINT ( 'NONE',  ( 1.157644175074338477, 41.64460122042581958, -4.767542833671250868 ) ) ;
#7794 = ADVANCED_FACE ( 'NONE', ( #55318 ), #36586, .F. ) ;
#7795 = B_SPLINE_CURVE_WITH_KNOTS ( 'NONE', 3,
 ( #60219, #11714, #46162, #49915, #59298, #40857, #7597, #26719, #2903, #17332, #27035, #55212, #6649, #6969, #3208, #25796 ),
 .UNSPECIFIED., .F., .F.,
 ( 4, 3, 3, 3, 3, 4 ),
 ( 2.168512762477887481E-17, 0.0002618515315864423021, 0.0003927756766341991296, 0.0005236998216950568058, 0.0007855159896329902240, 0.001047349442285927437 ),
 .UNSPECIFIED. ) ;
#7796 = ORIENTED_EDGE ( 'NONE', *, *, #42115, .F. ) ;
#7797 = CARTESIAN_POINT ( 'NONE',  ( 1.231276596079881047, 40.64579686208666232, -10.25650859035628315 ) ) ;
#7798 = VERTEX_POINT ( 'NONE', #8322 ) ;
#7799 = CARTESIAN_POINT ( 'NONE',  ( 0.5827357941260210561, -38.21849163199656374, -28.86820951701472993 ) ) ;
#7800 = ORIENTED_EDGE ( 'NONE', *, *, #31282, .F. ) ;
#7801 = ORIENTED_EDGE ( 'NONE', *, *, #2451, .T. ) ;
#7802 = CARTESIAN_POINT ( 'NONE',  ( 0.6001305935487422083, 24.50730504006400423, 41.40054608060301433 ) ) ;
#7803 = CARTESIAN_POINT ( 'NONE',  ( 0.8557997880470606944, 43.90420959842181503, 19.17299735372024827 ) ) ;
#7804 = AXIS2_PLACEMENT_3D ( 'NONE', #16277, #45419, #58546 ) ;
#7805 = CARTESIAN_POINT ( 'NONE',  ( 4.956653778116996811, 45.35992544608552635, -15.97476558431834626 ) ) ;
#7806 = AXIS2_PLACEMENT_3D ( 'NONE', #47297, #37610, #51672 ) ;
#7807 = CARTESIAN_POINT ( 'NONE',  ( 5.959547316686252039, -19.82715097195158194, -5.308980600728387067 ) ) ;
#7808 = CARTESIAN_POINT ( 'NONE',  ( 5.960721111146673579, -14.51823969584089902, -14.50930005615011709 ) ) ;
#7809 = ORIENTED_EDGE ( 'NONE', *, *, #36316, .T. ) ;
#7810 = CARTESIAN_POINT ( 'NONE',  ( 0.9756008150404602564, 11.24277293639989317, 41.40938772927936640 ) ) ;
#7811 = CARTESIAN_POINT ( 'NONE',  ( 0.9789889208857684988, -17.55352473101461541, 38.05533691297488730 ) ) ;
#7812 = CARTESIAN_POINT ( 'NONE',  ( 5.894904586330512508, 20.06791991542434772, -1.344619771443771983 ) ) ;
#7813 = VERTEX_POINT ( 'NONE', #3615 ) ;
#7814 = B_SPLINE_CURVE_WITH_KNOTS ( 'NONE', 3,
 ( #42063, #56420, #17612, #51102, #17006, #60811, #55491, #36738, #7253, #61116, #32331, #8193, #60495, #27620, #37346, #40831, #55807, #27312, #46439 ),
 .UNSPECIFIED., .F., .F.,
 ( 4, 3, 3, 3, 3, 3, 4 ),
 ( 1.734776414728241573E-18, 0.0002612768053151704622, 0.0003919133833142885402, 0.0005225499612322576093, 0.0006531865391693351995, 0.0008112755173415168216, 0.0009693688056799714889 ),
 .UNSPECIFIED. ) ;
#7815 = ORIENTED_EDGE ( 'NONE', *, *, #53010, .F. ) ;
#7816 = CARTESIAN_POINT ( 'NONE',  ( 0.9749527285493304607, 34.21468599366747299, -25.89384247702535902 ) ) ;
#7817 = CARTESIAN_POINT ( 'NONE',  ( -6.078075953587585900, 13.82887156709808707, -13.39990617235218195 ) ) ;
#7818 = CARTESIAN_POINT ( 'NONE',  ( 2.526552050251863246, 20.43086833796958146, 37.81244156770998188 ) ) ;
#7820 = ORIENTED_EDGE ( 'NONE', *, *, #35961, .F. ) ;
#7819 = EDGE_CURVE ( 'NONE', #10490, #42439, #36252, .T. ) ;
#7821 = CARTESIAN_POINT ( 'NONE',  ( 4.549368137175248350, -13.59764261105780214, 40.71620287708320518 ) ) ;
#7822 = CARTESIAN_POINT ( 'NONE',  ( 0.3676999524040366896, -34.85286720109691316, 27.04123205746257241 ) ) ;
#7823 = AXIS2_PLACEMENT_3D ( 'NONE', #42228, #55976, #37524 ) ;
#7824 = ORIENTED_EDGE ( 'NONE', *, *, #36380, .F. ) ;
#7825 = CARTESIAN_POINT ( 'NONE',  ( 0.7048096507298579061, 47.58126109679093219, 7.115188260604007553 ) ) ;
#7826 = ORIENTED_EDGE ( 'NONE', *, *, #52735, .T. ) ;
#7827 = CYLINDRICAL_SURFACE ( 'NONE', #56360, 12.49999999999999822 ) ;
#7828 = CARTESIAN_POINT ( 'NONE',  ( 5.896278296736517710, 5.964180709076651432, 19.20821511967891837 ) ) ;
#7829 = CARTESIAN_POINT ( 'NONE',  ( 0.9775691876210987896, 10.08232880996395231, -40.67776241090162870 ) ) ;
#7830 = ADVANCED_FACE ( 'NONE', ( #12757 ), #24137, .F. ) ;
#7831 =( NAMED_UNIT ( * ) SI_UNIT ( $, .STERADIAN. ) SOLID_ANGLE_UNIT ( ) );
#7832 = CARTESIAN_POINT ( 'NONE',  ( 2.299652685299200972, 36.48832987231130431, 32.75490051866358954 ) ) ;
#7833 = EDGE_LOOP ( 'NONE', ( #14073, #3393, #29984, #58366, #31344, #59467, #12435, #29249, #35550, #32333, #30010, #15696, #17840, #23579, #5709, #51551, #17996, #5862, #17836, #23764, #17763, #34498, #25131, #55002, #3033, #57867, #56581, #19438, #38316, #11408, #33649, #46009, #18622, #13187, #32232, #55430, #40330, #52699, #58241, #33818, #61241, #58849, #2238, #25942, #56557, #23092, #24902, #29847, #47215, #15291, #55193, #4922, #42698, #51489, #59699, #26830, #46402, #38263, #51818, #49941, #9418, #313, #35848, #51086, #34632, #47506, #18156, #13586, #33803, #8020, #27351, #35456, #59441, #18783, #13432, #7262, #53469, #43453, #9019, #50251, #41601, #2149, #7347, #57293, #54393, #34696, #59934, #19940, #26605, #33156, #22820, #46949, #42229, #50781, #55488, #704, #17993, #15594, #3469, #21447, #41586, #12341, #41136, #20145, #576, #49132, #35249, #17044, #43338, #6627, #11589, #28134, #17301, #32961, #2253, #8661, #42806, #57371, #40129, #36725, #37397, #25930, #59935, #28797, #54526, #27542, #16921, #13589, #37305, #11872, #18383, #10975, #28401, #19761, #53100, #3111, #59940, #21748, #9366, #15371, #34240, #33885, #24520, #41757 ) ) ;
#7834 = CARTESIAN_POINT ( 'NONE',  ( 0.5804410086790514622, -44.12183670707879202, 15.89916279082866701 ) ) ;
#7835 = LINE ( 'NONE', #46087, #45634 ) ;
#7836 = ADVANCED_FACE ( 'NONE', ( #22750 ), #45395, .F. ) ;
#7837 = VECTOR ( 'NONE', #47602, 1000.000000000000114 ) ;
#7838 = CARTESIAN_POINT ( 'NONE',  ( 0.5988103564986356764, 46.30780741915666709, -13.03604522143308664 ) ) ;
#7839 = CARTESIAN_POINT ( 'NONE',  ( 0.5809828226811553087, 41.20389530892342833, -24.41822904836879715 ) ) ;
#7840 = CARTESIAN_POINT ( 'NONE',  ( 0.9756950546413940550, 37.11135009583556865, -21.53795086961224570 ) ) ;
#7841 = CARTESIAN_POINT ( 'NONE',  ( 0.5804410086790514622, -46.06497594411315788, 8.805557513506700573 ) ) ;
#7842 = DIRECTION ( 'NONE',  ( 1.000000000000000000, 1.836909530733573776E-16, -1.925929944387235853E-32 ) ) ;
#7843 = CARTESIAN_POINT ( 'NONE',  ( 0.6027444965799114707, -49.10724443700913611, -0.1306127531153215560 ) ) ;
#7844 = CARTESIAN_POINT ( 'NONE',  ( 0.5806925824938502512, -7.260877859417425029, 46.33035738103242096 ) ) ;
#7845 = B_SPLINE_CURVE_WITH_KNOTS ( 'NONE', 3,
 ( #15534, #22846, #56341, #3710, #237, #39351, #27851, #41979, #61342, #34638, #51955, #37903, #23456, #23769, #8737, #61045, #52258, #53705, #33184, #9047, #47274, #19091, #14384, #32882, #46983 ),
 .UNSPECIFIED., .F., .F.,
 ( 4, 3, 3, 3, 3, 3, 3, 3, 4 ),
 ( 6.254634441385501517E-18, 0.0005656085177311403990, 0.001131215744874501140, 0.001696821861372765916, 0.002262427090022497284, 0.002828031679238746793, 0.003393635864401604862, 0.003977030878808130755, 0.004561030005651156398 ),
 .UNSPECIFIED. ) ;
#7846 = B_SPLINE_CURVE_WITH_KNOTS ( 'NONE', 3,
 ( #38100, #57145, #444, #47785, #19588, #57444 ),
 .UNSPECIFIED., .F., .F.,
 ( 4, 2, 4 ),
 ( 1.271478423208939840E-17, 0.0002445244328975392997, 0.0004890488657950658059 ),
 .UNSPECIFIED. ) ;
#7847 = EDGE_CURVE ( 'NONE', #36392, #33340, #52048, .T. ) ;
#7848 = CARTESIAN_POINT ( 'NONE',  ( -6.078075953587585900, -4.290048539733304800, -18.77207121694002367 ) ) ;
#7849 = CARTESIAN_POINT ( 'NONE',  ( 2.648799415243708655, 40.32403112341518892, -27.90143324719075579 ) ) ;
#7850 = VECTOR ( 'NONE', #33605, 1000.000000000000114 ) ;
#7851 = ORIENTED_EDGE ( 'NONE', *, *, #59711, .T. ) ;
#7852 = VECTOR ( 'NONE', #61954, 1000.000000000000114 ) ;
#7853 = CARTESIAN_POINT ( 'NONE',  ( 4.549368137175248350, -28.46244473166695954, 32.13400537129875545 ) ) ;
#7854 = CARTESIAN_POINT ( 'NONE',  ( 5.960721111146673579, -18.96557324978293124, 7.848955554238177257 ) ) ;
#7855 = B_SPLINE_CURVE_WITH_KNOTS ( 'NONE', 3,
 ( #11867, #17780, #51272, #8355, #46602, #3649 ),
 .UNSPECIFIED., .F., .F.,
 ( 4, 2, 4 ),
 ( 1.261454201589629882E-17, 0.0002445244328975406550, 0.0004890488657950686248 ),
 .UNSPECIFIED. ) ;
#7856 = CARTESIAN_POINT ( 'NONE',  ( 3.407937589446178528, -13.63405474014707686, -1.331713209622645833 ) ) ;
#7857 = ORIENTED_EDGE ( 'NONE', *, *, #8000, .T. ) ;
#7858 = ADVANCED_FACE ( 'NONE', ( #47489 ), #51754, .F. ) ;
#7859 = CARTESIAN_POINT ( 'NONE',  ( 0.5998501479064699549, 47.76154736470750350, 5.759754759340949271 ) ) ;
#7860 = CARTESIAN_POINT ( 'NONE',  ( 0.1149546198390368201, 3.964231739604973104, 43.94577831530497747 ) ) ;
#7861 = EDGE_CURVE ( 'NONE', #8195, #61878, #61035, .T. ) ;
#7862 = ORIENTED_EDGE ( 'NONE', *, *, #36238, .F. ) ;
#7863 = LINE ( 'NONE', #59553, #38085 ) ;
#7864 = CARTESIAN_POINT ( 'NONE',  ( 4.963659409799330291, 43.79875484948460951, -9.199077662858449855 ) ) ;
#7865 = DIRECTION ( 'NONE',  ( -1.000000000000000000, -0.000000000000000000, -0.000000000000000000 ) ) ;
#7866 = EDGE_LOOP ( 'NONE', ( #59243, #8556, #55440, #24343 ) ) ;
#7867 = CARTESIAN_POINT ( 'NONE',  ( 0.6028618097248863439, 29.42431480658679988, 38.05975027458347171 ) ) ;
#7868 = CIRCLE ( 'NONE', #1826, 43.08621763946400307 ) ;
#7869 = ORIENTED_EDGE ( 'NONE', *, *, #24049, .F. ) ;
#7870 = VERTEX_POINT ( 'NONE', #57461 ) ;
#7871 = CARTESIAN_POINT ( 'NONE',  ( 0.6064782688330849769, 21.91200102226807189, 41.46322054084672004 ) ) ;
#7872 = EDGE_LOOP ( 'NONE', ( #48131, #29211, #57257, #43270 ) ) ;
#7873 = CARTESIAN_POINT ( 'NONE',  ( 0.6000166863083090663, -49.10753961887881758, -0.5225268306041156441 ) ) ;
#7874 = EDGE_CURVE ( 'NONE', #13235, #28616, #34020, .T. ) ;
#7875 = ORIENTED_EDGE ( 'NONE', *, *, #11583, .T. ) ;
#7876 = CARTESIAN_POINT ( 'NONE',  ( 5.896782393890504181, -7.222780579330470019, -18.77118876312469808 ) ) ;
#7877 = PRODUCT_DEFINITION_FORMATION_WITH_SPECIFIED_SOURCE ( 'ANY', '', #3775, .NOT_KNOWN. ) ;
#7878 = CARTESIAN_POINT ( 'NONE',  ( 0.9757402383260944667, 16.34189654378434398, 39.67468066200765264 ) ) ;
#7879 = ORIENTED_EDGE ( 'NONE', *, *, #34759, .F. ) ;
#7880 = CARTESIAN_POINT ( 'NONE',  ( 4.000000000000002665, 1.557668341133517043, -5.440303434304241570 ) ) ;
#7881 = CARTESIAN_POINT ( 'NONE',  ( -6.063463321072278589, -14.67303933398460103, 12.47086080360175586 ) ) ;
#7882 = CARTESIAN_POINT ( 'NONE',  ( 3.050102900204245682, -37.41160462723878055, 23.14729116750437754 ) ) ;
#7883 = FACE_OUTER_BOUND ( 'NONE', #52234, .T. ) ;
#7884 = EDGE_LOOP ( 'NONE', ( #25736, #19842, #3769, #35817 ) ) ;
#7885 = CARTESIAN_POINT ( 'NONE',  ( -31.75000000000000000, 0.000000000000000000, 0.000000000000000000 ) ) ;
#7886 = B_SPLINE_CURVE_WITH_KNOTS ( 'NONE', 3,
 ( #46375, #36989, #3123, #46998 ),
 .UNSPECIFIED., .F., .F.,
 ( 4, 4 ),
 ( 0.000000000000000000, 0.001752131338475893668 ),
 .UNSPECIFIED. ) ;
#7887 = ORIENTED_EDGE ( 'NONE', *, *, #37869, .T. ) ;
#7888 = CARTESIAN_POINT ( 'NONE',  ( 1.227938101723756947, 22.18841447410719780, 36.73927144310519566 ) ) ;
#7889 = ORIENTED_EDGE ( 'NONE', *, *, #39686, .F. ) ;
#7890 = B_SPLINE_CURVE_WITH_KNOTS ( 'NONE', 3,
 ( #15512, #34620, #53685, #10815 ),
 .UNSPECIFIED., .F., .F.,
 ( 4, 4 ),
 ( 0.000000000000000000, 0.004444103432399267029 ),
 .UNSPECIFIED. ) ;
#7891 = CARTESIAN_POINT ( 'NONE',  ( 1.231276596079881047, -26.41281459480337546, -32.55211200826465756 ) ) ;
#7892 =( BOUNDED_SURFACE ( )  B_SPLINE_SURFACE ( 3, 1, ( 
 ( #41812, #59642 ),
 ( #45895, #2941 ),
 ( #56181, #36802 ),
 ( #60562, #16754 ) ),
 .UNSPECIFIED., .F., .F., .F. ) 
 B_SPLINE_SURFACE_WITH_KNOTS ( ( 4, 4 ),
 ( 2, 2 ),
 ( 0.000000000000000000, 1.000000000000000000 ),
 ( 0.000000000000000000, 1.000000000000000000 ),
 .UNSPECIFIED. ) 
 GEOMETRIC_REPRESENTATION_ITEM ( )  RATIONAL_B_SPLINE_SURFACE ( (
 ( 1.000000000000000000, 1.000000000000000000),
 ( 0.9751682680413298332, 0.9999560080971552356),
 ( 0.9751682680413298332, 0.9999560080971552356),
 ( 1.000000000000000000, 1.000000000000000000) ) ) 
 REPRESENTATION_ITEM ( '' )  SURFACE ( )  );
#7893 = CARTESIAN_POINT ( 'NONE',  ( 2.706805983486680223, 13.63466385414067794, -41.84342307823710883 ) ) ;
#7894 = ORIENTED_EDGE ( 'NONE', *, *, #27677, .F. ) ;
#7895 = LINE ( 'NONE', #16690, #2536 ) ;
#7896 = CARTESIAN_POINT ( 'NONE',  ( 2.301529144917016101, 48.01619158420459144, -1.287519423136770813 ) ) ;
#7897 = CARTESIAN_POINT ( 'NONE',  ( 0.6024113833632039894, 27.91636117921130733, 40.40072583027055941 ) ) ;
#7898 = DIRECTION ( 'NONE',  ( 0.000000000000000000, 0.000000000000000000, 1.000000000000000000 ) ) ;
#7899 = EDGE_CURVE ( 'NONE', #9596, #8039, #22226, .T. ) ;
#7900 = CIRCLE ( 'NONE', #12936, 42.92674063221959813 ) ;
#7901 = ORIENTED_EDGE ( 'NONE', *, *, #25168, .F. ) ;
#7902 = ORIENTED_EDGE ( 'NONE', *, *, #37074, .F. ) ;
#7903 = CARTESIAN_POINT ( 'NONE',  ( 0.5804410086790514622, -1.020940616196076123, 46.88792522722238232 ) ) ;
#7904 = CARTESIAN_POINT ( 'NONE',  ( 5.959547316686252039, -16.28190225198610008, -12.49803383497744136 ) ) ;
#7905 = EDGE_CURVE ( 'NONE', #7098, #5232, #10240, .T. ) ;
#7906 = LINE ( 'NONE', #3496, #2808 ) ;
#7907 = B_SPLINE_CURVE_WITH_KNOTS ( 'NONE', 3,
 ( #16622, #35125, #20096, #26017, #39214, #29782 ),
 .UNSPECIFIED., .F., .F.,
 ( 4, 2, 4 ),
 ( 0.000000000000000000, 0.0002450742804987355856, 0.0004901485609974711713 ),
 .UNSPECIFIED. ) ;
#7908 = CARTESIAN_POINT ( 'NONE',  ( 0.7044674535453004927, 46.33602660604233847, -16.27191940660486935 ) ) ;
#7909 = ADVANCED_FACE ( 'NONE', ( #4234 ), #30533, .F. ) ;
#7910 = CARTESIAN_POINT ( 'NONE',  ( 3.894904216938898323, 11.93731129210782704, 42.30395881701280558 ) ) ;
#7911 = FACE_OUTER_BOUND ( 'NONE', #20005, .T. ) ;
#7912 = EDGE_CURVE ( 'NONE', #23651, #51385, #33443, .T. ) ;
#7913 = CARTESIAN_POINT ( 'NONE',  ( 0.3622758884714730732, -39.50828911767010965, 17.25816669464924047 ) ) ;
#7914 = VECTOR ( 'NONE', #33747, 1000.000000000000000 ) ;
#7915 = B_SPLINE_CURVE_WITH_KNOTS ( 'NONE', 3,
 ( #15785, #38989, #20475, #48362 ),
 .UNSPECIFIED., .F., .F.,
 ( 4, 4 ),
 ( 1.301042606982605321E-18, 0.004041751736741002951 ),
 .UNSPECIFIED. ) ;
#7916 = CARTESIAN_POINT ( 'NONE',  ( 0.7044674535453004927, -48.80743866909963913, -5.443955673311811516 ) ) ;
#7917 = DIRECTION ( 'NONE',  ( -1.000000000000000000, -0.000000000000000000, -0.000000000000000000 ) ) ;
#7918 = CARTESIAN_POINT ( 'NONE',  ( 5.959547316686252039, 5.315863417546055736, 19.82530672674364070 ) ) ;
#7919 = CARTESIAN_POINT ( 'NONE',  ( 5.896782393890504181, -18.51935720350340731, 7.845985957612901629 ) ) ;
#7920 = CARTESIAN_POINT ( 'NONE',  ( 0.6023143664670691511, -33.83148565876907554, -34.20175727332116367 ) ) ;
#7921 = CARTESIAN_POINT ( 'NONE',  ( 1.154321485836933947, 42.64911658695776708, 4.782433484301333415 ) ) ;
#7922 = CARTESIAN_POINT ( 'NONE',  ( 0.9769922540276052558, -22.92146824146746908, 35.08472386582974423 ) ) ;
#7923 = CARTESIAN_POINT ( 'NONE',  ( 0.1073791018717483448, 43.12183934961191056, -0.4849339620928847516 ) ) ;
#7924 = ADVANCED_FACE ( 'NONE', ( #58394 ), #36987, .F. ) ;
#7925 = CARTESIAN_POINT ( 'NONE',  ( 4.000000000000004441, -1.549102112939112486, -5.442104661404058241 ) ) ;
#7926 = CARTESIAN_POINT ( 'NONE',  ( 0.6029443199889047422, -47.50133849333689540, 12.45634309080449320 ) ) ;
#7928 = ORIENTED_EDGE ( 'NONE', *, *, #5980, .T. ) ;
#7927 = CARTESIAN_POINT ( 'NONE',  ( -6.016761891674564211, -18.68153697670643609, 2.462934516563739518 ) ) ;
#7929 = VERTEX_POINT ( 'NONE', #54006 ) ;
#7930 = CARTESIAN_POINT ( 'NONE',  ( 0.5997462898726536595, 16.46871699354542429, -46.26373299606095202 ) ) ;
#7931 = CARTESIAN_POINT ( 'NONE',  ( 0.3622758884714600280, 31.06363466427727360, -29.89648521331598729 ) ) ;
#7933 = ADVANCED_FACE ( 'NONE', ( #11130 ), #43380, .F. ) ;
#7932 = CARTESIAN_POINT ( 'NONE',  ( 0.7048096507298579061, -47.58126109679096771, -7.115188260603675374 ) ) ;
#7934 = ORIENTED_EDGE ( 'NONE', *, *, #12257, .F. ) ;
#7935 = ORIENTED_EDGE ( 'NONE', *, *, #46789, .F. ) ;
#7936 = CARTESIAN_POINT ( 'NONE',  ( 0.7948878604505679180, 36.81796311561313928, -32.48286070092603239 ) ) ;
#7937 = LINE ( 'NONE', #22048, #60080 ) ;
#7938 = B_SPLINE_CURVE_WITH_KNOTS ( 'NONE', 3,
 ( #19490, #38607, #57659, #33906, #24484, #15100 ),
 .UNSPECIFIED., .F., .F.,
 ( 4, 2, 4 ),
 ( 9.825198971288231405E-18, 0.0002293755540694290146, 0.0004587511081388482171 ),
 .UNSPECIFIED. ) ;
#7939 = ADVANCED_FACE ( 'NONE', ( #44967 ), #21550, .F. ) ;
#7940 = VECTOR ( 'NONE', #15419, 1000.000000000000000 ) ;
#7941 = ORIENTED_EDGE ( 'NONE', *, *, #45929, .T. ) ;
#7942 = ORIENTED_EDGE ( 'NONE', *, *, #24819, .T. ) ;
#7943 = B_SPLINE_CURVE_WITH_KNOTS ( 'NONE', 3,
 ( #51531, #13664, #51846, #18363, #61243, #22739, #56850, #37475, #8017, #33085, #28357, #36546, #3918, #32451, #32768, #23057, #8309, #17735, #56238 ),
 .UNSPECIFIED., .F., .F.,
 ( 4, 3, 3, 3, 3, 3, 4 ),
 ( 1.734723475976807094E-18, 0.0002724573126191767855, 0.0004086839781548472846, 0.0005449106435901813778, 0.0006811373090491514579, 0.0008459866663933718681, 0.001010840725717217052 ),
 .UNSPECIFIED. ) ;
#7944 = CARTESIAN_POINT ( 'NONE',  ( 1.092182651088183354, 19.45474270483163082, -37.12511509384292197 ) ) ;
#7945 = CIRCLE ( 'NONE', #60970, 43.92652462719577500 ) ;
#7946 = CARTESIAN_POINT ( 'NONE',  ( 0.1073791018717578927, -34.50606437925563341, 25.86618856530653687 ) ) ;
#7947 = ORIENTED_EDGE ( 'NONE', *, *, #25114, .F. ) ;
#7948 = CARTESIAN_POINT ( 'NONE',  ( 2.500000000000000000, 0.000000000000000000, 2.041999999999999815 ) ) ;
#7949 = EDGE_CURVE ( 'NONE', #48449, #12657, #48543, .T. ) ;
#7950 = CARTESIAN_POINT ( 'NONE',  ( -6.077587904424778920, 16.78120357693994791, -9.443898977817823948 ) ) ;
#7951 =( BOUNDED_SURFACE ( )  B_SPLINE_SURFACE ( 3, 1, ( 
 ( #27984, #14516 ),
 ( #13588, #8552 ),
 ( #33620, #9482 ),
 ( #38035, #28899 ) ),
 .UNSPECIFIED., .F., .F., .F. ) 
 B_SPLINE_SURFACE_WITH_KNOTS ( ( 4, 4 ),
 ( 2, 2 ),
 ( 0.000000000000000000, 1.000000000000000000 ),
 ( 0.000000000000000000, 1.000000000000000000 ),
 .UNSPECIFIED. ) 
 GEOMETRIC_REPRESENTATION_ITEM ( )  RATIONAL_B_SPLINE_SURFACE ( (
 ( 1.000000000000000000, 1.000000000000000000),
 ( 0.9754377213608244057, 0.9999580625633939235),
 ( 0.9754377213608244057, 0.9999580625633939235),
 ( 1.000000000000000000, 1.000000000000000000) ) ) 
 REPRESENTATION_ITEM ( '' )  SURFACE ( )  );
#7952 = EDGE_CURVE ( 'NONE', #16902, #52610, #39650, .T. ) ;
#7953 = CARTESIAN_POINT ( 'NONE',  ( 0.1103744047535531458, 0.03874731383731806061, -43.12441516302519773 ) ) ;
#7954 = ORIENTED_EDGE ( 'NONE', *, *, #57829, .T. ) ;
#7955 = ORIENTED_EDGE ( 'NONE', *, *, #39147, .T. ) ;
#7956 = CARTESIAN_POINT ( 'NONE',  ( -6.077587904424778920, 0.6233693561571294062, -19.24597183931574662 ) ) ;
#7957 = VECTOR ( 'NONE', #27671, 1000.000000000000227 ) ;
#7958 = ORIENTED_EDGE ( 'NONE', *, *, #39697, .F. ) ;
#7959 = CARTESIAN_POINT ( 'NONE',  ( 0.5839879327111913154, 44.21534283185629022, -18.41291455875256489 ) ) ;
#7960 = CARTESIAN_POINT ( 'NONE',  ( 0.9730545539215883499, 16.88610103448558064, 39.44597740938066721 ) ) ;
#7961 = FACE_OUTER_BOUND ( 'NONE', #43830, .T. ) ;
#7962 = CARTESIAN_POINT ( 'NONE',  ( 0.7044674535453004927, -31.27352687970047995, -37.86514544162691465 ) ) ;
#7963 = CARTESIAN_POINT ( 'NONE',  ( -2.601141883200662974, -14.73982649082957330, 2.352220756992720929 ) ) ;
#7964 = ORIENTED_EDGE ( 'NONE', *, *, #36102, .F. ) ;
#7965 = DIRECTION ( 'NONE',  ( -0.07500201931887527651, -0.2825166499419927146, 0.9563258020170973817 ) ) ;
#7966 = CARTESIAN_POINT ( 'NONE',  ( 2.648799415243696664, -47.76469914295827834, 11.09283458239048592 ) ) ;
#7967 =( BOUNDED_SURFACE ( )  B_SPLINE_SURFACE ( 3, 1, ( 
 ( #18499, #51069 ),
 ( #61382, #56078 ),
 ( #55766, #4665 ),
 ( #13191, #32292 ) ),
 .UNSPECIFIED., .F., .F., .F. ) 
 B_SPLINE_SURFACE_WITH_KNOTS ( ( 4, 4 ),
 ( 2, 2 ),
 ( 0.000000000000000000, 1.000000000000000000 ),
 ( 0.000000000000000000, 1.000000000000000000 ),
 .UNSPECIFIED. ) 
 GEOMETRIC_REPRESENTATION_ITEM ( )  RATIONAL_B_SPLINE_SURFACE ( (
 ( 1.000000000000000000, 1.000000000000000000),
 ( 0.9953040768229005630, 0.8617119497784937465),
 ( 0.9953040768229005630, 0.8617119497784937465),
 ( 1.000000000000000000, 1.000000000000000000) ) ) 
 REPRESENTATION_ITEM ( '' )  SURFACE ( )  );
#7968 = CARTESIAN_POINT ( 'NONE',  ( 0.1103310638050661735, 39.87325896099741840, -16.42686748615365389 ) ) ;
#7969 = ORIENTED_EDGE ( 'NONE', *, *, #17415, .T. ) ;
#7970 = CARTESIAN_POINT ( 'NONE',  ( -2.000000000000022649, -3.464101615137742396, -5.600000000000000533 ) ) ;
#7971 = DIRECTION ( 'NONE',  ( -0.07836865515943411409, -0.9649662368512201827, -0.2503967164834565162 ) ) ;
#7972 = LINE ( 'NONE', #3874, #59630 ) ;
#7973 = CARTESIAN_POINT ( 'NONE',  ( 0.5806925824938499181, -41.60618895332673617, -21.63671424046719594 ) ) ;
#7974 = VERTEX_POINT ( 'NONE', #25830 ) ;
#7975 = FACE_OUTER_BOUND ( 'NONE', #39087, .T. ) ;
#7976 = FACE_OUTER_BOUND ( 'NONE', #29688, .T. ) ;
#7977 = EDGE_CURVE ( 'NONE', #56473, #16223, #37105, .T. ) ;
#7978 = CARTESIAN_POINT ( 'NONE',  ( 0.7044674535452954967, -2.415488218027790790, 49.05066910328008589 ) ) ;
#7979 = EDGE_CURVE ( 'NONE', #51706, #22341, #19237, .T. ) ;
#7980 = CARTESIAN_POINT ( 'NONE',  ( 0.9762797500689124330, -22.97506929404208975, 35.04955029839425151 ) ) ;
#7981 = CARTESIAN_POINT ( 'NONE',  ( 0.5817216825391108292, -46.75865999591429301, 3.586456133001590718 ) ) ;
#7982 = CARTESIAN_POINT ( 'NONE',  ( 2.281351352603282479, 40.87339198768997051, 25.11567449372724425 ) ) ;
#7983 = DIRECTION ( 'NONE',  ( 0.000000000000000000, 0.000000000000000000, -1.000000000000000000 ) ) ;
#7984 = CARTESIAN_POINT ( 'NONE',  ( 4.956445790443996913, 2.113652668516264654, 47.04328350079860854 ) ) ;
#7985 = EDGE_CURVE ( 'NONE', #6050, #43089, #20830, .T. ) ;
#7986 = CARTESIAN_POINT ( 'NONE',  ( 2.281448460670567613, 7.562315317391745673, 47.37344300043614709 ) ) ;
#7987 = EDGE_CURVE ( 'NONE', #21914, #24949, #48711, .T. ) ;
#7988 = CARTESIAN_POINT ( 'NONE',  ( 0.8557997880470606944, -19.17299735372040459, 43.90420959842174398 ) ) ;
#7989 = B_SPLINE_CURVE_WITH_KNOTS ( 'NONE', 3,
 ( #60201, #17313, #7575, #12626, #55499, #1635, #44914, #1951, #31717, #49568, #50808, #59271, #59897, #17012, #25453, #58967 ),
 .UNSPECIFIED., .F., .F.,
 ( 4, 3, 3, 3, 3, 4 ),
 ( 1.868480190406682863E-17, 0.0002618515315864444705, 0.0003927756766342024365, 0.0005236998216950591910, 0.0007855159896329946692, 0.001047349442285930039 ),
 .UNSPECIFIED. ) ;
#7990 = ORIENTED_EDGE ( 'NONE', *, *, #20163, .T. ) ;
#7991 = AXIS2_PLACEMENT_3D ( 'NONE', #15912, #45355, #30601 ) ;
#7992 = EDGE_CURVE ( 'NONE', #60545, #2852, #34872, .T. ) ;
#7993 = CARTESIAN_POINT ( 'NONE',  ( 0.7056759521544982983, -46.73287073726609009, -3.973364037055558295 ) ) ;
#7994 = CARTESIAN_POINT ( 'NONE',  ( 0.8557997880470599172, -41.02602466100761802, -24.73961900479294584 ) ) ;
#7995 = DIRECTION ( 'NONE',  ( -1.000000000000000000, -0.000000000000000000, -0.000000000000000000 ) ) ;
#7996 = CARTESIAN_POINT ( 'NONE',  ( 0.3676999524040323597, 10.61898383218351860, -42.81574203134477585 ) ) ;
#7997 = CARTESIAN_POINT ( 'NONE',  ( 0.8744876279028306332, -45.83369275826206746, -17.59609782084448071 ) ) ;
#7998 = DIRECTION ( 'NONE',  ( 0.000000000000000000, 1.000000000000000000, -1.224646799147353207E-16 ) ) ;
#7999 = CARTESIAN_POINT ( 'NONE',  ( 2.000000000000010658, -3.464101615137748169, 0.000000000000000000 ) ) ;
#8000 = EDGE_CURVE ( 'NONE', #42030, #46817, #32656, .T. ) ;
#8001 = CARTESIAN_POINT ( 'NONE',  ( 3.221118495291108719, 35.79969342022239687, -25.55666978852753601 ) ) ;
#8002 = CARTESIAN_POINT ( 'NONE',  ( 2.281351352603294913, 34.83869092251607213, -32.98025003937380717 ) ) ;
#8004 = ORIENTED_EDGE ( 'NONE', *, *, #2639, .F. ) ;
#8003 = CARTESIAN_POINT ( 'NONE',  ( 4.956445790443991584, 25.79263028817558023, 39.39896284113483915 ) ) ;
#8005 = ORIENTED_EDGE ( 'NONE', *, *, #16560, .F. ) ;
#8006 = AXIS2_PLACEMENT_3D ( 'NONE', #9681, #57575, #28793 ) ;
#8007 = CARTESIAN_POINT ( 'NONE',  ( -2.569797478183783568, 14.01151037928423015, -4.218948559326104686 ) ) ;
#8008 = DIRECTION ( 'NONE',  ( -1.000000000000000000, -0.000000000000000000, -0.000000000000000000 ) ) ;
#8009 = DIRECTION ( 'NONE',  ( 0.000000000000000000, -1.047444401652941269E-14, 1.000000000000000000 ) ) ;
#8010 = ORIENTED_EDGE ( 'NONE', *, *, #17850, .F. ) ;
#8011 = CARTESIAN_POINT ( 'NONE',  ( 0.8751705887134553219, -38.69254731947813752, -28.56654290188640033 ) ) ;
#8012 = CARTESIAN_POINT ( 'NONE',  ( 0.8751705887134553219, 47.79200036674271956, 5.393078191592866055 ) ) ;
#8014 = CARTESIAN_POINT ( 'NONE',  ( 0.1084644655670281149, 5.234391617063994140, -42.80575641816242438 ) ) ;
#8013 = B_SPLINE_CURVE_WITH_KNOTS ( 'NONE', 3,
 ( #36577, #2413, #50644, #55646, #12779, #41283, #21536, #27465, #13083, #36271, #59740, #32177, #41587, #31873, #7099, #55964, #7411, #11857, #16856 ),
 .UNSPECIFIED., .F., .F.,
 ( 4, 3, 3, 3, 3, 3, 4 ),
 ( 1.355252715606880543E-20, 0.0002612768053151734980, 0.0003919133833142895702, 0.0005225499612322635724, 0.0006531865391693340069, 0.0008112755173415186647, 0.0009693688056799699710 ),
 .UNSPECIFIED. ) ;
#8015 = ORIENTED_EDGE ( 'NONE', *, *, #44313, .T. ) ;
#8016 = VERTEX_POINT ( 'NONE', #51166 ) ;
#8017 = CARTESIAN_POINT ( 'NONE',  ( 0.9758171775293909000, 41.44794628856080720, 11.09981579996821566 ) ) ;
#8018 = LINE ( 'NONE', #36548, #39236 ) ;
#8019 = CARTESIAN_POINT ( 'NONE',  ( 4.975801465491695552, 3.702618843596801934, 47.76942479135487218 ) ) ;
#8020 = ORIENTED_EDGE ( 'NONE', *, *, #65, .T. ) ;
#8021 = CARTESIAN_POINT ( 'NONE',  ( 0.5807400328401637335, 47.55718917606843377, 5.711437504336126736 ) ) ;
#8022 = B_SPLINE_CURVE_WITH_KNOTS ( 'NONE', 3,
 ( #21305, #24767, #30688, #20688, #2170, #15382, #35417, #58251, #29765, #10367, #49806, #6235, #53257, #59189, #29455, #949 ),
 .UNSPECIFIED., .F., .F.,
 ( 4, 3, 3, 3, 3, 4 ),
 ( 6.938893903907228378E-18, 0.0002732102107932006790, 0.0004098135523333823471, 0.0005464168938825062979, 0.0008195847345945526594, 0.001092771384553103313 ),
 .UNSPECIFIED. ) ;
#8023 = CARTESIAN_POINT ( 'NONE',  ( 0.5988103622719990193, -23.52668907282314947, -41.96244039798782666 ) ) ;
#8024 = EDGE_CURVE ( 'NONE', #25443, #22251, #31564, .T. ) ;
#8025 = CARTESIAN_POINT ( 'NONE',  ( 0.1368894036331294861, 29.18906331529160170, -33.08866737569275074 ) ) ;
#8026 = CARTESIAN_POINT ( 'NONE',  ( -6.016489644550737204, -7.215050741358165709, 17.40716454747926889 ) ) ;
#8027 = ORIENTED_EDGE ( 'NONE', *, *, #4843, .T. ) ;
#8028 = CARTESIAN_POINT ( 'NONE',  ( 3.660176727303400934, -35.27264088192902136, 32.61164548483952785 ) ) ;
#8029 = CARTESIAN_POINT ( 'NONE',  ( 5.959547316686252039, 20.35048796920733238, 2.675599016784604434 ) ) ;
#8030 = ORIENTED_EDGE ( 'NONE', *, *, #27516, .F. ) ;
#8031 = CARTESIAN_POINT ( 'NONE',  ( 4.834790513006555379, -46.46485498442988415, -8.579428430861931076 ) ) ;
#8032 = CARTESIAN_POINT ( 'NONE',  ( 2.624215991343608501, -47.98682984381860450, -1.411420423865975993 ) ) ;
#8033 = CARTESIAN_POINT ( 'NONE',  ( 2.281351352603299354, 38.84542754822361132, -28.15073776031326602 ) ) ;
#8034 = CARTESIAN_POINT ( 'NONE',  ( 5.974727161628369032, -18.96851388233664082, 7.840226266082205520 ) ) ;
#8035 = EDGE_LOOP ( 'NONE', ( #17970, #6289, #55736, #47709, #8344, #44742 ) ) ;
#8036 = VERTEX_POINT ( 'NONE', #17671 ) ;
#8037 = CARTESIAN_POINT ( 'NONE',  ( -2.739355103387248747, 12.65256472621572570, 7.922131834294261488 ) ) ;
#8038 = CARTESIAN_POINT ( 'NONE',  ( 0.5838002273316446056, 41.41085122398249041, 24.06583301632217697 ) ) ;
#8039 = VERTEX_POINT ( 'NONE', #45892 ) ;
#8040 = CARTESIAN_POINT ( 'NONE',  ( 0.3622758884714730732, 42.84426538328725798, 4.808133778522027058 ) ) ;
#8041 = VECTOR ( 'NONE', #56086, 1000.000000000000227 ) ;
#8042 = ORIENTED_EDGE ( 'NONE', *, *, #61931, .F. ) ;
#8043 = CARTESIAN_POINT ( 'NONE',  ( 0.8744876279028263033, -39.87136468799916145, 28.64654129726773846 ) ) ;
#8044 = EDGE_LOOP ( 'NONE', ( #25808, #4591, #29841, #12297 ) ) ;
#8045 = DIRECTION ( 'NONE',  ( -1.000000000000000000, -5.380183451256491399E-17, -1.298891185607892835E-16 ) ) ;
#8046 = CARTESIAN_POINT ( 'NONE',  ( 0.8751705887134553219, 44.08562551107081617, -19.22545746485614870 ) ) ;
#8047 = CONICAL_SURFACE ( 'NONE', #3999, 42.88844316795388778, 0.04450589592585932341 ) ;
#8048 = CARTESIAN_POINT ( 'NONE',  ( 0.1103310638050662151, -26.31782144882266294, 34.16271402810823332 ) ) ;
#8049 = ORIENTED_EDGE ( 'NONE', *, *, #48591, .F. ) ;
#8050 = CARTESIAN_POINT ( 'NONE',  ( 0.1158816050234199035, 43.31156486878287382, 8.429139334616255752 ) ) ;
#8051 = CARTESIAN_POINT ( 'NONE',  ( 5.974727161628367256, -20.52494643607030156, 0.01551142186642607071 ) ) ;
#8052 = CARTESIAN_POINT ( 'NONE',  ( 1.157643937452369265, -41.87004049989154453, -1.975343801011922640 ) ) ;
#8053 = ADVANCED_FACE ( 'NONE', ( #60874 ), #49757, .F. ) ;
#8054 = ORIENTED_EDGE ( 'NONE', *, *, #56470, .F. ) ;
#8055 = CARTESIAN_POINT ( 'NONE',  ( 0.8557997880470599172, 17.48760788519217257, 44.60232077416692675 ) ) ;
#8056 = CARTESIAN_POINT ( 'NONE',  ( 0.7246131072078539903, -24.75818606403478483, 41.24126838495057967 ) ) ;
#8057 = DIRECTION ( 'NONE',  ( -0.1011922191286467460, 0.04473873795208903326, -0.9938604429769173354 ) ) ;
#8058 = CARTESIAN_POINT ( 'NONE',  ( 0.5988103622719986863, -11.86435782853401300, -46.62176011478417337 ) ) ;
#8059 = VERTEX_POINT ( 'NONE', #17366 ) ;
#8060 = ADVANCED_FACE ( 'NONE', ( #41495 ), #528, .F. ) ;
#8061 = B_SPLINE_CURVE_WITH_KNOTS ( 'NONE', 3,
 ( #58369, #53669, #10797, #41168, #36464, #35845 ),
 .UNSPECIFIED., .F., .F.,
 ( 4, 2, 4 ),
 ( 1.426045310262811165E-18, 0.0002450742804987333088, 0.0004901485609974652081 ),
 .UNSPECIFIED. ) ;
#8062 = CARTESIAN_POINT ( 'NONE',  ( 0.8751705887134423323, 46.67919521768887847, -11.58504748649151317 ) ) ;
#8063 = EDGE_CURVE ( 'NONE', #26937, #34397, #11682, .T. ) ;
#8064 = DIRECTION ( 'NONE',  ( 0.000000000000000000, 0.000000000000000000, -1.000000000000000000 ) ) ;
#8065 = EDGE_LOOP ( 'NONE', ( #61323, #16368, #47865, #8270 ) ) ;
#8066 = EDGE_CURVE ( 'NONE', #31261, #929, #43881, .T. ) ;
#8068 = FACE_OUTER_BOUND ( 'NONE', #58232, .T. ) ;
#8067 =( BOUNDED_SURFACE ( )  B_SPLINE_SURFACE ( 3, 1, ( 
 ( #55641, #54714 ),
 ( #2409, #35965 ),
 ( #40984, #17154 ),
 ( #35653, #30305 ) ),
 .UNSPECIFIED., .F., .F., .F. ) 
 B_SPLINE_SURFACE_WITH_KNOTS ( ( 4, 4 ),
 ( 2, 2 ),
 ( 0.000000000000000000, 1.000000000000000000 ),
 ( 0.000000000000000000, 1.000000000000000000 ),
 .UNSPECIFIED. ) 
 GEOMETRIC_REPRESENTATION_ITEM ( )  RATIONAL_B_SPLINE_SURFACE ( (
 ( 1.000000000000000000, 1.000000000000000000),
 ( 0.9953390228620291325, 0.8624445117760984880),
 ( 0.9953390228620291325, 0.8624445117760984880),
 ( 1.000000000000000000, 1.000000000000000000) ) ) 
 REPRESENTATION_ITEM ( '' )  SURFACE ( )  );
#8069 = CARTESIAN_POINT ( 'NONE',  ( 4.962356264823609031, -33.29728444345293781, 25.73958909062332268 ) ) ;
#8070 = CARTESIAN_POINT ( 'NONE',  ( 5.959828726073459926, -18.96492317065689193, -7.850628836606788674 ) ) ;
#8071 = DIRECTION ( 'NONE',  ( 0.000000000000000000, 0.000000000000000000, 1.000000000000000000 ) ) ;
#8072 = FACE_OUTER_BOUND ( 'NONE', #57018, .T. ) ;
#8073 = CARTESIAN_POINT ( 'NONE',  ( 0.8554163680231738898, -41.45413358837856066, -21.97180651536612572 ) ) ;
#8074 = CARTESIAN_POINT ( 'NONE',  ( 3.661921753702003013, 6.578073271537795641, 46.57638968263120205 ) ) ;
#8075 = SURFACE_STYLE_FILL_AREA ( #3057 ) ;
#8076 = CARTESIAN_POINT ( 'NONE',  ( 0.5830082357119563685, 10.60551434635580748, 45.68101466022376655 ) ) ;
#8077 = LINE ( 'NONE', #35687, #23721 ) ;
#8078 = DIRECTION ( 'NONE',  ( 0.000000000000000000, 1.224646799147353207E-16, 1.000000000000000000 ) ) ;
#8079 = CARTESIAN_POINT ( 'NONE',  ( 0.2285344041767087553, -28.09782188418681059, -34.01490225856849747 ) ) ;
#8081 = ADVANCED_FACE ( 'NONE', ( #22065 ), #58155, .F. ) ;
#8080 = DIRECTION ( 'NONE',  ( -1.000000000000000000, -1.836909530733573776E-16, 1.925929944387235853E-32 ) ) ;
#8082 = CARTESIAN_POINT ( 'NONE',  ( 0.1073791018717483448, 30.83464511437097499, 30.14884492832400298 ) ) ;
#8083 = CARTESIAN_POINT ( 'NONE',  ( 4.694002226626920127, -38.39382765324673841, -24.58045503197449833 ) ) ;
#8084 = CARTESIAN_POINT ( 'NONE',  ( 3.390910168358336918, 17.02218646828075421, 40.55049080310516274 ) ) ;
#8085 = EDGE_CURVE ( 'NONE', #13905, #29266, #61182, .T. ) ;
#8086 = DIRECTION ( 'NONE',  ( 0.1736481776669314137, -0.9848077530122077983, 9.436895709313830594E-16 ) ) ;
#8087 = CARTESIAN_POINT ( 'NONE',  ( 4.960386119450140185, -9.684723978932076704, 42.66898857629788466 ) ) ;
#8088 = CARTESIAN_POINT ( 'NONE',  ( 2.533389852662419894, 32.46881123593813356, -29.71913236719125706 ) ) ;
#8089 = CIRCLE ( 'NONE', #45101, 48.09070567114147110 ) ;
#8090 = ORIENTED_EDGE ( 'NONE', *, *, #46081, .F. ) ;
#8091 = CARTESIAN_POINT ( 'NONE',  ( 0.8551540677456834771, -44.61036085020937492, -17.49081417858834087 ) ) ;
#8092 = CARTESIAN_POINT ( 'NONE',  ( -6.010958268070873523, -11.45964880703837174, 14.95835081545469869 ) ) ;
#8093 = CARTESIAN_POINT ( 'NONE',  ( 5.896782393890504181, -11.93563916323470764, -16.18847134979303704 ) ) ;
#8094 = CARTESIAN_POINT ( 'NONE',  ( 4.963659409799330291, -3.403493583737629002, 44.62477100936214214 ) ) ;
#8095 = ORIENTED_EDGE ( 'NONE', *, *, #50368, .F. ) ;
#8096 = CARTESIAN_POINT ( 'NONE',  ( 4.963659409799332067, -44.68724496494575504, 2.450325214228241233 ) ) ;
#8097 = CARTESIAN_POINT ( 'NONE',  ( 5.896782393890504181, -19.39988559968486115, -5.307591317834501332 ) ) ;
#8098 = ORIENTED_EDGE ( 'NONE', *, *, #60955, .F. ) ;
#8099 = EDGE_CURVE ( 'NONE', #29343, #15708, #25871, .T. ) ;
#8100 = DIRECTION ( 'NONE',  ( 0.000000000000000000, 0.000000000000000000, 1.000000000000000000 ) ) ;
#8101 = VERTEX_POINT ( 'NONE', #56484 ) ;
#8102 = CARTESIAN_POINT ( 'NONE',  ( 0.5980894510889457338, 29.84264441023728054, 37.73932204245528510 ) ) ;
#8103 = CARTESIAN_POINT ( 'NONE',  ( 4.956653778116996811, 40.28700667097716348, -26.26162724282331951 ) ) ;
#8104 = VERTEX_POINT ( 'NONE', #26442 ) ;
#8105 = CARTESIAN_POINT ( 'NONE',  ( 4.694002226626921015, -9.808094470216147442, -44.52062504401135357 ) ) ;
#8106 = CARTESIAN_POINT ( 'NONE',  ( 0.1097557419366048670, 26.42915440612286204, 34.07666148910654158 ) ) ;
#8107 = ORIENTED_EDGE ( 'NONE', *, *, #51347, .F. ) ;
#8108 = CARTESIAN_POINT ( 'NONE',  ( -14.84250595937556483, -4.999999999999993783, 6.123233995736803753E-16 ) ) ;
#8109 = CARTESIAN_POINT ( 'NONE',  ( 0.1064266418746777493, -15.98292515284435744, -40.05351192729354892 ) ) ;
#8110 = B_SPLINE_CURVE_WITH_KNOTS ( 'NONE', 3,
 ( #40701, #20639, #15951, #58515 ),
 .UNSPECIFIED., .F., .F.,
 ( 4, 4 ),
 ( 0.000000000000000000, 0.004048833967417087357 ),
 .UNSPECIFIED. ) ;
#8111 = ORIENTED_EDGE ( 'NONE', *, *, #2312, .F. ) ;
#8112 = FACE_OUTER_BOUND ( 'NONE', #50632, .T. ) ;
#8113 = ORIENTED_EDGE ( 'NONE', *, *, #19810, .F. ) ;
#8114 = CARTESIAN_POINT ( 'NONE',  ( 0.1157506346131639274, -1.321521084112260436, 44.10435626814069110 ) ) ;
#8115 = VERTEX_POINT ( 'NONE', #45573 ) ;
#8116 = VERTEX_POINT ( 'NONE', #36800 ) ;
#8117 = CARTESIAN_POINT ( 'NONE',  ( 0.8554163680231816613, 37.37991192211390512, 28.35397075908109343 ) ) ;
#8118 = LINE ( 'NONE', #7482, #3379 ) ;
#8119 = CARTESIAN_POINT ( 'NONE',  ( 0.3676999524040366896, -41.19158123804976412, -15.78620342045500280 ) ) ;
#8120 = CARTESIAN_POINT ( 'NONE',  ( 0.8744876279028263033, -0.6840263623742536270, -49.09055060105834656 ) ) ;
#8121 = CARTESIAN_POINT ( 'NONE',  ( 0.8744876279028306332, 41.62483489565916983, 26.03311679935014666 ) ) ;
#8122 = ORIENTED_EDGE ( 'NONE', *, *, #15658, .F. ) ;
#8123 = CARTESIAN_POINT ( 'NONE',  ( 2.533389852662419894, 5.798859955822282863, 43.63282886710852893 ) ) ;
#8124 = CARTESIAN_POINT ( 'NONE',  ( 0.9772918015221172539, -17.26359481638464288, 38.18776178000455701 ) ) ;
#8125 = DIRECTION ( 'NONE',  ( 0.000000000000000000, 0.000000000000000000, -1.000000000000000000 ) ) ;
#8126 = ORIENTED_EDGE ( 'NONE', *, *, #7708, .F. ) ;
#8127 = B_SPLINE_CURVE_WITH_KNOTS ( 'NONE', 3,
 ( #53698, #49330, #24299, #25524, #48413, #24612 ),
 .UNSPECIFIED., .F., .F.,
 ( 4, 2, 4 ),
 ( 1.736958732247374613E-17, 0.0002293319059085094391, 0.0004586638118170014767 ),
 .UNSPECIFIED. ) ;
#8128 = B_SPLINE_CURVE_WITH_KNOTS ( 'NONE', 3,
 ( #39969, #19925, #15517, #30213 ),
 .UNSPECIFIED., .F., .F.,
 ( 4, 4 ),
 ( 8.673617379884035472E-19, 0.004042984057420974560 ),
 .UNSPECIFIED. ) ;
#8129 = ORIENTED_EDGE ( 'NONE', *, *, #5691, .F. ) ;
#8130 = CARTESIAN_POINT ( 'NONE',  ( 0.6041374136657476912, -48.10739871142803992, 0.1745662470643146724 ) ) ;
#8131 = B_SPLINE_CURVE_WITH_KNOTS ( 'NONE', 3,
 ( #5743, #24891, #44032, #1066, #20201, #39311 ),
 .UNSPECIFIED., .F., .F.,
 ( 4, 2, 4 ),
 ( 5.421010862427522170E-19, 0.0002293801035737082878, 0.0004587602071474160335 ),
 .UNSPECIFIED. ) ;
#8132 = CYLINDRICAL_SURFACE ( 'NONE', #55782, 2.649999999999992806 ) ;
#8133 = CARTESIAN_POINT ( 'NONE',  ( 0.5824935313925948543, -44.18041403804779321, 15.72670316628720144 ) ) ;
#8134 = ORIENTED_EDGE ( 'NONE', *, *, #5282, .T. ) ;
#8135 = CARTESIAN_POINT ( 'NONE',  ( 3.376099380956842921, 10.22925587767808331, -8.664335394076998043 ) ) ;
#8136 = CARTESIAN_POINT ( 'NONE',  ( 4.956445790444005794, -28.36659270909926533, -37.58822246682746737 ) ) ;
#8137 = EDGE_CURVE ( 'NONE', #25214, #42400, #21752, .T. ) ;
#8138 = ORIENTED_EDGE ( 'NONE', *, *, #53858, .F. ) ;
#8139 = CARTESIAN_POINT ( 'NONE',  ( 0.8557997880470599172, 34.51495345639595058, -33.22501220301865033 ) ) ;
#8140 = ADVANCED_FACE ( 'NONE', ( #47414 ), #8957, .F. ) ;
#8141 = CARTESIAN_POINT ( 'NONE',  ( 0.8753041380234471980, -20.68664920503345428, 44.53314352862224013 ) ) ;
#8142 = DIRECTION ( 'NONE',  ( -1.000000000000000000, -0.000000000000000000, -0.000000000000000000 ) ) ;
#8143 = CARTESIAN_POINT ( 'NONE',  ( 3.221118495291109163, -39.21725469344816872, -19.91904500649992471 ) ) ;
#8144 = CARTESIAN_POINT ( 'NONE',  ( 1.834102595619085507, -43.50031898818188125, 6.922426798753990695 ) ) ;
#8145 = CARTESIAN_POINT ( 'NONE',  ( 0.7954196712028471783, -5.415566793625004927, -47.79303691884129535 ) ) ;
#8146 =( BOUNDED_SURFACE ( )  B_SPLINE_SURFACE ( 3, 1, ( 
 ( #654, #31260 ),
 ( #41005, #19792 ),
 ( #45082, #1808 ),
 ( #11548, #30628 ) ),
 .UNSPECIFIED., .F., .F., .F. ) 
 B_SPLINE_SURFACE_WITH_KNOTS ( ( 4, 4 ),
 ( 2, 2 ),
 ( 0.000000000000000000, 1.000000000000000000 ),
 ( 0.000000000000000000, 1.000000000000000000 ),
 .UNSPECIFIED. ) 
 GEOMETRIC_REPRESENTATION_ITEM ( )  RATIONAL_B_SPLINE_SURFACE ( (
 ( 1.000000000000000000, 1.000000000000000000),
 ( 0.7282232189291693025, 0.9929344683865674037),
 ( 0.7282232189291693025, 0.9929344683865674037),
 ( 1.000000000000000000, 1.000000000000000000) ) ) 
 REPRESENTATION_ITEM ( '' )  SURFACE ( )  );
#8147 = VERTEX_POINT ( 'NONE', #4161 ) ;
#8148 = CARTESIAN_POINT ( 'NONE',  ( 0.3676999524040366896, -44.10520818713899871, 0.8253448321555690859 ) ) ;
#8149 = CARTESIAN_POINT ( 'NONE',  ( 5.960721111146673579, -16.28018152803701213, 12.50019045452710742 ) ) ;
#8150 = CARTESIAN_POINT ( 'NONE',  ( 5.981074661064941900, -16.28853686865607386, 12.48781255314261607 ) ) ;
#8152 = EDGE_CURVE ( 'NONE', #15900, #24850, #14529, .T. ) ;
#8151 = CARTESIAN_POINT ( 'NONE',  ( 0.1092565886968784594, -16.78938711553603014, -39.72209809039391359 ) ) ;
#8153 = CARTESIAN_POINT ( 'NONE',  ( 4.975610109902397937, 34.73360008816130318, 34.43873447229810836 ) ) ;
#8154 = ADVANCED_FACE ( 'NONE', ( #52093 ), #15377, .F. ) ;
#8155 = CARTESIAN_POINT ( 'NONE',  ( 4.962356264823593044, 18.10963840443015016, 37.99048031708913697 ) ) ;
#8156 = CARTESIAN_POINT ( 'NONE',  ( 0.5786265663353153954, -11.69877690266688219, 46.45062944555890994 ) ) ;
#8157 = CARTESIAN_POINT ( 'NONE',  ( 0.2885697896453121580, 33.71073718007502151, 26.88157175352899486 ) ) ;
#8158 = CARTESIAN_POINT ( 'NONE',  ( 0.5998501479064708430, 33.64490850298796687, 34.38546660123309096 ) ) ;
#8159 = VERTEX_POINT ( 'NONE', #57390 ) ;
#8160 = CARTESIAN_POINT ( 'NONE',  ( 0.6252788684277222897, 46.38381364802560114, -16.12408641253514219 ) ) ;
#8161 = CARTESIAN_POINT ( 'NONE',  ( 2.359973842542475442, 23.93452390393565921, -36.94962056807123219 ) ) ;
#8162 = CARTESIAN_POINT ( 'NONE',  ( 0.5987334363312692975, -42.48817524472720208, -24.62352271397064030 ) ) ;
#8163 = CARTESIAN_POINT ( 'NONE',  ( 0.6064515330803602611, -45.81048872046274312, 10.03660596165072150 ) ) ;
#8164 = VERTEX_POINT ( 'NONE', #19844 ) ;
#8165 = CARTESIAN_POINT ( 'NONE',  ( 0.5997462898726536595, 44.01516392039513903, -21.77652348757843015 ) ) ;
#8166 = B_SPLINE_CURVE_WITH_KNOTS ( 'NONE', 3,
 ( #31562, #26551, #45678, #60062 ),
 .UNSPECIFIED., .F., .F.,
 ( 4, 4 ),
 ( 2.216451077356609476E-17, 0.004564976165746189446 ),
 .UNSPECIFIED. ) ;
#8167 = AXIS2_PLACEMENT_3D ( 'NONE', #17572, #26969, #45475 ) ;
#8168 = ORIENTED_EDGE ( 'NONE', *, *, #50405, .T. ) ;
#8169 = CARTESIAN_POINT ( 'NONE',  ( 0.1129192098497455998, 4.719118110135312349, -43.87119455916086963 ) ) ;
#8170 = ADVANCED_FACE ( 'NONE', ( #19229 ), #551, .T. ) ;
#8171 = CARTESIAN_POINT ( 'NONE',  ( 5.838029081930957709, 44.61407408311379186, -15.51288019225814985 ) ) ;
#8172 = CARTESIAN_POINT ( 'NONE',  ( 0.5980894510889448457, -5.583794302584927038, -47.78766676462073804 ) ) ;
#8173 = ORIENTED_EDGE ( 'NONE', *, *, #51612, .T. ) ;
#8174 = DIRECTION ( 'NONE',  ( -1.000000000000000000, -0.000000000000000000, -0.000000000000000000 ) ) ;
#8175 = VERTEX_POINT ( 'NONE', #381 ) ;
#8176 = ORIENTED_EDGE ( 'NONE', *, *, #8686, .F. ) ;
#8177 = CARTESIAN_POINT ( 'NONE',  ( -6.057079549204054558, 7.787131596469407668, 17.61226313109721531 ) ) ;
#8178 = ORIENTED_EDGE ( 'NONE', *, *, #34680, .F. ) ;
#8179 = CARTESIAN_POINT ( 'NONE',  ( 0.1119899015040013157, -13.09165644557430852, 42.13751107627926729 ) ) ;
#8180 = ORIENTED_EDGE ( 'NONE', *, *, #42372, .T. ) ;
#8181 = CARTESIAN_POINT ( 'NONE',  ( 0.8560838555295223751, -35.39593983670150124, -30.78149244527203621 ) ) ;
#8182 = CARTESIAN_POINT ( 'NONE',  ( 0.9754402186311947887, 16.59348191374138537, 39.57010335554335256 ) ) ;
#8183 = VERTEX_POINT ( 'NONE', #33631 ) ;
#8184 = DIRECTION ( 'NONE',  ( -0.07439287786467649322, -0.2453289374370202780, 0.9665813013808169929 ) ) ;
#8185 = CARTESIAN_POINT ( 'NONE',  ( 50.15117465005047137, 12.21965674021488368, -2.632719331364402393 ) ) ;
#8186 = CARTESIAN_POINT ( 'NONE',  ( 1.112077966505210957, -37.88145627207394739, 22.53942314779827427 ) ) ;
#8187 = CARTESIAN_POINT ( 'NONE',  ( 0.5837157313716003770, -30.34684335673147260, 35.75340769582711431 ) ) ;
#8188 = VERTEX_POINT ( 'NONE', #57094 ) ;
#8189 = CYLINDRICAL_SURFACE ( 'NONE', #25650, 16.00000000000000000 ) ;
#8190 = ORIENTED_EDGE ( 'NONE', *, *, #30401, .T. ) ;
#8191 = CARTESIAN_POINT ( 'NONE',  ( 0.9730545539215883499, -42.90536227157002003, -0.5054011016617259155 ) ) ;
#8192 = ORIENTED_EDGE ( 'NONE', *, *, #38584, .F. ) ;
#8193 = CARTESIAN_POINT ( 'NONE',  ( 0.1156867017252034557, -12.67428682873097756, 42.26470466782232904 ) ) ;
#8194 = CARTESIAN_POINT ( 'NONE',  ( 0.6041374136657476912, -29.14743607025112482, 38.27243465845292292 ) ) ;
#8195 = VERTEX_POINT ( 'NONE', #37731 ) ;
#8196 = CARTESIAN_POINT ( 'NONE',  ( 1.227938101723756947, -42.65467462194914816, -4.762198645644879491 ) ) ;
#8197 = CARTESIAN_POINT ( 'NONE',  ( 2.648799415243708655, -18.57388519568396390, 45.38202564922758597 ) ) ;
#8198 = CARTESIAN_POINT ( 'NONE',  ( -6.079354080745853928, -18.90066517279534963, -3.682093327720422415 ) ) ;
#8199 = CARTESIAN_POINT ( 'NONE',  ( 0.5997462898726536595, -45.71211507932765983, -17.94308126043611296 ) ) ;
#8200 = ADVANCED_FACE ( 'NONE', ( #9810 ), #13120, .F. ) ;
#8201 = ORIENTED_EDGE ( 'NONE', *, *, #31758, .F. ) ;
#8202 = ORIENTED_EDGE ( 'NONE', *, *, #4082, .T. ) ;
#8203 = CARTESIAN_POINT ( 'NONE',  ( 0.7764139734771254853, 44.99430973300147230, 13.24962499686677653 ) ) ;
#8204 = EDGE_CURVE ( 'NONE', #24845, #44371, #42424, .T. ) ;
#8205 = CARTESIAN_POINT ( 'NONE',  ( 0.8744876279028263033, -26.20733431478184983, 41.51536677536103070 ) ) ;
#8206 = CARTESIAN_POINT ( 'NONE',  ( 0.5998501479064708430, 6.798102206414135651, -47.62484632993681544 ) ) ;
#8207 = ADVANCED_FACE ( 'NONE', ( #61786 ), #27920, .F. ) ;
#8208 = CARTESIAN_POINT ( 'NONE',  ( 0.5980271706414734822, -26.05568637495906614, -41.63112357805678698 ) ) ;
#8209 = LINE ( 'NONE', #8511, #3802 ) ;
#8210 = CONICAL_SURFACE ( 'NONE', #22229, 42.08604991992415023, 1.569615340895231137 ) ;
#8211 = CARTESIAN_POINT ( 'NONE',  ( 4.553261556744875094, 12.28162544311214432, 42.17465165592641796 ) ) ;
#8212 = DIRECTION ( 'NONE',  ( 0.000000000000000000, 0.000000000000000000, 1.000000000000000000 ) ) ;
#8213 = CARTESIAN_POINT ( 'NONE',  ( 5.838029081930955932, 35.04472919977185086, -31.66910187339669491 ) ) ;
#8214 = CARTESIAN_POINT ( 'NONE',  ( 0.6067099128993228563, 0.7089426894590579176, 47.89177823194876282 ) ) ;
#8215 = CARTESIAN_POINT ( 'NONE',  ( -6.072942160501519027, 13.82262479916533771, 13.40668512162942072 ) ) ;
#8216 = CARTESIAN_POINT ( 'NONE',  ( -6.072942160501519027, 5.492864488351536068, -18.45623477314988747 ) ) ;
#8217 = EDGE_CURVE ( 'NONE', #5057, #35220, #35610, .T. ) ;
#8218 = FACE_OUTER_BOUND ( 'NONE', #28377, .T. ) ;
#8219 = CARTESIAN_POINT ( 'NONE',  ( 4.975801465491695552, -26.14269827151708370, 40.15204426031488794 ) ) ;
#8220 = CARTESIAN_POINT ( 'NONE',  ( 0.9749527285493316819, 37.01618455594573476, 21.70110358462052957 ) ) ;
#8221 = FACE_OUTER_BOUND ( 'NONE', #3472, .T. ) ;
#8222 = CARTESIAN_POINT ( 'NONE',  ( 0.9752132459055862235, -37.27572867006947632, -21.25214916889629890 ) ) ;
#8223 = CARTESIAN_POINT ( 'NONE',  ( -5.995132425357893702, -4.885449473615202542, -18.19985213254577161 ) ) ;
#8224 = CARTESIAN_POINT ( 'NONE',  ( 0.6027444965799114707, -47.53431580546581614, 12.32993660947551895 ) ) ;
#8226 = ORIENTED_EDGE ( 'NONE', *, *, #32665, .F. ) ;
#8225 = CARTESIAN_POINT ( 'NONE',  ( 0.9730545539215892381, 39.44597740938061037, 16.88610103448572630 ) ) ;
#8227 = VERTEX_POINT ( 'NONE', #4771 ) ;
#8228 = CARTESIAN_POINT ( 'NONE',  ( 0.6029443449137436017, -39.38137730902946743, 29.33677997373246882 ) ) ;
#8229 = CARTESIAN_POINT ( 'NONE',  ( 0.8554163680231708922, -8.703479761965583705, 46.10265624825618147 ) ) ;
#8230 = CARTESIAN_POINT ( 'NONE',  ( 4.956653778116987041, -48.02038484091099235, -2.599733001514835884 ) ) ;
#8231 = ORIENTED_EDGE ( 'NONE', *, *, #23352, .F. ) ;
#8232 = ORIENTED_EDGE ( 'NONE', *, *, #54819, .F. ) ;
#8233 = DIRECTION ( 'NONE',  ( -1.000000000000000000, -5.380183451256670742E-17, 1.298891185607911324E-16 ) ) ;
#8234 = CARTESIAN_POINT ( 'NONE',  ( 0.1119899015040013435, 43.19989886304176707, 8.984990062068465733 ) ) ;
#8235 = EDGE_LOOP ( 'NONE', ( #25664, #60476, #24579, #39128 ) ) ;
#8236 = ORIENTED_EDGE ( 'NONE', *, *, #49791, .T. ) ;
#8237 = CARTESIAN_POINT ( 'NONE',  ( 1.157644175074336701, -37.77649504501447097, 18.16421475300208144 ) ) ;
#8238 = DIRECTION ( 'NONE',  ( -1.000000000000000000, -0.000000000000000000, -0.000000000000000000 ) ) ;
#8239 = CARTESIAN_POINT ( 'NONE',  ( 0.9749527285493317930, -41.51939261707890694, 10.82939760924488581 ) ) ;
#8240 = EDGE_CURVE ( 'NONE', #18777, #36635, #52836, .T. ) ;
#8241 = ORIENTED_EDGE ( 'NONE', *, *, #20312, .F. ) ;
#8242 = CARTESIAN_POINT ( 'NONE',  ( 4.975801465491694664, 26.14269827151623105, 40.15204426031542795 ) ) ;
#8243 = VECTOR ( 'NONE', #36010, 1000.000000000000227 ) ;
#8244 = ADVANCED_FACE ( 'NONE', ( #23912 ), #7032, .F. ) ;
#8245 = CARTESIAN_POINT ( 'NONE',  ( 0.8744876279028306332, -31.30103973185180521, -37.82320666052162039 ) ) ;
#8246 = VECTOR ( 'NONE', #43516, 1000.000000000000000 ) ;
#8247 = CARTESIAN_POINT ( 'NONE',  ( 0.1103310638050662290, 21.49083802119848841, 37.38800124003719105 ) ) ;
#8248 = VERTEX_POINT ( 'NONE', #58951 ) ;
#8249 = EDGE_CURVE ( 'NONE', #34923, #24850, #21435, .T. ) ;
#8250 = ORIENTED_EDGE ( 'NONE', *, *, #56975, .F. ) ;
#8251 = CARTESIAN_POINT ( 'NONE',  ( 0.6846871229502932144, -41.05093867799167384, -24.69859318104532164 ) ) ;
#8252 = B_SPLINE_CURVE_WITH_KNOTS ( 'NONE', 3,
 ( #50429, #22552, #60423, #60735 ),
 .UNSPECIFIED., .F., .F.,
 ( 4, 4 ),
 ( 2.308109569601360422E-17, 0.004559932413162185935 ),
 .UNSPECIFIED. ) ;
#8253 = EDGE_LOOP ( 'NONE', ( #53092, #54110, #50473, #48009 ) ) ;
#8254 = CARTESIAN_POINT ( 'NONE',  ( 0.6027444965799114707, -48.72077702715109382, 6.150154612533532905 ) ) ;
#8255 = CARTESIAN_POINT ( 'NONE',  ( 3.660087539127319989, 30.71416465583057231, 36.93668088065460609 ) ) ;
#8256 = CARTESIAN_POINT ( 'NONE',  ( 0.6023143664670691511, 34.20175727332128446, -33.83148565876894764 ) ) ;
#8257 = CARTESIAN_POINT ( 'NONE',  ( 0.7242003506639995702, -29.97003518583413140, 38.89484111146220613 ) ) ;
#8258 = CARTESIAN_POINT ( 'NONE',  ( 1.479689385636123067, -43.83641450621821889, -4.466834282432383674 ) ) ;
#8259 = ORIENTED_EDGE ( 'NONE', *, *, #9041, .T. ) ;
#8260 = CARTESIAN_POINT ( 'NONE',  ( 0.3622758884714730732, -41.85013935980095567, -10.35929834645908265 ) ) ;
#8261 = FACE_OUTER_BOUND ( 'NONE', #5997, .T. ) ;
#8262 = CARTESIAN_POINT ( 'NONE',  ( 10.00000000000002132, -80.00000000000001421, -2.532597876869216023E-31 ) ) ;
#8263 = CIRCLE ( 'NONE', #60308, 15.43999999999999240 ) ;
#8264 = VERTEX_POINT ( 'NONE', #1310 ) ;
#8265 = DIRECTION ( 'NONE',  ( 0.000000000000000000, 0.000000000000000000, 1.000000000000000000 ) ) ;
#8266 = CARTESIAN_POINT ( 'NONE',  ( 5.880360259849752858, -36.03610316515361234, -31.66572319753549536 ) ) ;
#8267 = CARTESIAN_POINT ( 'NONE',  ( -6.063463321072278589, 12.01854346922056749, -15.04576569530197006 ) ) ;
#8268 = LINE ( 'NONE', #32412, #27407 ) ;
#8269 = EDGE_CURVE ( 'NONE', #29773, #54373, #53933, .T. ) ;
#8270 = ORIENTED_EDGE ( 'NONE', *, *, #18755, .F. ) ;
#8271 = CARTESIAN_POINT ( 'NONE',  ( 0.9754292589017210524, -41.77202903865140371, 3.380097171582762794 ) ) ;
#8272 = CARTESIAN_POINT ( 'NONE',  ( 4.549368137175248350, 8.166781970325150297, 42.14271863032836762 ) ) ;
#8273 = CARTESIAN_POINT ( 'NONE',  ( -6.078726893082806448, 0.6137717894420866571, -19.24622886331774652 ) ) ;
#8274 = EDGE_CURVE ( 'NONE', #37463, #37711, #43978, .T. ) ;
#8275 = CARTESIAN_POINT ( 'NONE',  ( 0.5834584762367753807, -46.80309860109110787, 2.950584747085512660 ) ) ;
#8276 = LINE ( 'NONE', #18330, #24019 ) ;
#8277 = CARTESIAN_POINT ( 'NONE',  ( 0.7762783648524376190, -7.133808749409126904, -47.37038525648367937 ) ) ;
#8278 = CARTESIAN_POINT ( 'NONE',  ( 0.9730545539215892381, -21.89037132892461912, 36.90443313492323085 ) ) ;
#8279 = CARTESIAN_POINT ( 'NONE',  ( 0.9790724872846768845, 41.90863365906401583, 0.04043280624974921605 ) ) ;
#8280 = B_SPLINE_CURVE_WITH_KNOTS ( 'NONE', 3,
 ( #14858, #38367, #18629, #4797 ),
 .UNSPECIFIED., .F., .F.,
 ( 4, 4 ),
 ( 6.938893903907227607E-18, 0.005013413432710145043 ),
 .UNSPECIFIED. ) ;
#8281 = CARTESIAN_POINT ( 'NONE',  ( 0.8744876279028306332, -2.462621419132613454, -49.03351451941336592 ) ) ;
#8282 = ORIENTED_EDGE ( 'NONE', *, *, #46260, .F. ) ;
#8283 = CARTESIAN_POINT ( 'NONE',  ( 0.6067099128993238555, 11.71051825714768135, -46.44339333106602652 ) ) ;
#8284 = CARTESIAN_POINT ( 'NONE',  ( 2.643462169533613793, 47.78621045426868363, 4.896978544602314187 ) ) ;
#8285 = CARTESIAN_POINT ( 'NONE',  ( 0.1156867017252034557, -35.28683493765469592, -26.49116998846783844 ) ) ;
#8286 = CARTESIAN_POINT ( 'NONE',  ( 0.5835226383429282793, -34.90249509102868331, -31.32185037584284970 ) ) ;
#8287 = ADVANCED_FACE ( 'NONE', ( #24840 ), #46603, .F. ) ;
#8288 = CARTESIAN_POINT ( 'NONE',  ( 0.8560838555295158248, 21.73747136795142154, 41.56747734237938374 ) ) ;
#8289 = CONICAL_SURFACE ( 'NONE', #2295, 4.000000000000000000, 1.047197551196595855 ) ;
#8290 = CARTESIAN_POINT ( 'NONE',  ( 0.1098349054025746507, 42.72717686504321932, 5.840292671757814524 ) ) ;
#8291 = APPLICATION_PROTOCOL_DEFINITION ( 'draft international standard', 'automotive_design', 1998, #33157 ) ;
#8292 = FACE_OUTER_BOUND ( 'NONE', #12144, .T. ) ;
#8293 = CARTESIAN_POINT ( 'NONE',  ( 0.5839879882012665169, 12.39641777360522390, 46.26394433311391907 ) ) ;
#8294 = CARTESIAN_POINT ( 'NONE',  ( 0.1310142868023690677, 6.259743112235529594, -42.66681113736512287 ) ) ;
#8296 = EDGE_LOOP ( 'NONE', ( #13919, #10120, #9332, #16909 ) ) ;
#8295 = CARTESIAN_POINT ( 'NONE',  ( 4.956653778116966613, 48.02038484091100656, 2.599733001514495712 ) ) ;
#8297 = ORIENTED_EDGE ( 'NONE', *, *, #26239, .F. ) ;
#8298 = CARTESIAN_POINT ( 'NONE',  ( 0.5804410086790514622, -24.77328595090334318, -39.82215658462223473 ) ) ;
#8299 = DIRECTION ( 'NONE',  ( 0.07439287786467665975, 0.9903339163990680927, -0.1170659376278801317 ) ) ;
#8300 = CARTESIAN_POINT ( 'NONE',  ( 0.5809828226811617480, 47.55412398569215071, -5.711058609464832792 ) ) ;
#8301 = ORIENTED_EDGE ( 'NONE', *, *, #34172, .F. ) ;
#8302 = CARTESIAN_POINT ( 'NONE',  ( 2.282803330402959130, 42.71620289003610793, 19.54028961183163204 ) ) ;
#8304 = CARTESIAN_POINT ( 'NONE',  ( 0.5834584762367742705, -45.99222294191854132, 9.162500634327543025 ) ) ;
#8303 = CIRCLE ( 'NONE', #43354, 43.92652462719577500 ) ;
#8305 = DIRECTION ( 'NONE',  ( -1.000000000000000000, -0.000000000000000000, -0.000000000000000000 ) ) ;
#8306 =( BOUNDED_SURFACE ( )  B_SPLINE_SURFACE ( 3, 1, ( 
 ( #61808, #37434 ),
 ( #56198, #37754 ),
 ( #28017, #33352 ),
 ( #33043, #60580 ) ),
 .UNSPECIFIED., .F., .F., .F. ) 
 B_SPLINE_SURFACE_WITH_KNOTS ( ( 4, 4 ),
 ( 2, 2 ),
 ( 0.000000000000000000, 1.000000000000000000 ),
 ( 0.000000000000000000, 1.000000000000000000 ),
 .UNSPECIFIED. ) 
 GEOMETRIC_REPRESENTATION_ITEM ( )  RATIONAL_B_SPLINE_SURFACE ( (
 ( 1.000000000000000000, 1.000000000000000000),
 ( 0.9953040768229005630, 0.8617119497784937465),
 ( 0.9953040768229005630, 0.8617119497784937465),
 ( 1.000000000000000000, 1.000000000000000000) ) ) 
 REPRESENTATION_ITEM ( '' )  SURFACE ( )  );
#8307 = VERTEX_POINT ( 'NONE', #49554 ) ;
#8308 = ORIENTED_EDGE ( 'NONE', *, *, #46271, .F. ) ;
#8309 = CARTESIAN_POINT ( 'NONE',  ( 0.9741495583595169983, 41.34222751889826242, 11.48707840139599767 ) ) ;
#8310 = CARTESIAN_POINT ( 'NONE',  ( 0.9268187852002115479, 37.48124960562999775, 23.21444078389758303 ) ) ;
#8311 = CARTESIAN_POINT ( 'NONE',  ( 0.9784957157296372277, 32.74509629232474595, -26.15514721424351308 ) ) ;
#8312 = EDGE_CURVE ( 'NONE', #17976, #22076, #35662, .T. ) ;
#8313 = CARTESIAN_POINT ( 'NONE',  ( 1.479689385636123067, -44.04772423883621002, 1.175514630760941648 ) ) ;
#8314 = EDGE_CURVE ( 'NONE', #49156, #5480, #20665, .T. ) ;
#8315 = CARTESIAN_POINT ( 'NONE',  ( 0.1158516988532803660, -42.69354052901408636, -11.14467388173511431 ) ) ;
#8316 =( BOUNDED_SURFACE ( )  B_SPLINE_SURFACE ( 3, 1, ( 
 ( #14762, #48269 ),
 ( #39199, #35109 ),
 ( #10672, #45136 ),
 ( #11604, #26002 ) ),
 .UNSPECIFIED., .F., .F., .F. ) 
 B_SPLINE_SURFACE_WITH_KNOTS ( ( 4, 4 ),
 ( 2, 2 ),
 ( 0.000000000000000000, 1.000000000000000000 ),
 ( 0.000000000000000000, 1.000000000000000000 ),
 .UNSPECIFIED. ) 
 GEOMETRIC_REPRESENTATION_ITEM ( )  RATIONAL_B_SPLINE_SURFACE ( (
 ( 1.000000000000000000, 1.000000000000000000),
 ( 0.7211978278499970862, 0.9934217856018976445),
 ( 0.7211978278499970862, 0.9934217856018976445),
 ( 1.000000000000000000, 1.000000000000000000) ) ) 
 REPRESENTATION_ITEM ( '' )  SURFACE ( )  );
#8317 = CARTESIAN_POINT ( 'NONE',  ( 0.6000166863083090663, 17.45040302316650838, -45.90541270958704700 ) ) ;
#8318 = ORIENTED_EDGE ( 'NONE', *, *, #6403, .F. ) ;
#8319 = EDGE_CURVE ( 'NONE', #35750, #31302, #7212, .T. ) ;
#8320 = EDGE_CURVE ( 'NONE', #31692, #49531, #27575, .T. ) ;
#8321 = LINE ( 'NONE', #16832, #8839 ) ;
#8322 = CARTESIAN_POINT ( 'NONE',  ( 0.3676999524040366896, 9.009680404096547690, -43.18305503711933113 ) ) ;
#8323 = ORIENTED_EDGE ( 'NONE', *, *, #56024, .F. ) ;
#8324 = CARTESIAN_POINT ( 'NONE',  ( 0.5998501479064708430, -47.62484632993683675, -6.798102206413969562 ) ) ;
#8325 = ADVANCED_FACE ( 'NONE', ( #26372 ), #52471, .F. ) ;
#8326 = DIRECTION ( 'NONE',  ( 0.09722883295013594329, 0.9421506058508687387, -0.3207784125186660673 ) ) ;
#8327 = CARTESIAN_POINT ( 'NONE',  ( 2.706805983486680667, 38.90419121147174053, -20.57279804744605656 ) ) ;
#8328 = CARTESIAN_POINT ( 'NONE',  ( 4.553261556744873317, -4.442710778081946366, -43.70128015019640344 ) ) ;
#8329 = B_SPLINE_CURVE_WITH_KNOTS ( 'NONE', 3,
 ( #44628, #1360, #53373, #53670, #39312, #58370, #19904, #6354, #11407, #33999, #30192, #49298, #5744, #29270, #10175, #39622, #14893, #1067, #58679 ),
 .UNSPECIFIED., .F., .F.,
 ( 4, 3, 3, 3, 3, 3, 4 ),
 ( 0.000000000000000000, 0.0002612768053151685106, 0.0003919133833142900581, 0.0005225499612322606451, 0.0006531865391693344406, 0.0008112755173415184479, 0.0009693688056799704047 ),
 .UNSPECIFIED. ) ;
#8330 = VECTOR ( 'NONE', #21946, 1000.000000000000000 ) ;
#8331 = ORIENTED_EDGE ( 'NONE', *, *, #1677, .F. ) ;
#8332 = ORIENTED_EDGE ( 'NONE', *, *, #48397, .T. ) ;
#8333 = CARTESIAN_POINT ( 'NONE',  ( 1.000110580585052977, -31.51987383986781666, 27.62091663740936198 ) ) ;
#8334 = CARTESIAN_POINT ( 'NONE',  ( -1.200000000000000622, 6.887500000000022382, 0.000000000000000000 ) ) ;
#8335 = ORIENTED_EDGE ( 'NONE', *, *, #31336, .T. ) ;
#8336 = ADVANCED_FACE ( 'NONE', ( #40505 ), #26265, .F. ) ;
#8337 = ORIENTED_EDGE ( 'NONE', *, *, #57983, .F. ) ;
#8338 = DIRECTION ( 'NONE',  ( -1.000000000000000000, 0.000000000000000000, 0.000000000000000000 ) ) ;
#8339 = ORIENTED_EDGE ( 'NONE', *, *, #61076, .F. ) ;
#8340 = CARTESIAN_POINT ( 'NONE',  ( 5.440000000000000391, 6.831466544798160849E-15, 0.000000000000000000 ) ) ;
#8341 = CARTESIAN_POINT ( 'NONE',  ( 0.8551540677456739292, -43.91216198251525782, -19.17641535420899146 ) ) ;
#8342 = EDGE_CURVE ( 'NONE', #37554, #44352, #15472, .T. ) ;
#8343 = CARTESIAN_POINT ( 'NONE',  ( 0.8557997880470599172, -7.156447707086029730, 47.37054680076704472 ) ) ;
#8344 = ORIENTED_EDGE ( 'NONE', *, *, #2713, .F. ) ;
#8345 = CARTESIAN_POINT ( 'NONE',  ( 0.8554163680231816613, -34.17638377241251391, 32.14312158693671506 ) ) ;
#8346 = CARTESIAN_POINT ( 'NONE',  ( 0.1158816050234199174, -27.50652624945415781, 34.50120367455677695 ) ) ;
#8347 = CARTESIAN_POINT ( 'NONE',  ( 0.8753041380234524160, -0.6841799139051519818, 49.09857661601188283 ) ) ;
#8348 = AXIS2_PLACEMENT_3D ( 'NONE', #14921, #10510, #58399 ) ;
#8349 = B_SPLINE_CURVE_WITH_KNOTS ( 'NONE', 3,
 ( #35632, #44723, #10892, #11824, #59088, #50018 ),
 .UNSPECIFIED., .F., .F.,
 ( 4, 2, 4 ),
 ( 0.000000000000000000, 0.0002450742804987326583, 0.0004901485609974653166 ),
 .UNSPECIFIED. ) ;
#8350 = VERTEX_POINT ( 'NONE', #60798 ) ;
#8351 = CARTESIAN_POINT ( 'NONE',  ( -19.02632894112265305, -12.36669073209966641, -1.822342842981515831 ) ) ;
#8352 = CARTESIAN_POINT ( 'NONE',  ( 3.376099380956842921, -0.9076095657322794663, -13.37477583020583971 ) ) ;
#8353 = DIRECTION ( 'NONE',  ( 0.000000000000000000, 0.000000000000000000, 1.000000000000000000 ) ) ;
#8354 = CARTESIAN_POINT ( 'NONE',  ( 0.6009453534118440743, 47.75104957283898699, -5.846398087358881668 ) ) ;
#8355 = CARTESIAN_POINT ( 'NONE',  ( 0.7056555295713307085, 23.21854706865639173, -41.89804573586712166 ) ) ;
#8356 = ORIENTED_EDGE ( 'NONE', *, *, #2471, .T. ) ;
#8357 = CARTESIAN_POINT ( 'NONE',  ( 0.1081432562775997974, 37.55692207416026918, -21.19449538864519056 ) ) ;
#8358 = FACE_OUTER_BOUND ( 'NONE', #52722, .T. ) ;
#8359 = ORIENTED_EDGE ( 'NONE', *, *, #53462, .T. ) ;
#8360 = CARTESIAN_POINT ( 'NONE',  ( 5.960221823109900008, -7.849768660536680542, 18.96526051813967229 ) ) ;
#8361 = CARTESIAN_POINT ( 'NONE',  ( 5.901764892641307547, 45.40663509823473731, -18.33654701669415843 ) ) ;
#8362 = CARTESIAN_POINT ( 'NONE',  ( 4.303969348037246512, 4.133486515473304479, 47.93217632892349656 ) ) ;
#8363 = CARTESIAN_POINT ( 'NONE',  ( 0.1119898979215351448, 19.90994801901936739, -39.37709077791013357 ) ) ;
#8364 = EDGE_CURVE ( 'NONE', #22852, #26491, #50790, .T. ) ;
#8365 = CARTESIAN_POINT ( 'NONE',  ( 0.8751705887134423323, -38.69254731947852832, 28.56654290188588163 ) ) ;
#8366 = CARTESIAN_POINT ( 'NONE',  ( -2.569797478183783568, -2.353985772484652017, -14.44232325624825819 ) ) ;
#8367 = CARTESIAN_POINT ( 'NONE',  ( 5.838029081930955932, 1.598329895849277538, -47.20710115752665104 ) ) ;
#8368 = CARTESIAN_POINT ( 'NONE',  ( 4.303969348037258058, -10.35452842635876003, 46.98258166031687466 ) ) ;
#8369 = EDGE_CURVE ( 'NONE', #19302, #3395, #22884, .T. ) ;
#8370 = CARTESIAN_POINT ( 'NONE',  ( 0.8751705887134553219, -11.58504748649232496, 46.67919521768867241 ) ) ;
#8371 = DIRECTION ( 'NONE',  ( 0.07836865515943411409, -0.1223011693452849408, -0.9893941468723562727 ) ) ;
#8372 = CARTESIAN_POINT ( 'NONE',  ( 0.7948884756798513251, 48.35174766733348406, -8.532710127190703986 ) ) ;
#8373 = CARTESIAN_POINT ( 'NONE',  ( -6.072942160501519915, -18.27985097084430777, -6.054024345238677718 ) ) ;
#8374 = CARTESIAN_POINT ( 'NONE',  ( 5.896278296736517710, 17.95357321928062433, 9.066211351734164481 ) ) ;
#8375 = CARTESIAN_POINT ( 'NONE',  ( 0.5997462898726536595, -1.051648045106814422, -49.09628974305016413 ) ) ;
#8376 = CARTESIAN_POINT ( 'NONE',  ( 5.895596859100789899, -17.30698493747174993, -10.24677781483592121 ) ) ;
#8377 = PRODUCT_RELATED_PRODUCT_CATEGORY ( 'part', '', ( #27294 ) ) ;
#8378 = AXIS2_PLACEMENT_3D ( 'NONE', #7667, #26792, #55906 ) ;
#8379 = CARTESIAN_POINT ( 'NONE',  ( 0.8744876279028263033, -49.08725279547490317, -0.8897546699139439186 ) ) ;
#8380 = CARTESIAN_POINT ( 'NONE',  ( 9.999999999999994671, 56.56854249492371878, 56.56854249492391062 ) ) ;
#8381 = DIRECTION ( 'NONE',  ( 0.000000000000000000, 0.000000000000000000, 1.000000000000000000 ) ) ;
#8382 = ORIENTED_EDGE ( 'NONE', *, *, #8711, .F. ) ;
#8383 = LINE ( 'NONE', #23738, #23338 ) ;
#8384 = CARTESIAN_POINT ( 'NONE',  ( 5.880360259849739535, 47.05949693022694191, 9.312491912828287255 ) ) ;
#8385 = CARTESIAN_POINT ( 'NONE',  ( 4.553261556744875094, 27.56395660609745235, -34.20186927699732138 ) ) ;
#8386 = CARTESIAN_POINT ( 'NONE',  ( 1.231276596079881935, -41.76121777166937221, -3.643825084341031584 ) ) ;
#8387 = ORIENTED_EDGE ( 'NONE', *, *, #17072, .T. ) ;
#8388 = EDGE_CURVE ( 'NONE', #42119, #23449, #36112, .T. ) ;
#8389 = CARTESIAN_POINT ( 'NONE',  ( -6.078075953587585900, 13.82887156709789345, 13.39990617235237913 ) ) ;
#8390 = VECTOR ( 'NONE', #52185, 1000.000000000000000 ) ;
#8391 = EDGE_CURVE ( 'NONE', #41414, #60958, #35541, .T. ) ;
#8392 = DIRECTION ( 'NONE',  ( 0.000000000000000000, 0.000000000000000000, 1.000000000000000000 ) ) ;
#8393 = ORIENTED_EDGE ( 'NONE', *, *, #10526, .T. ) ;
#8394 = CARTESIAN_POINT ( 'NONE',  ( -6.077587904424778920, -6.644566705894775716, -18.07334376049006508 ) ) ;
#8395 = ORIENTED_EDGE ( 'NONE', *, *, #5351, .F. ) ;
#8397 = EDGE_CURVE ( 'NONE', #27868, #516, #34480, .T. ) ;
#8396 = B_SPLINE_CURVE_WITH_KNOTS ( 'NONE', 3,
 ( #14774, #9747, #4707, #56733, #9434, #42986, #13858, #33575, #33886, #52963, #10067, #3798, #22939, #42066, #48892, #25701 ),
 .UNSPECIFIED., .F., .F.,
 ( 4, 3, 3, 3, 3, 4 ),
 ( 1.040890552917501732E-17, 0.0002732102107931892406, 0.0004098135523333787692, 0.0005464168938824976243, 0.0008195847345945413837, 0.001092771384553106132 ),
 .UNSPECIFIED. ) ;
#8398 = DIRECTION ( 'NONE',  ( -0.07439287786467650709, 0.5100024374914878811, 0.8569499480575001327 ) ) ;
#8399 = CARTESIAN_POINT ( 'NONE',  ( -2.569797478183783568, 10.02484965418641316, -10.65947181927829135 ) ) ;
#8400 = ORIENTED_EDGE ( 'NONE', *, *, #16729, .F. ) ;
#8401 = DIRECTION ( 'NONE',  ( 0.000000000000000000, 0.7071067811865500152, -0.7071067811865449082 ) ) ;
#8402 = EDGE_CURVE ( 'NONE', #27686, #55688, #23531, .T. ) ;
#8403 = CARTESIAN_POINT ( 'NONE',  ( 0.5809828226811544205, -28.72298383114515374, 38.32755012159135077 ) ) ;
#8404 = ORIENTED_EDGE ( 'NONE', *, *, #3043, .T. ) ;
#8405 = CARTESIAN_POINT ( 'NONE',  ( 0.000000000000000000, 0.6959691356230525150, 0.000000000000000000 ) ) ;
#8406 = CARTESIAN_POINT ( 'NONE',  ( 4.975610109902397937, 19.27143522741721426, -44.95621415792522413 ) ) ;
#8407 = VERTEX_POINT ( 'NONE', #5011 ) ;
#8408 = CARTESIAN_POINT ( 'NONE',  ( 5.880360259849739535, -26.61251048557276633, 39.91356965504101595 ) ) ;
#8409 = ORIENTED_EDGE ( 'NONE', *, *, #16969, .F. ) ;
#8410 = CARTESIAN_POINT ( 'NONE',  ( 0.5998501479064708430, 29.69975237324613460, -37.84527566984826308 ) ) ;
#8411 = ORIENTED_EDGE ( 'NONE', *, *, #14855, .T. ) ;
#8412 = ORIENTED_EDGE ( 'NONE', *, *, #16776, .F. ) ;
#8413 = CARTESIAN_POINT ( 'NONE',  ( 1.092182651088186018, 28.57178434915972787, -30.66617556115198440 ) ) ;
#8414 = DIRECTION ( 'NONE',  ( 0.000000000000000000, 0.000000000000000000, 1.000000000000000000 ) ) ;
#8415 = CARTESIAN_POINT ( 'NONE',  ( 0.5832366564991506852, 29.37287047358880443, 37.83193087518319686 ) ) ;
#8416 = CARTESIAN_POINT ( 'NONE',  ( 0.3676999524040323597, 42.11837424242189343, -13.11461530118710428 ) ) ;
#8417 = CARTESIAN_POINT ( 'NONE',  ( 4.549368137175248350, -42.84816078363928682, 2.596185425821780246 ) ) ;
#8418 = ORIENTED_EDGE ( 'NONE', *, *, #25437, .T. ) ;
#8419 = CARTESIAN_POINT ( 'NONE',  ( 0.9740398440564311811, 11.50548031350441924, 41.33716823241935856 ) ) ;
#8420 = CARTESIAN_POINT ( 'NONE',  ( 0.9790320750461911636, -17.71876186423139643, 37.97871259720171366 ) ) ;
#8421 = FACE_OUTER_BOUND ( 'NONE', #40563, .T. ) ;
#8422 = EDGE_LOOP ( 'NONE', ( #3738, #47487, #20761, #27364 ) ) ;
#8423 = VECTOR ( 'NONE', #28732, 1000.000000000000114 ) ;
#8424 = ORIENTED_EDGE ( 'NONE', *, *, #6313, .T. ) ;
#8425 = CARTESIAN_POINT ( 'NONE',  ( 0.9741495583595166652, 34.28086552274328369, -25.80610403442874556 ) ) ;
#8426 =( BOUNDED_SURFACE ( )  B_SPLINE_SURFACE ( 3, 1, ( 
 ( #9570, #53399 ),
 ( #37815, #43744 ),
 ( #38414, #29603 ),
 ( #44061, #33098 ) ),
 .UNSPECIFIED., .F., .F., .F. ) 
 B_SPLINE_SURFACE_WITH_KNOTS ( ( 4, 4 ),
 ( 2, 2 ),
 ( 0.000000000000000000, 1.000000000000000000 ),
 ( 0.000000000000000000, 1.000000000000000000 ),
 .UNSPECIFIED. ) 
 GEOMETRIC_REPRESENTATION_ITEM ( )  RATIONAL_B_SPLINE_SURFACE ( (
 ( 1.000000000000000000, 1.000000000000000000),
 ( 0.9952954269826590483, 0.8620686068821307169),
 ( 0.9952954269826590483, 0.8620686068821307169),
 ( 1.000000000000000000, 1.000000000000000000) ) ) 
 REPRESENTATION_ITEM ( '' )  SURFACE ( )  );
#8427 = CARTESIAN_POINT ( 'NONE',  ( 0.3676999524040323597, 21.13209774130321250, -38.72189339862975288 ) ) ;
#8428 = CARTESIAN_POINT ( 'NONE',  ( 3.238018933889920792, -12.56031985276158913, 4.652510888109346432 ) ) ;
#8429 = CARTESIAN_POINT ( 'NONE',  ( 0.1073791018717578927, -34.50606437925563341, 25.86618856530653687 ) ) ;
#8431 = VECTOR ( 'NONE', #46665, 1000.000000000000227 ) ;
#8430 = CARTESIAN_POINT ( 'NONE',  ( 3.894904216938897878, -33.85124917310555759, 28.03956600763502749 ) ) ;
#8432 = ORIENTED_EDGE ( 'NONE', *, *, #41048, .T. ) ;
#8433 = DIRECTION ( 'NONE',  ( -1.000000000000000000, 0.000000000000000000, 0.000000000000000000 ) ) ;
#8434 = CARTESIAN_POINT ( 'NONE',  ( 4.549368137175248350, -8.582197505784725067, 42.06008734272381133 ) ) ;
#8435 = CARTESIAN_POINT ( 'NONE',  ( 0.7948878604505673628, -26.19034530854877119, -41.53028364841004105 ) ) ;
#8436 = DIRECTION ( 'NONE',  ( 0.07500201931887538753, 0.9463514676414640503, -0.3143144870840953731 ) ) ;
#8437 = CARTESIAN_POINT ( 'NONE',  ( 1.154321485836934835, 22.16897757994474460, 36.74718014677574018 ) ) ;
#8438 =( LENGTH_UNIT ( ) NAMED_UNIT ( * ) SI_UNIT ( .MILLI., .METRE. ) );
#8439 = CARTESIAN_POINT ( 'NONE',  ( 0.2885700199627511120, 39.51953436244172480, -17.24062365614554437 ) ) ;
#8440 = EDGE_CURVE ( 'NONE', #57079, #2634, #6437, .T. ) ;
#8441 = ORIENTED_EDGE ( 'NONE', *, *, #18404, .T. ) ;
#8442 = CARTESIAN_POINT ( 'NONE',  ( 0.9756354156337442296, 21.56699035436992418, -37.09450626018190889 ) ) ;
#8443 = CARTESIAN_POINT ( 'NONE',  ( 5.959547316686252039, -16.28190225198627061, 12.49803383497722642 ) ) ;
#8444 = DIRECTION ( 'NONE',  ( 0.000000000000000000, 1.000000000000000000, 0.000000000000000000 ) ) ;
#8445 = CARTESIAN_POINT ( 'NONE',  ( 0.1095718737110178420, 21.78439022773156353, -37.21776476380635046 ) ) ;
#8446 = CARTESIAN_POINT ( 'NONE',  ( 0.7044674535452954967, -0.7321618212251337354, -49.10465010442948142 ) ) ;
#8447 = CARTESIAN_POINT ( 'NONE',  ( 0.5809828226811544205, 5.711058609466008740, -47.55412398569200150 ) ) ;
#8448 = CARTESIAN_POINT ( 'NONE',  ( 0.6016117650947689910, -49.10631026021277279, 0.3483487795599483627 ) ) ;
#8449 = LINE ( 'NONE', #41702, #40687 ) ;
#8450 = VECTOR ( 'NONE', #46629, 1000.000000000000000 ) ;
#8451 = DIRECTION ( 'NONE',  ( -0.1024043820194934645, -0.9239750460186150205, 0.3684880688409106209 ) ) ;
#8452 = ORIENTED_EDGE ( 'NONE', *, *, #44287, .T. ) ;
#8453 = CARTESIAN_POINT ( 'NONE',  ( 4.956653778116992370, 14.93973939759951541, -45.71126949320233734 ) ) ;
#8454 = CARTESIAN_POINT ( 'NONE',  ( 2.009741617377216460, 24.05948448209586132, -36.88692565230712006 ) ) ;
#8455 = CARTESIAN_POINT ( 'NONE',  ( 0.5997462898726536595, 33.39998138387845472, 35.99990102348730403 ) ) ;
#8456 = CARTESIAN_POINT ( 'NONE',  ( 0.5263152470540364281, 0.000000000000000000, -42.88844316795388778 ) ) ;
#8457 = VERTEX_POINT ( 'NONE', #42351 ) ;
#8458 = CARTESIAN_POINT ( 'NONE',  ( 4.956445790444005794, -33.12351118015950391, -33.47194433010255921 ) ) ;
#8459 = CARTESIAN_POINT ( 'NONE',  ( 0.9780106845699503282, -41.79289930907007999, -3.112043347603926868 ) ) ;
#8460 = B_SPLINE_CURVE_WITH_KNOTS ( 'NONE', 3,
 ( #29009, #19311, #5176, #482 ),
 .UNSPECIFIED., .F., .F.,
 ( 4, 4 ),
 ( 1.084202172485504241E-18, 0.004041751736740997747 ),
 .UNSPECIFIED. ) ;
#8461 = ADVANCED_FACE ( 'NONE', ( #8808 ), #9070, .F. ) ;
#8462 = FILL_AREA_STYLE ('',( #55772 ) ) ;
#8463 = ORIENTED_EDGE ( 'NONE', *, *, #13128, .F. ) ;
#8464 = FACE_OUTER_BOUND ( 'NONE', #52154, .T. ) ;
#8465 = CARTESIAN_POINT ( 'NONE',  ( 0.8760168074887076939, -47.80016357497245849, -5.394043284319333331 ) ) ;
#8466 = VECTOR ( 'NONE', #50802, 1000.000000000000000 ) ;
#8467 = EDGE_CURVE ( 'NONE', #61383, #48962, #9326, .T. ) ;
#8468 = ORIENTED_EDGE ( 'NONE', *, *, #35586, .T. ) ;
#8469 = CARTESIAN_POINT ( 'NONE',  ( 0.8744876279028306332, 11.79038800009151089, 47.65854384249261244 ) ) ;
#8470 = CIRCLE ( 'NONE', #32520, 48.91267123290010943 ) ;
#8471 = ORIENTED_EDGE ( 'NONE', *, *, #1913, .F. ) ;
#8472 = ADVANCED_FACE ( 'NONE', ( #28840 ), #51498, .F. ) ;
#8473 = VERTEX_POINT ( 'NONE', #24139 ) ;
#8474 = CARTESIAN_POINT ( 'NONE',  ( 0.8753041380234471980, 23.49739456791673575, -43.11624724384784457 ) ) ;
#8475 = ORIENTED_EDGE ( 'NONE', *, *, #30680, .T. ) ;
#8476 = CARTESIAN_POINT ( 'NONE',  ( 5.838029081930955932, 30.51096402024728249, -36.05753919373999139 ) ) ;
#8477 = AXIS2_PLACEMENT_3D ( 'NONE', #20224, #48713, #15831 ) ;
#8478 = ORIENTED_EDGE ( 'NONE', *, *, #20625, .F. ) ;
#8479 = LINE ( 'NONE', #55790, #8753 ) ;
#8480 = CARTESIAN_POINT ( 'NONE',  ( -4.908599999999998964, 9.539392014169456147, -3.000000000000000000 ) ) ;
#8481 = CARTESIAN_POINT ( 'NONE',  ( 0.9756950546413933889, 16.50968749804439994, 39.60512406639350758 ) ) ;
#8482 = ORIENTED_EDGE ( 'NONE', *, *, #43760, .F. ) ;
#8483 = CARTESIAN_POINT ( 'NONE',  ( 5.901463166500146684, -19.39418503693773133, 5.327612701169004872 ) ) ;
#8484 = ADVANCED_FACE ( 'NONE', ( #42050 ), #415, .T. ) ;
#8485 = FACE_OUTER_BOUND ( 'NONE', #28209, .T. ) ;
#8486 = CARTESIAN_POINT ( 'NONE',  ( 4.549368137175248350, -28.14399996863522446, 32.41327393324091588 ) ) ;
#8487 = FACE_OUTER_BOUND ( 'NONE', #10114, .T. ) ;
#8488 = VERTEX_POINT ( 'NONE', #19456 ) ;
#8489 = CARTESIAN_POINT ( 'NONE',  ( 5.331200000000000827, 1.887314203987178256E-15, -15.38217999999999996 ) ) ;
#8490 = EDGE_CURVE ( 'NONE', #20568, #23600, #15343, .T. ) ;
#8491 = CARTESIAN_POINT ( 'NONE',  ( 0.1129192098497455998, -31.35755906439593943, -31.04279751098591689 ) ) ;
#8492 = VERTEX_POINT ( 'NONE', #61405 ) ;
#8493 = DIRECTION ( 'NONE',  ( -1.000000000000000000, -0.000000000000000000, -0.000000000000000000 ) ) ;
#8494 =( BOUNDED_SURFACE ( )  B_SPLINE_SURFACE ( 3, 1, ( 
 ( #24240, #52426 ),
 ( #43065, #19871 ),
 ( #57418, #48060 ),
 ( #42451, #43689 ) ),
 .UNSPECIFIED., .F., .F., .F. ) 
 B_SPLINE_SURFACE_WITH_KNOTS ( ( 4, 4 ),
 ( 2, 2 ),
 ( 0.000000000000000000, 1.000000000000000000 ),
 ( 0.000000000000000000, 1.000000000000000000 ),
 .UNSPECIFIED. ) 
 GEOMETRIC_REPRESENTATION_ITEM ( )  RATIONAL_B_SPLINE_SURFACE ( (
 ( 1.000000000000000000, 1.000000000000000000),
 ( 0.7282232189291694135, 0.9929344683865672927),
 ( 0.7282232189291694135, 0.9929344683865672927),
 ( 1.000000000000000000, 1.000000000000000000) ) ) 
 REPRESENTATION_ITEM ( '' )  SURFACE ( )  );
#8495 = ORIENTED_EDGE ( 'NONE', *, *, #55429, .F. ) ;
#8496 = DIRECTION ( 'NONE',  ( 0.000000000000000000, 1.000000000000000000, 0.000000000000000000 ) ) ;
#8497 = CONICAL_SURFACE ( 'NONE', #43550, 42.08604991992415023, 1.569615340895231137 ) ;
#8498 = B_SPLINE_CURVE_WITH_KNOTS ( 'NONE', 3,
 ( #18742, #41947, #42258, #37243, #23740, #42868, #23128, #61316, #37871, #56311, #13425, #56622, #13742, #32851, #9018, #28125, #47244, #848, #29354, #9632, #25277, #53155, #19357, #53754, #14664, #43486, #48461, #10570, #57529, #24662 ),
 .UNSPECIFIED., .F., .F.,
 ( 4, 2, 2, 2, 2, 2, 2, 2, 2, 2, 2, 2, 2, 2, 4 ),
 ( 0.006594498439790126912, 0.007418584928504671355, 0.007830628172861942710, 0.008242671417219215799, 0.008654714661576487153, 0.009066757905933758507, 0.009478801150291031596, 0.009890844394648302951, 0.01030288763900557431, 0.01071493088336284566, 0.01153901737207739184, 0.01195106061643467013, 0.01236310386079194669, 0.01277514710514922498, 0.01318719034950650328 ),
 .UNSPECIFIED. ) ;
#8499 = CARTESIAN_POINT ( 'NONE',  ( 0.3622758884714730732, 11.95365414648439462, 41.42293301073630118 ) ) ;
#8500 = VERTEX_POINT ( 'NONE', #51714 ) ;
#8501 = CARTESIAN_POINT ( 'NONE',  ( 0.5997462898726536595, -47.36625756029525292, -12.96106765957508244 ) ) ;
#8502 = CARTESIAN_POINT ( 'NONE',  ( 0.6028777368367060907, 28.02372537435406130, 40.32630215447304778 ) ) ;
#8503 = CARTESIAN_POINT ( 'NONE',  ( 4.975610109902397937, 0.000000000000000000, 0.000000000000000000 ) ) ;
#8504 = VERTEX_POINT ( 'NONE', #27924 ) ;
#8505 = DIRECTION ( 'NONE',  ( -0.07439287786467650709, -0.1432402660415156848, -0.9868880006907405633 ) ) ;
#8506 = CARTESIAN_POINT ( 'NONE',  ( 5.895881250540457863, -20.11287301435476849, 0.004551564636878664520 ) ) ;
#8507 = CARTESIAN_POINT ( 'NONE',  ( 0.5997462898726536595, -25.90236585764290922, 41.72072714036901431 ) ) ;
#8508 = CARTESIAN_POINT ( 'NONE',  ( 0.1129192098497447394, -18.30288010335054949, -40.14917642626718930 ) ) ;
#8509 = B_SPLINE_CURVE_WITH_KNOTS ( 'NONE', 3,
 ( #57113, #33353, #52421, #28936 ),
 .UNSPECIFIED., .F., .F.,
 ( 4, 4 ),
 ( 2.168404344971008868E-19, 0.004444878191957699932 ),
 .UNSPECIFIED. ) ;
#8510 = FACE_OUTER_BOUND ( 'NONE', #2404, .T. ) ;
#8511 = CARTESIAN_POINT ( 'NONE',  ( 3.238018933889920792, -12.56031985276152341, -4.652510888109532061 ) ) ;
#8512 = EDGE_CURVE ( 'NONE', #3834, #23453, #47048, .T. ) ;
#8513 = CARTESIAN_POINT ( 'NONE',  ( 0.5997462898726536595, 37.72933316222010802, -31.43324751403371664 ) ) ;
#8514 = AXIS2_PLACEMENT_3D ( 'NONE', #26914, #27834, #46963 ) ;
#8515 = CARTESIAN_POINT ( 'NONE',  ( -90.00000000000000000, 0.000000000000000000, 0.000000000000000000 ) ) ;
#8516 = CARTESIAN_POINT ( 'NONE',  ( -6.010958268070873523, 2.473955915502211944, 18.68034667844849750 ) ) ;
#8517 = VECTOR ( 'NONE', #44495, 1000.000000000000114 ) ;
#8518 = CARTESIAN_POINT ( 'NONE',  ( 0.9780303403264768436, -12.10685390290327490, 40.12186064938713770 ) ) ;
#8519 = FACE_OUTER_BOUND ( 'NONE', #28588, .T. ) ;
#8520 = ADVANCED_FACE ( 'NONE', ( #14151 ), #45489, .T. ) ;
#8521 = LINE ( 'NONE', #53284, #31 ) ;
#8522 = VECTOR ( 'NONE', #50729, 1000.000000000000000 ) ;
#8523 = DIRECTION ( 'NONE',  ( 1.000000000000000000, 1.836909530733573776E-16, 0.000000000000000000 ) ) ;
#8524 = CARTESIAN_POINT ( 'NONE',  ( 0.5997462898726536595, 27.66511329191646951, -40.57330571557777432 ) ) ;
#8525 = AXIS2_PLACEMENT_3D ( 'NONE', #28981, #32771, #52465 ) ;
#8526 = CARTESIAN_POINT ( 'NONE',  ( 0.9730545539215883499, 36.90443313492330901, 21.89037132892449478 ) ) ;
#8527 = DIRECTION ( 'NONE',  ( 0.000000000000000000, 0.000000000000000000, -1.000000000000000000 ) ) ;
#8528 = CARTESIAN_POINT ( 'NONE',  ( 0.9745511491811765792, -36.98831798234360235, -21.74846188963815052 ) ) ;
#8529 = CARTESIAN_POINT ( 'NONE',  ( 0.5837800005270548098, 45.22974258645800916, -12.38973947282719301 ) ) ;
#8530 = CARTESIAN_POINT ( 'NONE',  ( 0.6023143664670691511, 46.53533348214991605, -12.19804739160213281 ) ) ;
#8532 = ORIENTED_EDGE ( 'NONE', *, *, #2546, .T. ) ;
#8531 = CARTESIAN_POINT ( 'NONE',  ( -6.015611763856276717, -9.416239407363189429, -16.32183393015606754 ) ) ;
#8533 = EDGE_LOOP ( 'NONE', ( #56396, #12459 ) ) ;
#8534 = CARTESIAN_POINT ( 'NONE',  ( 7.000000000000005329, 2.649999999999721467, 80.00000000000002842 ) ) ;
#8535 = CARTESIAN_POINT ( 'NONE',  ( -6.077587904424778920, -17.34643006009198274, 8.360465630828690209 ) ) ;
#8536 = LINE ( 'NONE', #51761, #1678 ) ;
#8537 = VERTEX_POINT ( 'NONE', #44519 ) ;
#8538 = ORIENTED_EDGE ( 'NONE', *, *, #50205, .T. ) ;
#8539 = CARTESIAN_POINT ( 'NONE',  ( 2.533389852662419894, -30.49798923258317629, 31.73835510077449484 ) ) ;
#8540 = CARTESIAN_POINT ( 'NONE',  ( -6.078726893082806448, 15.42998809551227879, 11.51996131248145439 ) ) ;
#8541 = UNCERTAINTY_MEASURE_WITH_UNIT (LENGTH_MEASURE( 1.000000000000000082E-05 ), #57006, 'distance_accuracy_value', 'NONE');
#8542 = B_SPLINE_CURVE_WITH_KNOTS ( 'NONE', 3,
 ( #30436, #21056, #40196, #16054, #25433, #10428, #15750, #20437, #29517, #34857, #53924, #38955, #49869, #49547, #48625, #59247, #30130, #54228, #6929 ),
 .UNSPECIFIED., .F., .F.,
 ( 4, 3, 3, 3, 3, 3, 4 ),
 ( 6.938893903907228378E-18, 0.0002732106629380631367, 0.0004098138914053715831, 0.0005464171197651477739, 0.0006830203481512608617, 0.0008196235766963706803, 0.001011968216111143980 ),
 .UNSPECIFIED. ) ;
#8543 = VERTEX_POINT ( 'NONE', #15996 ) ;
#8544 = ORIENTED_EDGE ( 'NONE', *, *, #5580, .T. ) ;
#8545 = CARTESIAN_POINT ( 'NONE',  ( 0.9752570700956795235, -10.88256294660683032, -41.50550328400880318 ) ) ;
#8546 = EDGE_CURVE ( 'NONE', #2381, #23031, #37776, .T. ) ;
#8547 = DIRECTION ( 'NONE',  ( 0.000000000000000000, 0.000000000000000000, -1.000000000000000000 ) ) ;
#8548 = CARTESIAN_POINT ( 'NONE',  ( 4.549368137175248350, -8.166781970326043805, 42.14271863032818999 ) ) ;
#8549 = ORIENTED_EDGE ( 'NONE', *, *, #57307, .F. ) ;
#8550 = EDGE_CURVE ( 'NONE', #41582, #27020, #19127, .T. ) ;
#8551 = VERTEX_POINT ( 'NONE', #10671 ) ;
#8552 = CARTESIAN_POINT ( 'NONE',  ( 0.6039202388192953519, 44.16863261170606592, -21.46382086351650287 ) ) ;
#8553 = ORIENTED_EDGE ( 'NONE', *, *, #8769, .T. ) ;
#8554 = CARTESIAN_POINT ( 'NONE',  ( 1.827119703190779321, -33.38937793923705755, 27.17434071502546189 ) ) ;
#8555 = CARTESIAN_POINT ( 'NONE',  ( -2.569797478183783568, -14.62602397812941035, 0.4487456364278328835 ) ) ;
#8556 = ORIENTED_EDGE ( 'NONE', *, *, #39328, .F. ) ;
#8557 = AXIS2_PLACEMENT_3D ( 'NONE', #27994, #52402, #47723 ) ;
#8558 = CARTESIAN_POINT ( 'NONE',  ( 0.1100247026804066219, 0.1696715072117343237, -43.12411436000287779 ) ) ;
#8559 = VERTEX_POINT ( 'NONE', #34178 ) ;
#8560 = ORIENTED_EDGE ( 'NONE', *, *, #50552, .F. ) ;
#8561 = CARTESIAN_POINT ( 'NONE',  ( 5.959828726073459926, 17.77796293532158955, 10.25888482581865802 ) ) ;
#8562 = CONICAL_SURFACE ( 'NONE', #59585, 43.08621763946400307, 1.568696531533066763 ) ;
#8563 = VERTEX_POINT ( 'NONE', #6234 ) ;
#8564 = CARTESIAN_POINT ( 'NONE',  ( 0.6021447746440204973, 46.68736993825091730, 15.22598526655637485 ) ) ;
#8565 = CARTESIAN_POINT ( 'NONE',  ( 4.549368137175248350, 13.99871866169365653, -40.58005590356676606 ) ) ;
#8566 = DIRECTION ( 'NONE',  ( 0.000000000000000000, 0.000000000000000000, 1.000000000000000000 ) ) ;
#8567 = CARTESIAN_POINT ( 'NONE',  ( 4.956445790443988031, 0.000000000000000000, 0.000000000000000000 ) ) ;
#8568 = ADVANCED_FACE ( 'NONE', ( #5930 ), #12490, .F. ) ;
#8569 = AXIS2_PLACEMENT_3D ( 'NONE', #936, #23828, #33241 ) ;
#8570 = VERTEX_POINT ( 'NONE', #25687 ) ;
#8571 = CARTESIAN_POINT ( 'NONE',  ( 0.6041374136657475802, -24.20487816031549855, 41.57494627055102399 ) ) ;
#8572 = CARTESIAN_POINT ( 'NONE',  ( 0.2224561200757618484, -10.42482236669274620, -41.84032767736798775 ) ) ;
#8573 = CARTESIAN_POINT ( 'NONE',  ( 0.1073791018717578927, 40.02496097243057704, -16.05399293000775529 ) ) ;
#8574 = ORIENTED_EDGE ( 'NONE', *, *, #5688, .F. ) ;
#8575 = CARTESIAN_POINT ( 'NONE',  ( 0.1101816497532062400, 42.73758747687830351, -5.763501205266673644 ) ) ;
#8576 = CARTESIAN_POINT ( 'NONE',  ( 4.322998006666179727, -35.39923696758989990, -32.40067585697786967 ) ) ;
#8577 = LINE ( 'NONE', #31792, #50645 ) ;
#8578 = CARTESIAN_POINT ( 'NONE',  ( 0.5998501479064699549, 38.48283596221989455, 28.86886762351138103 ) ) ;
#8579 =( BOUNDED_SURFACE ( )  B_SPLINE_SURFACE ( 3, 1, ( 
 ( #36100, #25742 ),
 ( #30429, #26056 ),
 ( #12287, #55164 ),
 ( #6921, #2545 ) ),
 .UNSPECIFIED., .F., .F., .F. ) 
 B_SPLINE_SURFACE_WITH_KNOTS ( ( 4, 4 ),
 ( 2, 2 ),
 ( 0.000000000000000000, 1.000000000000000000 ),
 ( 0.000000000000000000, 1.000000000000000000 ),
 .UNSPECIFIED. ) 
 GEOMETRIC_REPRESENTATION_ITEM ( )  RATIONAL_B_SPLINE_SURFACE ( (
 ( 1.000000000000000000, 1.000000000000000000),
 ( 0.9953390228620291325, 0.8624445117760984880),
 ( 0.9953390228620291325, 0.8624445117760984880),
 ( 1.000000000000000000, 1.000000000000000000) ) ) 
 REPRESENTATION_ITEM ( '' )  SURFACE ( )  );
#8580 = ORIENTED_EDGE ( 'NONE', *, *, #12902, .T. ) ;
#8581 = CARTESIAN_POINT ( 'NONE',  ( 0.8551540677456715978, -43.91216198251525782, -19.17641535420899856 ) ) ;
#8582 = FACE_OUTER_BOUND ( 'NONE', #13735, .T. ) ;
#8583 = CARTESIAN_POINT ( 'NONE',  ( 0.7762777257811898091, -0.8897018348889329520, 47.89627391089018715 ) ) ;
#8584 = DIRECTION ( 'NONE',  ( 0.000000000000000000, -1.000000000000000000, 0.000000000000000000 ) ) ;
#8585 = CARTESIAN_POINT ( 'NONE',  ( 0.9757787079277444597, -42.54650880470565966, 5.561523338227001290 ) ) ;
#8586 = B_SPLINE_CURVE_WITH_KNOTS ( 'NONE', 3,
 ( #47657, #4705, #42362, #58889, #48889, #43920 ),
 .UNSPECIFIED., .F., .F.,
 ( 4, 2, 4 ),
 ( 1.506204625983992411E-16, 0.0002445252820015214666, 0.0004890505640028923375 ),
 .UNSPECIFIED. ) ;
#8587 = CARTESIAN_POINT ( 'NONE',  ( 0.5804410086790514622, 23.01644811389206424, 40.86273324284501740 ) ) ;
#8588 = CARTESIAN_POINT ( 'NONE',  ( 0.9741495583595178864, 42.90659993968954922, 0.3955098476633079896 ) ) ;
#8589 = CARTESIAN_POINT ( 'NONE',  ( -6.078726893082806448, -8.903615017412294108, -17.07394743140643456 ) ) ;
#8590 = CARTESIAN_POINT ( 'NONE',  ( 2.281448460670569833, -37.24544744441600130, 30.23587867650742211 ) ) ;
#8591 = CARTESIAN_POINT ( 'NONE',  ( 0.9789889208857687208, -1.496490579766653672, -41.88192228142159479 ) ) ;
#8592 = CARTESIAN_POINT ( 'NONE',  ( 5.959547316686252039, 10.25972575517505270, 17.77749189599220969 ) ) ;
#8593 = EDGE_LOOP ( 'NONE', ( #22108, #12281, #47397, #27989 ) ) ;
#8594 = EDGE_CURVE ( 'NONE', #34535, #25604, #45976, .T. ) ;
#8595 = CARTESIAN_POINT ( 'NONE',  ( -6.015611763856276717, -9.427003116184058840, -16.31561949997086103 ) ) ;
#8596 = CARTESIAN_POINT ( 'NONE',  ( 4.960156602257181468, 41.85906677498984862, -20.07163247083100188 ) ) ;
#8597 = DIRECTION ( 'NONE',  ( 1.000000000000000000, 1.836970198721029194E-16, -6.779273404243071298E-32 ) ) ;
#8598 = CARTESIAN_POINT ( 'NONE',  ( 2.533389852662419894, -24.15616722665976113, -36.79578938752730721 ) ) ;
#8599 = FACE_OUTER_BOUND ( 'NONE', #39049, .T. ) ;
#8600 = EDGE_CURVE ( 'NONE', #7019, #36997, #52703, .T. ) ;
#8601 = CONTEXT_DEPENDENT_SHAPE_REPRESENTATION ( #15255, #31279 ) ;
#8602 = CARTESIAN_POINT ( 'NONE',  ( 0.5835226383429293895, -25.08023547371319140, 39.62605535665972667 ) ) ;
#8603 = DIRECTION ( 'NONE',  ( -1.000000000000000000, -0.000000000000000000, 1.925929944387235853E-32 ) ) ;
#8604 = EDGE_CURVE ( 'NONE', #28634, #6825, #30687, .T. ) ;
#8605 = CARTESIAN_POINT ( 'NONE',  ( 4.962356264823608143, -42.08379584346670299, -0.4355746408611892995 ) ) ;
#8607 = ORIENTED_EDGE ( 'NONE', *, *, #34255, .F. ) ;
#8606 = CARTESIAN_POINT ( 'NONE',  ( 1.088908134280554441, -36.76788378223844944, 22.12904883058541472 ) ) ;
#8608 = ORIENTED_EDGE ( 'NONE', *, *, #46410, .T. ) ;
#8609 = AXIS2_PLACEMENT_3D ( 'NONE', #29297, #48408, #14919 ) ;
#8610 = CARTESIAN_POINT ( 'NONE',  ( 5.894904586330512508, 10.82344038793328345, 16.95236119926948248 ) ) ;
#8611 = CARTESIAN_POINT ( 'NONE',  ( 0.1073791018717578927, 39.65380858626191696, 16.95003405440326816 ) ) ;
#8612 = CIRCLE ( 'NONE', #20660, 42.08604991992415023 ) ;
#8613 = DIRECTION ( 'NONE',  ( 1.000000000000000000, 0.000000000000000000, 0.000000000000000000 ) ) ;
#8614 = VERTEX_POINT ( 'NONE', #7171 ) ;
#8615 = CARTESIAN_POINT ( 'NONE',  ( 0.6016118706126977189, 11.26678578505916661, -47.79760028346109380 ) ) ;
#8616 = CARTESIAN_POINT ( 'NONE',  ( 0.5806925824938499181, -46.06186276235273169, 8.804950948514585818 ) ) ;
#8617 = CARTESIAN_POINT ( 'NONE',  ( -2.601141883200665639, -14.91960803315171269, -0.4480218817239748907 ) ) ;
#8618 = B_SPLINE_CURVE_WITH_KNOTS ( 'NONE', 3,
 ( #55259, #21766, #31159, #2643, #45289, #7329 ),
 .UNSPECIFIED., .F., .F.,
 ( 4, 2, 4 ),
 ( 8.559238840292260229E-17, 0.0002293366620881447137, 0.0004586733241762038296 ),
 .UNSPECIFIED. ) ;
#8619 = VERTEX_POINT ( 'NONE', #8119 ) ;
#8620 = EDGE_LOOP ( 'NONE', ( #6426, #42259, #57995, #60415 ) ) ;
#8621 = B_SPLINE_CURVE_WITH_KNOTS ( 'NONE', 3,
 ( #34457, #10027, #15968, #53831, #29426, #30046 ),
 .UNSPECIFIED., .F., .F.,
 ( 4, 2, 4 ),
 ( 8.672106141451628927E-17, 0.0002293366620881453371, 0.0004586733241762039922 ),
 .UNSPECIFIED. ) ;
#8622 = LINE ( 'NONE', #13053, #40351 ) ;
#8623 = EDGE_CURVE ( 'NONE', #48578, #14125, #54796, .T. ) ;
#8624 = AXIS2_PLACEMENT_3D ( 'NONE', #54825, #11961, #35134 ) ;
#8625 = CARTESIAN_POINT ( 'NONE',  ( 2.533389852662419894, 37.72904932230753161, 22.67089254900441020 ) ) ;
#8626 = CARTESIAN_POINT ( 'NONE',  ( 0.6009453534118440743, 41.44251633523857947, 24.43073772334932769 ) ) ;
#8627 = EDGE_CURVE ( 'NONE', #50100, #6088, #60470, .T. ) ;
#8628 = CARTESIAN_POINT ( 'NONE',  ( 0.9268187852002115479, -44.07687711066218128, 0.9915831181550756046 ) ) ;
#8629 = CARTESIAN_POINT ( 'NONE',  ( 0.6008123274975391004, 48.97686038498178362, 3.580739866069544419 ) ) ;
#8630 = EDGE_CURVE ( 'NONE', #41667, #24079, #4876, .T. ) ;
#8631 = B_SPLINE_CURVE_WITH_KNOTS ( 'NONE', 3,
 ( #34444, #44178, #30336, #6501, #24724, #57905 ),
 .UNSPECIFIED., .F., .F.,
 ( 4, 2, 4 ),
 ( 7.818293051731876896E-19, 0.0002293801035737093178, 0.0004587602071474178225 ),
 .UNSPECIFIED. ) ;
#8632 = CARTESIAN_POINT ( 'NONE',  ( 4.956653778116975495, 26.26162724282373517, 40.28700667097690769 ) ) ;
#8633 = ORIENTED_EDGE ( 'NONE', *, *, #18367, .F. ) ;
#8634 = CARTESIAN_POINT ( 'NONE',  ( 0.5980271706414734822, 10.24496086146951157, -48.03217692119128657 ) ) ;
#8635 = CARTESIAN_POINT ( 'NONE',  ( 0.8551540677456715978, -47.37911285756614888, -7.157691013574858374 ) ) ;
#8636 = ORIENTED_EDGE ( 'NONE', *, *, #22285, .T. ) ;
#8637 = CARTESIAN_POINT ( 'NONE',  ( 0.6028618097248863439, -47.71844004092984903, -6.106174977918878533 ) ) ;
#8638 = CARTESIAN_POINT ( 'NONE',  ( 0.8744876279028263033, -47.25615711918255357, -13.31186180466976587 ) ) ;
#8639 = CARTESIAN_POINT ( 'NONE',  ( 4.060580049360325461, 38.53742723504589662, -21.12662766422393190 ) ) ;
#8640 = CARTESIAN_POINT ( 'NONE',  ( 0.2940133293162998651, -34.86814990962280802, -27.02688793513072696 ) ) ;
#8641 = EDGE_CURVE ( 'NONE', #7311, #16730, #48941, .T. ) ;
#8642 = EDGE_LOOP ( 'NONE', ( #23920, #43738 ) ) ;
#8643 = ORIENTED_EDGE ( 'NONE', *, *, #60921, .F. ) ;
#8644 = CARTESIAN_POINT ( 'NONE',  ( 0.1156867017252034141, -44.12399792677806687, -0.1249569240610424042 ) ) ;
#8645 = CARTESIAN_POINT ( 'NONE',  ( -6.078457390727109555, 18.62736532255352984, 4.880140589945982654 ) ) ;
#8646 = CARTESIAN_POINT ( 'NONE',  ( 0.6000166863083106206, 16.46965316277444913, 46.26633772416363399 ) ) ;
#8647 = ORIENTED_EDGE ( 'NONE', *, *, #30029, .T. ) ;
#8648 = PLANE ( 'NONE',  #34532 ) ;
#8649 = AXIS2_PLACEMENT_3D ( 'NONE', #10230, #54038, #59052 ) ;
#8650 = VERTEX_POINT ( 'NONE', #16608 ) ;
#8651 = CARTESIAN_POINT ( 'NONE',  ( 0.9268187852002115479, 43.45361200865025353, 7.452377896370549593 ) ) ;
#8652 = CARTESIAN_POINT ( 'NONE',  ( 4.960156602257179692, 38.31207700265985494, -26.21519897043388525 ) ) ;
#8653 = AXIS2_PLACEMENT_3D ( 'NONE', #6284, #44878, #6590 ) ;
#8654 = CARTESIAN_POINT ( 'NONE',  ( 0.1310142868023688456, 42.66681113736508024, 6.259743112235677920 ) ) ;
#8655 = EDGE_LOOP ( 'NONE', ( #44041, #48943, #43033, #36071 ) ) ;
#8656 = CARTESIAN_POINT ( 'NONE',  ( 0.1129192098497455998, 25.64022107388826655, -35.91003830501005467 ) ) ;
#8657 = AXIS2_PLACEMENT_3D ( 'NONE', #25610, #22154, #21846 ) ;
#8658 = CARTESIAN_POINT ( 'NONE',  ( 0.1155031312995260795, -27.64250437147500250, 34.39234776232634516 ) ) ;
#8659 = CARTESIAN_POINT ( 'NONE',  ( 0.9762797500689124330, -41.84568905980455611, -2.294143041716810050 ) ) ;
#8660 = B_SPLINE_CURVE_WITH_KNOTS ( 'NONE', 3,
 ( #56121, #42671, #61734, #47070 ),
 .UNSPECIFIED., .F., .F.,
 ( 4, 4 ),
 ( 0.000000000000000000, 0.004446090762761357312 ),
 .UNSPECIFIED. ) ;
#8661 = ORIENTED_EDGE ( 'NONE', *, *, #47753, .T. ) ;
#8662 = LINE ( 'NONE', #51889, #426 ) ;
#8663 = PLANE ( 'NONE',  #21844 ) ;
#8664 = CARTESIAN_POINT ( 'NONE',  ( 0.1073791018717578927, 26.63563652260167203, -33.91564619577780348 ) ) ;
#8665 = CARTESIAN_POINT ( 'NONE',  ( 0.5806925824938499181, 36.46274162637902094, 29.49052111156212774 ) ) ;
#8666 = ORIENTED_EDGE ( 'NONE', *, *, #34595, .F. ) ;
#8667 = VECTOR ( 'NONE', #6506, 999.9999999999998863 ) ;
#8668 = CARTESIAN_POINT ( 'NONE',  ( 4.956445790443996025, 14.46717203539371610, 44.81337951368942640 ) ) ;
#8669 = EDGE_CURVE ( 'NONE', #22852, #50100, #22234, .T. ) ;
#8670 = CARTESIAN_POINT ( 'NONE',  ( 0.5997462898726536595, -48.76843890605300658, -5.761162800241320880 ) ) ;
#8671 = ORIENTED_EDGE ( 'NONE', *, *, #32346, .F. ) ;
#8672 = EDGE_CURVE ( 'NONE', #31407, #817, #45315, .T. ) ;
#8673 = FACE_OUTER_BOUND ( 'NONE', #43508, .T. ) ;
#8674 = CARTESIAN_POINT ( 'NONE',  ( 4.960156602257181468, 20.07163247083145663, 41.85906677498964257 ) ) ;
#8675 = CARTESIAN_POINT ( 'NONE',  ( 2.528100132419516477, 32.18157850662347386, -26.95551489870128492 ) ) ;
#8676 = B_SPLINE_CURVE_WITH_KNOTS ( 'NONE', 3,
 ( #6785, #25929, #19695, #24695, #43836, #15312 ),
 .UNSPECIFIED., .F., .F.,
 ( 4, 2, 4 ),
 ( 1.710636569715182240E-17, 0.0002293755540694310746, 0.0004587511081388450729 ),
 .UNSPECIFIED. ) ;
#8677 = CARTESIAN_POINT ( 'NONE',  ( -1.129531546211723025, 6.886005254585696675E-16, 5.612499999999999822 ) ) ;
#8678 = CARTESIAN_POINT ( 'NONE',  ( 0.2940135542859012019, -40.58327627078308097, 17.29850386075961666 ) ) ;
#8679 = VECTOR ( 'NONE', #46616, 1000.000000000000114 ) ;
#8680 = CARTESIAN_POINT ( 'NONE',  ( 52.25008115675156972, 15.37124894287441279, 1.997531998838311784 ) ) ;
#8681 = EDGE_CURVE ( 'NONE', #15676, #44940, #19909, .T. ) ;
#8682 = CARTESIAN_POINT ( 'NONE',  ( 0.6017666602106490625, 47.74032907933390391, 5.933006478840855635 ) ) ;
#8683 =( BOUNDED_SURFACE ( )  B_SPLINE_SURFACE ( 3, 1, ( 
 ( #56282, #3959 ),
 ( #32817, #28400 ),
 ( #33744, #14635 ),
 ( #41916, #46923 ) ),
 .UNSPECIFIED., .F., .F., .F. ) 
 B_SPLINE_SURFACE_WITH_KNOTS ( ( 4, 4 ),
 ( 2, 2 ),
 ( 0.000000000000000000, 1.000000000000000000 ),
 ( 0.000000000000000000, 1.000000000000000000 ),
 .UNSPECIFIED. ) 
 GEOMETRIC_REPRESENTATION_ITEM ( )  RATIONAL_B_SPLINE_SURFACE ( (
 ( 1.000000000000000000, 1.000000000000000000),
 ( 0.7223157951917480446, 0.9931996967497186413),
 ( 0.7223157951917480446, 0.9931996967497186413),
 ( 1.000000000000000000, 1.000000000000000000) ) ) 
 REPRESENTATION_ITEM ( '' )  SURFACE ( )  );
#8684 = DIRECTION ( 'NONE',  ( 0.000000000000000000, 0.000000000000000000, -1.000000000000000000 ) ) ;
#8685 = CARTESIAN_POINT ( 'NONE',  ( 4.958415959904820092, 34.02476434053209431, -30.09184881980321435 ) ) ;
#8686 = EDGE_CURVE ( 'NONE', #57080, #6050, #60917, .T. ) ;
#8687 = EDGE_CURVE ( 'NONE', #23902, #42831, #24316, .T. ) ;
#8688 = CARTESIAN_POINT ( 'NONE',  ( 0.1103744047535531458, -5.667281528142711799, 42.75042227379817916 ) ) ;
#8689 = ORIENTED_EDGE ( 'NONE', *, *, #44321, .T. ) ;
#8690 = LINE ( 'NONE', #24345, #39546 ) ;
#8691 = DIRECTION ( 'NONE',  ( 1.000000000000000000, 1.836909530733573776E-16, -1.925929944387235853E-32 ) ) ;
#8692 = CARTESIAN_POINT ( 'NONE',  ( 0.5804410086790514622, 46.55025363952971418, -5.709092568074892071 ) ) ;
#8693 = CARTESIAN_POINT ( 'NONE',  ( 4.967162193818130511, -8.839793687085512275, 42.16965968614191240 ) ) ;
#8694 = CARTESIAN_POINT ( 'NONE',  ( 0.5834584762367743815, 46.45295943560137175, 6.431061241161131647 ) ) ;
#8695 = CARTESIAN_POINT ( 'NONE',  ( 0.6031357023905875581, -38.19275261685294964, 29.25135304925216673 ) ) ;
#8696 =( BOUNDED_SURFACE ( )  B_SPLINE_SURFACE ( 3, 1, ( 
 ( #11312, #44546 ),
 ( #5952, #54822 ),
 ( #59212, #39224 ),
 ( #34507, #30399 ) ),
 .UNSPECIFIED., .F., .F., .F. ) 
 B_SPLINE_SURFACE_WITH_KNOTS ( ( 4, 4 ),
 ( 2, 2 ),
 ( 0.000000000000000000, 1.000000000000000000 ),
 ( 0.000000000000000000, 1.000000000000000000 ),
 .UNSPECIFIED. ) 
 GEOMETRIC_REPRESENTATION_ITEM ( )  RATIONAL_B_SPLINE_SURFACE ( (
 ( 1.000000000000000000, 1.000000000000000000),
 ( 0.7282232189291694135, 0.9929344683865672927),
 ( 0.7282232189291694135, 0.9929344683865672927),
 ( 1.000000000000000000, 1.000000000000000000) ) ) 
 REPRESENTATION_ITEM ( '' )  SURFACE ( )  );
#8697 = ORIENTED_EDGE ( 'NONE', *, *, #25324, .T. ) ;
#8698 = VECTOR ( 'NONE', #6538, 1000.000000000000114 ) ;
#8699 = CARTESIAN_POINT ( 'NONE',  ( -0.5999999999999992006, -11.64055411052240352, 0.000000000000000000 ) ) ;
#8700 = ADVANCED_FACE ( 'NONE', ( #26931, #2485 ), #41357, .F. ) ;
#8701 = CARTESIAN_POINT ( 'NONE',  ( 4.390527457369401532, -33.24441824160808778, -28.72270865370560955 ) ) ;
#8702 = COLOUR_RGB ( '', 0.31764706, 0.68627451, 0.89019608) ;
#8703 = CARTESIAN_POINT ( 'NONE',  ( 4.975610109902397937, 30.94437158899635776, -37.88001153774755636 ) ) ;
#8704 = DIRECTION ( 'NONE',  ( 0.000000000000000000, 0.000000000000000000, 1.000000000000000000 ) ) ;
#8705 = CIRCLE ( 'NONE', #45716, 43.08621763946400307 ) ;
#8706 = EDGE_CURVE ( 'NONE', #43281, #4666, #59815, .T. ) ;
#8707 = ORIENTED_EDGE ( 'NONE', *, *, #11426, .T. ) ;
#8708 = CARTESIAN_POINT ( 'NONE',  ( 1.088313998177385944, -25.50107284445290645, -34.51470853099742442 ) ) ;
#8709 = B_SPLINE_CURVE_WITH_KNOTS ( 'NONE', 3,
 ( #7996, #36522, #55589, #41531 ),
 .UNSPECIFIED., .F., .F.,
 ( 4, 4 ),
 ( 2.189128766608093164E-17, 0.004559932413162186803 ),
 .UNSPECIFIED. ) ;
#8710 = CARTESIAN_POINT ( 'NONE',  ( 4.967162193818130511, 24.30453456948160351, -35.57684288741949530 ) ) ;
#8711 = EDGE_CURVE ( 'NONE', #19581, #34712, #36325, .T. ) ;
#8712 = ORIENTED_EDGE ( 'NONE', *, *, #6565, .T. ) ;
#8713 = B_SPLINE_CURVE_WITH_KNOTS ( 'NONE', 3,
 ( #59046, #15241, #54332, #34648, #44081, #39366 ),
 .UNSPECIFIED., .F., .F.,
 ( 4, 2, 4 ),
 ( 6.149443329761889321E-18, 0.0002445244328975385408, 0.0004890488657950710100 ),
 .UNSPECIFIED. ) ;
#8714 = CARTESIAN_POINT ( 'NONE',  ( 4.967162193818130511, 0.000000000000000000, 0.000000000000000000 ) ) ;
#8715 = ORIENTED_EDGE ( 'NONE', *, *, #16920, .T. ) ;
#8716 = CARTESIAN_POINT ( 'NONE',  ( 4.999999999999997335, 8.388739760877188892E-13, -80.00000000000001421 ) ) ;
#8717 = CARTESIAN_POINT ( 'NONE',  ( 0.9762797500689124330, -41.16654106227468901, -7.851158013551661874 ) ) ;
#8718 = ORIENTED_EDGE ( 'NONE', *, *, #28282, .F. ) ;
#8719 = CARTESIAN_POINT ( 'NONE',  ( -6.077587904424778920, -1.855182226446173921, 19.16648951426965652 ) ) ;
#8720 = CARTESIAN_POINT ( 'NONE',  ( 0.1081432562775997974, 25.91533557232844487, 34.46918062033758900 ) ) ;
#8721 = VERTEX_POINT ( 'NONE', #9904 ) ;
#8722 = DIRECTION ( 'NONE',  ( -0.07906939808003035641, -0.7338893160900470392, 0.6746513929550169708 ) ) ;
#8723 = CARTESIAN_POINT ( 'NONE',  ( 0.8554163680231720024, -30.98316862405900096, -35.23136010892773839 ) ) ;
#8724 = EDGE_CURVE ( 'NONE', #60706, #31862, #49446, .T. ) ;
#8725 = EDGE_LOOP ( 'NONE', ( #21967, #50733 ) ) ;
#8726 = CARTESIAN_POINT ( 'NONE',  ( 0.000000000000000000, 0.000000000000000000, 0.000000000000000000 ) ) ;
#8727 = ORIENTED_EDGE ( 'NONE', *, *, #13986, .F. ) ;
#8728 = CARTESIAN_POINT ( 'NONE',  ( 5.958863334805807099, -20.34989385289159713, 2.680345151634269563 ) ) ;
#8729 = EDGE_CURVE ( 'NONE', #47950, #24982, #28690, .T. ) ;
#8730 = ORIENTED_EDGE ( 'NONE', *, *, #44282, .T. ) ;
#8731 = AXIS2_PLACEMENT_3D ( 'NONE', #33371, #56221, #47768 ) ;
#8732 = EDGE_LOOP ( 'NONE', ( #11599, #57179, #8828, #6689 ) ) ;
#8733 = LINE ( 'NONE', #42898, #13653 ) ;
#8734 = CARTESIAN_POINT ( 'NONE',  ( 4.956653778116971054, 47.05699031914949160, 9.917440902361329691 ) ) ;
#8735 = DIRECTION ( 'NONE',  ( 0.000000000000000000, 0.000000000000000000, 1.000000000000000000 ) ) ;
#8736 = CARTESIAN_POINT ( 'NONE',  ( 4.962356264823608143, -41.76635909427997717, 5.177532797578748180 ) ) ;
#8737 = CARTESIAN_POINT ( 'NONE',  ( 2.185380717157383579, -28.56354028868287642, -33.51035614916662553 ) ) ;
#8738 = ORIENTED_EDGE ( 'NONE', *, *, #31114, .F. ) ;
#8739 = CARTESIAN_POINT ( 'NONE',  ( 0.8760168074887090262, -29.98565522133319661, -37.61398439004523198 ) ) ;
#8740 = CARTESIAN_POINT ( 'NONE',  ( 0.6064515330803571524, -46.09360457555626311, -8.643723345257249946 ) ) ;
#8741 = CARTESIAN_POINT ( 'NONE',  ( 0.5980271706414711508, 48.33586592461352893, -8.700190122028747197 ) ) ;
#8742 = EDGE_LOOP ( 'NONE', ( #29205, #37448, #8707, #12677 ) ) ;
#8743 = EDGE_LOOP ( 'NONE', ( #38260, #32247, #50095, #31091 ) ) ;
#8744 = CARTESIAN_POINT ( 'NONE',  ( 4.962356264823602814, 39.61238188121407688, -14.21600504921160812 ) ) ;
#8745 = CARTESIAN_POINT ( 'NONE',  ( 0.8557997880470599172, -0.9121262075949487791, 47.89938907511593413 ) ) ;
#8746 = CARTESIAN_POINT ( 'NONE',  ( 4.303969348037246512, 14.52400616872432870, -45.86537346639043022 ) ) ;
#8747 = CARTESIAN_POINT ( 'NONE',  ( 4.962356264823608143, 0.000000000000000000, 0.000000000000000000 ) ) ;
#8748 = CARTESIAN_POINT ( 'NONE',  ( 2.185380717157383579, -34.40864559835211622, 27.47480502486236631 ) ) ;
#8749 = CONICAL_SURFACE ( 'NONE', #19766, 43.08621763946400307, 1.568696531533066763 ) ;
#8750 = ORIENTED_EDGE ( 'NONE', *, *, #36136, .F. ) ;
#8752 = CARTESIAN_POINT ( 'NONE',  ( -2.739355103387248747, 11.19469682329931892, -9.875542009704030733 ) ) ;
#8751 = VECTOR ( 'NONE', #46827, 1000.000000000000000 ) ;
#8753 = VECTOR ( 'NONE', #12913, 1000.000000000000114 ) ;
#8754 = EDGE_CURVE ( 'NONE', #33340, #13848, #14492, .T. ) ;
#8755 = CARTESIAN_POINT ( 'NONE',  ( 4.967162193818130511, 0.000000000000000000, 0.000000000000000000 ) ) ;
#8756 = CARTESIAN_POINT ( 'NONE',  ( 1.112077966505211624, 43.05397124352811744, -9.454410890690590819 ) ) ;
#8757 = B_SPLINE_CURVE_WITH_KNOTS ( 'NONE', 3,
 ( #22902, #37316, #42631, #60779 ),
 .UNSPECIFIED., .F., .F.,
 ( 4, 4 ),
 ( 8.335815620909995262E-17, 0.005004741218457509078 ),
 .UNSPECIFIED. ) ;
#8758 = CARTESIAN_POINT ( 'NONE',  ( 1.657374760986086049, -38.97867883796889288, -20.53175694622165182 ) ) ;
#8759 = CARTESIAN_POINT ( 'NONE',  ( 3.727782113643637540, -41.50446234663599654, -14.49680589725369906 ) ) ;
#8760 = ADVANCED_FACE ( 'NONE', ( #51331 ), #19307, .F. ) ;
#8761 = CARTESIAN_POINT ( 'NONE',  ( 4.975610109902397937, 0.000000000000000000, 0.000000000000000000 ) ) ;
#8762 = ORIENTED_EDGE ( 'NONE', *, *, #51146, .F. ) ;
#8763 = CARTESIAN_POINT ( 'NONE',  ( 0.9762797500689124330, -39.42083772998332591, 14.22400568939802845 ) ) ;
#8764 = LINE ( 'NONE', #5582, #34623 ) ;
#8765 = EDGE_CURVE ( 'NONE', #61767, #13813, #42317, .T. ) ;
#8766 = DIRECTION ( 'NONE',  ( 1.000000000000000000, 0.000000000000000000, 0.000000000000000000 ) ) ;
#8767 = ADVANCED_FACE ( 'NONE', ( #48416 ), #19510, .F. ) ;
#8768 = CARTESIAN_POINT ( 'NONE',  ( 5.959547316686252039, 17.77392908783934189, -10.26589671991344588 ) ) ;
#8769 = EDGE_CURVE ( 'NONE', #45625, #51992, #27539, .T. ) ;
#8770 = CARTESIAN_POINT ( 'NONE',  ( 0.5807400328401574052, 18.83234461715242247, -44.04145271122545324 ) ) ;
#8771 = CARTESIAN_POINT ( 'NONE',  ( 8.000000000000007105, -58.44237546506767700, -54.69470952477997372 ) ) ;
#8772 = CARTESIAN_POINT ( 'NONE',  ( 0.6021448801613057400, -49.10674992472959843, -0.2612478842340035801 ) ) ;
#8773 = VECTOR ( 'NONE', #37916, 1000.000000000000227 ) ;
#8774 = CARTESIAN_POINT ( 'NONE',  ( 5.959828726073459926, 5.316791119501089291, -19.82504517499707575 ) ) ;
#8775 = ADVANCED_FACE ( 'NONE', ( #19620 ), #30648, .F. ) ;
#8776 = AXIS2_PLACEMENT_3D ( 'NONE', #7366, #21488, #59694 ) ;
#8777 = FACE_OUTER_BOUND ( 'NONE', #56708, .T. ) ;
#8778 = EDGE_LOOP ( 'NONE', ( #51634, #40057, #32805, #57932 ) ) ;
#8779 = CARTESIAN_POINT ( 'NONE',  ( 0.2500000000000002220, 0.000000000000000000, 0.000000000000000000 ) ) ;
#8780 = CARTESIAN_POINT ( 'NONE',  ( 0.5837374860065639437, 46.31070423340730713, 12.22086613152778689 ) ) ;
#8781 = CARTESIAN_POINT ( 'NONE',  ( 0.7948884756798503259, -42.34838783475078827, -24.84577816043769971 ) ) ;
#8782 = CARTESIAN_POINT ( 'NONE',  ( 0.5806925824938511393, -45.84420715090610798, 9.875780123533177246 ) ) ;
#8783 = ORIENTED_EDGE ( 'NONE', *, *, #50750, .T. ) ;
#8784 = FACE_OUTER_BOUND ( 'NONE', #52546, .T. ) ;
#8785 = CARTESIAN_POINT ( 'NONE',  ( 0.9787464366903556590, -41.80285375509220103, -2.975804230933245531 ) ) ;
#8786 = ORIENTED_EDGE ( 'NONE', *, *, #12925, .T. ) ;
#8788 = CARTESIAN_POINT ( 'NONE',  ( 0.1157506346131639274, 4.144581685519440839, -43.92906899144222876 ) ) ;
#8787 = B_SPLINE_CURVE_WITH_KNOTS ( 'NONE', 3,
 ( #25654, #59154, #35387, #54763, #49772, #6832, #25973, #45106, #2133, #11897, #30979, #50089, #36620, #3074, #24277, #38712, #27205, #22201, #60695 ),
 .UNSPECIFIED., .F., .F.,
 ( 4, 3, 3, 3, 3, 3, 4 ),
 ( 6.938893903907228378E-18, 0.0002724573126191740208, 0.0004086839781548500493, 0.0005449106435901848473, 0.0006811373090491499400, 0.0008459866663933689407, 0.001010840725717213149 ),
 .UNSPECIFIED. ) ;
#8789 = DIRECTION ( 'NONE',  ( -1.000000000000000000, -1.836909530733573529E-16, 1.361838123766461297E-32 ) ) ;
#8790 = CARTESIAN_POINT ( 'NONE',  ( 4.956445790444035104, 41.78282513192535674, -21.71942849465849079 ) ) ;
#8791 = VERTEX_POINT ( 'NONE', #20234 ) ;
#8792 = DIRECTION ( 'NONE',  ( 0.000000000000000000, 0.000000000000000000, 1.000000000000000000 ) ) ;
#8793 = VECTOR ( 'NONE', #24862, 1000.000000000000227 ) ;
#8794 = ORIENTED_EDGE ( 'NONE', *, *, #56127, .F. ) ;
#8795 = ORIENTED_EDGE ( 'NONE', *, *, #50444, .T. ) ;
#8796 = CARTESIAN_POINT ( 'NONE',  ( 0.5827357941260203900, -6.611647889510890330, -47.43746130990125209 ) ) ;
#8797 = CARTESIAN_POINT ( 'NONE',  ( 0.1129192098497447394, 10.29049805561828101, 42.90754522869457332 ) ) ;
#8798 = ORIENTED_EDGE ( 'NONE', *, *, #12257, .T. ) ;
#8799 = CARTESIAN_POINT ( 'NONE',  ( 5.895881250540457863, 5.954605924856151589, -19.21120375947246117 ) ) ;
#8800 = PRODUCT ( 'socket head cap screw_iso_ISO 4762 M5 x 16 - 16N', 'socket head cap screw_iso_ISO 4762 M5 x 16 - 16N', '', ( #13033 ) ) ;
#8801 = ORIENTED_EDGE ( 'NONE', *, *, #40023, .F. ) ;
#8802 = CARTESIAN_POINT ( 'NONE',  ( 5.895596859100789899, -19.39731145114843613, -5.317188324634858354 ) ) ;
#8803 = SHAPE_REPRESENTATION ( 'straight bevel gear(wobble out)_iso_ISO - Straight bevel gear 2M 48GT 47PT 20PA 5FW ---48O1H50MD20.0S1', ( #14677 ), #46738 ) ;
#8804 = EDGE_CURVE ( 'NONE', #21034, #50035, #5479, .T. ) ;
#8805 = CARTESIAN_POINT ( 'NONE',  ( 0.9730545539215883499, 0.5054011016618756846, -42.90536227157002003 ) ) ;
#8806 = DIRECTION ( 'NONE',  ( -1.000000000000000000, -0.000000000000000000, -0.000000000000000000 ) ) ;
#8807 = ORIENTED_EDGE ( 'NONE', *, *, #6062, .F. ) ;
#8808 = FACE_OUTER_BOUND ( 'NONE', #44624, .T. ) ;
#8809 = AXIS2_PLACEMENT_3D ( 'NONE', #40609, #59673, #51199 ) ;
#8810 = CARTESIAN_POINT ( 'NONE',  ( 5.896782393890504181, 19.71107130340476132, -3.999969368645934775 ) ) ;
#8811 = FACE_OUTER_BOUND ( 'NONE', #14221, .T. ) ;
#8812 = CARTESIAN_POINT ( 'NONE',  ( 1.231276596079887264, -18.40965318903149495, -37.66113965983570466 ) ) ;
#8813 = ORIENTED_EDGE ( 'NONE', *, *, #49722, .T. ) ;
#8815 = B_SPLINE_CURVE_WITH_KNOTS ( 'NONE', 3,
 ( #55248, #40896, #6378, #59027, #2008, #16142 ),
 .UNSPECIFIED., .F., .F.,
 ( 4, 2, 4 ),
 ( 2.611104600503255956E-18, 0.0002447193893791698165, 0.0004894387787583370309 ),
 .UNSPECIFIED. ) ;
#8814 = PRODUCT_DEFINITION ( 'UNKNOWN', '', #18901, #17974 ) ;
#8816 = CARTESIAN_POINT ( 'NONE',  ( 0.5832366564991503521, -34.05963937630778560, -33.67434452455949412 ) ) ;
#8817 = CARTESIAN_POINT ( 'NONE',  ( 4.967162193818130511, -28.74031574030035685, 32.10009971360062764 ) ) ;
#8818 = VERTEX_POINT ( 'NONE', #3708 ) ;
#8819 = CARTESIAN_POINT ( 'NONE',  ( 4.694002226626921015, -34.48859517587319345, -29.81311077765740691 ) ) ;
#8820 = EDGE_LOOP ( 'NONE', ( #35334, #23438, #54149, #26586, #53475, #36247, #53939, #33039, #39499, #36197, #28900, #16415, #54154, #61632, #47114, #21323 ) ) ;
#8821 = CARTESIAN_POINT ( 'NONE',  ( 0.8560838555295158248, -20.57050347530512724, 42.15717282805135113 ) ) ;
#8822 = CARTESIAN_POINT ( 'NONE',  ( 0.5837800304671224572, 10.91570225908018976, -45.60794641694153029 ) ) ;
#8823 = VERTEX_POINT ( 'NONE', #47817 ) ;
#8824 = DIRECTION ( 'NONE',  ( -1.000000000000000000, -0.000000000000000000, -0.000000000000000000 ) ) ;
#8825 = CARTESIAN_POINT ( 'NONE',  ( -6.079354080745853928, 0.6183512803183812689, -19.24605406160677390 ) ) ;
#8826 = CARTESIAN_POINT ( 'NONE',  ( 0.6016117650947691020, 28.38024422091337229, 40.07633706073713142 ) ) ;
#8827 = CARTESIAN_POINT ( 'NONE',  ( 0.3676999524040323597, 43.96170928169360081, 3.649479463525401535 ) ) ;
#8828 = ORIENTED_EDGE ( 'NONE', *, *, #47468, .T. ) ;
#8829 = CARTESIAN_POINT ( 'NONE',  ( 0.1147471544378676350, -40.78200343799206706, 16.84578238185594046 ) ) ;
#8830 = FACE_OUTER_BOUND ( 'NONE', #27064, .T. ) ;
#8831 = CARTESIAN_POINT ( 'NONE',  ( 0.6846871229502899947, 29.84551600520632419, 37.47592888575258741 ) ) ;
#8832 = CARTESIAN_POINT ( 'NONE',  ( 0.7048096507298579061, 48.10291524268439645, 0.8437160066908956368 ) ) ;
#8833 = EDGE_CURVE ( 'NONE', #54885, #48040, #13913, .T. ) ;
#8834 = CARTESIAN_POINT ( 'NONE',  ( 4.962356264823600149, -40.47344704301802665, 11.53844366967928892 ) ) ;
#8835 = FACE_BOUND ( 'NONE', #30751, .T. ) ;
#8836 = B_SPLINE_CURVE_WITH_KNOTS ( 'NONE', 3,
 ( #19425, #58525, #43552, #11253 ),
 .UNSPECIFIED., .F., .F.,
 ( 4, 4 ),
 ( 4.336808689942017736E-19, 0.004041751736740990808 ),
 .UNSPECIFIED. ) ;
#8837 = CARTESIAN_POINT ( 'NONE',  ( 0.8560838555295158248, -26.00596412780176081, 39.03924517540291106 ) ) ;
#8838 = EDGE_CURVE ( 'NONE', #6280, #38091, #55467, .T. ) ;
#8839 = VECTOR ( 'NONE', #12141, 1000.000000000000000 ) ;
#8840 = CARTESIAN_POINT ( 'NONE',  ( 0.1119899015040011353, -41.10694703553422613, 16.03683926496394818 ) ) ;
#8841 = ADVANCED_FACE ( 'NONE', ( #6386 ), #39104, .F. ) ;
#8842 = AXIS2_PLACEMENT_3D ( 'NONE', #54750, #8080, #13112 ) ;
#8843 = EDGE_CURVE ( 'NONE', #18602, #6564, #61679, .T. ) ;
#8844 = CARTESIAN_POINT ( 'NONE',  ( 0.5824935313925944103, 40.16257500733529895, -24.21168614190273161 ) ) ;
#8845 = CARTESIAN_POINT ( 'NONE',  ( -2.708315649062916552, 10.53288422393042190, 10.16016146078292337 ) ) ;
#8846 = CARTESIAN_POINT ( 'NONE',  ( 5.960721111146673579, 5.318514366754659939, 19.82454228767747750 ) ) ;
#8847 = DIRECTION ( 'NONE',  ( -1.000000000000000000, -0.000000000000000000, -0.000000000000000000 ) ) ;
#8848 = CYLINDRICAL_SURFACE ( 'NONE', #35618, 85.00000000000001421 ) ;
#8849 = CARTESIAN_POINT ( 'NONE',  ( 1.154321485836933503, -41.66001465002020154, -10.30834589251754885 ) ) ;
#8850 = CARTESIAN_POINT ( 'NONE',  ( 2.185380717157383135, -21.58356241136808862, 38.37928655800909894 ) ) ;
#8851 = CARTESIAN_POINT ( 'NONE',  ( 1.231276596079881047, -7.805643096902013411, 41.18675402191647805 ) ) ;
#8852 = FACE_OUTER_BOUND ( 'NONE', #10553, .T. ) ;
#8854 = ORIENTED_EDGE ( 'NONE', *, *, #26219, .T. ) ;
#8853 = DIRECTION ( 'NONE',  ( 0.000000000000000000, 0.000000000000000000, -1.000000000000000000 ) ) ;
#8855 = EDGE_CURVE ( 'NONE', #53370, #10587, #31155, .T. ) ;
#8856 = AXIS2_PLACEMENT_3D ( 'NONE', #61433, #23252, #33586 ) ;
#8857 = DIRECTION ( 'NONE',  ( 0.000000000000000000, 0.000000000000000000, 1.000000000000000000 ) ) ;
#8858 = CARTESIAN_POINT ( 'NONE',  ( 0.7242486021783839378, 5.529549040179291275, -48.78970741648514320 ) ) ;
#8859 = CARTESIAN_POINT ( 'NONE',  ( 5.917102823773431552, -2.021675920616845090, -20.01006108245899640 ) ) ;
#8860 = ORIENTED_EDGE ( 'NONE', *, *, #4969, .F. ) ;
#8861 = EDGE_CURVE ( 'NONE', #12452, #23359, #2014, .T. ) ;
#8862 = EDGE_LOOP ( 'NONE', ( #56115, #11543, #2675, #57158 ) ) ;
#8863 = CARTESIAN_POINT ( 'NONE',  ( 0.1129192098497447394, -23.28677643606880565, -37.47903188453118162 ) ) ;
#8864 = CARTESIAN_POINT ( 'NONE',  ( 0.9762797500689124330, -12.89881610234976961, 39.87411852747928265 ) ) ;
#8865 = AXIS2_PLACEMENT_3D ( 'NONE', #38770, #61601, #9610 ) ;
#8866 = EDGE_LOOP ( 'NONE', ( #32957, #24976, #25219, #52602 ) ) ;
#8867 = ORIENTED_EDGE ( 'NONE', *, *, #40512, .T. ) ;
#8868 = CARTESIAN_POINT ( 'NONE',  ( 0.9730545539215883499, -10.61654491617534291, -41.57420493492396929 ) ) ;
#8869 = CARTESIAN_POINT ( 'NONE',  ( 4.834790513006555379, 13.88525928490712325, 45.16402235757220041 ) ) ;
#8870 = CARTESIAN_POINT ( 'NONE',  ( 1.231276596079881047, 8.892602616353681100, 40.96581977363184990 ) ) ;
#8871 = CIRCLE ( 'NONE', #51883, 47.91270532121795611 ) ;
#8872 = ORIENTED_EDGE ( 'NONE', *, *, #28249, .T. ) ;
#8873 = ORIENTED_EDGE ( 'NONE', *, *, #25606, .F. ) ;
#8874 = DIRECTION ( 'NONE',  ( 1.000000000000000000, 1.836909530733573776E-16, -1.925929944387235853E-32 ) ) ;
#8875 = EDGE_LOOP ( 'NONE', ( #2213, #27439, #19781, #12399 ) ) ;
#8876 = CARTESIAN_POINT ( 'NONE',  ( 0.1313383488274124933, 15.91164383651745950, -40.08066228784247897 ) ) ;
#8877 = CARTESIAN_POINT ( 'NONE',  ( -2.569797478183783568, -4.218948559326153536, -14.01151037928421417 ) ) ;
#8878 = CARTESIAN_POINT ( 'NONE',  ( 2.643462169533600914, -46.02269433264222442, -13.76277278785544844 ) ) ;
#8879 = ORIENTED_EDGE ( 'NONE', *, *, #397, .T. ) ;
#8880 =( BOUNDED_SURFACE ( )  B_SPLINE_SURFACE ( 3, 1, ( 
 ( #17028, #30172 ),
 ( #40239, #44930 ),
 ( #59603, #54268 ),
 ( #53653, #25473 ) ),
 .UNSPECIFIED., .F., .F., .F. ) 
 B_SPLINE_SURFACE_WITH_KNOTS ( ( 4, 4 ),
 ( 2, 2 ),
 ( 0.000000000000000000, 1.000000000000000000 ),
 ( 0.000000000000000000, 1.000000000000000000 ),
 .UNSPECIFIED. ) 
 GEOMETRIC_REPRESENTATION_ITEM ( )  RATIONAL_B_SPLINE_SURFACE ( (
 ( 1.000000000000000000, 1.000000000000000000),
 ( 0.9953040768229005630, 0.8617119497784937465),
 ( 0.9953040768229005630, 0.8617119497784937465),
 ( 1.000000000000000000, 1.000000000000000000) ) ) 
 REPRESENTATION_ITEM ( '' )  SURFACE ( )  );
#8881 = ADVANCED_FACE ( 'NONE', ( #30225 ), #45502, .F. ) ;
#8882 = CARTESIAN_POINT ( 'NONE',  ( 4.956445790444004018, -45.55738122058057371, -11.91902120403893761 ) ) ;
#8883 = EDGE_LOOP ( 'NONE', ( #35923, #47412 ) ) ;
#8884 = CIRCLE ( 'NONE', #22888, 42.92674063221959813 ) ;
#8885 = ORIENTED_EDGE ( 'NONE', *, *, #3793, .F. ) ;
#8886 = CARTESIAN_POINT ( 'NONE',  ( 0.6000166863083106206, 40.87138819217342700, 27.22780029589463879 ) ) ;
#8887 = CONICAL_SURFACE ( 'NONE', #4838, 43.92652462719577500, 1.486293639869522343 ) ;
#8888 = ORIENTED_EDGE ( 'NONE', *, *, #56001, .F. ) ;
#8889 = CARTESIAN_POINT ( 'NONE',  ( 4.956653778116971942, 35.79382859084115864, 32.11725092155054995 ) ) ;
#8890 = CARTESIAN_POINT ( 'NONE',  ( 2.347571140040969784, -0.2125464247640618254, 41.96959966789661678 ) ) ;
#8891 = DIRECTION ( 'NONE',  ( 0.07439287786467665975, -0.4871392060438023974, -0.8701500408883660054 ) ) ;
#8892 = CARTESIAN_POINT ( 'NONE',  ( 0.5824935313925952984, -38.45572481770904716, 26.84018267073592057 ) ) ;
#8893 = CARTESIAN_POINT ( 'NONE',  ( 0.5997462898726536595, -2.096122762665173944, 49.06279547180476897 ) ) ;
#8894 = ORIENTED_EDGE ( 'NONE', *, *, #17678, .F. ) ;
#8895 = CARTESIAN_POINT ( 'NONE',  ( 0.9741495583595178864, -30.05988007970374198, -30.61921547032183355 ) ) ;
#8896 = CARTESIAN_POINT ( 'NONE',  ( 4.975801465491695552, 27.09127437476327671, 39.51822597168504814 ) ) ;
#8897 = B_SPLINE_CURVE_WITH_KNOTS ( 'NONE', 3,
 ( #41700, #36386, #17882, #8772, #46095, #56066, #7843, #23187, #42315, #12881, #22267, #42011, #51364, #8448, #2829, #61374 ),
 .UNSPECIFIED., .F., .F.,
 ( 4, 3, 3, 3, 3, 4 ),
 ( 2.081781105835003463E-17, 0.0002612764279487746265, 0.0003919131003184792451, 0.0005225497727000651474, 0.0007837925190632462217, 0.001045051706266716084 ),
 .UNSPECIFIED. ) ;
#8898 = DIRECTION ( 'NONE',  ( 0.000000000000000000, 0.000000000000000000, 1.000000000000000000 ) ) ;
#8899 = ORIENTED_EDGE ( 'NONE', *, *, #52265, .T. ) ;
#8900 = CARTESIAN_POINT ( 'NONE',  ( 0.5987334308729317378, 41.48360633127789754, 26.28066422907324906 ) ) ;
#8901 = CARTESIAN_POINT ( 'NONE',  ( 4.956445790443991584, 34.56007374686787159, 31.98654955994301829 ) ) ;
#8902 = CARTESIAN_POINT ( 'NONE',  ( 3.727782113643637096, -4.897728981986997354, 43.68970160947520753 ) ) ;
#8903 = AXIS2_PLACEMENT_3D ( 'NONE', #61895, #29030, #43150 ) ;
#8904 = ORIENTED_EDGE ( 'NONE', *, *, #18545, .F. ) ;
#8905 = ORIENTED_EDGE ( 'NONE', *, *, #57389, .F. ) ;
#8906 = CARTESIAN_POINT ( 'NONE',  ( 0.5809828226811556418, 44.45562576850601744, 17.82437196699697424 ) ) ;
#8907 = DIRECTION ( 'NONE',  ( 0.07836865515943411409, 0.8672783706145194005, -0.4916162952473462910 ) ) ;
#8908 = CARTESIAN_POINT ( 'NONE',  ( 0.5782707292762442330, 21.90237606067556442, 41.47315127409978430 ) ) ;
#8909 = CARTESIAN_POINT ( 'NONE',  ( 0.6021447746440204973, 33.20792045667346315, 36.17699763705849136 ) ) ;
#8910 = B_SPLINE_CURVE_WITH_KNOTS ( 'NONE', 3,
 ( #37420, #33341, #42137, #61794 ),
 .UNSPECIFIED., .F., .F.,
 ( 4, 4 ),
 ( 3.736708725176134707E-17, 0.005004948556313845200 ),
 .UNSPECIFIED. ) ;
#8911 = CARTESIAN_POINT ( 'NONE',  ( 5.960721111146673579, -14.50930005615006912, -14.51823969584094698 ) ) ;
#8912 = CARTESIAN_POINT ( 'NONE',  ( 5.959547316686252039, -19.82715097195166010, 5.308980600728112620 ) ) ;
#8913 = CARTESIAN_POINT ( 'NONE',  ( 0.5997462898726536595, -42.52950339524503676, 24.55184251941493301 ) ) ;
#8914 = DIRECTION ( 'NONE',  ( 0.09835009131224552170, 0.6119264800004677873, 0.7847759187265561653 ) ) ;
#8915 = CARTESIAN_POINT ( 'NONE',  ( 0.1064266418746777493, 42.82540703015432371, -5.071708474752798956 ) ) ;
#8916 = DIRECTION ( 'NONE',  ( 0.000000000000000000, 0.000000000000000000, 1.000000000000000000 ) ) ;
#8917 = EDGE_CURVE ( 'NONE', #36339, #21667, #6087, .T. ) ;
#8918 = CARTESIAN_POINT ( 'NONE',  ( 0.9772918015221165877, 41.90661890918757138, -0.4149064362024745267 ) ) ;
#8919 = CARTESIAN_POINT ( 'NONE',  ( 0.5850706913938534814, -24.10530971368259401, -41.38834827854233112 ) ) ;
#8920 = ORIENTED_EDGE ( 'NONE', *, *, #6670, .T. ) ;
#8921 = EDGE_CURVE ( 'NONE', #37463, #45480, #43484, .T. ) ;
#8922 = CARTESIAN_POINT ( 'NONE',  ( 0.7764146366350254125, -46.73184010359712914, 4.021889381994030899 ) ) ;
#8923 = CARTESIAN_POINT ( 'NONE',  ( 0.1100247026804066219, -34.10937070541727678, -26.38690693952944955 ) ) ;
#8924 = CARTESIAN_POINT ( 'NONE',  ( -6.016761891674564211, -11.46828378093569789, 14.95139917749700587 ) ) ;
#8925 = CARTESIAN_POINT ( 'NONE',  ( 0.6001305935487315502, -37.84751346122835969, -29.70149728382423504 ) ) ;
#8926 = B_SPLINE_CURVE_WITH_KNOTS ( 'NONE', 3,
 ( #49851, #21658, #40799, #36089 ),
 .UNSPECIFIED., .F., .F.,
 ( 4, 4 ),
 ( 5.057544569639794935E-18, 0.004050076154992999014 ),
 .UNSPECIFIED. ) ;
#8927 = CARTESIAN_POINT ( 'NONE',  ( 0.3676999524040366896, -23.56959980820299094, -37.28839696479317212 ) ) ;
#8928 = CARTESIAN_POINT ( 'NONE',  ( 0.3676999524040366896, -22.15802448780013378, 38.14410221935873579 ) ) ;
#8929 = CARTESIAN_POINT ( 'NONE',  ( 0.8751705887134553219, 17.57879340691544101, -44.76769609654218129 ) ) ;
#8930 = CARTESIAN_POINT ( 'NONE',  ( 4.291220156522060236, -40.01826627095181266, -24.85814478139707617 ) ) ;
#8931 = CARTESIAN_POINT ( 'NONE',  ( 0.6008123274975392114, -2.009114500091637279, 49.06646522915604436 ) ) ;
#8933 = ORIENTED_EDGE ( 'NONE', *, *, #24644, .F. ) ;
#8932 = CARTESIAN_POINT ( 'NONE',  ( 4.956653778116827169, 32.11725092155053574, 35.79382859084104496 ) ) ;
#8934 = ORIENTED_EDGE ( 'NONE', *, *, #17619, .F. ) ;
#8935 = CIRCLE ( 'NONE', #37990, 48.09070567114147110 ) ;
#8936 = CARTESIAN_POINT ( 'NONE',  ( 0.1152339509894530906, -6.821579089989193712, 43.59367785785303084 ) ) ;
#8937 = CARTESIAN_POINT ( 'NONE',  ( 0.1073791018717483448, 42.81622261970987608, 5.147744207007008299 ) ) ;
#8938 = CARTESIAN_POINT ( 'NONE',  ( 0.5800708057587388167, 17.74761804745402571, 44.48635630048006107 ) ) ;
#8939 = EDGE_CURVE ( 'NONE', #15929, #52958, #58686, .T. ) ;
#8940 = ORIENTED_EDGE ( 'NONE', *, *, #56776, .F. ) ;
#8941 = CARTESIAN_POINT ( 'NONE',  ( 0.6021447746440204973, 10.67256517526007187, -47.93367805278783322 ) ) ;
#8942 = CARTESIAN_POINT ( 'NONE',  ( -6.077587904424778920, 3.067159685105322442, 19.01022232536997691 ) ) ;
#8943 = FACE_OUTER_BOUND ( 'NONE', #6934, .T. ) ;
#8944 = VERTEX_POINT ( 'NONE', #16147 ) ;
#8945 = ORIENTED_EDGE ( 'NONE', *, *, #1006, .F. ) ;
#8946 = CARTESIAN_POINT ( 'NONE',  ( 0.9789233960466690032, 24.96512103919651082, -33.66124564436990596 ) ) ;
#8947 = VECTOR ( 'NONE', #29702, 1000.000000000000114 ) ;
#8948 = CARTESIAN_POINT ( 'NONE',  ( 0.8744876279028263033, 23.49358985382666631, -43.10917867646825385 ) ) ;
#8949 = DIRECTION ( 'NONE',  ( -1.000000000000000000, -0.000000000000000000, -0.000000000000000000 ) ) ;
#8950 = CARTESIAN_POINT ( 'NONE',  ( 0.9780106845699481077, 33.08330293080910423, -25.72598518315200522 ) ) ;
#8951 = CARTESIAN_POINT ( 'NONE',  ( 5.895596859100789899, 14.91436009500240445, 13.49407448360528861 ) ) ;
#8952 = B_SPLINE_CURVE_WITH_KNOTS ( 'NONE', 3,
 ( #31803, #55578, #36204, #22090, #45920, #46523 ),
 .UNSPECIFIED., .F., .F.,
 ( 4, 2, 4 ),
 ( 1.266058488688919593E-17, 0.0002448709889506581867, 0.0004897419779013036881 ),
 .UNSPECIFIED. ) ;
#8953 = CARTESIAN_POINT ( 'NONE',  ( 0.8760168074887076939, 19.22870327415240865, 44.09317760313759749 ) ) ;
#8954 = EDGE_CURVE ( 'NONE', #19678, #28808, #7438, .T. ) ;
#8955 = CARTESIAN_POINT ( 'NONE',  ( 0.5987334308729319599, -24.93754662327836868, 42.30462947458052270 ) ) ;
#8956 = ORIENTED_EDGE ( 'NONE', *, *, #8402, .F. ) ;
#8957 =( BOUNDED_SURFACE ( )  B_SPLINE_SURFACE ( 3, 1, ( 
 ( #61481, #48333 ),
 ( #38646, #47116 ),
 ( #24518, #57701 ),
 ( #53019, #33331 ) ),
 .UNSPECIFIED., .F., .F., .F. ) 
 B_SPLINE_SURFACE_WITH_KNOTS ( ( 4, 4 ),
 ( 2, 2 ),
 ( 0.000000000000000000, 1.000000000000000000 ),
 ( 0.000000000000000000, 1.000000000000000000 ),
 .UNSPECIFIED. ) 
 GEOMETRIC_REPRESENTATION_ITEM ( )  RATIONAL_B_SPLINE_SURFACE ( (
 ( 1.000000000000000000, 1.000000000000000000),
 ( 0.9953040768229013402, 0.8617119497784988535),
 ( 0.9953040768229013402, 0.8617119497784988535),
 ( 1.000000000000000000, 1.000000000000000000) ) ) 
 REPRESENTATION_ITEM ( '' )  SURFACE ( )  );
#8958 = B_SPLINE_CURVE_WITH_KNOTS ( 'NONE', 3,
 ( #26566, #55670, #46618, #3353, #16878, #12801, #59448, #55986, #40698, #36920, #51283, #12484, #45390, #55056, #35994, #3662 ),
 .UNSPECIFIED., .F., .F.,
 ( 4, 3, 3, 3, 3, 4 ),
 ( 2.081781105835003155E-17, 0.0002612764279487750059, 0.0003919131003184806545, 0.0005225497727000651474, 0.0007837925190632466553, 0.001045051706266716084 ),
 .UNSPECIFIED. ) ;
#8959 = CARTESIAN_POINT ( 'NONE',  ( 0.5800708119828335008, -11.78915056783740489, 46.42229822050692434 ) ) ;
#8960 = VERTEX_POINT ( 'NONE', #10832 ) ;
#8961 = CARTESIAN_POINT ( 'NONE',  ( 0.9787464366903563251, -37.32407051563441769, -19.05905960519595155 ) ) ;
#8962 = CARTESIAN_POINT ( 'NONE',  ( 5.981074661064941900, 20.52466374824937034, -0.008585178657404223673 ) ) ;
#8963 = CARTESIAN_POINT ( 'NONE',  ( 5.838029081930955932, 35.01788019483823433, 31.69878743442524538 ) ) ;
#8964 = CARTESIAN_POINT ( 'NONE',  ( 0.8744876279028263033, 23.49358985382666631, -43.10917867646825385 ) ) ;
#8965 = ORIENTED_EDGE ( 'NONE', *, *, #15871, .T. ) ;
#8967 = EDGE_CURVE ( 'NONE', #22241, #56714, #44545, .T. ) ;
#8966 = ORIENTED_EDGE ( 'NONE', *, *, #42743, .F. ) ;
#8968 = CARTESIAN_POINT ( 'NONE',  ( 0.6846871229502899947, -17.53234844287773697, 44.58493949243999310 ) ) ;
#8969 = CARTESIAN_POINT ( 'NONE',  ( 3.680974057930774812, -39.15945827951728830, 27.71659654258229821 ) ) ;
#8970 = CARTESIAN_POINT ( 'NONE',  ( 0.8560838555295223751, -2.480523550130904642, -46.84250032821665854 ) ) ;
#8971 = ORIENTED_EDGE ( 'NONE', *, *, #44937, .T. ) ;
#8972 = CARTESIAN_POINT ( 'NONE',  ( 4.000000000000003553, 2.309401076758524685, -0.3572655899081733644 ) ) ;
#8973 = EDGE_CURVE ( 'NONE', #49007, #4007, #56449, .T. ) ;
#8974 = ORIENTED_EDGE ( 'NONE', *, *, #34006, .T. ) ;
#8975 = CARTESIAN_POINT ( 'NONE',  ( 1.479689385636123067, 43.46015683608160884, 7.266265412912084720 ) ) ;
#8976 = CARTESIAN_POINT ( 'NONE',  ( 0.5817216825391123836, 28.18300595765020233, 37.48270437679907019 ) ) ;
#8977 = VECTOR ( 'NONE', #58949, 1000.000000000000227 ) ;
#8978 = CARTESIAN_POINT ( 'NONE',  ( 0.6024113833632039894, -13.76358228951890439, -47.13921585750561150 ) ) ;
#8979 = ORIENTED_EDGE ( 'NONE', *, *, #57457, .T. ) ;
#8980 = CARTESIAN_POINT ( 'NONE',  ( 4.958415959904820092, -21.38448066593202768, -40.07378121005077531 ) ) ;
#8981 = CARTESIAN_POINT ( 'NONE',  ( 0.7044674535453004927, -49.10288787214295070, 0.8420958536080205281 ) ) ;
#8982 = CARTESIAN_POINT ( 'NONE',  ( 5.894904586330512508, 14.91596325940019341, 13.49234790931016015 ) ) ;
#8983 = CARTESIAN_POINT ( 'NONE',  ( 0.5832366564991509073, -18.58038995918320779, -44.14509737861668981 ) ) ;
#8984 = CARTESIAN_POINT ( 'NONE',  ( 0.1156495703730067576, 33.50965052305380709, -28.70620621144267304 ) ) ;
#8985 = CARTESIAN_POINT ( 'NONE',  ( 1.157643937452370153, -40.90424016976600541, 9.156713970025162297 ) ) ;
#8986 = CARTESIAN_POINT ( 'NONE',  ( 0.1100053167205930771, 26.10991185395887371, -34.32189548568256754 ) ) ;
#8987 = CARTESIAN_POINT ( 'NONE',  ( 0.3676999524040323597, -38.83470403830501994, 20.92406140260764857 ) ) ;
#8988 = ORIENTED_EDGE ( 'NONE', *, *, #52156, .T. ) ;
#8989 = ADVANCED_FACE ( 'NONE', ( #17078 ), #2650, .F. ) ;
#8990 = CARTESIAN_POINT ( 'NONE',  ( 0.5804410086790514622, -46.06497594411302288, -8.805557513507338285 ) ) ;
#8991 = VERTEX_POINT ( 'NONE', #17376 ) ;
#8992 = ADVANCED_FACE ( 'NONE', ( #36811 ), #19890, .F. ) ;
#8993 = CARTESIAN_POINT ( 'NONE',  ( 0.3622758884714730732, 33.69533458712344753, -26.89560658783350178 ) ) ;
#8994 = FACE_OUTER_BOUND ( 'NONE', #13159, .T. ) ;
#8995 = CARTESIAN_POINT ( 'NONE',  ( 0.9762797500689124330, 9.222352665238926051, -40.88120590813907285 ) ) ;
#8996 = CARTESIAN_POINT ( 'NONE',  ( 0.9722240741986377666, 41.59310805473383255, -10.54237114526840102 ) ) ;
#8997 = CARTESIAN_POINT ( 'NONE',  ( -6.015611763856276717, -18.84324252354755203, 0.006214430185075541652 ) ) ;
#8998 = CARTESIAN_POINT ( 'NONE',  ( 5.959828726073459926, 18.96492317065693811, -7.850628836606658112 ) ) ;
#8999 = EDGE_CURVE ( 'NONE', #43474, #32408, #26529, .T. ) ;
#9000 = DIRECTION ( 'NONE',  ( 1.000000000000000000, 0.000000000000000000, 0.000000000000000000 ) ) ;
#9001 = DIRECTION ( 'NONE',  ( 0.000000000000000000, 0.000000000000000000, -1.000000000000000000 ) ) ;
#9002 = CARTESIAN_POINT ( 'NONE',  ( 5.440000000000000391, 6.831466544798160849E-15, 0.000000000000000000 ) ) ;
#9003 = CARTESIAN_POINT ( 'NONE',  ( 4.967162193818130511, 0.000000000000000000, 0.000000000000000000 ) ) ;
#9004 = CARTESIAN_POINT ( 'NONE',  ( 5.896782393890504181, -18.51439742298330771, -7.857682542699298445 ) ) ;
#9005 = CARTESIAN_POINT ( 'NONE',  ( -2.601141883200662974, 13.63649176842536903, 6.069721552019974098 ) ) ;
#9006 = ORIENTED_EDGE ( 'NONE', *, *, #23413, .F. ) ;
#9007 = CARTESIAN_POINT ( 'NONE',  ( 0.8551540677456834771, 23.16399837394605044, -41.94570365541178347 ) ) ;
#9008 = CARTESIAN_POINT ( 'NONE',  ( 5.960721111146673579, -2.672857320903454514, 20.35079619394241135 ) ) ;
#9009 = EDGE_CURVE ( 'NONE', #38620, #38431, #11443, .T. ) ;
#9010 = B_SPLINE_CURVE_WITH_KNOTS ( 'NONE', 3,
 ( #61082, #22586, #56688, #13817 ),
 .UNSPECIFIED., .F., .F.,
 ( 4, 4 ),
 ( 0.000000000000000000, 0.004445488388166994251 ),
 .UNSPECIFIED. ) ;
#9011 = CARTESIAN_POINT ( 'NONE',  ( -2.739355103387247858, 14.24824591804153151, -4.453656386614238905 ) ) ;
#9012 = CARTESIAN_POINT ( 'NONE',  ( 0.5837157313716021534, 46.46537190809685569, 6.340841980704805536 ) ) ;
#9013 = CARTESIAN_POINT ( 'NONE',  ( 3.783278058412225864, -24.80906179324464844, 35.16831859152123485 ) ) ;
#9014 = B_SPLINE_CURVE_WITH_KNOTS ( 'NONE', 3,
 ( #31756, #56463, #13576, #56159, #36471, #22975 ),
 .UNSPECIFIED., .F., .F.,
 ( 4, 2, 4 ),
 ( 5.208685977958202256E-18, 0.0002291459268755725387, 0.0004582918537511398733 ),
 .UNSPECIFIED. ) ;
#9015 = ORIENTED_EDGE ( 'NONE', *, *, #12328, .F. ) ;
#9016 = CARTESIAN_POINT ( 'NONE',  ( 0.9756950546413942771, 11.01205619898776611, -41.47131842451888417 ) ) ;
#9017 = DIRECTION ( 'NONE',  ( 0.000000000000000000, 0.000000000000000000, 1.000000000000000000 ) ) ;
#9018 = CARTESIAN_POINT ( 'NONE',  ( -20.07366590805694173, -7.999991050865260966, -0.1389904710012628553 ) ) ;
#9019 = ORIENTED_EDGE ( 'NONE', *, *, #42404, .T. ) ;
#9020 = CARTESIAN_POINT ( 'NONE',  ( 4.960156602257182357, 25.36362146861383948, 38.88108289790868355 ) ) ;
#9021 = CARTESIAN_POINT ( 'NONE',  ( 2.281351352603293581, -42.18750813859374205, 22.83955855331502249 ) ) ;
#9022 = ORIENTED_EDGE ( 'NONE', *, *, #27947, .F. ) ;
#9023 = VECTOR ( 'NONE', #16272, 1000.000000000000114 ) ;
#9024 = CARTESIAN_POINT ( 'NONE',  ( 4.390527457369401532, -25.39775462712438170, 35.84884093703730201 ) ) ;
#9025 = ORIENTED_EDGE ( 'NONE', *, *, #22448, .T. ) ;
#9026 = CARTESIAN_POINT ( 'NONE',  ( 53.01412262506746487, 15.47721078833569841, -0.8552660025069994676 ) ) ;
#9027 = CIRCLE ( 'NONE', #50043, 44.12552607296456131 ) ;
#9028 = CARTESIAN_POINT ( 'NONE',  ( 0.3622758884714600280, -43.10531414739104861, -0.8252992914326565677 ) ) ;
#9029 = ORIENTED_EDGE ( 'NONE', *, *, #27026, .T. ) ;
#9030 = CARTESIAN_POINT ( 'NONE',  ( 1.227938101723756947, -22.18841447410693846, -36.73927144310534487 ) ) ;
#9031 = CARTESIAN_POINT ( 'NONE',  ( -6.077587904424778920, -14.65844225831500225, -12.48703695652317158 ) ) ;
#9032 = CARTESIAN_POINT ( 'NONE',  ( 0.9730545539215883499, 21.01499094264548972, 37.40983423658480689 ) ) ;
#9033 = CARTESIAN_POINT ( 'NONE',  ( -6.078726893082806448, 19.09748444646209009, -2.465791776662926260 ) ) ;
#9034 = EDGE_CURVE ( 'NONE', #19218, #60297, #31757, .T. ) ;
#9035 = ORIENTED_EDGE ( 'NONE', *, *, #42959, .F. ) ;
#9036 = ADVANCED_FACE ( 'NONE', ( #18004 ), #55897, .F. ) ;
#9037 = CARTESIAN_POINT ( 'NONE',  ( 0.9789233960466703355, -6.840937495575606597, -41.34656335191559862 ) ) ;
#9038 = ORIENTED_EDGE ( 'NONE', *, *, #46850, .F. ) ;
#9039 = LINE ( 'NONE', #42894, #20173 ) ;
#9040 = ORIENTED_EDGE ( 'NONE', *, *, #7979, .F. ) ;
#9041 = EDGE_CURVE ( 'NONE', #15197, #37408, #42738, .T. ) ;
#9042 = VERTEX_POINT ( 'NONE', #19239 ) ;
#9043 = CARTESIAN_POINT ( 'NONE',  ( -6.016761891674564211, 13.32657647165355286, 13.32172022638596509 ) ) ;
#9044 = CARTESIAN_POINT ( 'NONE',  ( 0.6030672727741701600, -34.07876014368883943, 33.95535904584727405 ) ) ;
#9045 = B_SPLINE_CURVE_WITH_KNOTS ( 'NONE', 3,
 ( #955, #10997, #45143, #40147 ),
 .UNSPECIFIED., .F., .F.,
 ( 4, 4 ),
 ( 1.734723475976807094E-18, 0.004042984057420977162 ),
 .UNSPECIFIED. ) ;
#9046 = CARTESIAN_POINT ( 'NONE',  ( 5.895881250540457863, 10.82621851909546606, -16.95053610317665616 ) ) ;
#9047 = CARTESIAN_POINT ( 'NONE',  ( 1.296416391601052931, -28.33827876547036340, -33.75276774853657002 ) ) ;
#9048 = ORIENTED_EDGE ( 'NONE', *, *, #31687, .F. ) ;
#9049 = CARTESIAN_POINT ( 'NONE',  ( 0.6845945791218023269, 11.71498854670038803, 45.42208233959143371 ) ) ;
#9050 = CARTESIAN_POINT ( 'NONE',  ( 0.3676999524040366896, -42.87209381266877983, -10.38913641457107673 ) ) ;
#9051 = B_SPLINE_CURVE_WITH_KNOTS ( 'NONE', 3,
 ( #47774, #19271, #4820, #51212, #18350, #37462 ),
 .UNSPECIFIED., .F., .F.,
 ( 4, 2, 4 ),
 ( 8.673617379884035472E-19, 0.0002291966416970791869, 0.0004583932833941575065 ),
 .UNSPECIFIED. ) ;
#9052 = FACE_OUTER_BOUND ( 'NONE', #54405, .T. ) ;
#9053 = ORIENTED_EDGE ( 'NONE', *, *, #53430, .F. ) ;
#9054 =( BOUNDED_SURFACE ( )  B_SPLINE_SURFACE ( 3, 1, ( 
 ( #37297, #42009 ),
 ( #61070, #42313 ),
 ( #18184, #47012 ),
 ( #51674, #8770 ) ),
 .UNSPECIFIED., .F., .F., .F. ) 
 B_SPLINE_SURFACE_WITH_KNOTS ( ( 4, 4 ),
 ( 2, 2 ),
 ( 0.000000000000000000, 1.000000000000000000 ),
 ( 0.000000000000000000, 1.000000000000000000 ),
 .UNSPECIFIED. ) 
 GEOMETRIC_REPRESENTATION_ITEM ( )  RATIONAL_B_SPLINE_SURFACE ( (
 ( 1.000000000000000000, 1.000000000000000000),
 ( 0.9732289882329797637, 0.9999525324661233672),
 ( 0.9732289882329797637, 0.9999525324661233672),
 ( 1.000000000000000000, 1.000000000000000000) ) ) 
 REPRESENTATION_ITEM ( '' )  SURFACE ( )  );
#9055 = EDGE_LOOP ( 'NONE', ( #29051, #3381, #40249, #58939 ) ) ;
#9056 = CARTESIAN_POINT ( 'NONE',  ( 0.1102144999581333301, -21.45299314243968070, -37.40973521037455640 ) ) ;
#9057 = CARTESIAN_POINT ( 'NONE',  ( -6.063463321072278589, -11.00428472829034199, -15.80272666656567182 ) ) ;
#9058 = CARTESIAN_POINT ( 'NONE',  ( 4.963659409799328515, -33.96111158240268679, 29.14784479683099860 ) ) ;
#9059 = CARTESIAN_POINT ( 'NONE',  ( 1.154321485836934391, -26.77578840293013940, -33.53917069757678604 ) ) ;
#9060 = EDGE_CURVE ( 'NONE', #25214, #51700, #6297, .T. ) ;
#9061 = B_SPLINE_CURVE_WITH_KNOTS ( 'NONE', 3,
 ( #46028, #3066, #36006, #12195, #50380, #2757 ),
 .UNSPECIFIED., .F., .F.,
 ( 4, 2, 4 ),
 ( 7.006328859705253345E-18, 0.0002291472222819953208, 0.0004582944445639836484 ),
 .UNSPECIFIED. ) ;
#9062 = ORIENTED_EDGE ( 'NONE', *, *, #4798, .T. ) ;
#9063 = EDGE_CURVE ( 'NONE', #23007, #8551, #28748, .T. ) ;
#9064 = CARTESIAN_POINT ( 'NONE',  ( 4.335381028904201628, -21.75407475222759146, 43.89210725561986948 ) ) ;
#9065 = CARTESIAN_POINT ( 'NONE',  ( 48.74902663329513786, 15.37135949308304816, 1.996608280103705058 ) ) ;
#9066 = CARTESIAN_POINT ( 'NONE',  ( 2.009741617377216460, -39.02673983696633542, -20.40631410423721448 ) ) ;
#9067 = CARTESIAN_POINT ( 'NONE',  ( 4.963659409799330291, 44.68724496494573373, -2.450325214228551651 ) ) ;
#9068 = ADVANCED_FACE ( 'NONE', ( #14539 ), #47502, .F. ) ;
#9069 = CARTESIAN_POINT ( 'NONE',  ( 4.963659409799332067, 33.33129552235085669, 29.86601237216419236 ) ) ;
#9070 =( BOUNDED_SURFACE ( )  B_SPLINE_SURFACE ( 3, 1, ( 
 ( #9734, #43278 ),
 ( #33562, #57026 ),
 ( #61710, #23223 ),
 ( #32948, #14453 ) ),
 .UNSPECIFIED., .F., .F., .F. ) 
 B_SPLINE_SURFACE_WITH_KNOTS ( ( 4, 4 ),
 ( 2, 2 ),
 ( 0.000000000000000000, 1.000000000000000000 ),
 ( 0.000000000000000000, 1.000000000000000000 ),
 .UNSPECIFIED. ) 
 GEOMETRIC_REPRESENTATION_ITEM ( )  RATIONAL_B_SPLINE_SURFACE ( (
 ( 1.000000000000000000, 1.000000000000000000),
 ( 0.9952954269826590483, 0.8620686068821339365),
 ( 0.9952954269826590483, 0.8620686068821339365),
 ( 1.000000000000000000, 1.000000000000000000) ) ) 
 REPRESENTATION_ITEM ( '' )  SURFACE ( )  );
#9071 = ORIENTED_EDGE ( 'NONE', *, *, #35173, .T. ) ;
#9072 = CARTESIAN_POINT ( 'NONE',  ( 2.500000000000000000, 1.768423874527822459, -1.021000000000002794 ) ) ;
#9073 = CARTESIAN_POINT ( 'NONE',  ( 0.5809828226811553087, 47.89273459658653564, -0.5448590168534052092 ) ) ;
#9074 = B_SPLINE_CURVE_WITH_KNOTS ( 'NONE', 3,
 ( #53053, #49280, #10155, #57739, #24562, #48365 ),
 .UNSPECIFIED., .F., .F.,
 ( 4, 2, 4 ),
 ( 9.341771812940338307E-18, 0.0002291978881530158348, 0.0004583957763060222913 ),
 .UNSPECIFIED. ) ;
#9075 = CARTESIAN_POINT ( 'NONE',  ( 2.624215991343608501, 47.39206852872457887, 7.662883702704825772 ) ) ;
#9076 = B_SPLINE_CURVE_WITH_KNOTS ( 'NONE', 3,
 ( #7110, #23023, #27711, #2422, #21548, #16866 ),
 .UNSPECIFIED., .F., .F.,
 ( 4, 2, 4 ),
 ( 0.002336974151641539946, 0.003500975885716448889, 0.004664977619791357832 ),
 .UNSPECIFIED. ) ;
#9077 = CARTESIAN_POINT ( 'NONE',  ( 4.960156602257182357, -45.62767441207056862, 8.553784487772720269 ) ) ;
#9078 = CARTESIAN_POINT ( 'NONE',  ( 0.9762797500689124330, 28.76866969767982951, 30.47438972336447804 ) ) ;
#9079 = CARTESIAN_POINT ( 'NONE',  ( 4.549368137175248350, -35.57418903283098643, -24.02461520945259466 ) ) ;
#9080 = ADVANCED_FACE ( 'NONE', ( #14234 ), #25906, .F. ) ;
#9081 = CARTESIAN_POINT ( 'NONE',  ( 0.5786265663353196143, -46.07681357296475255, -13.09387673186383516 ) ) ;
#9082 = DIRECTION ( 'NONE',  ( -1.000000000000000000, -0.000000000000000000, -0.000000000000000000 ) ) ;
#9083 = CARTESIAN_POINT ( 'NONE',  ( 3.344563996438205677, 2.687817229851463097, -0.1586754815284831532 ) ) ;
#9084 = EDGE_LOOP ( 'NONE', ( #51733, #47873, #37640, #53233 ) ) ;
#9085 = CARTESIAN_POINT ( 'NONE',  ( 4.553261556744875094, 0.000000000000000000, 0.000000000000000000 ) ) ;
#9086 = CARTESIAN_POINT ( 'NONE',  ( 5.959547316686252039, 17.77392908783919978, 10.26589671991369457 ) ) ;
#9087 = DIRECTION ( 'NONE',  ( -1.000000000000000000, -0.000000000000000000, -0.000000000000000000 ) ) ;
#9088 = FACE_OUTER_BOUND ( 'NONE', #32004, .T. ) ;
#9089 = ORIENTED_EDGE ( 'NONE', *, *, #13073, .F. ) ;
#9090 = CARTESIAN_POINT ( 'NONE',  ( 0.5800708119828336118, -46.09746484493488339, 13.00144522946642489 ) ) ;
#9091 = FACE_OUTER_BOUND ( 'NONE', #17758, .T. ) ;
#9092 = B_SPLINE_CURVE_WITH_KNOTS ( 'NONE', 3,
 ( #46469, #32673, #37079, #56147, #46785, #56451 ),
 .UNSPECIFIED., .F., .F.,
 ( 4, 2, 4 ),
 ( 9.543442895606953578E-18, 0.0002291978881530148048, 0.0004583957763060200687 ),
 .UNSPECIFIED. ) ;
#9093 = B_SPLINE_CURVE_WITH_KNOTS ( 'NONE', 3,
 ( #50187, #45510, #46431, #2560, #55485, #21681, #40824, #8187, #12612, #31705, #60802, #3476, #46129, #50794, #17000, #3175 ),
 .UNSPECIFIED., .F., .F.,
 ( 4, 3, 3, 3, 3, 4 ),
 ( 1.250973872328959318E-17, 0.0002732102107931876143, 0.0004098135523333815882, 0.0005464168938824977327, 0.0008195847345945442026, 0.001092771384553106132 ),
 .UNSPECIFIED. ) ;
#9094 = VERTEX_POINT ( 'NONE', #5701 ) ;
#9095 = CARTESIAN_POINT ( 'NONE',  ( 3.782542959838397056, -5.285775259587299324, -41.70489699425842645 ) ) ;
#9096 = CARTESIAN_POINT ( 'NONE',  ( 0.5824935313925956315, -46.02748767734610880, -8.983794029561840588 ) ) ;
#9097 = LINE ( 'NONE', #28206, #17938 ) ;
#9098 = VERTEX_POINT ( 'NONE', #33343 ) ;
#9099 = CARTESIAN_POINT ( 'NONE',  ( 4.975610109902397937, 13.36434394399692316, 47.05150069959858428 ) ) ;
#9100 = ORIENTED_EDGE ( 'NONE', *, *, #49370, .F. ) ;
#9101 = VERTEX_POINT ( 'NONE', #392 ) ;
#9102 = CARTESIAN_POINT ( 'NONE',  ( 0.5837374860065638327, -6.431731162805466084, -47.46223477511620104 ) ) ;
#9103 = CARTESIAN_POINT ( 'NONE',  ( 0.8753041380234530822, -48.57841546934886168, 7.160717726618431200 ) ) ;
#9104 = EDGE_CURVE ( 'NONE', #22095, #22251, #38658, .T. ) ;
#9105 = VERTEX_POINT ( 'NONE', #14841 ) ;
#9106 = CARTESIAN_POINT ( 'NONE',  ( -16.60577576646023346, 5.000000000000006217, 4.095239503579248533E-30 ) ) ;
#9107 = ORIENTED_EDGE ( 'NONE', *, *, #12328, .T. ) ;
#9108 = ADVANCED_FACE ( 'NONE', ( #19854 ), #34217, .F. ) ;
#9109 = DIRECTION ( 'NONE',  ( -1.000000000000000000, -0.000000000000000000, -0.000000000000000000 ) ) ;
#9110 = CARTESIAN_POINT ( 'NONE',  ( 1.154321713695928286, 0.8253077511132634880, -42.90848032340444007 ) ) ;
#9111 = CARTESIAN_POINT ( 'NONE',  ( 3.259860905586184021, 10.22135424391044012, 4.719314477116953545E-16 ) ) ;
#9112 = ADVANCED_FACE ( 'NONE', ( #20454 ), #30284, .F. ) ;
#9113 = ORIENTED_EDGE ( 'NONE', *, *, #15254, .F. ) ;
#9114 = EDGE_CURVE ( 'NONE', #28847, #31387, #58453, .T. ) ;
#9115 = CARTESIAN_POINT ( 'NONE',  ( 5.895881250540457863, 20.06826253866637444, -1.338850360369210568 ) ) ;
#9116 = DIRECTION ( 'NONE',  ( -0.9990097760809876215, 0.000000000000000000, 0.04449120468828354769 ) ) ;
#9117 = CARTESIAN_POINT ( 'NONE',  ( 5.981074661064941900, 2.670494474391997386, -20.35019299530686254 ) ) ;
#9118 = CARTESIAN_POINT ( 'NONE',  ( -6.077587904424778920, 3.079371755031420133, 19.00824797261034149 ) ) ;
#9120 = EDGE_CURVE ( 'NONE', #8619, #2209, #1629, .T. ) ;
#9119 = ORIENTED_EDGE ( 'NONE', *, *, #44109, .F. ) ;
#9121 = CARTESIAN_POINT ( 'NONE',  ( 0.5809828226811544205, -34.25055090842130312, -33.48000389720652947 ) ) ;
#9122 = CARTESIAN_POINT ( 'NONE',  ( 0.1147471544378677183, -31.91187174540620930, -30.47268662553386775 ) ) ;
#9123 = EDGE_LOOP ( 'NONE', ( #47938, #5609 ) ) ;
#9124 = CARTESIAN_POINT ( 'NONE',  ( 0.5824935313925970748, 43.03132588641753387, -18.64250974281010897 ) ) ;
#9125 = ORIENTED_EDGE ( 'NONE', *, *, #42028, .F. ) ;
#9126 = CARTESIAN_POINT ( 'NONE',  ( 4.549368137175248350, 8.582197505783829783, 42.06008734272398897 ) ) ;
#9127 = ADVANCED_FACE ( 'NONE', ( #39583 ), #21510, .F. ) ;
#9128 = CARTESIAN_POINT ( 'NONE',  ( 0.6026777506516368677, 46.55057256863531734, -15.63939206521266279 ) ) ;
#9129 = ORIENTED_EDGE ( 'NONE', *, *, #2251, .T. ) ;
#9130 = CARTESIAN_POINT ( 'NONE',  ( 0.1313383488274124933, -37.66088038379825775, -21.00709374781526861 ) ) ;
#9131 = CARTESIAN_POINT ( 'NONE',  ( 1.227938101723748288, 4.762198645644436290, 42.65467462194920500 ) ) ;
#9132 = CYLINDRICAL_SURFACE ( 'NONE', #51717, 6.887500000000022382 ) ;
#9133 = CARTESIAN_POINT ( 'NONE',  ( 3.678834586032787790, -3.416869612372130049, 48.85629306118508453 ) ) ;
#9134 = EDGE_CURVE ( 'NONE', #2574, #17781, #17598, .T. ) ;
#9135 = ORIENTED_EDGE ( 'NONE', *, *, #48508, .F. ) ;
#9136 = LINE ( 'NONE', #37992, #43980 ) ;
#9137 = DIRECTION ( 'NONE',  ( 1.000000000000000000, 1.836909530733573776E-16, 0.000000000000000000 ) ) ;
#9138 = FACE_OUTER_BOUND ( 'NONE', #14138, .T. ) ;
#9139 = CARTESIAN_POINT ( 'NONE',  ( 0.8554163680231708922, -26.01084021241273092, 39.04666009476548538 ) ) ;
#9140 = B_SPLINE_CURVE_WITH_KNOTS ( 'NONE', 3,
 ( #4645, #23796, #28176, #42608, #56981, #42922, #19115, #38227, #14409, #33516 ),
 .UNSPECIFIED., .F., .F.,
 ( 4, 3, 3, 4 ),
 ( 0.0005236741812378729226, 0.0005236998216949948978, 0.0007855159896329592158, 0.001047349442285928304 ),
 .UNSPECIFIED. ) ;
#9141 = CARTESIAN_POINT ( 'NONE',  ( 0.3622758884714600280, -6.444611261694905835, 42.62881903538198713 ) ) ;
#9142 = CARTESIAN_POINT ( 'NONE',  ( 0.5807400328401574052, 37.66660715020906736, -29.58941477092977124 ) ) ;
#9143 = DIRECTION ( 'NONE',  ( -1.000000000000000000, -0.000000000000000000, -0.000000000000000000 ) ) ;
#9144 = DIRECTION ( 'NONE',  ( -0.1024043820194934507, -0.7811075516170038480, -0.6159418278945628655 ) ) ;
#9145 = CARTESIAN_POINT ( 'NONE',  ( 50.50000000000000000, 15.27178771460631168, -2.649999999999992806 ) ) ;
#9146 = CARTESIAN_POINT ( 'NONE',  ( 0.9730545539215892381, 25.71816799638828499, -34.34678117142529175 ) ) ;
#9147 = CARTESIAN_POINT ( 'NONE',  ( 0.9757892942422822236, 30.30456399643835042, -30.37715353261962647 ) ) ;
#9148 = EDGE_CURVE ( 'NONE', #45060, #25025, #40513, .T. ) ;
#9149 = CARTESIAN_POINT ( 'NONE',  ( 4.962356264823608143, 0.000000000000000000, 0.000000000000000000 ) ) ;
#9150 = CARTESIAN_POINT ( 'NONE',  ( 0.5804410086790514622, 46.40460073163232835, -6.792119168064279400 ) ) ;
#9151 = CIRCLE ( 'NONE', #25157, 43.08621763946400307 ) ;
#9152 = CARTESIAN_POINT ( 'NONE',  ( 0.7048096507298635682, -38.67623024744029436, -28.61383451045685078 ) ) ;
#9153 = CARTESIAN_POINT ( 'NONE',  ( 0.5809828226811617480, -29.58751527316205809, 37.66417181417541826 ) ) ;
#9154 = ADVANCED_FACE ( 'NONE', ( #20766 ), #40639, .F. ) ;
#9155 = CARTESIAN_POINT ( 'NONE',  ( 0.9754402186311948997, -37.25324696807214764, -21.29160191075036224 ) ) ;
#9156 = FILL_AREA_STYLE ('',( #50 ) ) ;
#9157 = CARTESIAN_POINT ( 'NONE',  ( 0.6039202388192952409, -48.72646899558821332, 6.106957677188616707 ) ) ;
#9159 = ORIENTED_EDGE ( 'NONE', *, *, #8320, .F. ) ;
#9158 = CARTESIAN_POINT ( 'NONE',  ( 0.5806925824938502512, 43.38503874128546300, 17.80339225430713057 ) ) ;
#9160 = CARTESIAN_POINT ( 'NONE',  ( 5.896278296736517710, -18.51475911848199374, 7.856887067978758132 ) ) ;
#9161 = CARTESIAN_POINT ( 'NONE',  ( 0.8760168074887090262, -46.22580377597795120, 13.30888447661999940 ) ) ;
#9162 = LINE ( 'NONE', #3833, #4660 ) ;
#9163 = VERTEX_POINT ( 'NONE', #30450 ) ;
#9164 = CARTESIAN_POINT ( 'NONE',  ( 0.5827357941260207230, -33.60975216782508568, 34.12346967353447269 ) ) ;
#9165 = UNCERTAINTY_MEASURE_WITH_UNIT (LENGTH_MEASURE( 1.000000000000000082E-05 ), #26832, 'distance_accuracy_value', 'NONE');
#9166 = EDGE_LOOP ( 'NONE', ( #13444, #4647 ) ) ;
#9167 = ORIENTED_EDGE ( 'NONE', *, *, #7224, .T. ) ;
#9168 =( BOUNDED_SURFACE ( )  B_SPLINE_SURFACE ( 3, 1, ( 
 ( #37787, #4208 ),
 ( #42175, #18354 ),
 ( #37466, #33076 ),
 ( #32759, #56842 ) ),
 .UNSPECIFIED., .F., .F., .F. ) 
 B_SPLINE_SURFACE_WITH_KNOTS ( ( 4, 4 ),
 ( 2, 2 ),
 ( 0.000000000000000000, 1.000000000000000000 ),
 ( 0.000000000000000000, 1.000000000000000000 ),
 .UNSPECIFIED. ) 
 GEOMETRIC_REPRESENTATION_ITEM ( )  RATIONAL_B_SPLINE_SURFACE ( (
 ( 1.000000000000000000, 1.000000000000000000),
 ( 0.9953485035131437453, 0.8621029689291515030),
 ( 0.9953485035131437453, 0.8621029689291515030),
 ( 1.000000000000000000, 1.000000000000000000) ) ) 
 REPRESENTATION_ITEM ( '' )  SURFACE ( )  );
#9169 = CARTESIAN_POINT ( 'NONE',  ( 0.9752132459055850022, -11.33038172416123679, -41.38545930839059395 ) ) ;
#9170 = ORIENTED_EDGE ( 'NONE', *, *, #2966, .T. ) ;
#9171 = CARTESIAN_POINT ( 'NONE',  ( 7.000000000000016875, -58.44237546506767700, -54.69470952477997372 ) ) ;
#9172 = CARTESIAN_POINT ( 'NONE',  ( 0.9745511491811756910, -41.53317535253980708, 10.77620558745922352 ) ) ;
#9173 = B_SPLINE_CURVE_WITH_KNOTS ( 'NONE', 3,
 ( #3430, #36072, #45773, #42004, #31971, #55131 ),
 .UNSPECIFIED., .F., .F.,
 ( 4, 2, 4 ),
 ( 1.870625823323990238E-17, 0.0002293755540694308035, 0.0004587511081388429045 ),
 .UNSPECIFIED. ) ;
#9174 = VERTEX_POINT ( 'NONE', #35494 ) ;
#9175 = ORIENTED_EDGE ( 'NONE', *, *, #40466, .F. ) ;
#9176 = CARTESIAN_POINT ( 'NONE',  ( 0.5837374860065638327, -12.57177159055130389, -46.21667939904229172 ) ) ;
#9177 = ORIENTED_EDGE ( 'NONE', *, *, #52825, .T. ) ;
#9178 = CARTESIAN_POINT ( 'NONE',  ( 4.967162193818130511, 32.10009971360111791, -28.74031574029977776 ) ) ;
#9179 = CARTESIAN_POINT ( 'NONE',  ( 2.643462169533600914, -28.13401304854693663, -38.93558293168531037 ) ) ;
#9180 = CARTESIAN_POINT ( 'NONE',  ( 0.1100247026804066219, -30.37337782329870350, -30.61332956994571575 ) ) ;
#9181 = ORIENTED_EDGE ( 'NONE', *, *, #235, .F. ) ;
#9182 = ADVANCED_FACE ( 'NONE', ( #15451 ), #24848, .F. ) ;
#9183 = DIRECTION ( 'NONE',  ( 0.000000000000000000, 0.000000000000000000, 1.000000000000000000 ) ) ;
#9184 = CARTESIAN_POINT ( 'NONE',  ( 0.9785694773339257413, -39.66226175059299663, 13.53663172809687332 ) ) ;
#9185 = ADVANCED_FACE ( 'NONE', ( #26078 ), #54232, .F. ) ;
#9186 = ORIENTED_EDGE ( 'NONE', *, *, #52351, .F. ) ;
#9187 = ORIENTED_EDGE ( 'NONE', *, *, #32181, .F. ) ;
#9189 = ADVANCED_FACE ( 'NONE', ( #2250 ), #1945, .T. ) ;
#9188 = B_SPLINE_CURVE_WITH_KNOTS ( 'NONE', 3,
 ( #10758, #29848, #44596, #20770 ),
 .UNSPECIFIED., .F., .F.,
 ( 4, 4 ),
 ( 9.697399036122160616E-19, 0.004050076154992999014 ),
 .UNSPECIFIED. ) ;
#9190 = CARTESIAN_POINT ( 'NONE',  ( 0.5850706913938534814, -44.18063951072233664, 18.49682194437948723 ) ) ;
#9191 = ORIENTED_EDGE ( 'NONE', *, *, #54584, .F. ) ;
#9192 = CARTESIAN_POINT ( 'NONE',  ( 3.559346040607745287, 34.77628641160756473, 26.90799481492122069 ) ) ;
#9193 = CARTESIAN_POINT ( 'NONE',  ( -6.015611763856276717, -2.465697960551179513, 18.68122482568278997 ) ) ;
#9194 = LINE ( 'NONE', #14226, #10642 ) ;
#9195 = EDGE_CURVE ( 'NONE', #6486, #21289, #7814, .T. ) ;
#9196 = DIRECTION ( 'NONE',  ( 0.000000000000000000, -1.047444401652941269E-14, 1.000000000000000000 ) ) ;
#9197 = DIRECTION ( 'NONE',  ( 0.000000000000000000, 0.000000000000000000, 1.000000000000000000 ) ) ;
#9198 = EDGE_LOOP ( 'NONE', ( #61449, #54592, #49997, #27287 ) ) ;
#9199 = CARTESIAN_POINT ( 'NONE',  ( -5.995132425357893702, -4.869002713216700862, 18.20425902871266288 ) ) ;
#9200 = VECTOR ( 'NONE', #57976, 999.9999999999998863 ) ;
#9201 = DIRECTION ( 'NONE',  ( 0.000000000000000000, 0.000000000000000000, -1.000000000000000000 ) ) ;
#9202 = AXIS2_PLACEMENT_3D ( 'NONE', #32772, #8949, #3000 ) ;
#9203 = CARTESIAN_POINT ( 'NONE',  ( 0.5837800005270550319, 36.80393597436502517, -29.06381866576765205 ) ) ;
#9204 = ORIENTED_EDGE ( 'NONE', *, *, #2279, .F. ) ;
#9205 = CARTESIAN_POINT ( 'NONE',  ( 0.5806925824938499181, -42.09901922557445175, 20.66143612114793626 ) ) ;
#9206 = CARTESIAN_POINT ( 'NONE',  ( -69.95594261585601714, 0.000000000000000000, 0.000000000000000000 ) ) ;
#9207 = CARTESIAN_POINT ( 'NONE',  ( 0.5997462898726536595, 49.03735788587799505, 2.624721264559015221 ) ) ;
#9208 = VERTEX_POINT ( 'NONE', #60196 ) ;
#9209 = EDGE_LOOP ( 'NONE', ( #30149, #13529, #33866, #6800 ) ) ;
#9210 = CARTESIAN_POINT ( 'NONE',  ( 5.901764892641288895, -44.13851569553263943, -21.20808571358803363 ) ) ;
#9211 = CARTESIAN_POINT ( 'NONE',  ( 0.1095718737110178836, -42.78833451865671123, 5.374020908746216740 ) ) ;
#9212 = CARTESIAN_POINT ( 'NONE',  ( -1.600000000000000089, -11.64055411052240352, 0.000000000000000000 ) ) ;
#9213 = CARTESIAN_POINT ( 'NONE',  ( 0.3676999524040323597, 43.13409918076290950, 9.241215893319909114 ) ) ;
#9214 = DIRECTION ( 'NONE',  ( 0.09835009131224552170, -0.7941905447268777785, -0.5996571005210378225 ) ) ;
#9215 = CARTESIAN_POINT ( 'NONE',  ( -6.001507490154111224, -4.892199142591432626, 18.19774963328906736 ) ) ;
#9216 = CARTESIAN_POINT ( 'NONE',  ( 0.9722240750034599754, -21.95618656573978456, -36.86535092060696428 ) ) ;
#9217 = CARTESIAN_POINT ( 'NONE',  ( 3.238018933889920792, 13.39148516828231372, -0.2749861002446565839 ) ) ;
#9218 = DIRECTION ( 'NONE',  ( 0.000000000000000000, 0.000000000000000000, 1.000000000000000000 ) ) ;
#9219 = CARTESIAN_POINT ( 'NONE',  ( 4.960156602257182357, -9.558288641082077319, 45.42786611289310628 ) ) ;
#9220 = CARTESIAN_POINT ( 'NONE',  ( 4.322998006666179727, -4.155494336619063311, 47.80838462754057616 ) ) ;
#9221 = CARTESIAN_POINT ( 'NONE',  ( 0.5807400328401574052, 12.92266817606014762, 46.12278621143501312 ) ) ;
#9222 = EDGE_LOOP ( 'NONE', ( #6535, #46586 ) ) ;
#9223 = CARTESIAN_POINT ( 'NONE',  ( -2.601141883200662974, -3.815535891688014214, 14.43042318605484198 ) ) ;
#9224 = CARTESIAN_POINT ( 'NONE',  ( 0.1073791018717483448, -34.50606437925530656, -25.86618856530698451 ) ) ;
#9225 = CARTESIAN_POINT ( 'NONE',  ( 0.2500000000000002220, 5.204748896376250699E-16, -4.250000000000000000 ) ) ;
#9226 = CARTESIAN_POINT ( 'NONE',  ( 3.238018933889920792, -9.747366695765240507, -9.186747785040122238 ) ) ;
#9227 = CARTESIAN_POINT ( 'NONE',  ( 4.956445790444029775, 25.79263028817611314, -39.39896284113449809 ) ) ;
#9228 = DIRECTION ( 'NONE',  ( 0.000000000000000000, 0.000000000000000000, 1.000000000000000000 ) ) ;
#9229 = CONTEXT_DEPENDENT_SHAPE_REPRESENTATION ( #753, #9836 ) ;
#9230 = DIRECTION ( 'NONE',  ( 0.000000000000000000, 0.000000000000000000, 1.000000000000000000 ) ) ;
#9231 = EDGE_CURVE ( 'NONE', #3027, #51786, #36424, .T. ) ;
#9232 = DIRECTION ( 'NONE',  ( 1.000000000000000000, 1.836909530733573776E-16, -1.925929944387235853E-32 ) ) ;
#9233 = CARTESIAN_POINT ( 'NONE',  ( 3.680974057930773924, -43.58300585207908995, -20.05478739720721038 ) ) ;
#9235 = ORIENTED_EDGE ( 'NONE', *, *, #29359, .F. ) ;
#9234 = CARTESIAN_POINT ( 'NONE',  ( 2.301430502907645170, 4.990893951996359768, 47.77346269870101736 ) ) ;
#9236 = ORIENTED_EDGE ( 'NONE', *, *, #4093, .T. ) ;
#9237 = CARTESIAN_POINT ( 'NONE',  ( 0.8557997880470697982, -37.44587306708118035, 29.88293891557457371 ) ) ;
#9238 = CARTESIAN_POINT ( 'NONE',  ( 0.5987334308729320709, 49.04182532646215265, 2.542100552398203650 ) ) ;
#9239 = CARTESIAN_POINT ( 'NONE',  ( 0.8551540677456739292, 33.23105123575900421, 34.52115452272940388 ) ) ;
#9240 = VERTEX_POINT ( 'NONE', #3184 ) ;
#9241 = CARTESIAN_POINT ( 'NONE',  ( 4.975610109902397937, 0.000000000000000000, 0.000000000000000000 ) ) ;
#9242 = CARTESIAN_POINT ( 'NONE',  ( 1.827119703190779765, -4.394694966566802030, 42.82501615430323483 ) ) ;
#9243 = CARTESIAN_POINT ( 'NONE',  ( 0.6017667736363749853, -44.31084570541189294, -18.73201910948646542 ) ) ;
#9244 =( BOUNDED_SURFACE ( )  B_SPLINE_SURFACE ( 3, 1, ( 
 ( #54733, #15936 ),
 ( #20327, #2106 ),
 ( #20934, #25941 ),
 ( #49428, #40078 ) ),
 .UNSPECIFIED., .F., .F., .F. ) 
 B_SPLINE_SURFACE_WITH_KNOTS ( ( 4, 4 ),
 ( 2, 2 ),
 ( 0.000000000000000000, 1.000000000000000000 ),
 ( 0.000000000000000000, 1.000000000000000000 ),
 .UNSPECIFIED. ) 
 GEOMETRIC_REPRESENTATION_ITEM ( )  RATIONAL_B_SPLINE_SURFACE ( (
 ( 1.000000000000000000, 1.000000000000000000),
 ( 0.9953485035131437453, 0.8621029689291515030),
 ( 0.9953485035131437453, 0.8621029689291515030),
 ( 1.000000000000000000, 1.000000000000000000) ) ) 
 REPRESENTATION_ITEM ( '' )  SURFACE ( )  );
#9245 = ORIENTED_EDGE ( 'NONE', *, *, #48043, .T. ) ;
#9246 = VERTEX_POINT ( 'NONE', #3482 ) ;
#9247 = LINE ( 'NONE', #47479, #4296 ) ;
#9248 = CARTESIAN_POINT ( 'NONE',  ( 3.050102900204245682, -40.06446576558427353, 18.17316241319562309 ) ) ;
#9249 = CARTESIAN_POINT ( 'NONE',  ( 4.549368137175248350, -40.58005590356681580, -13.99871866169351442 ) ) ;
#9250 = EDGE_CURVE ( 'NONE', #56285, #10350, #54176, .T. ) ;
#9251 = FACE_OUTER_BOUND ( 'NONE', #6060, .T. ) ;
#9252 = B_SPLINE_CURVE_WITH_KNOTS ( 'NONE', 3,
 ( #25301, #15613, #44448, #5857, #20310, #30002 ),
 .UNSPECIFIED., .F., .F.,
 ( 4, 2, 4 ),
 ( 6.938893903907228378E-18, 0.0002291472222819913905, 0.0004582944445639758422 ),
 .UNSPECIFIED. ) ;
#9253 = EDGE_CURVE ( 'NONE', #37333, #59587, #19057, .T. ) ;
#9254 = B_SPLINE_CURVE_WITH_KNOTS ( 'NONE', 3,
 ( #9592, #47211, #47833, #23704 ),
 .UNSPECIFIED., .F., .F.,
 ( 4, 4 ),
 ( 2.153172013482225773E-17, 0.004559932413162188537 ),
 .UNSPECIFIED. ) ;
#9255 = B_SPLINE_CURVE_WITH_KNOTS ( 'NONE', 3,
 ( #3965, #50972, #18409, #13714, #12796, #61289, #36915, #23104, #18096, #37215, #41921, #37527, #55356, #51580, #7749, #60359, #32823, #12479, #55980 ),
 .UNSPECIFIED., .F., .F.,
 ( 4, 3, 3, 3, 3, 3, 4 ),
 ( 3.469446951953614189E-18, 0.0002732106629380679072, 0.0004098138914053798230, 0.0005464171197651472318, 0.0006830203481512555491, 0.0008196235766963701382, 0.001011968216111141161 ),
 .UNSPECIFIED. ) ;
#9256 = CARTESIAN_POINT ( 'NONE',  ( 0.09136607875274982415, 0.000000000000000000, 10.00000000000000000 ) ) ;
#9257 = EDGE_CURVE ( 'NONE', #14998, #26349, #10499, .T. ) ;
#9258 = VERTEX_POINT ( 'NONE', #12619 ) ;
#9259 = CARTESIAN_POINT ( 'NONE',  ( 4.960386119450142850, -34.04466635746601355, 27.48448939458694795 ) ) ;
#9260 = CARTESIAN_POINT ( 'NONE',  ( 2.643462169533600914, -34.93025802711748895, 32.97543604874614687 ) ) ;
#9261 = EDGE_LOOP ( 'NONE', ( #5893, #39349, #34028, #50319 ) ) ;
#9262 = CARTESIAN_POINT ( 'NONE',  ( 0.9769922540276048117, -37.20286211167621104, -19.29452268872523391 ) ) ;
#9263 = CARTESIAN_POINT ( 'NONE',  ( 0.8557997880470599172, -47.89938907511592703, -0.9121262075951160897 ) ) ;
#9264 = EDGE_CURVE ( 'NONE', #26111, #22599, #13837, .T. ) ;
#9265 = CARTESIAN_POINT ( 'NONE',  ( 3.050102900204245682, 38.81779051020957638, -20.70276283696318131 ) ) ;
#9266 = CARTESIAN_POINT ( 'NONE',  ( 1.830465331921977024, -43.82878250349589422, 4.406118489060570020 ) ) ;
#9267 = ORIENTED_EDGE ( 'NONE', *, *, #38028, .F. ) ;
#9268 = ORIENTED_EDGE ( 'NONE', *, *, #53045, .F. ) ;
#9269 = FACE_OUTER_BOUND ( 'NONE', #14500, .T. ) ;
#9270 = CARTESIAN_POINT ( 'NONE',  ( 0.8753041380234465318, -47.26389509135280775, -13.31399822241900210 ) ) ;
#9271 = CARTESIAN_POINT ( 'NONE',  ( -6.078726893082806448, -6.653559303940109082, -18.06998035022927596 ) ) ;
#9272 = VERTEX_POINT ( 'NONE', #32641 ) ;
#9273 = CARTESIAN_POINT ( 'NONE',  ( 0.6024113833632038784, 4.932097281942475320, -48.85914740867182360 ) ) ;
#9274 = EDGE_LOOP ( 'NONE', ( #932, #8885, #18791, #61113 ) ) ;
#9275 = CARTESIAN_POINT ( 'NONE',  ( 3.894904216938898323, 43.51529871852972065, 6.208309746889793423 ) ) ;
#9276 = CARTESIAN_POINT ( 'NONE',  ( 4.962356264823608143, -41.65024625884313991, -6.040909239515997342 ) ) ;
#9277 = EDGE_CURVE ( 'NONE', #5799, #50136, #36966, .T. ) ;
#9278 = EDGE_LOOP ( 'NONE', ( #13579, #17920, #7734, #56591 ) ) ;
#9279 = B_SPLINE_CURVE_WITH_KNOTS ( 'NONE', 3,
 ( #43735, #52472, #52783, #29595 ),
 .UNSPECIFIED., .F., .F.,
 ( 4, 4 ),
 ( 0.000000000000000000, 0.004442905043737214836 ),
 .UNSPECIFIED. ) ;
#9280 = CARTESIAN_POINT ( 'NONE',  ( 0.5839254010752159552, -0.09079837481654944031, 47.89590033178485129 ) ) ;
#9281 = CARTESIAN_POINT ( 'NONE',  ( 0.9762797500689124330, -30.73989051779308568, -28.48480149377557424 ) ) ;
#9282 = EDGE_CURVE ( 'NONE', #45511, #17579, #59398, .T. ) ;
#9283 = DIRECTION ( 'NONE',  ( 1.000000000000000000, 0.000000000000000000, 0.000000000000000000 ) ) ;
#9284 = AXIS2_PLACEMENT_3D ( 'NONE', #2376, #59701, #16818 ) ;
#9285 = ORIENTED_EDGE ( 'NONE', *, *, #37599, .F. ) ;
#9286 = CARTESIAN_POINT ( 'NONE',  ( 0.1368894036331257669, 24.71813664103433794, -36.54962444291990664 ) ) ;
#9287 = CARTESIAN_POINT ( 'NONE',  ( 0.1129192098497447394, -43.69739906996321110, 6.122834499276631703 ) ) ;
#9288 = CARTESIAN_POINT ( 'NONE',  ( 4.962356264823608143, 0.000000000000000000, 0.000000000000000000 ) ) ;
#9289 = CARTESIAN_POINT ( 'NONE',  ( 4.335381028904201628, -36.63547605605852198, 32.52074325427246748 ) ) ;
#9290 = B_SPLINE_CURVE_WITH_KNOTS ( 'NONE', 3,
 ( #37553, #27509, #8094, #27206 ),
 .UNSPECIFIED., .F., .F.,
 ( 4, 4 ),
 ( 6.961759998889881502E-17, 0.005004741218457482189 ),
 .UNSPECIFIED. ) ;
#9291 = CARTESIAN_POINT ( 'NONE',  ( 0.1102847568649952675, 16.41780866919043191, -39.87696813145912245 ) ) ;
#9292 = ORIENTED_EDGE ( 'NONE', *, *, #50010, .F. ) ;
#9293 = CARTESIAN_POINT ( 'NONE',  ( -6.079354080745853928, 5.477739963082026264, -18.46042578449956295 ) ) ;
#9294 = CARTESIAN_POINT ( 'NONE',  ( 3.727782113643637096, -15.81964116771539608, 41.01849252752591468 ) ) ;
#9295 = ORIENTED_EDGE ( 'NONE', *, *, #33396, .T. ) ;
#9296 = LINE ( 'NONE', #28101, #23884 ) ;
#9297 = FACE_OUTER_BOUND ( 'NONE', #14210, .T. ) ;
#9298 = CARTESIAN_POINT ( 'NONE',  ( 0.8554163680231738898, -34.17638377241206626, -32.14312158693720534 ) ) ;
#9299 = CARTESIAN_POINT ( 'NONE',  ( 0.9754402186311948997, 5.414674803234379219, -42.56545569314703670 ) ) ;
#9300 = CARTESIAN_POINT ( 'NONE',  ( 2.643462169533613793, -25.20536747735751604, -40.89244134039102363 ) ) ;
#9301 = DIRECTION ( 'NONE',  ( 0.000000000000000000, 0.000000000000000000, 1.000000000000000000 ) ) ;
#9303 = B_SPLINE_CURVE_WITH_KNOTS ( 'NONE', 3,
 ( #8205, #4715, #4106, #14474, #28862, #8507 ),
 .UNSPECIFIED., .F., .F.,
 ( 4, 2, 4 ),
 ( 1.734723475976807094E-18, 0.0002447193893791677023, 0.0004894387787583336698 ),
 .UNSPECIFIED. ) ;
#9302 = CARTESIAN_POINT ( 'NONE',  ( 53.06470156691138129, 15.48560858660915507, 0.6891024955566218413 ) ) ;
#9304 = SURFACE_STYLE_FILL_AREA ( #10241 ) ;
#9305 = CARTESIAN_POINT ( 'NONE',  ( 0.5998501479064699549, 47.76154736470750350, 5.759754759340949271 ) ) ;
#9307 = ADVANCED_FACE ( 'NONE', ( #37662 ), #47030, .F. ) ;
#9306 = AXIS2_PLACEMENT_3D ( 'NONE', #30808, #35849, #2919 ) ;
#9308 = DIRECTION ( 'NONE',  ( -1.000000000000000000, -0.000000000000000000, -0.000000000000000000 ) ) ;
#9309 = B_SPLINE_CURVE_WITH_KNOTS ( 'NONE', 3,
 ( #60999, #18418, #38161, #28114, #37857, #51592, #37538, #47853, #18106, #8688, #4280, #56917, #37229, #56299, #43163, #42543, #57207, #13412, #56610 ),
 .UNSPECIFIED., .F., .F.,
 ( 4, 3, 3, 3, 3, 3, 4 ),
 ( 1.161956753697875813E-16, 0.0002618519381806255915, 0.0003927759815485971679, 0.0005237000248299424543, 0.0006546240681324976083, 0.0007855481115631327092, 0.0009699050456655109419 ),
 .UNSPECIFIED. ) ;
#9310 = CARTESIAN_POINT ( 'NONE',  ( 0.9790320750461911636, 29.19632847532770015, -30.06512158802884471 ) ) ;
#9311 = CARTESIAN_POINT ( 'NONE',  ( 0.1310142868023669860, 22.11113027429286504, -37.02349354742221266 ) ) ;
#9312 = ORIENTED_EDGE ( 'NONE', *, *, #34332, .F. ) ;
#9313 = CARTESIAN_POINT ( 'NONE',  ( 4.956653778116966613, 0.000000000000000000, 0.000000000000000000 ) ) ;
#9314 = CARTESIAN_POINT ( 'NONE',  ( 50.32467004767242713, 15.27178771460630635, -2.649999999999991918 ) ) ;
#9315 = CARTESIAN_POINT ( 'NONE',  ( 0.9762797500689124330, -17.18051571332090788, -38.22505284509149703 ) ) ;
#9316 = CARTESIAN_POINT ( 'NONE',  ( 0.9756950546413942771, 42.52863374229713855, -5.696573146291551204 ) ) ;
#9317 = DIRECTION ( 'NONE',  ( 0.000000000000000000, 0.000000000000000000, 1.000000000000000000 ) ) ;
#9318 = ORIENTED_EDGE ( 'NONE', *, *, #14753, .T. ) ;
#9319 = DIRECTION ( 'NONE',  ( 0.1011922191286468153, -0.6302926308031335800, -0.7697345869474001567 ) ) ;
#9320 =( BOUNDED_SURFACE ( )  B_SPLINE_SURFACE ( 3, 1, ( 
 ( #54851, #11044 ),
 ( #11987, #45492 ),
 ( #54531, #21665 ),
 ( #34851, #11658 ) ),
 .UNSPECIFIED., .F., .F., .F. ) 
 B_SPLINE_SURFACE_WITH_KNOTS ( ( 4, 4 ),
 ( 2, 2 ),
 ( 0.000000000000000000, 1.000000000000000000 ),
 ( 0.000000000000000000, 1.000000000000000000 ),
 .UNSPECIFIED. ) 
 GEOMETRIC_REPRESENTATION_ITEM ( )  RATIONAL_B_SPLINE_SURFACE ( (
 ( 1.000000000000000000, 1.000000000000000000),
 ( 0.9953485035131437453, 0.8621029689291515030),
 ( 0.9953485035131437453, 0.8621029689291515030),
 ( 1.000000000000000000, 1.000000000000000000) ) ) 
 REPRESENTATION_ITEM ( '' )  SURFACE ( )  );
#9321 = CARTESIAN_POINT ( 'NONE',  ( 0.6016117650947689910, -45.64818567478292977, -18.10508765085221938 ) ) ;
#9322 = CARTESIAN_POINT ( 'NONE',  ( -6.057079549204054558, 0.6087215340718761247, 19.24735538181013794 ) ) ;
#9323 = ORIENTED_EDGE ( 'NONE', *, *, #44485, .F. ) ;
#9324 = B_SPLINE_CURVE_WITH_KNOTS ( 'NONE', 3,
 ( #31028, #11950, #35751, #49510 ),
 .UNSPECIFIED., .F., .F.,
 ( 4, 4 ),
 ( 1.301042606982605128E-18, 0.004446298630425103184 ),
 .UNSPECIFIED. ) ;
#9325 = CONICAL_SURFACE ( 'NONE', #52336, 43.92652462719577500, 1.486293639869522343 ) ;
#9326 = B_SPLINE_CURVE_WITH_KNOTS ( 'NONE', 3,
 ( #52637, #56715, #18525, #19159 ),
 .UNSPECIFIED., .F., .F.,
 ( 4, 4 ),
 ( 0.000000000000000000, 0.005004948556313811373 ),
 .UNSPECIFIED. ) ;
#9327 = CARTESIAN_POINT ( 'NONE',  ( 5.999999999999995559, 15.14599999999999902, 0.000000000000000000 ) ) ;
#9328 = CARTESIAN_POINT ( 'NONE',  ( 0.9972139404380306882, -20.88226186415256791, 37.48536715150219578 ) ) ;
#9329 = ORIENTED_EDGE ( 'NONE', *, *, #24824, .T. ) ;
#9330 = CARTESIAN_POINT ( 'NONE',  ( 3.894904216938898323, -25.63177498392933984, 35.70905268485031314 ) ) ;
#9331 = EDGE_CURVE ( 'NONE', #58675, #43360, #47350, .T. ) ;
#9332 = ORIENTED_EDGE ( 'NONE', *, *, #61298, .F. ) ;
#9333 =( BOUNDED_SURFACE ( )  B_SPLINE_SURFACE ( 3, 1, ( 
 ( #35813, #54880 ),
 ( #12016, #45520 ),
 ( #21693, #56736 ),
 ( #3801, #27018 ) ),
 .UNSPECIFIED., .F., .F., .F. ) 
 B_SPLINE_SURFACE_WITH_KNOTS ( ( 4, 4 ),
 ( 2, 2 ),
 ( 0.000000000000000000, 1.000000000000000000 ),
 ( 0.000000000000000000, 1.000000000000000000 ),
 .UNSPECIFIED. ) 
 GEOMETRIC_REPRESENTATION_ITEM ( )  RATIONAL_B_SPLINE_SURFACE ( (
 ( 1.000000000000000000, 1.000000000000000000),
 ( 0.7223157951917480446, 0.9931996967497186413),
 ( 0.7223157951917480446, 0.9931996967497186413),
 ( 1.000000000000000000, 1.000000000000000000) ) ) 
 REPRESENTATION_ITEM ( '' )  SURFACE ( )  );
#9334 = CARTESIAN_POINT ( 'NONE',  ( 0.5809828226811553087, -29.58751527316153940, -37.66417181417581617 ) ) ;
#9335 = CARTESIAN_POINT ( 'NONE',  ( 1.154321485836934169, 42.90848031452335931, -0.8253076867720463561 ) ) ;
#9336 = EDGE_LOOP ( 'NONE', ( #57439, #15063, #12618, #803, #4401, #57375 ) ) ;
#9337 = CARTESIAN_POINT ( 'NONE',  ( 4.956445790444004018, -47.08764048036452721, 0.5405220916596411573 ) ) ;
#9338 = CARTESIAN_POINT ( 'NONE',  ( 4.694002226626921015, -44.81211596887084170, 8.376098963038019818 ) ) ;
#9339 = EDGE_CURVE ( 'NONE', #49193, #29142, #52340, .T. ) ;
#9340 = DIRECTION ( 'NONE',  ( -0.07500201931887527651, -0.8296863770785034564, -0.5531683403706671998 ) ) ;
#9341 = CARTESIAN_POINT ( 'NONE',  ( -6.077587904424778920, 19.09718056542708453, -2.468545289316033120 ) ) ;
#9342 =( BOUNDED_SURFACE ( )  B_SPLINE_SURFACE ( 3, 1, ( 
 ( #31954, #27247 ),
 ( #26314, #55118 ),
 ( #41073, #45449 ),
 ( #2498, #21621 ) ),
 .UNSPECIFIED., .F., .F., .F. ) 
 B_SPLINE_SURFACE_WITH_KNOTS ( ( 4, 4 ),
 ( 2, 2 ),
 ( 0.000000000000000000, 1.000000000000000000 ),
 ( 0.000000000000000000, 1.000000000000000000 ),
 .UNSPECIFIED. ) 
 GEOMETRIC_REPRESENTATION_ITEM ( )  RATIONAL_B_SPLINE_SURFACE ( (
 ( 1.000000000000000000, 1.000000000000000000),
 ( 0.7223157951917480446, 0.9931996967497186413),
 ( 0.7223157951917480446, 0.9931996967497186413),
 ( 1.000000000000000000, 1.000000000000000000) ) ) 
 REPRESENTATION_ITEM ( '' )  SURFACE ( )  );
#9343 = CONICAL_SURFACE ( 'NONE', #30314, 4.000000000000000000, 1.047197551196595855 ) ;
#9344 = EDGE_LOOP ( 'NONE', ( #50484, #22064, #59969, #542 ) ) ;
#9345 = CARTESIAN_POINT ( 'NONE',  ( 0.9787464366903561030, -6.796004491807877024, -41.35393954435043895 ) ) ;
#9346 = EDGE_CURVE ( 'NONE', #56041, #41141, #34520, .T. ) ;
#9347 = ORIENTED_EDGE ( 'NONE', *, *, #16371, .F. ) ;
#9348 = CARTESIAN_POINT ( 'NONE',  ( 0.5809828226811617480, -5.711058609464997105, -47.55412398569212939 ) ) ;
#9349 = ORIENTED_EDGE ( 'NONE', *, *, #17264, .T. ) ;
#9350 = EDGE_LOOP ( 'NONE', ( #4071, #29435, #9361, #39183 ) ) ;
#9351 = CARTESIAN_POINT ( 'NONE',  ( 0.6016117650947691020, -42.95818748055889102, -23.79380555164838640 ) ) ;
#9352 = CARTESIAN_POINT ( 'NONE',  ( 0.5998501479064708430, -34.38546660123321175, 33.64490850298784608 ) ) ;
#9353 = CARTESIAN_POINT ( 'NONE',  ( 3.661921753701995907, 46.83251652495474104, 4.398467889376776796 ) ) ;
#9354 = DIRECTION ( 'NONE',  ( -1.000000000000000000, -0.000000000000000000, 1.925929944387235853E-32 ) ) ;
#9355 = EDGE_LOOP ( 'NONE', ( #2923, #54842, #10669, #51163 ) ) ;
#9356 = CARTESIAN_POINT ( 'NONE',  ( 0.9754642270333693244, 0.1757168848625156043, -42.90808635884410194 ) ) ;
#9357 = CARTESIAN_POINT ( 'NONE',  ( 5.895596859100789899, -19.39731145114851074, 5.317188324634581242 ) ) ;
#9358 = EDGE_CURVE ( 'NONE', #22596, #20457, #26502, .T. ) ;
#9359 = CARTESIAN_POINT ( 'NONE',  ( 0.1158816050234198480, -38.44342348468149595, 21.65745211428624017 ) ) ;
#9360 = VERTEX_POINT ( 'NONE', #38586 ) ;
#9361 = ORIENTED_EDGE ( 'NONE', *, *, #37068, .F. ) ;
#9362 = CARTESIAN_POINT ( 'NONE',  ( 4.975801465491694664, -2.564218696447152279, -47.84403947906842092 ) ) ;
#9363 = CARTESIAN_POINT ( 'NONE',  ( 5.981074661064941900, -19.82752479807523827, -5.303881226583607500 ) ) ;
#9364 = CARTESIAN_POINT ( 'NONE',  ( 4.962356264823603702, 17.31942680647464528, -38.35717733303005161 ) ) ;
#9365 = CARTESIAN_POINT ( 'NONE',  ( 0.5980894510889457338, 42.01322166096886690, 23.44630161211600949 ) ) ;
#9366 = ORIENTED_EDGE ( 'NONE', *, *, #1777, .T. ) ;
#9367 = ORIENTED_EDGE ( 'NONE', *, *, #22995, .F. ) ;
#9368 = CARTESIAN_POINT ( 'NONE',  ( 0.5997462898726536595, -34.91088276334750873, 34.53667463477217581 ) ) ;
#9369 = CARTESIAN_POINT ( 'NONE',  ( 0.5980894510889448457, 37.73932204245478772, 29.84264441023791292 ) ) ;
#9370 = LINE ( 'NONE', #28476, #1952 ) ;
#9371 = AXIS2_PLACEMENT_3D ( 'NONE', #24169, #14791, #38606 ) ;
#9372 = CARTESIAN_POINT ( 'NONE',  ( 0.9752570700956783023, -21.65368877244782553, 37.04395688491842975 ) ) ;
#9373 =( NAMED_UNIT ( * ) PLANE_ANGLE_UNIT ( ) SI_UNIT ( $, .RADIAN. ) );
#9374 = CARTESIAN_POINT ( 'NONE',  ( 0.7056555295713335951, -34.46100226633713959, -33.27140645154231180 ) ) ;
#9375 = ORIENTED_EDGE ( 'NONE', *, *, #22140, .T. ) ;
#9376 = CARTESIAN_POINT ( 'NONE',  ( 0.1139756605157204450, 20.05585777468466091, -39.30289796715559447 ) ) ;
#9377 = CARTESIAN_POINT ( 'NONE',  ( -6.072942160501519915, 9.994728154871237891, 16.45933083084620563 ) ) ;
#9378 = CARTESIAN_POINT ( 'NONE',  ( 0.5800708119828333897, -46.42229822050688171, -11.78915056783756832 ) ) ;
#9379 = FACE_OUTER_BOUND ( 'NONE', #20756, .T. ) ;
#9380 = FACE_OUTER_BOUND ( 'NONE', #23143, .T. ) ;
#9381 = EDGE_CURVE ( 'NONE', #44630, #5475, #48223, .T. ) ;
#9382 = CARTESIAN_POINT ( 'NONE',  ( -6.063463321072276813, 7.809047921946303816, 17.60225051043803290 ) ) ;
#9383 = AXIS2_PLACEMENT_3D ( 'NONE', #33100, #23073, #22447 ) ;
#9384 = DIRECTION ( 'NONE',  ( 0.000000000000000000, 0.000000000000000000, 1.000000000000000000 ) ) ;
#9385 = EDGE_CURVE ( 'NONE', #58158, #789, #19783, .T. ) ;
#9386 = ADVANCED_FACE ( 'NONE', ( #47973 ), #40758, .F. ) ;
#9387 = CARTESIAN_POINT ( 'NONE',  ( -5.995132425357893702, 14.95525565067290508, -11.46484027925352578 ) ) ;
#9388 = VERTEX_POINT ( 'NONE', #52031 ) ;
#9389 = CARTESIAN_POINT ( 'NONE',  ( 0.1100053167205930632, 37.43629428538733350, 21.40663161101006295 ) ) ;
#9390 = CARTESIAN_POINT ( 'NONE',  ( 0.5809828226811553087, 46.40184912890838831, 11.86925843957183879 ) ) ;
#9391 = DIRECTION ( 'NONE',  ( 0.09722883295013594329, -0.8021136117729473769, -0.5892031125611201237 ) ) ;
#9392 = ORIENTED_EDGE ( 'NONE', *, *, #21746, .F. ) ;
#9393 = CARTESIAN_POINT ( 'NONE',  ( 0.8557997880470697982, -46.03118133706034598, 13.27832040216623355 ) ) ;
#9394 = CARTESIAN_POINT ( 'NONE',  ( -6.000000000000004441, 15.14599999999999902, 0.000000000000000000 ) ) ;
#9395 = CARTESIAN_POINT ( 'NONE',  ( 4.975610109902397937, 0.000000000000000000, 0.000000000000000000 ) ) ;
#9396 = ORIENTED_EDGE ( 'NONE', *, *, #58464, .F. ) ;
#9397 = CARTESIAN_POINT ( 'NONE',  ( 2.624215991343620935, 45.98641578154050791, -13.78323291683735796 ) ) ;
#9398 = CARTESIAN_POINT ( 'NONE',  ( 4.963659409799330291, 2.450325214229022830, -44.68724496494571952 ) ) ;
#9399 = CARTESIAN_POINT ( 'NONE',  ( -6.016489644550736315, 2.463898142942760661, 18.68142234211825325 ) ) ;
#9400 = EDGE_CURVE ( 'NONE', #54025, #59710, #40038, .T. ) ;
#9401 = VERTEX_POINT ( 'NONE', #57636 ) ;
#9402 = CARTESIAN_POINT ( 'NONE',  ( 4.960386119450149955, -34.62801484853867606, 26.74578569273533901 ) ) ;
#9403 = VERTEX_POINT ( 'NONE', #33883 ) ;
#9404 = CARTESIAN_POINT ( 'NONE',  ( 0.5809828226811617480, -17.82437196699647686, -44.45562576850621639 ) ) ;
#9406 = ORIENTED_EDGE ( 'NONE', *, *, #3803, .T. ) ;
#9405 = EDGE_CURVE ( 'NONE', #27059, #50629, #47060, .T. ) ;
#9407 = CARTESIAN_POINT ( 'NONE',  ( 0.5827359174754822568, -5.891371786504645769, -47.53228759166454864 ) ) ;
#9408 = FACE_OUTER_BOUND ( 'NONE', #13827, .T. ) ;
#9409 = VERTEX_POINT ( 'NONE', #9126 ) ;
#9410 = CARTESIAN_POINT ( 'NONE',  ( 0.5804410086790514622, -14.41595396256475325, 44.62846763227043567 ) ) ;
#9411 = VECTOR ( 'NONE', #61831, 1000.000000000000000 ) ;
#9412 = EDGE_LOOP ( 'NONE', ( #57442, #10733, #57075, #39051 ) ) ;
#9413 = CARTESIAN_POINT ( 'NONE',  ( 5.974727161628367256, 16.27409205901376055, -12.50710176109990890 ) ) ;
#9414 = EDGE_CURVE ( 'NONE', #6735, #47955, #11545, .T. ) ;
#9415 =( BOUNDED_SURFACE ( )  B_SPLINE_SURFACE ( 3, 1, ( 
 ( #51436, #42391 ),
 ( #43010, #14493 ),
 ( #33602, #61146 ),
 ( #13564, #56757 ) ),
 .UNSPECIFIED., .F., .F., .F. ) 
 B_SPLINE_SURFACE_WITH_KNOTS ( ( 4, 4 ),
 ( 2, 2 ),
 ( 0.000000000000000000, 1.000000000000000000 ),
 ( 0.000000000000000000, 1.000000000000000000 ),
 .UNSPECIFIED. ) 
 GEOMETRIC_REPRESENTATION_ITEM ( )  RATIONAL_B_SPLINE_SURFACE ( (
 ( 1.000000000000000000, 1.000000000000000000),
 ( 0.9952954269826590483, 0.8620686068821339365),
 ( 0.9952954269826590483, 0.8620686068821339365),
 ( 1.000000000000000000, 1.000000000000000000) ) ) 
 REPRESENTATION_ITEM ( '' )  SURFACE ( )  );
#9416 = CARTESIAN_POINT ( 'NONE',  ( -6.017396004339687465, -18.20079405513546433, -4.878103249821258203 ) ) ;
#9417 = CARTESIAN_POINT ( 'NONE',  ( 2.624215991343608501, -37.21129343241584309, -30.33228621715073459 ) ) ;
#9418 = ORIENTED_EDGE ( 'NONE', *, *, #24178, .T. ) ;
#9419 = CARTESIAN_POINT ( 'NONE',  ( 0.9730545539215883499, -15.95224156741799426, -39.83279466599056917 ) ) ;
#9420 = CARTESIAN_POINT ( 'NONE',  ( 5.896782393890504181, -9.671431223051156323, 17.63489452692596515 ) ) ;
#9421 = FACE_OUTER_BOUND ( 'NONE', #44600, .T. ) ;
#9422 = CARTESIAN_POINT ( 'NONE',  ( 0.5835871038041854364, 16.72726757634624661, 43.81133383418971761 ) ) ;
#9423 = ORIENTED_EDGE ( 'NONE', *, *, #50453, .F. ) ;
#9424 = CARTESIAN_POINT ( 'NONE',  ( 5.959547316686252039, -5.308980600728319565, -19.82715097195160325 ) ) ;
#9425 = EDGE_CURVE ( 'NONE', #33472, #11600, #8586, .T. ) ;
#9426 = CARTESIAN_POINT ( 'NONE',  ( 0.7954196712028465122, -13.28627209367609474, 46.22745629466049877 ) ) ;
#9427 = CIRCLE ( 'NONE', #42464, 47.09074272231896430 ) ;
#9428 = ORIENTED_EDGE ( 'NONE', *, *, #8843, .T. ) ;
#9429 = CARTESIAN_POINT ( 'NONE',  ( 0.5837800304671212359, 43.19256532450906860, -18.26580501558905922 ) ) ;
#9430 = VERTEX_POINT ( 'NONE', #6243 ) ;
#9431 = CARTESIAN_POINT ( 'NONE',  ( 0.9762797500689124330, 25.26481495167865532, 33.43671500974846822 ) ) ;
#9432 = CARTESIAN_POINT ( 'NONE',  ( 0.2885697896453109368, -41.43179225254756659, -11.93479333319010216 ) ) ;
#9433 = VERTEX_POINT ( 'NONE', #53266 ) ;
#9434 = CARTESIAN_POINT ( 'NONE',  ( 0.5832655196449147983, 4.467535350384531867, 46.68271961728872554 ) ) ;
#9435 = CARTESIAN_POINT ( 'NONE',  ( -6.078457390727109555, -12.94259897003402493, -14.25775728992403835 ) ) ;
#9436 = DIRECTION ( 'NONE',  ( 0.000000000000000000, 0.000000000000000000, 1.000000000000000000 ) ) ;
#9437 = CARTESIAN_POINT ( 'NONE',  ( 0.9788927965476029724, -22.66962964973810202, -35.24804255806969877 ) ) ;
#9438 = VERTEX_POINT ( 'NONE', #45147 ) ;
#9439 = DIRECTION ( 'NONE',  ( 0.000000000000000000, 0.000000000000000000, 1.000000000000000000 ) ) ;
#9440 = CARTESIAN_POINT ( 'NONE',  ( 4.975801465491695552, 3.702618843596801934, 47.76942479135487218 ) ) ;
#9441 = CARTESIAN_POINT ( 'NONE',  ( 0.8551540677456715978, 24.74404575822775598, 41.03346287276436755 ) ) ;
#9442 = B_SPLINE_CURVE_WITH_KNOTS ( 'NONE', 3,
 ( #47358, #56738, #33277, #32340 ),
 .UNSPECIFIED., .F., .F.,
 ( 4, 4 ),
 ( 0.000000000000000000, 0.005013413432710141573 ),
 .UNSPECIFIED. ) ;
#9443 = CARTESIAN_POINT ( 'NONE',  ( 0.7044674535453004927, -26.17468433047353216, -41.55344297421058997 ) ) ;
#9444 = CARTESIAN_POINT ( 'NONE',  ( 5.959547316686252039, -16.28624005235107930, 12.49238070347948870 ) ) ;
#9445 = B_SPLINE_CURVE_WITH_KNOTS ( 'NONE', 3,
 ( #47028, #13201, #42633, #57009, #37953, #56695, #37634, #23503, #18206, #18826, #17904, #14135, #33236, #9096, #13825, #42032 ),
 .UNSPECIFIED., .F., .F.,
 ( 4, 3, 3, 3, 3, 4 ),
 ( 1.214354834101861570E-17, 0.0002732102107931916801, 0.0004098135523333818592, 0.0005464168938824978412, 0.0008195847345945461541, 0.001092771384553108084 ),
 .UNSPECIFIED. ) ;
#9446 = AXIS2_PLACEMENT_3D ( 'NONE', #1058, #9860, #53659 ) ;
#9447 = CARTESIAN_POINT ( 'NONE',  ( 0.5809828226811553087, -46.11980934799348830, 12.92184523170186594 ) ) ;
#9448 = CARTESIAN_POINT ( 'NONE',  ( 0.3622758884714600280, 42.84426538328730771, -4.808133778521432866 ) ) ;
#9449 = CARTESIAN_POINT ( 'NONE',  ( 0.9789233960466712237, -12.54205289678194468, 39.98791862508804940 ) ) ;
#9450 = DIRECTION ( 'NONE',  ( -1.000000000000000000, -0.000000000000000000, -0.000000000000000000 ) ) ;
#9451 = EDGE_CURVE ( 'NONE', #9272, #43892, #42251, .T. ) ;
#9452 = CARTESIAN_POINT ( 'NONE',  ( 5.880360259849739535, 43.00389496650614518, -21.25991003419908054 ) ) ;
#9453 = CARTESIAN_POINT ( 'NONE',  ( 0.7056313189692727805, 33.20628302271070709, 33.12237026200259749 ) ) ;
#9454 = CARTESIAN_POINT ( 'NONE',  ( 0.1139756605157202229, 39.92552665614537233, 18.78583351689372805 ) ) ;
#9455 = CARTESIAN_POINT ( 'NONE',  ( 0.9722240750034573109, -41.59310803641454868, -10.54237121715129177 ) ) ;
#9457 = ADVANCED_FACE ( 'NONE', ( #5940 ), #7477, .T. ) ;
#9456 = CARTESIAN_POINT ( 'NONE',  ( 0.5848930533535030563, 17.02477461160273009, -43.69702657860927530 ) ) ;
#9458 = DIRECTION ( 'NONE',  ( 1.000000000000000000, 0.000000000000000000, 0.000000000000000000 ) ) ;
#9459 = AXIS2_PLACEMENT_3D ( 'NONE', #4865, #54949, #35261 ) ;
#9460 = EDGE_CURVE ( 'NONE', #7089, #4962, #16827, .T. ) ;
#9461 = CARTESIAN_POINT ( 'NONE',  ( -2.708315649062916552, 14.20182604343555255, 3.532515819624394204 ) ) ;
#9462 = CARTESIAN_POINT ( 'NONE',  ( -6.010958268070873523, -18.68034667844850460, 2.473955915502147107 ) ) ;
#9463 = ADVANCED_FACE ( 'NONE', ( #24777 ), #51873, .F. ) ;
#9464 = ORIENTED_EDGE ( 'NONE', *, *, #59161, .F. ) ;
#9465 = CARTESIAN_POINT ( 'NONE',  ( 4.956445790444006683, -32.34643101787064978, -34.22347806032829709 ) ) ;
#9466 = CARTESIAN_POINT ( 'NONE',  ( 0.6064782688330861982, -19.09363116089746271, -42.83418839560724223 ) ) ;
#9467 = DIRECTION ( 'NONE',  ( -1.000000000000000000, 0.000000000000000000, 0.000000000000000000 ) ) ;
#9468 = ORIENTED_EDGE ( 'NONE', *, *, #21369, .F. ) ;
#9469 = CARTESIAN_POINT ( 'NONE',  ( 0.5837374860065641657, -33.73893264285572968, 33.99581326751421528 ) ) ;
#9470 = VECTOR ( 'NONE', #55576, 1000.000000000000114 ) ;
#9471 = CARTESIAN_POINT ( 'NONE',  ( 1.296416391601052265, 26.11750747786893001, 35.49905882160285131 ) ) ;
#9472 = VERTEX_POINT ( 'NONE', #25698 ) ;
#9473 = ORIENTED_EDGE ( 'NONE', *, *, #451, .T. ) ;
#9474 = EDGE_CURVE ( 'NONE', #2450, #29811, #44838, .T. ) ;
#9475 = FACE_OUTER_BOUND ( 'NONE', #24210, .T. ) ;
#9476 = EDGE_CURVE ( 'NONE', #4600, #50690, #44476, .T. ) ;
#9477 = VERTEX_POINT ( 'NONE', #39209 ) ;
#9478 = CARTESIAN_POINT ( 'NONE',  ( 0.000000000000000000, -2.357898499370432166, 3.035766082959412415E-15 ) ) ;
#9479 = CARTESIAN_POINT ( 'NONE',  ( 0.6064515330803581517, 28.38734125881933323, 37.32952172600688101 ) ) ;
#9480 = VERTEX_POINT ( 'NONE', #35121 ) ;
#9481 = ORIENTED_EDGE ( 'NONE', *, *, #55351, .T. ) ;
#9482 = CARTESIAN_POINT ( 'NONE',  ( 0.6039202388192952409, 44.31978288059539040, -21.14995409607015375 ) ) ;
#9483 = ORIENTED_EDGE ( 'NONE', *, *, #60077, .T. ) ;
#9484 = DIRECTION ( 'NONE',  ( 0.000000000000000000, 0.000000000000000000, 1.000000000000000000 ) ) ;
#9485 = CARTESIAN_POINT ( 'NONE',  ( 5.901764892641288895, 19.86141101510633433, 44.76065035194071839 ) ) ;
#9486 = CARTESIAN_POINT ( 'NONE',  ( 0.6039202388192953519, -45.58380534490247982, -18.26692100839743205 ) ) ;
#9487 = ORIENTED_EDGE ( 'NONE', *, *, #45842, .T. ) ;
#9488 = CARTESIAN_POINT ( 'NONE',  ( -2.569797478183790229, 11.87678401312194865, -8.547745408040670512 ) ) ;
#9489 = AXIS2_PLACEMENT_3D ( 'NONE', #27123, #26814, #21811 ) ;
#9490 = B_SPLINE_CURVE_WITH_KNOTS ( 'NONE', 3,
 ( #9141, #61739, #27951, #3498 ),
 .UNSPECIFIED., .F., .F.,
 ( 4, 4 ),
 ( 2.292215966409847588E-17, 0.004564976165746187711 ),
 .UNSPECIFIED. ) ;
#9491 = LINE ( 'NONE', #57698, #49981 ) ;
#9492 = ORIENTED_EDGE ( 'NONE', *, *, #58968, .F. ) ;
#9493 = ORIENTED_EDGE ( 'NONE', *, *, #59196, .F. ) ;
#9494 = CARTESIAN_POINT ( 'NONE',  ( 5.958863334805807099, 18.96369761673819809, -7.853699934219702250 ) ) ;
#9495 = ORIENTED_EDGE ( 'NONE', *, *, #44581, .F. ) ;
#9496 = CARTESIAN_POINT ( 'NONE',  ( 0.6028777368367060907, 46.57818122485500822, 15.55676261616270217 ) ) ;
#9497 = CARTESIAN_POINT ( 'NONE',  ( -6.016761891674565099, -2.462934516563935805, 18.68153697670640767 ) ) ;
#9498 = CARTESIAN_POINT ( 'NONE',  ( 5.860006189529246790, -9.393028332204430342, -47.30964106197868091 ) ) ;
#9499 = CARTESIAN_POINT ( 'NONE',  ( 0.8560838555295223751, 39.88643293834682879, -24.68694597426934223 ) ) ;
#9500 = EDGE_CURVE ( 'NONE', #2066, #3834, #13506, .T. ) ;
#9501 = ORIENTED_EDGE ( 'NONE', *, *, #54923, .T. ) ;
#9502 = CARTESIAN_POINT ( 'NONE',  ( 4.975801465491695552, 0.000000000000000000, 0.000000000000000000 ) ) ;
#9503 = FACE_OUTER_BOUND ( 'NONE', #46168, .T. ) ;
#9504 = EDGE_CURVE ( 'NONE', #4300, #6071, #58262, .T. ) ;
#9505 = CARTESIAN_POINT ( 'NONE',  ( 0.6064515330803623705, -30.81728595274794813, -35.35009508535515721 ) ) ;
#9506 = CIRCLE ( 'NONE', #12530, 42.08604991992415023 ) ;
#9507 = ORIENTED_EDGE ( 'NONE', *, *, #12614, .F. ) ;
#9508 = CARTESIAN_POINT ( 'NONE',  ( 0.3622758884714730732, -29.89648521331652731, 31.06363466427676201 ) ) ;
#9509 = CARTESIAN_POINT ( 'NONE',  ( 4.967162193818130511, -8.839793687084915419, -42.16965968614202609 ) ) ;
#9510 = CARTESIAN_POINT ( 'NONE',  ( 4.060580049360325461, -4.720430316018839889, 43.69422424063414212 ) ) ;
#9511 = ORIENTED_EDGE ( 'NONE', *, *, #7147, .T. ) ;
#9512 = ORIENTED_EDGE ( 'NONE', *, *, #54654, .T. ) ;
#9513 = CARTESIAN_POINT ( 'NONE',  ( 2.648799415243696664, -44.91402171431661827, -19.67862080369183531 ) ) ;
#9514 = CARTESIAN_POINT ( 'NONE',  ( 0.1103744047535531458, -42.76053735246615872, 5.590449877749870566 ) ) ;
#9515 = CARTESIAN_POINT ( 'NONE',  ( 0.1092565886968784594, -39.72209809039409834, 16.78938711553560026 ) ) ;
#9516 = CARTESIAN_POINT ( 'NONE',  ( -6.063463321072276813, 16.77106408806610460, -9.463184550321813049 ) ) ;
#9517 = DIRECTION ( 'NONE',  ( 0.9848077530122080203, 0.1736481776669315524, -2.220446049250313574E-16 ) ) ;
#9518 = CARTESIAN_POINT ( 'NONE',  ( 0.1139756605157202923, -18.22362019290597601, -40.18525708216549930 ) ) ;
#9519 = CARTESIAN_POINT ( 'NONE',  ( 0.1064266418746774995, 40.05351192729361287, -15.98292515284421533 ) ) ;
#9520 = CARTESIAN_POINT ( 'NONE',  ( 4.956653778116997699, 42.88673967249161478, -21.75875759808661059 ) ) ;
#9521 = FACE_OUTER_BOUND ( 'NONE', #45722, .T. ) ;
#9522 = CARTESIAN_POINT ( 'NONE',  ( 4.975801465491695552, -45.55012473237743365, -14.85979367497158599 ) ) ;
#9523 = CARTESIAN_POINT ( 'NONE',  ( 0.9784957157296361174, 41.90798102287331517, -0.2327736644509323383 ) ) ;
#9524 = CARTESIAN_POINT ( 'NONE',  ( 0.7048096507298579061, -44.11842270945960109, -19.18768066167107023 ) ) ;
#9525 = ORIENTED_EDGE ( 'NONE', *, *, #59237, .T. ) ;
#9526 = DIRECTION ( 'NONE',  ( 0.000000000000000000, -0.7071067811865487940, 0.7071067811865461294 ) ) ;
#9527 = CARTESIAN_POINT ( 'NONE',  ( 0.6016118706126976079, 40.96538442997461260, 27.08114350038277962 ) ) ;
#9528 = EDGE_CURVE ( 'NONE', #33475, #24938, #56404, .T. ) ;
#9529 = DIRECTION ( 'NONE',  ( 0.000000000000000000, 0.000000000000000000, -1.000000000000000000 ) ) ;
#9530 = CARTESIAN_POINT ( 'NONE',  ( 3.894904216938897434, -24.65949896380412198, -36.38727034733911125 ) ) ;
#9531 = CARTESIAN_POINT ( 'NONE',  ( 0.1095718737110178281, 42.72125633542926693, 5.883530294870284116 ) ) ;
#9533 = EDGE_CURVE ( 'NONE', #7813, #39205, #37037, .T. ) ;
#9532 = DIRECTION ( 'NONE',  ( 1.000000000000000000, 0.000000000000000000, 0.000000000000000000 ) ) ;
#9534 = CARTESIAN_POINT ( 'NONE',  ( 0.6026777506516368677, 22.55952138954113195, -43.61896818257001485 ) ) ;
#9535 = APPLICATION_CONTEXT ( 'automotive_design' ) ;
#9536 =( BOUNDED_SURFACE ( )  B_SPLINE_SURFACE ( 3, 1, ( 
 ( #49153, #30045 ),
 ( #6206, #53527 ),
 ( #58530, #10643 ),
 ( #43554, #44489 ) ),
 .UNSPECIFIED., .F., .F., .F. ) 
 B_SPLINE_SURFACE_WITH_KNOTS ( ( 4, 4 ),
 ( 2, 2 ),
 ( 0.000000000000000000, 1.000000000000000000 ),
 ( 0.000000000000000000, 1.000000000000000000 ),
 .UNSPECIFIED. ) 
 GEOMETRIC_REPRESENTATION_ITEM ( )  RATIONAL_B_SPLINE_SURFACE ( (
 ( 1.000000000000000000, 1.000000000000000000),
 ( 0.9751682680413298332, 0.9999560080971552356),
 ( 0.9751682680413298332, 0.9999560080971552356),
 ( 1.000000000000000000, 1.000000000000000000) ) ) 
 REPRESENTATION_ITEM ( '' )  SURFACE ( )  );
#9537 = CARTESIAN_POINT ( 'NONE',  ( 0.5837374860065657201, 12.57177159055162008, 46.21667939904217093 ) ) ;
#9538 = EDGE_CURVE ( 'NONE', #6553, #22299, #49501, .T. ) ;
#9539 = CARTESIAN_POINT ( 'NONE',  ( 1.157643937452367933, -37.03171704562910094, 19.63808053877000859 ) ) ;
#9540 = EDGE_CURVE ( 'NONE', #25579, #7415, #36246, .T. ) ;
#9542 = ORIENTED_EDGE ( 'NONE', *, *, #50112, .T. ) ;
#9541 = CARTESIAN_POINT ( 'NONE',  ( 0.5998501479064708430, -46.33007877220729398, -12.95623334615486222 ) ) ;
#9544 = ORIENTED_EDGE ( 'NONE', *, *, #25506, .T. ) ;
#9543 = B_SPLINE_CURVE_WITH_KNOTS ( 'NONE', 3,
 ( #22942, #42069, #55813, #61123, #18241, #17618, #27627, #37353, #36745, #18540, #56426, #32030, #37668, #60817, #23541, #15087 ),
 .UNSPECIFIED., .F., .F.,
 ( 4, 3, 3, 3, 3, 4 ),
 ( 1.084256381238943740E-17, 0.0002732102107931889154, 0.0004098135523333797450, 0.0005464168938824980580, 0.0008195847345945433352, 0.001092771384553107867 ),
 .UNSPECIFIED. ) ;
#9545 = CARTESIAN_POINT ( 'NONE',  ( 3.783198216974387851, -31.62918462580860535, 29.18723368117353090 ) ) ;
#9546 = CARTESIAN_POINT ( 'NONE',  ( 0.1100247026804066219, 39.77655614012830654, 16.65964013375399588 ) ) ;
#9547 = EDGE_CURVE ( 'NONE', #33579, #48168, #28023, .T. ) ;
#9548 = FACE_OUTER_BOUND ( 'NONE', #58302, .T. ) ;
#9549 = ORIENTED_EDGE ( 'NONE', *, *, #43584, .T. ) ;
#9550 = CARTESIAN_POINT ( 'NONE',  ( 0.5835226383429280572, 22.69696281568404217, 41.03766993250741990 ) ) ;
#9551 = CARTESIAN_POINT ( 'NONE',  ( 0.7948878604505679180, -47.26562360489970871, 13.29133072865033682 ) ) ;
#9552 = CARTESIAN_POINT ( 'NONE',  ( -6.015611763856276717, 17.40650793417844255, 7.216738110653344584 ) ) ;
#9553 = ORIENTED_EDGE ( 'NONE', *, *, #50497, .F. ) ;
#9554 = VERTEX_POINT ( 'NONE', #46070 ) ;
#9555 = ADVANCED_FACE ( 'NONE', ( #46367 ), #6651, .F. ) ;
#9556 = COLOUR_RGB ( '', 0.09019608, 0.27058824, 0.51372549) ;
#9557 = CARTESIAN_POINT ( 'NONE',  ( 2.643462169533600914, -30.32726672320828243, 37.25264019563361018 ) ) ;
#9558 = CARTESIAN_POINT ( 'NONE',  ( 0.8751705887134553219, 13.30665218149297857, 46.21789262997761938 ) ) ;
#9559 = CONICAL_SURFACE ( 'NONE', #7528, 43.92652462719577500, 1.486293639869522343 ) ;
#9560 = CARTESIAN_POINT ( 'NONE',  ( 0.5837800304671192375, 46.89600475158708548, 0.04550295183057281867 ) ) ;
#9562 = CARTESIAN_POINT ( 'NONE',  ( 0.7245667037590739490, -17.64710816761290957, 44.74806999162959187 ) ) ;
#9561 = VECTOR ( 'NONE', #15395, 1000.000000000000114 ) ;
#9563 = CARTESIAN_POINT ( 'NONE',  ( 0.2885700199627514451, 10.38006184593202263, -41.84838128711413674 ) ) ;
#9564 = CARTESIAN_POINT ( 'NONE',  ( 0.5834872094924161701, 38.13619618345251183, -28.97678700412145858 ) ) ;
#9565 = ORIENTED_EDGE ( 'NONE', *, *, #16783, .F. ) ;
#9566 = CARTESIAN_POINT ( 'NONE',  ( -5.995132425357893702, -9.429450169548070804, 16.31525984181029898 ) ) ;
#9567 = CARTESIAN_POINT ( 'NONE',  ( 0.7413678028165009426, 44.05566091053800193, 1.893365655634854372 ) ) ;
#9568 = ORIENTED_EDGE ( 'NONE', *, *, #52001, .F. ) ;
#9569 = CARTESIAN_POINT ( 'NONE',  ( 4.956445790443998689, -22.15545010017797622, 41.55326799420426198 ) ) ;
#9570 = CARTESIAN_POINT ( 'NONE',  ( 5.896782393890504181, 0.6657210432555761281, 20.10181341000306077 ) ) ;
#9571 = CARTESIAN_POINT ( 'NONE',  ( 0.6009453534118441853, 46.35353704332094082, 12.87216801774561326 ) ) ;
#9572 = CARTESIAN_POINT ( 'NONE',  ( 1.154321713695929397, 15.65787958845416661, 39.95809834491002732 ) ) ;
#9573 = VERTEX_POINT ( 'NONE', #36982 ) ;
#9574 = VERTEX_POINT ( 'NONE', #54807 ) ;
#9575 = CARTESIAN_POINT ( 'NONE',  ( 1.827326673878743923, 34.89023127623421061, -25.21837361081552586 ) ) ;
#9576 = CARTESIAN_POINT ( 'NONE',  ( 0.5804410086790514622, -2.113107284889306658, 46.85141011173456604 ) ) ;
#9577 = CARTESIAN_POINT ( 'NONE',  ( 0.1102847568649952675, -37.39286109091562338, -21.48234084756682805 ) ) ;
#9578 = ADVANCED_FACE ( 'NONE', ( #13163 ), #32315, .F. ) ;
#9579 = ORIENTED_EDGE ( 'NONE', *, *, #27370, .T. ) ;
#9580 = CARTESIAN_POINT ( 'NONE',  ( -6.017396004339687465, 18.20140164570675978, -4.875835690938989053 ) ) ;
#9581 = VERTEX_POINT ( 'NONE', #32261 ) ;
#9582 = CARTESIAN_POINT ( 'NONE',  ( 0.1073791018717483448, -26.63563652260144821, -33.91564619577798823 ) ) ;
#9583 = CARTESIAN_POINT ( 'NONE',  ( 4.958415959904820092, -44.94704195038531225, -6.554950322690599407 ) ) ;
#9584 = VERTEX_POINT ( 'NONE', #2802 ) ;
#9585 = CARTESIAN_POINT ( 'NONE',  ( 3.782542959838393504, 34.03285927320680315, -24.67797283179218226 ) ) ;
#9586 = CARTESIAN_POINT ( 'NONE',  ( -6.078726893082806448, 19.25601281685051802, 0.003415553934478593023 ) ) ;
#9587 = B_SPLINE_CURVE_WITH_KNOTS ( 'NONE', 3,
 ( #877, #43515, #44748, #10916 ),
 .UNSPECIFIED., .F., .F.,
 ( 4, 4 ),
 ( 0.000000000000000000, 0.004444103432399267896 ),
 .UNSPECIFIED. ) ;
#9588 = CARTESIAN_POINT ( 'NONE',  ( 0.5998501479064699549, -46.33007877220747872, 12.95623334615421740 ) ) ;
#9589 = ORIENTED_EDGE ( 'NONE', *, *, #23311, .T. ) ;
#9590 =( BOUNDED_SURFACE ( )  B_SPLINE_SURFACE ( 3, 1, ( 
 ( #50403, #21597 ),
 ( #49793, #54155 ),
 ( #36034, #55096 ),
 ( #60398, #50103 ) ),
 .UNSPECIFIED., .F., .F., .F. ) 
 B_SPLINE_SURFACE_WITH_KNOTS ( ( 4, 4 ),
 ( 2, 2 ),
 ( 0.000000000000000000, 1.000000000000000000 ),
 ( 0.000000000000000000, 1.000000000000000000 ),
 .UNSPECIFIED. ) 
 GEOMETRIC_REPRESENTATION_ITEM ( )  RATIONAL_B_SPLINE_SURFACE ( (
 ( 1.000000000000000000, 1.000000000000000000),
 ( 0.7282232189291694135, 0.9929344683865672927),
 ( 0.7282232189291694135, 0.9929344683865672927),
 ( 1.000000000000000000, 1.000000000000000000) ) ) 
 REPRESENTATION_ITEM ( '' )  SURFACE ( )  );
#9591 = CARTESIAN_POINT ( 'NONE',  ( 3.238018933889920792, 12.22151767825363500, 5.481058110236275205 ) ) ;
#9592 = CARTESIAN_POINT ( 'NONE',  ( 0.3676999524040323597, -42.87209381266892194, 10.38913641457044434 ) ) ;
#9593 = CARTESIAN_POINT ( 'NONE',  ( 0.9968887458511656030, 26.64009929991552994, -33.63815526548957280 ) ) ;
#9594 = CARTESIAN_POINT ( 'NONE',  ( 4.000000000000004441, -1.549102112939112486, -0.1578953385959447620 ) ) ;
#9595 = CARTESIAN_POINT ( 'NONE',  ( 0.1092355843206037486, 16.78033551728664108, -39.72582785521899496 ) ) ;
#9596 = VERTEX_POINT ( 'NONE', #60422 ) ;
#9597 = CARTESIAN_POINT ( 'NONE',  ( 5.880360259849739535, -36.09847387447837974, -31.59460303415970017 ) ) ;
#9598 = CARTESIAN_POINT ( 'NONE',  ( 2.185380717157383135, -16.49852742981111930, 40.82423784610031703 ) ) ;
#9599 = EDGE_LOOP ( 'NONE', ( #10284, #54599, #52012, #38499 ) ) ;
#9600 = CIRCLE ( 'NONE', #47619, 47.09074272231896430 ) ;
#9601 = CARTESIAN_POINT ( 'NONE',  ( 3.661921753702004789, -28.90718528634099371, 37.10802827765424894 ) ) ;
#9602 = CARTESIAN_POINT ( 'NONE',  ( 3.270143674763207553, 11.71453292426889270, -7.080034332678136089 ) ) ;
#9603 = CARTESIAN_POINT ( 'NONE',  ( 3.678748215320120973, 40.00785673245739815, -28.24861437264927133 ) ) ;
#9604 = CIRCLE ( 'NONE', #48512, 47.09074272231896430 ) ;
#9605 = CARTESIAN_POINT ( 'NONE',  ( -2.601141883200665639, -14.85441002404438571, 1.463533500456443592 ) ) ;
#9606 = B_SPLINE_CURVE_WITH_KNOTS ( 'NONE', 3,
 ( #30958, #26247, #21561, #59764 ),
 .UNSPECIFIED., .F., .F.,
 ( 4, 4 ),
 ( 2.153172013482225773E-17, 0.004559932413162188537 ),
 .UNSPECIFIED. ) ;
#9607 = CARTESIAN_POINT ( 'NONE',  ( 0.7764139734771253742, -6.921054633042174054, -46.39115727887494955 ) ) ;
#9608 = CARTESIAN_POINT ( 'NONE',  ( 0.1368894036331265163, -40.65507205369316068, 17.14719925329937311 ) ) ;
#9609 = DIRECTION ( 'NONE',  ( 0.000000000000000000, 0.000000000000000000, 1.000000000000000000 ) ) ;
#9610 = DIRECTION ( 'NONE',  ( -1.000000000000000000, -1.669129244541435802E-16, 4.163336342344376470E-17 ) ) ;
#9612 = EDGE_CURVE ( 'NONE', #10587, #27245, #10829, .T. ) ;
#9611 = CARTESIAN_POINT ( 'NONE',  ( 1.227938101723748288, -41.66816631169199070, 10.28900963485366127 ) ) ;
#9613 =( BOUNDED_SURFACE ( )  B_SPLINE_SURFACE ( 3, 1, ( 
 ( #18179, #56367 ),
 ( #13483, #19118 ),
 ( #56673, #38230 ),
 ( #57277, #42308 ) ),
 .UNSPECIFIED., .F., .F., .F. ) 
 B_SPLINE_SURFACE_WITH_KNOTS ( ( 4, 4 ),
 ( 2, 2 ),
 ( 0.000000000000000000, 1.000000000000000000 ),
 ( 0.000000000000000000, 1.000000000000000000 ),
 .UNSPECIFIED. ) 
 GEOMETRIC_REPRESENTATION_ITEM ( )  RATIONAL_B_SPLINE_SURFACE ( (
 ( 1.000000000000000000, 1.000000000000000000),
 ( 0.9754377213608244057, 0.9999580625633939235),
 ( 0.9754377213608244057, 0.9999580625633939235),
 ( 1.000000000000000000, 1.000000000000000000) ) ) 
 REPRESENTATION_ITEM ( '' )  SURFACE ( )  );
#9614 = CARTESIAN_POINT ( 'NONE',  ( 2.301529144917014769, -11.18385659262710696, 46.71331407887419118 ) ) ;
#9615 = EDGE_CURVE ( 'NONE', #31234, #33708, #30222, .T. ) ;
#9617 = CIRCLE ( 'NONE', #23618, 43.08621763946400307 ) ;
#9616 = B_SPLINE_CURVE_WITH_KNOTS ( 'NONE', 3,
 ( #23259, #32358, #18562, #51130 ),
 .UNSPECIFIED., .F., .F.,
 ( 4, 4 ),
 ( 4.336808689942017736E-19, 0.004041751736740987339 ),
 .UNSPECIFIED. ) ;
#9618 = CARTESIAN_POINT ( 'NONE',  ( 0.5807400328401574052, -46.40483864045153695, 11.87003418057227044 ) ) ;
#9619 = EDGE_CURVE ( 'NONE', #54223, #24092, #42541, .T. ) ;
#9621 = EDGE_LOOP ( 'NONE', ( #48967, #45953 ) ) ;
#9620 = CARTESIAN_POINT ( 'NONE',  ( 0.3622758884714730732, 20.83792692158972670, -37.74294673546565804 ) ) ;
#9622 = EDGE_LOOP ( 'NONE', ( #28453, #33189 ) ) ;
#9623 = CARTESIAN_POINT ( 'NONE',  ( 1.000110580585052533, -2.057808565348302032, 41.85908392070087558 ) ) ;
#9624 = ADVANCED_FACE ( 'NONE', ( #3412 ), #27490, .F. ) ;
#9625 = CARTESIAN_POINT ( 'NONE',  ( 50.15149541334723438, 15.27480702088406694, -2.632769263815124994 ) ) ;
#9626 = CARTESIAN_POINT ( 'NONE',  ( -2.339468227445729021, -3.268109542640674547, -1.786138375875142494E-14 ) ) ;
#9627 = CARTESIAN_POINT ( 'NONE',  ( 0.9756008150404608115, 42.52260101821271121, -5.741579752919210300 ) ) ;
#9628 = CARTESIAN_POINT ( 'NONE',  ( 0.6067375320500724145, -11.71046088714719424, -46.44340905096873939 ) ) ;
#9629 = ORIENTED_EDGE ( 'NONE', *, *, #19274, .F. ) ;
#9630 = CARTESIAN_POINT ( 'NONE',  ( 7.000000000000021316, -80.00000000000001421, -1.954818893553044610E-31 ) ) ;
#9631 = EDGE_CURVE ( 'NONE', #32619, #12277, #11611, .T. ) ;
#9632 = CARTESIAN_POINT ( 'NONE',  ( -19.80804008900104307, -7.933751071888869077, 1.058477306457110689 ) ) ;
#9633 = CARTESIAN_POINT ( 'NONE',  ( 0.9730545539215883499, -37.40983423658487794, 21.01499094264535472 ) ) ;
#9634 = EDGE_LOOP ( 'NONE', ( #20675, #36236, #53453, #58942 ) ) ;
#9635 = EDGE_CURVE ( 'NONE', #38949, #9360, #22738, .T. ) ;
#9636 = B_SPLINE_CURVE_WITH_KNOTS ( 'NONE', 3,
 ( #4548, #17759, #61871, #55954 ),
 .UNSPECIFIED., .F., .F.,
 ( 4, 4 ),
 ( 0.000000000000000000, 0.004447772540403829335 ),
 .UNSPECIFIED. ) ;
#9637 = LINE ( 'NONE', #29665, #5518 ) ;
#9638 = CARTESIAN_POINT ( 'NONE',  ( 0.5824936645240094135, -24.92615255297814514, -39.72310534117351466 ) ) ;
#9639 = ORIENTED_EDGE ( 'NONE', *, *, #13375, .T. ) ;
#9640 = CARTESIAN_POINT ( 'NONE',  ( -1.400000000000000799, 0.000000000000000000, 0.000000000000000000 ) ) ;
#9641 = AXIS2_PLACEMENT_3D ( 'NONE', #7413, #2097, #36898 ) ;
#9642 = ORIENTED_EDGE ( 'NONE', *, *, #9425, .F. ) ;
#9643 = CARTESIAN_POINT ( 'NONE',  ( 0.7762783648524368418, -29.86325223096987358, -37.45705264446610272 ) ) ;
#9644 = CARTESIAN_POINT ( 'NONE',  ( 2.500000000000002220, 3.061616997868386099E-16, -5.574599999999999334 ) ) ;
#9645 = AXIS2_PLACEMENT_3D ( 'NONE', #3618, #13063, #22753 ) ;
#9646 = VERTEX_POINT ( 'NONE', #46991 ) ;
#9647 = AXIS2_PLACEMENT_3D ( 'NONE', #37352, #27626, #46755 ) ;
#9648 = DIRECTION ( 'NONE',  ( 0.000000000000000000, 0.000000000000000000, 1.000000000000000000 ) ) ;
#9649 = CARTESIAN_POINT ( 'NONE',  ( 4.291220156522059348, 47.06111669607643933, 2.154133845417246729 ) ) ;
#9650 = CARTESIAN_POINT ( 'NONE',  ( 4.963659409799330291, 40.34793212403968710, 19.36487359954713483 ) ) ;
#9651 = CARTESIAN_POINT ( 'NONE',  ( 4.967162193818130511, 38.44485641567072776, 19.45289607368836116 ) ) ;
#9652 = ORIENTED_EDGE ( 'NONE', *, *, #29175, .T. ) ;
#9653 = CARTESIAN_POINT ( 'NONE',  ( 0.9785694773339252972, -6.751071488010489396, -41.36131573679015361 ) ) ;
#9654 = ORIENTED_EDGE ( 'NONE', *, *, #59977, .F. ) ;
#9655 = CARTESIAN_POINT ( 'NONE',  ( 0.5806925824938502512, -7.260877859417425029, 46.33035738103242096 ) ) ;
#9656 = EDGE_CURVE ( 'NONE', #20911, #39074, #33957, .T. ) ;
#9657 = EDGE_LOOP ( 'NONE', ( #39247, #52628, #38757, #31554 ) ) ;
#9658 = ORIENTED_EDGE ( 'NONE', *, *, #32338, .F. ) ;
#9659 = CARTESIAN_POINT ( 'NONE',  ( 7.000000000000016875, -54.69470952477976056, 58.44237546506787595 ) ) ;
#9661 = AXIS2_PLACEMENT_3D ( 'NONE', #16892, #36007, #30645 ) ;
#9660 = CARTESIAN_POINT ( 'NONE',  ( -2.601141883200662974, -11.68881050534889532, 9.282625514337734529 ) ) ;
#9662 = CARTESIAN_POINT ( 'NONE',  ( 0.8560838555295223751, 46.60258007729417784, 5.345312359546021241 ) ) ;
#9663 = CARTESIAN_POINT ( 'NONE',  ( 5.960221823109900008, 16.28736530777573321, 12.49086489703233482 ) ) ;
#9664 = ORIENTED_EDGE ( 'NONE', *, *, #34726, .T. ) ;
#9665 = CARTESIAN_POINT ( 'NONE',  ( 5.895596859100789899, -4.659086063545737844, -19.56581458219824299 ) ) ;
#9666 = CARTESIAN_POINT ( 'NONE',  ( 2.624215991343620935, -4.864192649745717745, 47.76052319582214523 ) ) ;
#9667 = FACE_OUTER_BOUND ( 'NONE', #49800, .T. ) ;
#9668 = EDGE_LOOP ( 'NONE', ( #56954, #26057, #40425, #47945 ) ) ;
#9669 = VECTOR ( 'NONE', #15946, 1000.000000000000114 ) ;
#9670 = B_SPLINE_CURVE_WITH_KNOTS ( 'NONE', 3,
 ( #37007, #50752, #13489, #8155 ),
 .UNSPECIFIED., .F., .F.,
 ( 4, 4 ),
 ( 1.951563910473907981E-18, 0.004041751736740987339 ),
 .UNSPECIFIED. ) ;
#9671 = ORIENTED_EDGE ( 'NONE', *, *, #59670, .F. ) ;
#9672 = CARTESIAN_POINT ( 'NONE',  ( 0.1081432562775998946, -21.19449538864532556, -37.55692207416018391 ) ) ;
#9673 = CARTESIAN_POINT ( 'NONE',  ( 0.6254311100348648456, 47.60023274471269872, 6.960804577576987562 ) ) ;
#9674 = CARTESIAN_POINT ( 'NONE',  ( 3.680974057930773924, -42.44218549341225355, 22.36814223828894299 ) ) ;
#9675 = CARTESIAN_POINT ( 'NONE',  ( 0.1098349054025746230, -34.34238705454320240, 26.08296594991481854 ) ) ;
#9676 = CARTESIAN_POINT ( 'NONE',  ( 5.959828726073459926, 12.49160845136034936, -16.28681682518051588 ) ) ;
#9677 = EDGE_LOOP ( 'NONE', ( #19779, #12136, #50628, #42564 ) ) ;
#9678 = ORIENTED_EDGE ( 'NONE', *, *, #11192, .T. ) ;
#9679 = DIRECTION ( 'NONE',  ( -1.000000000000000000, -0.000000000000000000, -0.000000000000000000 ) ) ;
#9680 = CARTESIAN_POINT ( 'NONE',  ( 3.727782113643637540, 42.69290976567378237, -10.49253218465454296 ) ) ;
#9681 = CARTESIAN_POINT ( 'NONE',  ( 4.553261556744875094, 0.000000000000000000, 0.000000000000000000 ) ) ;
#9682 = CARTESIAN_POINT ( 'NONE',  ( 4.960156602257181468, -43.79161740034464856, -15.40604254112689731 ) ) ;
#9683 = CARTESIAN_POINT ( 'NONE',  ( 4.553261556744875094, 0.000000000000000000, 0.000000000000000000 ) ) ;
#9684 = FACE_OUTER_BOUND ( 'NONE', #947, .T. ) ;
#9685 = ORIENTED_EDGE ( 'NONE', *, *, #45229, .T. ) ;
#9686 = CARTESIAN_POINT ( 'NONE',  ( 0.1154773475650541087, 20.24948860305302389, -39.20333967101458938 ) ) ;
#9687 = CARTESIAN_POINT ( 'NONE',  ( -6.063463321072276813, -11.02986456480170752, -15.78488327994861962 ) ) ;
#9688 = EDGE_CURVE ( 'NONE', #40342, #50920, #6345, .T. ) ;
#9689 = VECTOR ( 'NONE', #2336, 1000.000000000000000 ) ;
#9690 =( BOUNDED_SURFACE ( )  B_SPLINE_SURFACE ( 3, 1, ( 
 ( #7919, #41773 ),
 ( #17636, #56444 ),
 ( #27336, #3821 ),
 ( #13557, #47370 ) ),
 .UNSPECIFIED., .F., .F., .F. ) 
 B_SPLINE_SURFACE_WITH_KNOTS ( ( 4, 4 ),
 ( 2, 2 ),
 ( 0.000000000000000000, 1.000000000000000000 ),
 ( 0.000000000000000000, 1.000000000000000000 ),
 .UNSPECIFIED. ) 
 GEOMETRIC_REPRESENTATION_ITEM ( )  RATIONAL_B_SPLINE_SURFACE ( (
 ( 1.000000000000000000, 1.000000000000000000),
 ( 0.9952954269826590483, 0.8620686068821307169),
 ( 0.9952954269826590483, 0.8620686068821307169),
 ( 1.000000000000000000, 1.000000000000000000) ) ) 
 REPRESENTATION_ITEM ( '' )  SURFACE ( )  );
#9691 = CARTESIAN_POINT ( 'NONE',  ( 5.896278296736517710, 3.350760724586565154, -19.83177708075985279 ) ) ;
#9692 = CARTESIAN_POINT ( 'NONE',  ( 0.6000166863083106206, 23.17738933882536401, -43.29702189694988590 ) ) ;
#9693 = CIRCLE ( 'NONE', #17708, 2.649999999999992806 ) ;
#9694 = VECTOR ( 'NONE', #20895, 999.9999999999998863 ) ;
#9695 = FACE_OUTER_BOUND ( 'NONE', #29934, .T. ) ;
#9696 = EDGE_CURVE ( 'NONE', #5968, #46746, #45129, .T. ) ;
#9697 = CARTESIAN_POINT ( 'NONE',  ( -4.923482091946715045, -0.9563062221994793610, 5.749747411347113621E-14 ) ) ;
#9698 = FACE_OUTER_BOUND ( 'NONE', #25135, .T. ) ;
#9699 = ORIENTED_EDGE ( 'NONE', *, *, #36793, .F. ) ;
#9700 =( BOUNDED_SURFACE ( )  B_SPLINE_SURFACE ( 3, 1, ( 
 ( #18318, #32722 ),
 ( #18618, #17691 ),
 ( #23317, #56500 ),
 ( #13616, #52110 ) ),
 .UNSPECIFIED., .F., .F., .F. ) 
 B_SPLINE_SURFACE_WITH_KNOTS ( ( 4, 4 ),
 ( 2, 2 ),
 ( 0.000000000000000000, 1.000000000000000000 ),
 ( 0.000000000000000000, 1.000000000000000000 ),
 .UNSPECIFIED. ) 
 GEOMETRIC_REPRESENTATION_ITEM ( )  RATIONAL_B_SPLINE_SURFACE ( (
 ( 1.000000000000000000, 1.000000000000000000),
 ( 0.9953485035131437453, 0.8621029689291523912),
 ( 0.9953485035131437453, 0.8621029689291523912),
 ( 1.000000000000000000, 1.000000000000000000) ) ) 
 REPRESENTATION_ITEM ( '' )  SURFACE ( )  );
#9701 = B_SPLINE_CURVE_WITH_KNOTS ( 'NONE', 3,
 ( #23323, #47747, #726, #23937 ),
 .UNSPECIFIED., .F., .F.,
 ( 4, 4 ),
 ( 0.000000000000000000, 0.005013413432710151114 ),
 .UNSPECIFIED. ) ;
#9702 = CARTESIAN_POINT ( 'NONE',  ( -6.072942160501519027, -12.93525546908854018, -14.26475826077803788 ) ) ;
#9703 = CARTESIAN_POINT ( 'NONE',  ( 4.962356264823608143, -29.56943756613123497, 29.94802096775367772 ) ) ;
#9704 = CARTESIAN_POINT ( 'NONE',  ( 0.6254087463353908971, -23.45485308995630191, 42.00124903776029583 ) ) ;
#9705 = ORIENTED_EDGE ( 'NONE', *, *, #22576, .T. ) ;
#9707 = MANIFOLD_SOLID_BREP ( 'M5 Tapped Hole1', #5024 ) ;
#9706 =( BOUNDED_SURFACE ( )  B_SPLINE_SURFACE ( 3, 1, ( 
 ( #26629, #12554 ),
 ( #2187, #6563 ),
 ( #50437, #40768 ),
 ( #7503, #16310 ) ),
 .UNSPECIFIED., .F., .F., .F. ) 
 B_SPLINE_SURFACE_WITH_KNOTS ( ( 4, 4 ),
 ( 2, 2 ),
 ( 0.000000000000000000, 1.000000000000000000 ),
 ( 0.000000000000000000, 1.000000000000000000 ),
 .UNSPECIFIED. ) 
 GEOMETRIC_REPRESENTATION_ITEM ( )  RATIONAL_B_SPLINE_SURFACE ( (
 ( 1.000000000000000000, 1.000000000000000000),
 ( 0.7223157951917476005, 0.9931996967497186413),
 ( 0.7223157951917476005, 0.9931996967497186413),
 ( 1.000000000000000000, 1.000000000000000000) ) ) 
 REPRESENTATION_ITEM ( '' )  SURFACE ( )  );
#9708 = B_SPLINE_CURVE_WITH_KNOTS ( 'NONE', 3,
 ( #15296, #20905, #39420, #39115 ),
 .UNSPECIFIED., .F., .F.,
 ( 4, 4 ),
 ( 2.602085213965211027E-18, 0.004050076154993003351 ),
 .UNSPECIFIED. ) ;
#9709 = ADVANCED_FACE ( 'NONE', ( #18164 ), #48208, .F. ) ;
#9710 = CARTESIAN_POINT ( 'NONE',  ( 0.9740398440564311811, -36.95080095316289714, 21.81228698783128905 ) ) ;
#9711 = CARTESIAN_POINT ( 'NONE',  ( 2.301430502907644726, -44.85388302506918734, 17.18551536142172154 ) ) ;
#9712 = CIRCLE ( 'NONE', #52672, 47.91270532121795611 ) ;
#9713 = CARTESIAN_POINT ( 'NONE',  ( 0.8557997880470697982, -5.347802024197571669, 47.60865952216997243 ) ) ;
#9714 = ORIENTED_EDGE ( 'NONE', *, *, #38801, .T. ) ;
#9715 = CARTESIAN_POINT ( 'NONE',  ( 4.975801465491694664, -45.55012473237763260, 14.85979367497093762 ) ) ;
#9716 = CARTESIAN_POINT ( 'NONE',  ( 0.5998501479064699549, -12.95623334615470057, -46.33007877220734372 ) ) ;
#9717 = ORIENTED_EDGE ( 'NONE', *, *, #54918, .T. ) ;
#9718 = CARTESIAN_POINT ( 'NONE',  ( 4.956653778116995035, 36.51451553856460919, -31.29546495791814209 ) ) ;
#9719 = ORIENTED_EDGE ( 'NONE', *, *, #25063, .T. ) ;
#9720 = FACE_BOUND ( 'NONE', #40678, .T. ) ;
#9721 = ORIENTED_EDGE ( 'NONE', *, *, #4864, .T. ) ;
#9722 = CARTESIAN_POINT ( 'NONE',  ( 1.227938101723756947, 0.8460948827225182045, 42.91134962331487657 ) ) ;
#9723 = DIRECTION ( 'NONE',  ( 1.000000000000000000, 0.000000000000000000, 0.000000000000000000 ) ) ;
#9724 = ORIENTED_EDGE ( 'NONE', *, *, #59905, .T. ) ;
#9725 = CARTESIAN_POINT ( 'NONE',  ( 5.960221823109900008, 20.52559243573973546, 0.005450390361793623108 ) ) ;
#9726 = VERTEX_POINT ( 'NONE', #9362 ) ;
#9727 = CARTESIAN_POINT ( 'NONE',  ( 0.5809828226811553087, 0.5448590168532381206, 47.89273459658653564 ) ) ;
#9728 = CARTESIAN_POINT ( 'NONE',  ( -6.017396004339686577, -18.20140164570665675, -4.875835690939370970 ) ) ;
#9729 = ADVANCED_FACE ( 'NONE', ( #13465 ), #38739, .F. ) ;
#9730 = B_SPLINE_CURVE_WITH_KNOTS ( 'NONE', 3,
 ( #49212, #57656, #47995, #29178, #10082, #43619 ),
 .UNSPECIFIED., .F., .F.,
 ( 4, 2, 4 ),
 ( 1.525179609227833153E-16, 0.0002445252820015225508, 0.0004890505640028926628 ),
 .UNSPECIFIED. ) ;
#9731 = VECTOR ( 'NONE', #57617, 1000.000000000000000 ) ;
#9732 = ORIENTED_EDGE ( 'NONE', *, *, #57586, .F. ) ;
#9733 = B_SPLINE_CURVE_WITH_KNOTS ( 'NONE', 3,
 ( #19146, #39184, #29747, #616 ),
 .UNSPECIFIED., .F., .F.,
 ( 4, 4 ),
 ( 0.000000000000000000, 0.004442905043737214836 ),
 .UNSPECIFIED. ) ;
#9734 = CARTESIAN_POINT ( 'NONE',  ( 5.895596859100789899, -19.93390588528919949, -2.677233529022096992 ) ) ;
#9735 = AXIS2_PLACEMENT_3D ( 'NONE', #42965, #9109, #57313 ) ;
#9736 = CARTESIAN_POINT ( 'NONE',  ( 0.5824936645240106348, 16.51438908705373265, 43.89206229059765008 ) ) ;
#9737 = ORIENTED_EDGE ( 'NONE', *, *, #28548, .F. ) ;
#9738 = DIRECTION ( 'NONE',  ( -1.000000000000000000, -0.000000000000000000, -0.000000000000000000 ) ) ;
#9739 = CARTESIAN_POINT ( 'NONE',  ( 5.571549742892842438, -9.254395351074542475, -1.199999999999999956 ) ) ;
#9740 = VERTEX_POINT ( 'NONE', #20622 ) ;
#9741 = CARTESIAN_POINT ( 'NONE',  ( 0.8560838555295223751, 46.35895890951135812, -7.156798369939577853 ) ) ;
#9742 = EDGE_CURVE ( 'NONE', #21941, #5232, #9506, .T. ) ;
#9743 = ORIENTED_EDGE ( 'NONE', *, *, #57307, .T. ) ;
#9744 = CARTESIAN_POINT ( 'NONE',  ( 1.000433927950265423, 25.38714267670817293, 33.34533946993654752 ) ) ;
#9745 = CARTESIAN_POINT ( 'NONE',  ( 0.1140933569871964842, 24.93221288801916202, 36.40514675963271429 ) ) ;
#9746 = ORIENTED_EDGE ( 'NONE', *, *, #9619, .T. ) ;
#9747 = CARTESIAN_POINT ( 'NONE',  ( 0.5817217712918344441, 4.240847850817598186, 46.70385598122052784 ) ) ;
#9748 = LINE ( 'NONE', #646, #37303 ) ;
#9749 = EDGE_CURVE ( 'NONE', #26754, #37717, #25681, .T. ) ;
#9750 = CARTESIAN_POINT ( 'NONE',  ( -6.016761891674565099, -18.68153697670640057, -2.462934516564000198 ) ) ;
#9751 = FACE_OUTER_BOUND ( 'NONE', #47596, .T. ) ;
#9752 = VERTEX_POINT ( 'NONE', #10928 ) ;
#9753 = CARTESIAN_POINT ( 'NONE',  ( 0.6023143664670691511, 18.65155446683251839, -44.34466302085804301 ) ) ;
#9754 = CARTESIAN_POINT ( 'NONE',  ( -2.708315649062916552, -14.20182604343557742, -3.532515819624296061 ) ) ;
#9755 = CARTESIAN_POINT ( 'NONE',  ( 0.6846871229502899947, 24.69859318104488821, 41.05093867799194385 ) ) ;
#9756 = B_SPLINE_CURVE_WITH_KNOTS ( 'NONE', 3,
 ( #47834, #28708, #33429, #57490 ),
 .UNSPECIFIED., .F., .F.,
 ( 4, 4 ),
 ( 7.046480070129584215E-18, 0.005014147105413696917 ),
 .UNSPECIFIED. ) ;
#9757 = CARTESIAN_POINT ( 'NONE',  ( -6.016104459813371719, 0.005335450885065978234, 18.84322058118302579 ) ) ;
#9758 = LINE ( 'NONE', #5038, #18868 ) ;
#9759 = CARTESIAN_POINT ( 'NONE',  ( 2.359973842542475886, -8.511856589336208145, -43.19356655840164905 ) ) ;
#9760 = EDGE_CURVE ( 'NONE', #45826, #6741, #22690, .T. ) ;
#9761 = AXIS2_PLACEMENT_3D ( 'NONE', #41863, #60931, #18043 ) ;
#9762 = CARTESIAN_POINT ( 'NONE',  ( 0.8557997880470697982, 38.55640757422439435, 28.43566216844983074 ) ) ;
#9763 = CARTESIAN_POINT ( 'NONE',  ( 0.9790320750461907195, -12.49859903051836696, 40.00152690606341821 ) ) ;
#9764 = ADVANCED_FACE ( 'NONE', ( #886 ), #20928, .T. ) ;
#9765 = CARTESIAN_POINT ( 'NONE',  ( 0.3676999524040323597, 14.45783756353398175, 41.67639039443440652 ) ) ;
#9766 = CARTESIAN_POINT ( 'NONE',  ( 0.6028618097248863439, 48.10721794025128162, -0.1745704727160814207 ) ) ;
#9767 = CARTESIAN_POINT ( 'NONE',  ( 0.6543461111163461075, 4.241015250120812929, -5.460849780464856806 ) ) ;
#9768 = B_SPLINE_CURVE_WITH_KNOTS ( 'NONE', 3,
 ( #40195, #8179, #36106, #21988, #59246, #21670 ),
 .UNSPECIFIED., .F., .F.,
 ( 4, 2, 4 ),
 ( 2.032917020132191951E-17, 0.0002293755540694313185, 0.0004587511081388423082 ),
 .UNSPECIFIED. ) ;
#9769 = CARTESIAN_POINT ( 'NONE',  ( 0.1135584504625007790, 39.56526998914637261, 19.53308636189390057 ) ) ;
#9770 = CARTESIAN_POINT ( 'NONE',  ( 0.6001305935487315502, -11.94532529598346038, -46.60388846085719194 ) ) ;
#9771 = DIRECTION ( 'NONE',  ( 1.000000000000000000, 0.000000000000000000, 0.000000000000000000 ) ) ;
#9772 = EDGE_CURVE ( 'NONE', #38048, #30064, #42909, .T. ) ;
#9773 = CARTESIAN_POINT ( 'NONE',  ( 0.6252788684277226228, -45.77085809703806518, -17.78968465809531807 ) ) ;
#9774 = CARTESIAN_POINT ( 'NONE',  ( 0.5837800304671210139, 45.24177268675465768, -12.34582262708807754 ) ) ;
#9775 = CARTESIAN_POINT ( 'NONE',  ( 3.661933894777869014, 15.13536249802464262, 44.53708529983796183 ) ) ;
#9776 = VERTEX_POINT ( 'NONE', #5565 ) ;
#9777 = B_SPLINE_CURVE_WITH_KNOTS ( 'NONE', 3,
 ( #57324, #9426, #42976, #24772, #43915, #20086 ),
 .UNSPECIFIED., .F., .F.,
 ( 4, 2, 4 ),
 ( 1.266794085606387986E-16, 0.0002450741128632346190, 0.0004901482257263424947 ),
 .UNSPECIFIED. ) ;
#9778 = AXIS2_PLACEMENT_3D ( 'NONE', #51653, #51965, #61961 ) ;
#9779 = CARTESIAN_POINT ( 'NONE',  ( 0.3676999524040323597, -44.10520818713899871, -0.8253448321555690859 ) ) ;
#9780 = CARTESIAN_POINT ( 'NONE',  ( 0.6252788684277188480, -7.158686030355511321, 48.58186436822340681 ) ) ;
#9781 = CONICAL_SURFACE ( 'NONE', #61622, 42.08604991992415023, 1.569615340895231137 ) ;
#9782 = CARTESIAN_POINT ( 'NONE',  ( 0.5807400328401574052, -46.12278621143487811, -12.92266817606063256 ) ) ;
#9783 = ORIENTED_EDGE ( 'NONE', *, *, #44718, .F. ) ;
#9784 = EDGE_CURVE ( 'NONE', #3346, #38797, #7013, .T. ) ;
#9785 = CARTESIAN_POINT ( 'NONE',  ( 0.9754642270333678811, 5.426415525315814392, 42.56393738774954016 ) ) ;
#9786 = CARTESIAN_POINT ( 'NONE',  ( 5.960221823109900008, -16.28736530777599611, 12.49086489703200442 ) ) ;
#9787 =( BOUNDED_SURFACE ( )  B_SPLINE_SURFACE ( 3, 1, ( 
 ( #13622, #51809 ),
 ( #43369, #8908 ),
 ( #23322, #47138 ),
 ( #42749, #4181 ) ),
 .UNSPECIFIED., .F., .F., .F. ) 
 B_SPLINE_SURFACE_WITH_KNOTS ( ( 4, 4 ),
 ( 2, 2 ),
 ( 0.000000000000000000, 1.000000000000000000 ),
 ( 0.000000000000000000, 1.000000000000000000 ),
 .UNSPECIFIED. ) 
 GEOMETRIC_REPRESENTATION_ITEM ( )  RATIONAL_B_SPLINE_SURFACE ( (
 ( 1.000000000000000000, 1.000000000000000000),
 ( 0.9952954269826590483, 0.8620686068821339365),
 ( 0.9952954269826590483, 0.8620686068821339365),
 ( 1.000000000000000000, 1.000000000000000000) ) ) 
 REPRESENTATION_ITEM ( '' )  SURFACE ( )  );
#9788 = UNCERTAINTY_MEASURE_WITH_UNIT (LENGTH_MEASURE( 1.000000000000000082E-05 ), #33208, 'distance_accuracy_value', 'NONE');
#9789 = VERTEX_POINT ( 'NONE', #43524 ) ;
#9790 = ORIENTED_EDGE ( 'NONE', *, *, #22745, .F. ) ;
#9791 = CARTESIAN_POINT ( 'NONE',  ( 0.9754402186311935674, -11.28658745892489890, -41.39745964575707404 ) ) ;
#9792 = VERTEX_POINT ( 'NONE', #19704 ) ;
#9793 = CARTESIAN_POINT ( 'NONE',  ( 0.9762797500689124330, -41.84568905980458453, 2.294143041716202092 ) ) ;
#9794 = ORIENTED_EDGE ( 'NONE', *, *, #16249, .F. ) ;
#9795 = EDGE_LOOP ( 'NONE', ( #30879, #24084, #1625, #110 ) ) ;
#9796 = DIRECTION ( 'NONE',  ( 0.000000000000000000, 0.000000000000000000, -1.000000000000000000 ) ) ;
#9797 = VERTEX_POINT ( 'NONE', #57885 ) ;
#9798 = CARTESIAN_POINT ( 'NONE',  ( 0.1365634738349406074, -23.41534997664304285, 37.39764705291722180 ) ) ;
#9799 = CARTESIAN_POINT ( 'NONE',  ( 5.880360259849739535, -26.69116321728542829, -39.86101557989661615 ) ) ;
#9800 = CONICAL_SURFACE ( 'NONE', #44852, 43.08621763946400307, 1.568696531533066763 ) ;
#9801 = CARTESIAN_POINT ( 'NONE',  ( 3.660087539127323097, -45.87884541725755838, 14.24113226412033661 ) ) ;
#9802 = VERTEX_POINT ( 'NONE', #15319 ) ;
#9803 = CARTESIAN_POINT ( 'NONE',  ( 4.962356264823608143, 0.000000000000000000, 0.000000000000000000 ) ) ;
#9804 = B_SPLINE_CURVE_WITH_KNOTS ( 'NONE', 3,
 ( #8605, #27734, #13645, #7676 ),
 .UNSPECIFIED., .F., .F.,
 ( 4, 4 ),
 ( 3.954366397011470641E-18, 0.004042984057420973693 ),
 .UNSPECIFIED. ) ;
#9805 = CARTESIAN_POINT ( 'NONE',  ( 0.9780303403264770656, -39.48244899217856840, 14.05260954325215472 ) ) ;
#9806 = VERTEX_POINT ( 'NONE', #29699 ) ;
#9807 = AXIS2_PLACEMENT_3D ( 'NONE', #19182, #42679, #10392 ) ;
#9808 = VERTEX_POINT ( 'NONE', #21856 ) ;
#9809 = EDGE_CURVE ( 'NONE', #50058, #26084, #40680, .T. ) ;
#9810 = FACE_OUTER_BOUND ( 'NONE', #24653, .T. ) ;
#9811 = VERTEX_POINT ( 'NONE', #8055 ) ;
#9812 = CARTESIAN_POINT ( 'NONE',  ( 0.6029443199889047422, 46.60567665519338476, 15.47412502747618035 ) ) ;
#9813 = DIRECTION ( 'NONE',  ( -0.8191520442889896891, 0.000000000000000000, -0.5735764363510490460 ) ) ;
#9814 = CARTESIAN_POINT ( 'NONE',  ( 0.9757402383260949108, -0.08489923450668514227, 42.90839848328079853 ) ) ;
#9815 = CARTESIAN_POINT ( 'NONE',  ( 0.9730545539215883499, -0.5054011016609686324, -42.90536227157002713 ) ) ;
#9816 = EDGE_CURVE ( 'NONE', #23687, #10199, #35665, .T. ) ;
#9817 = VERTEX_POINT ( 'NONE', #54728 ) ;
#9818 = CARTESIAN_POINT ( 'NONE',  ( 0.5998501479064708430, -12.95623334615534716, 46.33007877220716608 ) ) ;
#9819 = CARTESIAN_POINT ( 'NONE',  ( 4.975610109902397937, 34.73360008816180056, -34.43873447229760387 ) ) ;
#9820 = EDGE_CURVE ( 'NONE', #34877, #31646, #17524, .T. ) ;
#9821 = CARTESIAN_POINT ( 'NONE',  ( 5.910764540655178756, 10.83508461757070229, 16.94408981914477863 ) ) ;
#9822 = ORIENTED_EDGE ( 'NONE', *, *, #19455, .T. ) ;
#9823 = CARTESIAN_POINT ( 'NONE',  ( 0.1129192098497447394, 33.28205046155626690, -28.96993104685574139 ) ) ;
#9824 = EDGE_CURVE ( 'NONE', #8650, #9811, #36923, .T. ) ;
#9825 = CARTESIAN_POINT ( 'NONE',  ( 0.7048096507298579061, -46.68221792389248037, 11.63498350884255750 ) ) ;
#9826 = CARTESIAN_POINT ( 'NONE',  ( 0.6029443449137436017, -35.24599845889794381, -34.19443128081963579 ) ) ;
#9827 = VECTOR ( 'NONE', #60704, 1000.000000000000000 ) ;
#9828 = CONICAL_SURFACE ( 'NONE', #44869, 42.92674063221959813, 1.485477209440487556 ) ;
#9829 = ORIENTED_EDGE ( 'NONE', *, *, #4629, .F. ) ;
#9830 = ORIENTED_EDGE ( 'NONE', *, *, #48672, .F. ) ;
#9831 = CARTESIAN_POINT ( 'NONE',  ( 1.088908134280555773, 39.34174992079780253, -17.14055988408877340 ) ) ;
#9832 = CARTESIAN_POINT ( 'NONE',  ( 4.549368137175248350, 0.000000000000000000, 0.000000000000000000 ) ) ;
#9833 = CARTESIAN_POINT ( 'NONE',  ( 3.661921753702002569, -31.78300939732352859, -34.67666993071396320 ) ) ;
#9834 = B_SPLINE_CURVE_WITH_KNOTS ( 'NONE', 3,
 ( #4128, #56452, #23267, #51756 ),
 .UNSPECIFIED., .F., .F.,
 ( 4, 4 ),
 ( 0.000000000000000000, 0.005013413432710142441 ),
 .UNSPECIFIED. ) ;
#9835 = CARTESIAN_POINT ( 'NONE',  ( 0.6001305935487315502, -24.50730504006429200, -41.40054608060284380 ) ) ;
#9836 = PRODUCT_DEFINITION_SHAPE ( 'NONE', 'NONE',  #61990 ) ;
#9837 = FACE_OUTER_BOUND ( 'NONE', #31442, .T. ) ;
#9838 = CARTESIAN_POINT ( 'NONE',  ( -5.995132425357893702, -2.468096378288251458, 18.68182899165010724 ) ) ;
#9839 = SURFACE_STYLE_FILL_AREA ( #34821 ) ;
#9840 = CARTESIAN_POINT ( 'NONE',  ( -6.072942160501519915, -14.65319399899862596, 12.49352103759107813 ) ) ;
#9841 = CARTESIAN_POINT ( 'NONE',  ( 0.8557997880470599172, 46.03118133706026072, 13.27832040216655507 ) ) ;
#9842 = CARTESIAN_POINT ( 'NONE',  ( 5.974727161628367256, 20.35137732084672635, 2.663664384318852996 ) ) ;
#9843 = EDGE_CURVE ( 'NONE', #47838, #15681, #28673, .T. ) ;
#9844 = CARTESIAN_POINT ( 'NONE',  ( 0.6030672727741701600, -18.32928433899722975, -44.47882233696916643 ) ) ;
#9845 = CARTESIAN_POINT ( 'NONE',  ( 9.999999999999994671, 56.56854249492450037, -56.56854249492312192 ) ) ;
#9846 = VERTEX_POINT ( 'NONE', #31558 ) ;
#9847 = CIRCLE ( 'NONE', #25848, 15.38218000000000174 ) ;
#9848 = EDGE_CURVE ( 'NONE', #26701, #25227, #25509, .T. ) ;
#9849 = CARTESIAN_POINT ( 'NONE',  ( -6.016761891674564211, 2.456125503350979677, -18.68243340030200272 ) ) ;
#9850 = CARTESIAN_POINT ( 'NONE',  ( 0.1100053167205930771, -34.32189548568265991, -26.10991185395875291 ) ) ;
#9851 = CARTESIAN_POINT ( 'NONE',  ( 0.1158403557922069033, -35.38432672690284164, 26.36076116631703314 ) ) ;
#9852 = CARTESIAN_POINT ( 'NONE',  ( 0.3676999524040323597, -26.85386693986589890, -34.99743438737782242 ) ) ;
#9853 = CARTESIAN_POINT ( 'NONE',  ( -6.015611763856276717, 7.216738110653516891, -17.40650793417836439 ) ) ;
#9855 = B_SPLINE_CURVE_WITH_KNOTS ( 'NONE', 3,
 ( #36017, #11577, #16267, #41034 ),
 .UNSPECIFIED., .F., .F.,
 ( 4, 4 ),
 ( 3.469446951953614189E-18, 0.004042984057420975427 ),
 .UNSPECIFIED. ) ;
#9854 = CARTESIAN_POINT ( 'NONE',  ( 0.5998501479064708430, -46.60114184914326074, 11.94461217097388328 ) ) ;
#9856 = CONTEXT_DEPENDENT_SHAPE_REPRESENTATION ( #42406, #40815 ) ;
#9857 = CARTESIAN_POINT ( 'NONE',  ( 0.1129192098497447394, 44.06201484046244587, 2.343210614524684487 ) ) ;
#9858 = EDGE_CURVE ( 'NONE', #57398, #23436, #30891, .T. ) ;
#9859 = CARTESIAN_POINT ( 'NONE',  ( 0.6016117650947689910, 22.40470300146127514, -43.69874526414702132 ) ) ;
#9860 = DIRECTION ( 'NONE',  ( 1.000000000000000000, 0.000000000000000000, 0.000000000000000000 ) ) ;
#9861 = CARTESIAN_POINT ( 'NONE',  ( 4.956653778116488773, 2.599733001513538255, 48.02038484091099235 ) ) ;
#9862 = DIRECTION ( 'NONE',  ( 0.07439287786467664587, 0.1170659376278770925, 0.9903339163990684257 ) ) ;
#9864 = ORIENTED_EDGE ( 'NONE', *, *, #36688, .F. ) ;
#9863 = DIRECTION ( 'NONE',  ( 0.09722883295013594329, -0.1662994675516027976, -0.9812701162958178402 ) ) ;
#9865 = ORIENTED_EDGE ( 'NONE', *, *, #10807, .F. ) ;
#9866 = CARTESIAN_POINT ( 'NONE',  ( 5.896782393890504181, 19.70854070425251692, -4.012419492878830596 ) ) ;
#9867 = CARTESIAN_POINT ( 'NONE',  ( 0.5824935313925952984, -7.440769710676105042, 46.30197752976132364 ) ) ;
#9868 = AXIS2_PLACEMENT_3D ( 'NONE', #18102, #56295, #4898 ) ;
#9869 = CARTESIAN_POINT ( 'NONE',  ( 2.299746137290199943, -48.44936871168312820, 7.545860396635869272 ) ) ;
#9870 = EDGE_CURVE ( 'NONE', #19741, #26818, #59747, .T. ) ;
#9871 = VERTEX_POINT ( 'NONE', #45675 ) ;
#9872 = CARTESIAN_POINT ( 'NONE',  ( 0.5837800005270550319, 22.53739213693909704, 41.12543269447289163 ) ) ;
#9873 = DIRECTION ( 'NONE',  ( 1.000000000000000000, 0.000000000000000000, 0.000000000000000000 ) ) ;
#9874 = DIRECTION ( 'NONE',  ( 0.000000000000000000, 0.000000000000000000, 1.000000000000000000 ) ) ;
#9876 = EDGE_CURVE ( 'NONE', #20738, #20913, #246, .T. ) ;
#9875 = ORIENTED_EDGE ( 'NONE', *, *, #55439, .F. ) ;
#9877 = ORIENTED_EDGE ( 'NONE', *, *, #26281, .F. ) ;
#9878 = CARTESIAN_POINT ( 'NONE',  ( 0.1310142868023669305, 17.08943085418587415, -39.59283406808313543 ) ) ;
#9879 = CIRCLE ( 'NONE', #2881, 47.09074272231896430 ) ;
#9880 = CARTESIAN_POINT ( 'NONE',  ( 4.967162193818130511, -42.16965968614187688, -8.839793687085657936 ) ) ;
#9881 = CARTESIAN_POINT ( 'NONE',  ( 0.5837157313716013762, 16.93971847026775279, -43.72965814787597338 ) ) ;
#9882 = CARTESIAN_POINT ( 'NONE',  ( 0.6845945791218023269, -35.36481895536415720, -30.81778870990359209 ) ) ;
#9883 = B_SPLINE_CURVE_WITH_KNOTS ( 'NONE', 3,
 ( #28263, #57985, #52064, #15107, #42392, #18569 ),
 .UNSPECIFIED., .F., .F.,
 ( 4, 2, 4 ),
 ( 0.000000000000000000, 0.0002447195606305764808, 0.0004894391212611529617 ),
 .UNSPECIFIED. ) ;
#9884 = CARTESIAN_POINT ( 'NONE',  ( 0.09136607875274982415, 9.539392014169456147, -3.000000000000000000 ) ) ;
#9885 = CARTESIAN_POINT ( 'NONE',  ( 0.000000000000000000, 0.000000000000000000, -1.199999999999999956 ) ) ;
#9886 = ORIENTED_EDGE ( 'NONE', *, *, #46634, .F. ) ;
#9887 = ORIENTED_EDGE ( 'NONE', *, *, #11183, .T. ) ;
#9888 = CARTESIAN_POINT ( 'NONE',  ( 3.680882792899937250, 22.36818923730770337, -42.44216617524794799 ) ) ;
#9889 = CARTESIAN_POINT ( 'NONE',  ( 4.335381028904201628, -48.26758661664241856, -8.366416787924562115 ) ) ;
#9890 = VECTOR ( 'NONE', #28402, 999.9999999999998863 ) ;
#9891 = ORIENTED_EDGE ( 'NONE', *, *, #52458, .T. ) ;
#9892 = CARTESIAN_POINT ( 'NONE',  ( 0.1139756605157205421, 41.74945270199659575, -14.28070092043005701 ) ) ;
#9893 = CARTESIAN_POINT ( 'NONE',  ( -2.708315649062916552, 8.698422600177121211, -11.76894112707803863 ) ) ;
#9894 = CARTESIAN_POINT ( 'NONE',  ( 4.975610109902397937, -40.67634447773578898, -27.16402781375298403 ) ) ;
#9895 = CARTESIAN_POINT ( 'NONE',  ( 4.962356264823597485, -9.332162870646813602, 41.03835198954837438 ) ) ;
#9896 = ADVANCED_FACE ( 'NONE', ( #36905 ), #41292, .F. ) ;
#9897 = ORIENTED_EDGE ( 'NONE', *, *, #19326, .T. ) ;
#9898 = ORIENTED_EDGE ( 'NONE', *, *, #30008, .T. ) ;
#9899 = DIRECTION ( 'NONE',  ( -1.000000000000000000, -0.000000000000000000, -0.000000000000000000 ) ) ;
#9900 = CARTESIAN_POINT ( 'NONE',  ( 0.9756008150404585910, -42.55970871350807982, -5.459718823765970619 ) ) ;
#9901 = EDGE_CURVE ( 'NONE', #15368, #32472, #50651, .T. ) ;
#9902 = CARTESIAN_POINT ( 'NONE',  ( 0.1084644655670284202, -37.54424727804286022, -21.21700107124035029 ) ) ;
#9903 = AXIS2_PLACEMENT_3D ( 'NONE', #4897, #61902, #19045 ) ;
#9904 = CARTESIAN_POINT ( 'NONE',  ( 4.975610109902397937, -46.59897809419055648, 14.86555238512586463 ) ) ;
#9905 = ORIENTED_EDGE ( 'NONE', *, *, #22654, .F. ) ;
#9906 = CARTESIAN_POINT ( 'NONE',  ( -6.017396004339687465, 13.32495836419643176, -13.32329839588541098 ) ) ;
#9908 = VERTEX_POINT ( 'NONE', #55969 ) ;
#9907 = EDGE_CURVE ( 'NONE', #18903, #22826, #14541, .T. ) ;
#9909 = CARTESIAN_POINT ( 'NONE',  ( 0.8560838555295158248, -44.00447048317951726, -16.24744323198929052 ) ) ;
#9910 = CARTESIAN_POINT ( 'NONE',  ( 0.5980894510889457338, -42.01322166096903743, -23.44630161211571462 ) ) ;
#9911 = EDGE_CURVE ( 'NONE', #14140, #14065, #52633, .T. ) ;
#9912 = ORIENTED_EDGE ( 'NONE', *, *, #16853, .F. ) ;
#9913 = CARTESIAN_POINT ( 'NONE',  ( 5.896278296736517710, -17.30234040492943492, 10.25455977242953409 ) ) ;
#9914 = ADVANCED_FACE ( 'NONE', ( #45998 ), #22491, .F. ) ;
#9915 = CARTESIAN_POINT ( 'NONE',  ( 0.6845945791218034371, 27.12315006394041816, 38.27193817045215241 ) ) ;
#9916 = CARTESIAN_POINT ( 'NONE',  ( 4.975801465491695552, -27.09127437476353251, -39.51822597168487050 ) ) ;
#9917 = B_SPLINE_CURVE_WITH_KNOTS ( 'NONE', 3,
 ( #60608, #17727, #36854, #31829 ),
 .UNSPECIFIED., .F., .F.,
 ( 4, 4 ),
 ( 0.000000000000000000, 0.004444103432399269631 ),
 .UNSPECIFIED. ) ;
#9918 = VERTEX_POINT ( 'NONE', #31252 ) ;
#9919 = DIRECTION ( 'NONE',  ( 0.07906939808003035641, -0.9145849808368756717, -0.3965883799544224764 ) ) ;
#9920 = CARTESIAN_POINT ( 'NONE',  ( 5.838029081930957709, 19.86434078294020011, -42.85408992630853220 ) ) ;
#9921 = CARTESIAN_POINT ( 'NONE',  ( 0.9722240741986386547, 26.58024228478344853, -33.68410525900254271 ) ) ;
#9922 = EDGE_CURVE ( 'NONE', #29558, #51387, #9254, .T. ) ;
#9923 = DIRECTION ( 'NONE',  ( -0.07906939808003035641, 0.7873210066865946599, 0.6114520935586604811 ) ) ;
#9924 =( BOUNDED_SURFACE ( )  B_SPLINE_SURFACE ( 3, 1, ( 
 ( #46446, #47356 ),
 ( #46142, #12935 ),
 ( #52037, #4400 ),
 ( #41753, #46756 ) ),
 .UNSPECIFIED., .F., .F., .F. ) 
 B_SPLINE_SURFACE_WITH_KNOTS ( ( 4, 4 ),
 ( 2, 2 ),
 ( 0.000000000000000000, 1.000000000000000000 ),
 ( 0.000000000000000000, 1.000000000000000000 ),
 .UNSPECIFIED. ) 
 GEOMETRIC_REPRESENTATION_ITEM ( )  RATIONAL_B_SPLINE_SURFACE ( (
 ( 1.000000000000000000, 1.000000000000000000),
 ( 0.9754377213608244057, 0.9999580625633939235),
 ( 0.9754377213608244057, 0.9999580625633939235),
 ( 1.000000000000000000, 1.000000000000000000) ) ) 
 REPRESENTATION_ITEM ( '' )  SURFACE ( )  );
#9925 = CARTESIAN_POINT ( 'NONE',  ( 0.8560838555295223751, -24.46533024579953164, 40.02274915651970133 ) ) ;
#9926 = ORIENTED_EDGE ( 'NONE', *, *, #41681, .T. ) ;
#9927 = CARTESIAN_POINT ( 'NONE',  ( 0.5838002273316450497, -24.06583301632231908, 41.41085122398241936 ) ) ;
#9928 = CARTESIAN_POINT ( 'NONE',  ( 5.895881250540457863, 19.70893872444546702, 4.010662783674901810 ) ) ;
#9929 = DIRECTION ( 'NONE',  ( 1.000000000000000000, 0.000000000000000000, 0.000000000000000000 ) ) ;
#9930 = VERTEX_POINT ( 'NONE', #50349 ) ;
#9931 = AXIS2_PLACEMENT_3D ( 'NONE', #46411, #56088, #42336 ) ;
#9932 = CARTESIAN_POINT ( 'NONE',  ( 0.9741495583595173313, -30.61921547032174828, 30.05988007970385212 ) ) ;
#9933 = CARTESIAN_POINT ( 'NONE',  ( 0.5839254010752165103, 0.09079837481677424660, -47.89590033178483708 ) ) ;
#9934 = CARTESIAN_POINT ( 'NONE',  ( 0.8751705887134423323, -28.56654290188627243, -38.69254731947824411 ) ) ;
#9935 = CARTESIAN_POINT ( 'NONE',  ( 10.00000000000000533, -2.774815975767171530E-13, 80.00000000000001421 ) ) ;
#9936 = CARTESIAN_POINT ( 'NONE',  ( 0.5809828226811617480, 46.11980934799338883, 12.92184523170220345 ) ) ;
#9937 = CARTESIAN_POINT ( 'NONE',  ( 0.6067099128993264090, -28.59222530349251556, 38.42667919752394567 ) ) ;
#9938 = B_SPLINE_CURVE_WITH_KNOTS ( 'NONE', 3,
 ( #15456, #58331, #33959, #24853 ),
 .UNSPECIFIED., .F., .F.,
 ( 4, 4 ),
 ( 4.336808689942017255E-19, 0.004048833967417088224 ),
 .UNSPECIFIED. ) ;
#9939 = CARTESIAN_POINT ( 'NONE',  ( 0.1129192098497447394, 3.754263797494919341, -43.96427289429421137 ) ) ;
#9940 = CARTESIAN_POINT ( 'NONE',  ( 0.6030672727741701600, 47.68443224372862943, 6.365785297724940506 ) ) ;
#9941 = DIRECTION ( 'NONE',  ( 0.000000000000000000, 0.000000000000000000, 1.000000000000000000 ) ) ;
#9942 = DIRECTION ( 'NONE',  ( -1.000000000000000000, -0.000000000000000000, -0.000000000000000000 ) ) ;
#9944 = VERTEX_POINT ( 'NONE', #4563 ) ;
#9943 = CARTESIAN_POINT ( 'NONE',  ( -79.49999999999975842, -5.510910596163058790E-15, 1.848892746611746419E-29 ) ) ;
#9945 = VERTEX_POINT ( 'NONE', #33428 ) ;
#9946 = AXIS2_PLACEMENT_3D ( 'NONE', #56969, #14091, #23465 ) ;
#9947 = CARTESIAN_POINT ( 'NONE',  ( 1.231276596079887264, 28.52807286890788419, -30.71523773966838888 ) ) ;
#9948 = CARTESIAN_POINT ( 'NONE',  ( 5.959547316686252039, -20.52562247508876681, -0.003562808152834123603 ) ) ;
#9949 = ADVANCED_FACE ( 'NONE', ( #38141 ), #57455, .T. ) ;
#9950 = CARTESIAN_POINT ( 'NONE',  ( 0.9972139404380306882, 30.80335716430317206, 29.87264297738535745 ) ) ;
#9951 = CARTESIAN_POINT ( 'NONE',  ( 4.833616638992205949, 26.07076047129135787, -38.20222678111910852 ) ) ;
#9952 = CARTESIAN_POINT ( 'NONE',  ( 0.5804410086790514622, 27.37779091617001370, -38.07855586029853612 ) ) ;
#9953 = CARTESIAN_POINT ( 'NONE',  ( 4.960156602257184133, 9.558288641081755799, 45.42786611289316312 ) ) ;
#9954 = EDGE_CURVE ( 'NONE', #61199, #14671, #27244, .T. ) ;
#9955 = VERTEX_POINT ( 'NONE', #4258 ) ;
#9956 = CARTESIAN_POINT ( 'NONE',  ( 4.956445790443988919, 44.65954324082213134, 14.93530206124989945 ) ) ;
#9957 = CARTESIAN_POINT ( 'NONE',  ( 4.322998006666179727, -27.50295597456480934, 39.32552843303803058 ) ) ;
#9958 = DIRECTION ( 'NONE',  ( 0.09722883295013595717, -0.9607671998409456071, -0.2597555422949489046 ) ) ;
#9959 = ORIENTED_EDGE ( 'NONE', *, *, #44454, .F. ) ;
#9960 = CARTESIAN_POINT ( 'NONE',  ( 0.8554163680231816613, 5.604726001788831624, 46.58103175710786559 ) ) ;
#9961 = CARTESIAN_POINT ( 'NONE',  ( 0.5836750258453364815, 47.50958153310759258, -6.071582023533789396 ) ) ;
#9962 = ORIENTED_EDGE ( 'NONE', *, *, #60027, .T. ) ;
#9963 = VECTOR ( 'NONE', #10105, 1000.000000000000000 ) ;
#9964 = DIRECTION ( 'NONE',  ( 0.9997530559290660479, -0.02222222222222222307, 0.000000000000000000 ) ) ;
#9965 = EDGE_LOOP ( 'NONE', ( #44143, #39711, #36937, #41503 ) ) ;
#9966 = CARTESIAN_POINT ( 'NONE',  ( 51.35572961735444153, 15.29490605596151553, -2.514040278272794637 ) ) ;
#9968 = CARTESIAN_POINT ( 'NONE',  ( 0.6027935024548037868, 33.89348162668930087, 34.14031893787236527 ) ) ;
#9967 = CIRCLE ( 'NONE', #19997, 42.08604991992415023 ) ;
#9969 = B_SPLINE_CURVE_WITH_KNOTS ( 'NONE', 3,
 ( #23478, #4041, #43232, #27878 ),
 .UNSPECIFIED., .F., .F.,
 ( 4, 4 ),
 ( 0.000000000000000000, 0.004446090762760573217 ),
 .UNSPECIFIED. ) ;
#9970 = ORIENTED_EDGE ( 'NONE', *, *, #49268, .F. ) ;
#9971 = FACE_BOUND ( 'NONE', #15664, .T. ) ;
#9972 = CARTESIAN_POINT ( 'NONE',  ( 3.407937589446178528, -12.08659953757604377, -6.447869442558291198 ) ) ;
#9973 = CARTESIAN_POINT ( 'NONE',  ( 0.6253024248130470975, 22.10248858687955931, 43.85115991264656543 ) ) ;
#9974 = CARTESIAN_POINT ( 'NONE',  ( 0.1310142868023697060, 43.11885108606329453, 0.6370537502137997299 ) ) ;
#9975 = VERTEX_POINT ( 'NONE', #24011 ) ;
#9976 = CARTESIAN_POINT ( 'NONE',  ( 0.9769922540276037015, -6.534541844522391507, -41.39603021991737819 ) ) ;
#9977 = EDGE_CURVE ( 'NONE', #55549, #12205, #23094, .T. ) ;
#9979 = ORIENTED_EDGE ( 'NONE', *, *, #46543, .T. ) ;
#9978 =( BOUNDED_SURFACE ( )  B_SPLINE_SURFACE ( 3, 1, ( 
 ( #27228, #35411 ),
 ( #40428, #41053 ),
 ( #16601, #2786 ),
 ( #60115, #22228 ) ),
 .UNSPECIFIED., .F., .F., .F. ) 
 B_SPLINE_SURFACE_WITH_KNOTS ( ( 4, 4 ),
 ( 2, 2 ),
 ( 0.000000000000000000, 1.000000000000000000 ),
 ( 0.000000000000000000, 1.000000000000000000 ),
 .UNSPECIFIED. ) 
 GEOMETRIC_REPRESENTATION_ITEM ( )  RATIONAL_B_SPLINE_SURFACE ( (
 ( 1.000000000000000000, 1.000000000000000000),
 ( 0.9952954269826590483, 0.8620686068821307169),
 ( 0.9952954269826590483, 0.8620686068821307169),
 ( 1.000000000000000000, 1.000000000000000000) ) ) 
 REPRESENTATION_ITEM ( '' )  SURFACE ( )  );
#9980 = FACE_OUTER_BOUND ( 'NONE', #60697, .T. ) ;
#9982 = EDGE_CURVE ( 'NONE', #7415, #29994, #46918, .T. ) ;
#9981 = ORIENTED_EDGE ( 'NONE', *, *, #53884, .F. ) ;
#9983 = EDGE_LOOP ( 'NONE', ( #17589, #8113, #18768, #28651 ) ) ;
#9984 = CARTESIAN_POINT ( 'NONE',  ( 1.827119703190779321, 37.88337895042268144, 20.44859290426050791 ) ) ;
#9985 = CARTESIAN_POINT ( 'NONE',  ( 4.549368137175248350, -38.59302160394740611, -18.79584381673521065 ) ) ;
#9987 = EDGE_CURVE ( 'NONE', #40550, #46800, #48100, .T. ) ;
#9986 = B_SPLINE_CURVE_WITH_KNOTS ( 'NONE', 3,
 ( #60800, #51092, #16676, #49878 ),
 .UNSPECIFIED., .F., .F.,
 ( 4, 4 ),
 ( 2.271992152883876391E-17, 0.004559932413162184200 ),
 .UNSPECIFIED. ) ;
#9988 = CIRCLE ( 'NONE', #8006, 43.92652462719577500 ) ;
#9989 = CARTESIAN_POINT ( 'NONE',  ( 0.2885697896453110478, 20.85752796052960889, 37.73587455644754840 ) ) ;
#9990 = VERTEX_POINT ( 'NONE', #37206 ) ;
#9991 = DIRECTION ( 'NONE',  ( 0.000000000000000000, 0.000000000000000000, 1.000000000000000000 ) ) ;
#9992 = ADVANCED_FACE ( 'NONE', ( #3954 ), #56495, .T. ) ;
#9993 = CARTESIAN_POINT ( 'NONE',  ( 5.917102823773431552, 12.97825203069059974, -15.36407147469762613 ) ) ;
#9994 = CARTESIAN_POINT ( 'NONE',  ( 5.959547316686252039, 16.28190225198601127, 12.49803383497755682 ) ) ;
#9995 = VERTEX_POINT ( 'NONE', #56276 ) ;
#9996 = ORIENTED_EDGE ( 'NONE', *, *, #3868, .F. ) ;
#9997 =( BOUNDED_SURFACE ( )  B_SPLINE_SURFACE ( 3, 1, ( 
 ( #5528, #10888 ),
 ( #529, #58456 ),
 ( #61923, #48774 ),
 ( #6140, #38474 ) ),
 .UNSPECIFIED., .F., .F., .F. ) 
 B_SPLINE_SURFACE_WITH_KNOTS ( ( 4, 4 ),
 ( 2, 2 ),
 ( 0.000000000000000000, 1.000000000000000000 ),
 ( 0.000000000000000000, 1.000000000000000000 ),
 .UNSPECIFIED. ) 
 GEOMETRIC_REPRESENTATION_ITEM ( )  RATIONAL_B_SPLINE_SURFACE ( (
 ( 1.000000000000000000, 1.000000000000000000),
 ( 0.9953485035131437453, 0.8621029689291523912),
 ( 0.9953485035131437453, 0.8621029689291523912),
 ( 1.000000000000000000, 1.000000000000000000) ) ) 
 REPRESENTATION_ITEM ( '' )  SURFACE ( )  );
#9998 = DIRECTION ( 'NONE',  ( 0.000000000000000000, 0.000000000000000000, -1.000000000000000000 ) ) ;
#9999 = DIRECTION ( 'NONE',  ( -1.000000000000000000, -0.000000000000000000, -0.000000000000000000 ) ) ;
#10000 = LINE ( 'NONE', #38516, #61550 ) ;
#10001 = DIRECTION ( 'NONE',  ( -1.000000000000000000, -1.836909530733573776E-16, 1.925929944387235853E-32 ) ) ;
#10002 = ORIENTED_EDGE ( 'NONE', *, *, #25992, .T. ) ;
#10003 = ADVANCED_FACE ( 'NONE', ( #46598 ), #3646, .F. ) ;
#10004 = ORIENTED_EDGE ( 'NONE', *, *, #47299, .F. ) ;
#10005 = EDGE_CURVE ( 'NONE', #14306, #23536, #5460, .T. ) ;
#10006 = CARTESIAN_POINT ( 'NONE',  ( 0.8753041380234524160, -47.26389509135299249, 13.31399822241830755 ) ) ;
#10007 = CARTESIAN_POINT ( 'NONE',  ( 0.9762797500689124330, -40.96497924994823592, 8.842808390834631993 ) ) ;
#10008 = CARTESIAN_POINT ( 'NONE',  ( 3.238931869106854489, -12.88361013339135219, -41.01619136531521548 ) ) ;
#10009 = CARTESIAN_POINT ( 'NONE',  ( 0.9752132459055863345, -21.25214916889619232, 37.27572867006956159 ) ) ;
#10010 = CARTESIAN_POINT ( 'NONE',  ( -48.95476116535499500, 0.000000000000000000, -12.50000000000000000 ) ) ;
#10011 = CARTESIAN_POINT ( 'NONE',  ( 4.962356264823608143, 1.841560470688809792, -42.04574000888963781 ) ) ;
#10012 = ORIENTED_EDGE ( 'NONE', *, *, #20922, .F. ) ;
#10013 = DIRECTION ( 'NONE',  ( 0.000000000000000000, 0.000000000000000000, -1.000000000000000000 ) ) ;
#10014 = CARTESIAN_POINT ( 'NONE',  ( 1.000110580585050979, -39.80167790415918461, 13.12417307053917170 ) ) ;
#10015 = CARTESIAN_POINT ( 'NONE',  ( 1.227938101723748288, 0.8460948827231143943, -42.91134962331486236 ) ) ;
#10016 = CARTESIAN_POINT ( 'NONE',  ( 0.5804410086790514622, -46.75463715370012352, -3.677466040800478453 ) ) ;
#10017 = DIRECTION ( 'NONE',  ( 0.000000000000000000, 0.000000000000000000, 1.000000000000000000 ) ) ;
#10018 = CARTESIAN_POINT ( 'NONE',  ( 0.3676999524040323597, -22.15802448779959377, -38.14410221935904843 ) ) ;
#10019 = CARTESIAN_POINT ( 'NONE',  ( -2.708315649062910779, -11.76894112707817897, 8.698422600176929365 ) ) ;
#10020 = CONICAL_SURFACE ( 'NONE', #26028, 43.08621763946400307, 1.568696531533066763 ) ;
#10021 = EDGE_CURVE ( 'NONE', #24833, #19678, #19702, .T. ) ;
#10022 = ORIENTED_EDGE ( 'NONE', *, *, #26746, .F. ) ;
#10023 = CARTESIAN_POINT ( 'NONE',  ( 3.783198216974394956, -7.325057189010705905, 42.41041696600774458 ) ) ;
#10024 = AXIS2_PLACEMENT_3D ( 'NONE', #54408, #20618, #21538 ) ;
#10025 = CARTESIAN_POINT ( 'NONE',  ( 5.958863334805807099, -12.49619391867170926, -16.28335246510363277 ) ) ;
#10026 = CARTESIAN_POINT ( 'NONE',  ( 0.6026112563231247332, -47.45690295771330369, -12.62471213796142422 ) ) ;
#10027 = CARTESIAN_POINT ( 'NONE',  ( 0.2885700199627511675, -29.91358789498803361, 31.05173037893190013 ) ) ;
#10028 = CARTESIAN_POINT ( 'NONE',  ( 2.526464513654344657, -36.59988118252419298, 22.53107770806409960 ) ) ;
#10029 = VERTEX_POINT ( 'NONE', #14629 ) ;
#10030 = CARTESIAN_POINT ( 'NONE',  ( 0.8751705887134553219, -33.37254303619578621, 34.63284514348527665 ) ) ;
#10031 = CARTESIAN_POINT ( 'NONE',  ( 5.894904586330512508, 19.00045333391160085, -6.596376669618728705 ) ) ;
#10032 = LINE ( 'NONE', #1224, #50554 ) ;
#10033 = ORIENTED_EDGE ( 'NONE', *, *, #53974, .F. ) ;
#10034 = FACE_OUTER_BOUND ( 'NONE', #6322, .T. ) ;
#10035 = CARTESIAN_POINT ( 'NONE',  ( 5.959828726073459926, -2.674641840416033478, -20.35060134307033763 ) ) ;
#10036 = VERTEX_POINT ( 'NONE', #23396 ) ;
#10037 = CARTESIAN_POINT ( 'NONE',  ( 0.6001305935487422083, -37.84751346122836679, -29.70149728382421728 ) ) ;
#10038 = VERTEX_POINT ( 'NONE', #37516 ) ;
#10039 = LINE ( 'NONE', #29138, #45624 ) ;
#10040 = ORIENTED_EDGE ( 'NONE', *, *, #25957, .F. ) ;
#10041 = CARTESIAN_POINT ( 'NONE',  ( 0.1158403557922069033, 29.69272295667737893, -32.63866588268925284 ) ) ;
#10042 = CARTESIAN_POINT ( 'NONE',  ( 0.1073791018717483448, 40.02496097243036388, 16.05399293000829175 ) ) ;
#10043 = ORIENTED_EDGE ( 'NONE', *, *, #25894, .F. ) ;
#10044 = CARTESIAN_POINT ( 'NONE',  ( 0.6252788684277206244, 4.031327004993904950, -48.94070630622808693 ) ) ;
#10045 = VERTEX_POINT ( 'NONE', #14018 ) ;
#10046 = B_SPLINE_CURVE_WITH_KNOTS ( 'NONE', 3,
 ( #32877, #18151, #56956, #33180, #28149, #56338 ),
 .UNSPECIFIED., .F., .F.,
 ( 4, 2, 4 ),
 ( 8.673617379884035472E-19, 0.0002291966416970792140, 0.0004583932833941575607 ),
 .UNSPECIFIED. ) ;
#10047 = CARTESIAN_POINT ( 'NONE',  ( 5.981074661064941900, 16.27808421740026290, -12.50143471347264246 ) ) ;
#10048 = CARTESIAN_POINT ( 'NONE',  ( 1.227938101723747621, 22.18841447410770940, -36.73927144310489012 ) ) ;
#10049 = CARTESIAN_POINT ( 'NONE',  ( 0.6041374136657476912, 46.51335992032601752, 12.28249295042061817 ) ) ;
#10050 = ADVANCED_FACE ( 'NONE', ( #13393, #51569 ), #8663, .T. ) ;
#10051 = VECTOR ( 'NONE', #17047, 1000.000000000000114 ) ;
#10052 = EDGE_LOOP ( 'NONE', ( #14699, #12061, #30892, #46964 ) ) ;
#10053 = CARTESIAN_POINT ( 'NONE',  ( 0.9756354156337448957, -16.29989858042598527, -39.69194847698947370 ) ) ;
#10054 = CARTESIAN_POINT ( 'NONE',  ( 0.5807400328401637335, 18.83234461715183272, 44.04145271122570904 ) ) ;
#10055 = CARTESIAN_POINT ( 'NONE',  ( 0.1158816050234199035, -22.87849723619521214, -37.72951637005925107 ) ) ;
#10056 = EDGE_LOOP ( 'NONE', ( #21421, #31430, #51764, #32614 ) ) ;
#10057 = EDGE_CURVE ( 'NONE', #55165, #22556, #21256, .T. ) ;
#10058 = CARTESIAN_POINT ( 'NONE',  ( 5.894904586330512508, 0.6732998044288336370, -20.10164369983208488 ) ) ;
#10059 = CARTESIAN_POINT ( 'NONE',  ( 0.9730545539215892381, -10.61654491617593266, 41.57420493492382008 ) ) ;
#10060 = ORIENTED_EDGE ( 'NONE', *, *, #49290, .T. ) ;
#10061 = CARTESIAN_POINT ( 'NONE',  ( 4.962356264823608143, 26.83784316460287300, 32.41860225448540689 ) ) ;
#10062 = ORIENTED_EDGE ( 'NONE', *, *, #30145, .F. ) ;
#10063 = AXIS2_PLACEMENT_3D ( 'NONE', #46224, #23631, #8916 ) ;
#10064 = CARTESIAN_POINT ( 'NONE',  ( -2.708315649062910779, 10.53288422393055690, -10.16016146078278481 ) ) ;
#10065 = CARTESIAN_POINT ( 'NONE',  ( 0.9784957157296378938, 40.35745815350055921, -11.29639891207905578 ) ) ;
#10066 = VERTEX_POINT ( 'NONE', #10847 ) ;
#10067 = CARTESIAN_POINT ( 'NONE',  ( 0.5837799406558246140, 4.784718297332236858, 46.65136675803160671 ) ) ;
#10068 = CARTESIAN_POINT ( 'NONE',  ( -6.078075953587585900, -12.94192373113783390, -14.25839347137493363 ) ) ;
#10069 = DIRECTION ( 'NONE',  ( 0.000000000000000000, 0.000000000000000000, 1.000000000000000000 ) ) ;
#10070 = CARTESIAN_POINT ( 'NONE',  ( 0.2885697896453107703, -40.13549262224790226, 15.75356890148085398 ) ) ;
#10071 =( BOUNDED_SURFACE ( )  B_SPLINE_SURFACE ( 3, 1, ( 
 ( #60543, #7610 ),
 ( #17972, #42103 ),
 ( #45875, #61159 ),
 ( #8540, #60855 ) ),
 .UNSPECIFIED., .F., .F., .F. ) 
 B_SPLINE_SURFACE_WITH_KNOTS ( ( 4, 4 ),
 ( 2, 2 ),
 ( 0.000000000000000000, 1.000000000000000000 ),
 ( 0.000000000000000000, 1.000000000000000000 ),
 .UNSPECIFIED. ) 
 GEOMETRIC_REPRESENTATION_ITEM ( )  RATIONAL_B_SPLINE_SURFACE ( (
 ( 1.000000000000000000, 1.000000000000000000),
 ( 0.9953485035131437453, 0.8621029689291515030),
 ( 0.9953485035131437453, 0.8621029689291515030),
 ( 1.000000000000000000, 1.000000000000000000) ) ) 
 REPRESENTATION_ITEM ( '' )  SURFACE ( )  );
#10072 = EDGE_CURVE ( 'NONE', #15708, #48962, #27830, .T. ) ;
#10073 = ORIENTED_EDGE ( 'NONE', *, *, #51684, .T. ) ;
#10074 = CARTESIAN_POINT ( 'NONE',  ( 5.901463166500146684, 0.6865185226677115171, 20.10090949829561424 ) ) ;
#10075 = EDGE_CURVE ( 'NONE', #60616, #47712, #45903, .T. ) ;
#10076 = CARTESIAN_POINT ( 'NONE',  ( 0.5839254288179540620, -44.21529885210816957, -18.41284501069725721 ) ) ;
#10077 = CARTESIAN_POINT ( 'NONE',  ( 0.8551540677456715978, 17.49081417858847232, -44.61036085020933228 ) ) ;
#10078 = CARTESIAN_POINT ( 'NONE',  ( 0.6039202388192952409, -39.25113122883236372, -29.51122515426921211 ) ) ;
#10079 = CARTESIAN_POINT ( 'NONE',  ( 3.390910168358336474, -8.956706784861477644, -43.05664339104539096 ) ) ;
#10080 = CARTESIAN_POINT ( 'NONE',  ( -6.016489644550737204, -2.455165042129613617, -18.68257207665199005 ) ) ;
#10081 = B_SPLINE_CURVE_WITH_KNOTS ( 'NONE', 3,
 ( #18951, #14252, #61210, #9841 ),
 .UNSPECIFIED., .F., .F.,
 ( 4, 4 ),
 ( 0.000000000000000000, 0.004446090762761318281 ),
 .UNSPECIFIED. ) ;
#10082 = CARTESIAN_POINT ( 'NONE',  ( 0.5800708057587405930, 38.37709891224502456, -28.65679888493019334 ) ) ;
#10083 = CARTESIAN_POINT ( 'NONE',  ( 1.830465331921979022, 14.04846951621181894, 41.74944981829649038 ) ) ;
#10084 =( BOUNDED_SURFACE ( )  B_SPLINE_SURFACE ( 3, 1, ( 
 ( #44674, #35269 ),
 ( #54327, #15539 ),
 ( #49041, #10218 ),
 ( #11450, #29314 ) ),
 .UNSPECIFIED., .F., .F., .F. ) 
 B_SPLINE_SURFACE_WITH_KNOTS ( ( 4, 4 ),
 ( 2, 2 ),
 ( 0.000000000000000000, 1.000000000000000000 ),
 ( 0.000000000000000000, 1.000000000000000000 ),
 .UNSPECIFIED. ) 
 GEOMETRIC_REPRESENTATION_ITEM ( )  RATIONAL_B_SPLINE_SURFACE ( (
 ( 1.000000000000000000, 1.000000000000000000),
 ( 0.9729067724841187204, 0.9999501103223794596),
 ( 0.9729067724841187204, 0.9999501103223794596),
 ( 1.000000000000000000, 1.000000000000000000) ) ) 
 REPRESENTATION_ITEM ( '' )  SURFACE ( )  );
#10085 = CARTESIAN_POINT ( 'NONE',  ( 0.9754642270333683252, 30.46484943293199521, -30.21634823122134605 ) ) ;
#10086 = LINE ( 'NONE', #345, #16146 ) ;
#10087 = CARTESIAN_POINT ( 'NONE',  ( 4.691466044806103852, -39.84135254923150882, 20.01963481131589617 ) ) ;
#10088 = CARTESIAN_POINT ( 'NONE',  ( 0.5837800304671232343, -1.612506461858141060, 46.86829584153834816 ) ) ;
#10089 = LINE ( 'NONE', #40394, #37799 ) ;
#10090 = EDGE_CURVE ( 'NONE', #22979, #56285, #25238, .T. ) ;
#10091 = DIRECTION ( 'NONE',  ( 1.000000000000000000, 0.000000000000000000, 0.000000000000000000 ) ) ;
#10092 = CARTESIAN_POINT ( 'NONE',  ( 3.376099380956838925, -9.001307264898121829, 9.934024922203457564 ) ) ;
#10093 = ORIENTED_EDGE ( 'NONE', *, *, #9282, .F. ) ;
#10094 = DIRECTION ( 'NONE',  ( -1.000000000000000000, -0.000000000000000000, -0.000000000000000000 ) ) ;
#10095 = CARTESIAN_POINT ( 'NONE',  ( 2.533389852662419894, 18.94327543464629571, -39.73163534943841313 ) ) ;
#10096 = CARTESIAN_POINT ( 'NONE',  ( 0.5848930533535030563, 46.89605428954452293, 0.1821385726608843458 ) ) ;
#10097 = VERTEX_POINT ( 'NONE', #44080 ) ;
#10098 = DIRECTION ( 'NONE',  ( -1.000000000000000000, -0.000000000000000000, -0.000000000000000000 ) ) ;
#10099 = CARTESIAN_POINT ( 'NONE',  ( 0.5807400328401637335, 37.66660715020906025, -29.58941477092977834 ) ) ;
#10101 = ORIENTED_EDGE ( 'NONE', *, *, #29151, .T. ) ;
#10100 = AXIS2_PLACEMENT_3D ( 'NONE', #28562, #38305, #5655 ) ;
#10102 = ORIENTED_EDGE ( 'NONE', *, *, #45014, .F. ) ;
#10103 = CARTESIAN_POINT ( 'NONE',  ( 5.880360259849752858, -15.37531919565204852, -45.44137230084876933 ) ) ;
#10104 = VERTEX_POINT ( 'NONE', #15543 ) ;
#10105 = DIRECTION ( 'NONE',  ( 0.07836865515943412797, 0.7104869166657089563, -0.6993330359244840366 ) ) ;
#10106 = ORIENTED_EDGE ( 'NONE', *, *, #57624, .T. ) ;
#10107 = ORIENTED_EDGE ( 'NONE', *, *, #13247, .T. ) ;
#10108 = LINE ( 'NONE', #35166, #36766 ) ;
#10109 = ORIENTED_EDGE ( 'NONE', *, *, #8240, .F. ) ;
#10110 = CARTESIAN_POINT ( 'NONE',  ( 4.975610109902397937, 24.86209007718959185, 42.12274782266089801 ) ) ;
#10111 = CARTESIAN_POINT ( 'NONE',  ( 0.2279481005628809787, -11.82334179845439515, -42.50543583813526283 ) ) ;
#10112 = B_SPLINE_CURVE_WITH_KNOTS ( 'NONE', 3,
 ( #44541, #29169, #24785, #29788 ),
 .UNSPECIFIED., .F., .F.,
 ( 4, 4 ),
 ( 0.000000000000000000, 0.005013413432710140706 ),
 .UNSPECIFIED. ) ;
#10113 = CARTESIAN_POINT ( 'NONE',  ( -5.995132425357893702, 18.20425902871267354, 4.869002713216636913 ) ) ;
#10114 = EDGE_LOOP ( 'NONE', ( #1485, #33255, #6452, #29907 ) ) ;
#10115 = DIRECTION ( 'NONE',  ( 1.000000000000000000, 0.000000000000000000, 0.000000000000000000 ) ) ;
#10116 = B_SPLINE_CURVE_WITH_KNOTS ( 'NONE', 3,
 ( #39101, #38178, #48780, #33467, #28432, #18749, #58159, #42559, #37877, #14057, #52543, #33155, #52232, #24053, #38795, #47559 ),
 .UNSPECIFIED., .F., .F.,
 ( 4, 3, 3, 3, 3, 4 ),
 ( 1.551621725782133898E-17, 0.0002732102107931851749, 0.0004098135523333776308, 0.0005464168938824964317, 0.0008195847345945365047, 0.001092771384553102880 ),
 .UNSPECIFIED. ) ;
#10117 = CARTESIAN_POINT ( 'NONE',  ( 5.838029081930957709, 25.39899213859872518, -39.82406629785964469 ) ) ;
#10118 = ORIENTED_EDGE ( 'NONE', *, *, #43988, .F. ) ;
#10119 = EDGE_CURVE ( 'NONE', #40756, #33475, #53421, .T. ) ;
#10120 = ORIENTED_EDGE ( 'NONE', *, *, #38954, .F. ) ;
#10121 = EDGE_LOOP ( 'NONE', ( #20530, #10196, #50993, #52557, #32679, #57552, #32238, #18922, #31162, #5515, #28779, #7040, #16061, #39516, #12381, #892, #8475, #57619, #40887, #17367, #45366, #17162, #14829, #44888, #29046, #21353, #46871, #33117, #56025, #60786, #39179, #27041, #32875, #8452, #9724, #22997, #20294, #57475, #34657, #22056, #26990, #40291, #23243, #49799, #52378, #33926, #50535, #61573, #43964, #15493, #50774, #2334, #45456, #3113, #58921, #22687, #48529, #25775, #53297, #16349, #22174, #23505, #29927, #6844, #3789, #25384, #52643, #388, #30696, #39945, #11914, #29752, #1675, #48051, #34599, #23050, #6, #40947, #25187, #17279, #46661, #44059, #31070, #26808, #4514, #5250, #29197, #25192, #290, #17293, #8332, #24817, #4142, #48113, #24779, #56533, #12315, #41899, #59418, #40482, #10269, #38616, #12888, #32500, #52773, #45873, #47513, #60475, #38019, #3252, #18936, #151, #54369, #27591, #8813, #10101, #40568, #52176, #12012, #1555, #36797, #23452, #14601, #48080, #50479, #58177, #28215, #46354, #3523, #8965, #8715, #32894, #24230, #7851, #6773, #29698, #49850, #59079, #43816, #43458, #34760, #57446, #58192, #34465, #11652, #9898 ) ) ;
#10122 = CARTESIAN_POINT ( 'NONE',  ( 48.88249858120726543, 12.32166152761977429, 2.106239978570320304 ) ) ;
#10123 = CARTESIAN_POINT ( 'NONE',  ( 1.088313998177378839, -30.89087247895950838, 29.78798111128817538 ) ) ;
#10124 = CARTESIAN_POINT ( 'NONE',  ( 0.5263152470540294336, 9.797174393178825657E-16, -8.000000000000000000 ) ) ;
#10125 = CARTESIAN_POINT ( 'NONE',  ( 0.7056313189692698939, 39.91795815694759142, -24.62326665042111529 ) ) ;
#10126 = EDGE_CURVE ( 'NONE', #37598, #40820, #30817, .T. ) ;
#10127 = ORIENTED_EDGE ( 'NONE', *, *, #38525, .T. ) ;
#10128 = CARTESIAN_POINT ( 'NONE',  ( 0.6039202388192952409, -19.71856863334322796, -44.97490148850938141 ) ) ;
#10129 = DIRECTION ( 'NONE',  ( 0.000000000000000000, 0.000000000000000000, 1.000000000000000000 ) ) ;
#10130 = ADVANCED_FACE ( 'NONE', ( #20547 ), #53875, .F. ) ;
#10131 = CARTESIAN_POINT ( 'NONE',  ( 0.5835226383429302777, 36.69085443737677110, -29.20656904193287673 ) ) ;
#10132 = CARTESIAN_POINT ( 'NONE',  ( 1.827119703190777988, -31.30004882613822303, -29.55676396270173711 ) ) ;
#10133 = ORIENTED_EDGE ( 'NONE', *, *, #14726, .T. ) ;
#10134 = FACE_OUTER_BOUND ( 'NONE', #45353, .T. ) ;
#10135 = CARTESIAN_POINT ( 'NONE',  ( 0.6016118706126976079, -13.63816021288923608, -47.17575267859004384 ) ) ;
#10136 = CARTESIAN_POINT ( 'NONE',  ( 0.8753041380234524160, -31.30612550145381334, -37.82941757363181523 ) ) ;
#10137 = CARTESIAN_POINT ( 'NONE',  ( 1.231276596079881047, 33.41651732065586344, -25.31033664684003170 ) ) ;
#10138 = ORIENTED_EDGE ( 'NONE', *, *, #39716, .T. ) ;
#10139 = ORIENTED_EDGE ( 'NONE', *, *, #5282, .F. ) ;
#10140 = DIRECTION ( 'NONE',  ( 1.000000000000000000, 0.000000000000000000, 0.000000000000000000 ) ) ;
#10141 = LINE ( 'NONE', #724, #12709 ) ;
#10142 = CARTESIAN_POINT ( 'NONE',  ( 0.1073791018717578927, 33.91564619577771111, 26.63563652260178927 ) ) ;
#10143 = ADVANCED_FACE ( 'NONE', ( #48133 ), #53827, .F. ) ;
#10144 = CARTESIAN_POINT ( 'NONE',  ( 0.5804410086790514622, 27.37779091617000304, -38.07855586029853612 ) ) ;
#10145 = CARTESIAN_POINT ( 'NONE',  ( 0.5848930533535030563, -44.24150702629536624, -15.55513222154723429 ) ) ;
#10146 = CARTESIAN_POINT ( 'NONE',  ( 1.227938101723748288, 34.55893248994541267, -25.45152231597022308 ) ) ;
#10147 = VECTOR ( 'NONE', #28351, 1000.000000000000000 ) ;
#10148 = CIRCLE ( 'NONE', #37175, 9.499999999999996447 ) ;
#10149 = CARTESIAN_POINT ( 'NONE',  ( 0.5800708057587371513, 47.56394202401747151, -5.628966369368563427 ) ) ;
#10150 = CARTESIAN_POINT ( 'NONE',  ( -6.078075953587585900, -6.655346486686200436, -18.06935354099004698 ) ) ;
#10151 = CARTESIAN_POINT ( 'NONE',  ( 0.000000000000000000, -1.178949249685214307, 2.042000000000001592 ) ) ;
#10152 = CARTESIAN_POINT ( 'NONE',  ( 4.322998006666179727, 32.40067585697798336, -35.39923696758977911 ) ) ;
#10153 = CARTESIAN_POINT ( 'NONE',  ( 1.140000000000004343, 5.633200000000004870, 0.000000000000000000 ) ) ;
#10154 = ORIENTED_EDGE ( 'NONE', *, *, #31991, .F. ) ;
#10155 = CARTESIAN_POINT ( 'NONE',  ( 1.088908134280555329, -42.43751564162686662, 6.374115321932934286 ) ) ;
#10156 = DIRECTION ( 'NONE',  ( -0.07439287786467650709, -0.9971416435352943308, 0.01320009283085898759 ) ) ;
#10157 = FACE_BOUND ( 'NONE', #19069, .T. ) ;
#10158 = LINE ( 'NONE', #9226, #43090 ) ;
#10159 = B_SPLINE_CURVE_WITH_KNOTS ( 'NONE', 3,
 ( #25569, #6427, #30265, #44706 ),
 .UNSPECIFIED., .F., .F.,
 ( 4, 4 ),
 ( 0.000000000000000000, 0.004445488388166993383 ),
 .UNSPECIFIED. ) ;
#10160 = CARTESIAN_POINT ( 'NONE',  ( 0.5998501479064708430, -24.50586714782633280, 41.39809967730445095 ) ) ;
#10161 = CARTESIAN_POINT ( 'NONE',  ( 0.6029443199889047422, 33.01493686021951390, -36.35315097718657285 ) ) ;
#10162 = CARTESIAN_POINT ( 'NONE',  ( 0.5988103564986357874, 23.52668867203648517, -41.96244062389627061 ) ) ;
#10163 = CARTESIAN_POINT ( 'NONE',  ( 0.3622758884714730732, 31.06363466427686504, 29.89648521331642428 ) ) ;
#10164 =( BOUNDED_SURFACE ( )  B_SPLINE_SURFACE ( 3, 1, ( 
 ( #5115, #33662 ),
 ( #42456, #52743 ),
 ( #53353, #9524 ),
 ( #24244, #23634 ) ),
 .UNSPECIFIED., .F., .F., .F. ) 
 B_SPLINE_SURFACE_WITH_KNOTS ( ( 4, 4 ),
 ( 2, 2 ),
 ( 0.000000000000000000, 1.000000000000000000 ),
 ( 0.000000000000000000, 1.000000000000000000 ),
 .UNSPECIFIED. ) 
 GEOMETRIC_REPRESENTATION_ITEM ( )  RATIONAL_B_SPLINE_SURFACE ( (
 ( 1.000000000000000000, 1.000000000000000000),
 ( 0.9953040768229013402, 0.8617119497784988535),
 ( 0.9953040768229013402, 0.8617119497784988535),
 ( 1.000000000000000000, 1.000000000000000000) ) ) 
 REPRESENTATION_ITEM ( '' )  SURFACE ( )  );
#10165 = CARTESIAN_POINT ( 'NONE',  ( 0.5987334363312689645, 48.31411593427914397, -8.792559807081808287 ) ) ;
#10166 = CARTESIAN_POINT ( 'NONE',  ( 0.5786265663353196143, 37.55861529268553056, 29.72999788434305302 ) ) ;
#10167 = B_SPLINE_CURVE_WITH_KNOTS ( 'NONE', 3,
 ( #56203, #51497, #59664, #27093, #55896, #3571 ),
 .UNSPECIFIED., .F., .F.,
 ( 4, 2, 4 ),
 ( 4.878909776184769953E-19, 0.0002293801035737080981, 0.0004587602071474157083 ),
 .UNSPECIFIED. ) ;
#10168 = CARTESIAN_POINT ( 'NONE',  ( 4.553261556744873317, -36.93702150832076825, -23.77385134801438937 ) ) ;
#10169 = LINE ( 'NONE', #15186, #22435 ) ;
#10171 = ORIENTED_EDGE ( 'NONE', *, *, #27355, .T. ) ;
#10170 = CARTESIAN_POINT ( 'NONE',  ( 30.00000000000000711, 19.00000000000000000, -1.502225356622044491E-30 ) ) ;
#10172 = ORIENTED_EDGE ( 'NONE', *, *, #6394, .F. ) ;
#10173 = CARTESIAN_POINT ( 'NONE',  ( 5.838029081930957709, -46.81003243000947123, 6.315530227493348470 ) ) ;
#10174 = CARTESIAN_POINT ( 'NONE',  ( 0.5782707292762423457, 32.08118243870044495, -34.21306895094969036 ) ) ;
#10175 = CARTESIAN_POINT ( 'NONE',  ( 0.1149546198390368201, 41.78922939623867450, 14.16357551932990155 ) ) ;
#10176 = EDGE_CURVE ( 'NONE', #3786, #18314, #15274, .T. ) ;
#10177 = EDGE_LOOP ( 'NONE', ( #23582, #45017, #50603, #37230 ) ) ;
#10178 = CARTESIAN_POINT ( 'NONE',  ( 0.1073791018717578927, -11.62916352156179123, 41.52698815987148606 ) ) ;
#10179 = CARTESIAN_POINT ( 'NONE',  ( 3.376099380956838925, -2.682194557846333094, 13.13446671874906002 ) ) ;
#10180 = CARTESIAN_POINT ( 'NONE',  ( 4.553261556744873317, -43.15908619232978083, -8.175135770535248980 ) ) ;
#10181 = EDGE_CURVE ( 'NONE', #47052, #478, #37690, .T. ) ;
#10182 = ORIENTED_EDGE ( 'NONE', *, *, #9414, .F. ) ;
#10183 = EDGE_LOOP ( 'NONE', ( #31528, #45968, #2037, #2732 ) ) ;
#10184 = CARTESIAN_POINT ( 'NONE',  ( 2.618530812446111078, 26.73752065161024305, 38.66305443964451172 ) ) ;
#10185 =( NAMED_UNIT ( * ) PLANE_ANGLE_UNIT ( ) SI_UNIT ( $, .RADIAN. ) );
#10186 = ADVANCED_FACE ( 'NONE', ( #6717, #8835 ), #32044, .T. ) ;
#10187 = FACE_OUTER_BOUND ( 'NONE', #26628, .T. ) ;
#10188 = LINE ( 'NONE', #19598, #54924 ) ;
#10189 = CARTESIAN_POINT ( 'NONE',  ( 0.9968887458511664912, -10.46947792236065489, -41.61262323391479612 ) ) ;
#10190 = CIRCLE ( 'NONE', #30161, 43.92652462719577500 ) ;
#10191 = CARTESIAN_POINT ( 'NONE',  ( 0.8744876279028263033, -42.33402326122615733, -24.86323641237110493 ) ) ;
#10192 = CIRCLE ( 'NONE', #194, 12.55882000000000076 ) ;
#10193 = CARTESIAN_POINT ( 'NONE',  ( 0.5839254288179548391, 38.05364096126358220, -29.08514953649782342 ) ) ;
#10194 = ORIENTED_EDGE ( 'NONE', *, *, #24626, .F. ) ;
#10195 = EDGE_CURVE ( 'NONE', #42917, #722, #45302, .T. ) ;
#10196 = ORIENTED_EDGE ( 'NONE', *, *, #20453, .F. ) ;
#10197 = CARTESIAN_POINT ( 'NONE',  ( 0.9730545539215883499, 15.95224156741883270, -39.83279466599022811 ) ) ;
#10198 = CARTESIAN_POINT ( 'NONE',  ( 0.8760168074886960365, -34.63873394077511136, 33.37827814204065646 ) ) ;
#10199 = VERTEX_POINT ( 'NONE', #3811 ) ;
#10200 = CARTESIAN_POINT ( 'NONE',  ( 4.975801465491695552, -47.10002938642136883, -8.787181743659990829 ) ) ;
#10201 = CARTESIAN_POINT ( 'NONE',  ( -6.063463321072278589, 17.84349906452534640, 7.240855861965011186 ) ) ;
#10202 = DIRECTION ( 'NONE',  ( -1.000000000000000000, -0.000000000000000000, -0.000000000000000000 ) ) ;
#10203 = CARTESIAN_POINT ( 'NONE',  ( -3.345653888883663996, 2.687187980154699840, -5.460849780464863024 ) ) ;
#10204 = VERTEX_POINT ( 'NONE', #13242 ) ;
#10205 = ORIENTED_EDGE ( 'NONE', *, *, #57903, .T. ) ;
#10206 = CARTESIAN_POINT ( 'NONE',  ( 0.5832655196449147983, 46.50736770247006291, -6.024942519275434449 ) ) ;
#10207 = FACE_OUTER_BOUND ( 'NONE', #6923, .T. ) ;
#10208 = ADVANCED_FACE ( 'NONE', ( #32658 ), #41856, .F. ) ;
#10209 = CARTESIAN_POINT ( 'NONE',  ( 4.960386119450149955, 41.48529788082174719, -13.90706742673764396 ) ) ;
#10210 = CARTESIAN_POINT ( 'NONE',  ( 5.974727161628369032, -17.78288073588509732, 10.24903993264978119 ) ) ;
#10211 = B_SPLINE_CURVE_WITH_KNOTS ( 'NONE', 3,
 ( #47763, #23950, #43075, #33667, #52749, #28952 ),
 .UNSPECIFIED., .F., .F.,
 ( 4, 2, 4 ),
 ( 1.216356941739949889E-16, 0.0002448718616795908195, 0.0004897437233590599915 ),
 .UNSPECIFIED. ) ;
#10212 = ORIENTED_EDGE ( 'NONE', *, *, #33422, .T. ) ;
#10213 = CARTESIAN_POINT ( 'NONE',  ( 1.227938101723748288, 37.58536632582807613, -20.72293514920711033 ) ) ;
#10214 = VERTEX_POINT ( 'NONE', #30861 ) ;
#10215 = CARTESIAN_POINT ( 'NONE',  ( 4.975801465491694664, -40.15204426031552032, 26.14269827151608894 ) ) ;
#10216 = CARTESIAN_POINT ( 'NONE',  ( -2.569797478183790229, 14.62602397812940680, 0.4487456364279327481 ) ) ;
#10217 = ORIENTED_EDGE ( 'NONE', *, *, #52003, .F. ) ;
#10218 = CARTESIAN_POINT ( 'NONE',  ( 0.5848930533535030563, -1.384993715959497163, -46.87595198813897923 ) ) ;
#10219 = CARTESIAN_POINT ( 'NONE',  ( 0.7048096507298579061, -42.08020459959998050, 23.32077812596807576 ) ) ;
#10220 = CARTESIAN_POINT ( 'NONE',  ( 4.691466044806102076, -24.49380602310786870, -37.25818859570297548 ) ) ;
#10222 = EDGE_CURVE ( 'NONE', #8104, #28949, #8209, .T. ) ;
#10221 = B_SPLINE_CURVE_WITH_KNOTS ( 'NONE', 3,
 ( #27888, #61376, #56994, #18492 ),
 .UNSPECIFIED., .F., .F.,
 ( 4, 4 ),
 ( 4.470280076681872512E-19, 0.004444878191957686055 ),
 .UNSPECIFIED. ) ;
#10223 = CARTESIAN_POINT ( 'NONE',  ( 0.3676999524040323597, -28.14442808720941969, 33.96824621564581292 ) ) ;
#10224 = CARTESIAN_POINT ( 'NONE',  ( 1.660531772554325158, -3.660093687634888404, -5.599999999999981881 ) ) ;
#10225 = CARTESIAN_POINT ( 'NONE',  ( 0.9730545539215892381, 26.52009130076819687, -33.73144377768529978 ) ) ;
#10226 = CARTESIAN_POINT ( 'NONE',  ( 0.1365634738349406074, -7.669977273387969419, 43.45151399259823677 ) ) ;
#10227 = CARTESIAN_POINT ( 'NONE',  ( 0.5800708057587381505, 47.89175345272234097, 0.6275304576132049172 ) ) ;
#10228 = VERTEX_POINT ( 'NONE', #42079 ) ;
#10229 = CARTESIAN_POINT ( 'NONE',  ( 4.291220156522060236, 47.06111669607644643, -2.154133845417245396 ) ) ;
#10230 = CARTESIAN_POINT ( 'NONE',  ( 100.0000507999999968, 0.000000000000000000, 0.000000000000000000 ) ) ;
#10231 = CARTESIAN_POINT ( 'NONE',  ( 4.553261556744875094, -14.95853073564453339, -41.30111286702108941 ) ) ;
#10232 = ORIENTED_EDGE ( 'NONE', *, *, #4309, .F. ) ;
#10233 = DIRECTION ( 'NONE',  ( 0.000000000000000000, 0.000000000000000000, 1.000000000000000000 ) ) ;
#10234 = CARTESIAN_POINT ( 'NONE',  ( 4.322998006666179727, 27.50295597456451802, -39.32552843303822243 ) ) ;
#10235 = CARTESIAN_POINT ( 'NONE',  ( 0.6021447746440204973, 22.94538958722560906, 43.41716522043932969 ) ) ;
#10236 = CARTESIAN_POINT ( 'NONE',  ( 5.896278296736517710, 19.71091930359935773, 4.000829891582261766 ) ) ;
#10237 = CARTESIAN_POINT ( 'NONE',  ( 5.960721111146673579, 19.82454228767738158, 5.318514366755001888 ) ) ;
#10238 = AXIS2_PLACEMENT_3D ( 'NONE', #44179, #43866, #48837 ) ;
#10239 = CARTESIAN_POINT ( 'NONE',  ( 4.975610109902397937, -23.13264022976583334, 43.09675583078141869 ) ) ;
#10240 = B_SPLINE_CURVE_WITH_KNOTS ( 'NONE', 3,
 ( #43741, #150, #15215, #34321 ),
 .UNSPECIFIED., .F., .F.,
 ( 4, 4 ),
 ( 2.168404344971008627E-19, 0.004041751736740995145 ),
 .UNSPECIFIED. ) ;
#10241 = FILL_AREA_STYLE ('',( #5205 ) ) ;
#10242 = CARTESIAN_POINT ( 'NONE',  ( 5.896782393890504181, 20.06749419425502978, 1.349727247095894089 ) ) ;
#10243 = VECTOR ( 'NONE', #17454, 1000.000000000000000 ) ;
#10244 = B_SPLINE_CURVE_WITH_KNOTS ( 'NONE', 3,
 ( #59164, #25979, #11580, #35395 ),
 .UNSPECIFIED., .F., .F.,
 ( 4, 4 ),
 ( 0.000000000000000000, 0.005004948556313804434 ),
 .UNSPECIFIED. ) ;
#10245 = CARTESIAN_POINT ( 'NONE',  ( 0.9762797500689124330, -6.471194619075845367, 41.40589843715202534 ) ) ;
#10246 = FACE_OUTER_BOUND ( 'NONE', #7174, .T. ) ;
#10248 = VERTEX_POINT ( 'NONE', #7038 ) ;
#10247 = CARTESIAN_POINT ( 'NONE',  ( 4.956445790444004906, -37.28933980949924631, -28.75835855384189443 ) ) ;
#10249 = ORIENTED_EDGE ( 'NONE', *, *, #36588, .T. ) ;
#10250 = CARTESIAN_POINT ( 'NONE',  ( 0.5809828226811626362, -12.92184523170236510, 46.11980934799335330 ) ) ;
#10251 = CARTESIAN_POINT ( 'NONE',  ( 4.956445790443998689, -23.10347171912865250, 41.03373788314999615 ) ) ;
#10252 = CARTESIAN_POINT ( 'NONE',  ( 0.1098349054025746230, 16.30574661324314079, 39.92296693299713439 ) ) ;
#10253 = EDGE_CURVE ( 'NONE', #6126, #12149, #26165, .T. ) ;
#10254 = CARTESIAN_POINT ( 'NONE',  ( 0.9972139404380289118, 0.6581143129160298422, 42.90441115546389028 ) ) ;
#10255 = CARTESIAN_POINT ( 'NONE',  ( 0.9757402383260934675, 42.55239275983119285, -5.516496958496648340 ) ) ;
#10256 = CARTESIAN_POINT ( 'NONE',  ( -6.001507490154110336, 18.68062548815628787, -2.475062734132249975 ) ) ;
#10257 = ADVANCED_FACE ( 'NONE', ( #21469 ), #7785, .T. ) ;
#10258 = VERTEX_POINT ( 'NONE', #12945 ) ;
#10259 = CARTESIAN_POINT ( 'NONE',  ( 4.553261556744875094, -33.30082861731464305, -28.64601855797546648 ) ) ;
#10260 = EDGE_CURVE ( 'NONE', #45251, #59386, #39917, .T. ) ;
#10261 = EDGE_CURVE ( 'NONE', #7367, #49767, #50809, .T. ) ;
#10262 = B_SPLINE_CURVE_WITH_KNOTS ( 'NONE', 3,
 ( #7750, #26873, #46013, #3052, #22177, #41304 ),
 .UNSPECIFIED., .F., .F.,
 ( 4, 2, 4 ),
 ( 9.913782460405889843E-18, 0.0002448709889506571025, 0.0004897419779013042302 ),
 .UNSPECIFIED. ) ;
#10263 = CARTESIAN_POINT ( 'NONE',  ( 3.238018933889920792, 12.98832471626931628, 3.272753188433335847 ) ) ;
#10264 = EDGE_CURVE ( 'NONE', #45332, #37468, #13550, .T. ) ;
#10265 = LINE ( 'NONE', #28745, #21770 ) ;
#10266 = ORIENTED_EDGE ( 'NONE', *, *, #56859, .T. ) ;
#10267 = CARTESIAN_POINT ( 'NONE',  ( 0.9730545539215883499, -30.69604515769629316, -29.98130006528894498 ) ) ;
#10268 = CARTESIAN_POINT ( 'NONE',  ( 0.5809828226811617480, 47.55412398569215071, -5.711058609464832792 ) ) ;
#10269 = ORIENTED_EDGE ( 'NONE', *, *, #52661, .T. ) ;
#10270 = ADVANCED_FACE ( 'NONE', ( #40607 ), #45146, .F. ) ;
#10271 = FACE_OUTER_BOUND ( 'NONE', #25820, .T. ) ;
#10272 = ORIENTED_EDGE ( 'NONE', *, *, #41824, .F. ) ;
#10273 = ADVANCED_FACE ( 'NONE', ( #49658 ), #58261, .F. ) ;
#10274 = CARTESIAN_POINT ( 'NONE',  ( 0.7056555295713328180, -29.82339362082569778, -37.48482836297259979 ) ) ;
#10275 = ORIENTED_EDGE ( 'NONE', *, *, #36168, .F. ) ;
#10276 = CARTESIAN_POINT ( 'NONE',  ( 0.6067099128993249657, -24.55985149487293029, -41.12102523654879604 ) ) ;
#10277 = CARTESIAN_POINT ( 'NONE',  ( 4.975801465491694664, -27.09127437476410805, 39.51822597168447260 ) ) ;
#10278 = DIRECTION ( 'NONE',  ( -0.000000000000000000, -0.000000000000000000, 1.000000000000000000 ) ) ;
#10279 = CARTESIAN_POINT ( 'NONE',  ( 0.5997462898726536595, 28.52220283460625438, 39.97543715340569292 ) ) ;
#10280 = B_SPLINE_CURVE_WITH_KNOTS ( 'NONE', 3,
 ( #15638, #10008, #52903, #24715 ),
 .UNSPECIFIED., .F., .F.,
 ( 4, 4 ),
 ( 6.254634441385501517E-18, 0.004566006591234645501 ),
 .UNSPECIFIED. ) ;
#10281 = AXIS2_PLACEMENT_3D ( 'NONE', #36082, #46097, #40791 ) ;
#10282 = VERTEX_POINT ( 'NONE', #16787 ) ;
#10283 = CARTESIAN_POINT ( 'NONE',  ( 1.227938101723748288, -42.91134962331486946, -0.8460948827229646252 ) ) ;
#10284 = ORIENTED_EDGE ( 'NONE', *, *, #40341, .F. ) ;
#10285 = DIRECTION ( 'NONE',  ( 0.000000000000000000, 0.000000000000000000, 1.000000000000000000 ) ) ;
#10286 =( BOUNDED_SURFACE ( )  B_SPLINE_SURFACE ( 3, 1, ( 
 ( #18328, #56511 ),
 ( #9215, #37759 ),
 ( #32731, #61813 ),
 ( #18948, #409 ) ),
 .UNSPECIFIED., .F., .F., .F. ) 
 B_SPLINE_SURFACE_WITH_KNOTS ( ( 4, 4 ),
 ( 2, 2 ),
 ( 0.000000000000000000, 1.000000000000000000 ),
 ( 0.000000000000000000, 1.000000000000000000 ),
 .UNSPECIFIED. ) 
 GEOMETRIC_REPRESENTATION_ITEM ( )  RATIONAL_B_SPLINE_SURFACE ( (
 ( 1.000000000000000000, 1.000000000000000000),
 ( 0.7223157951917476005, 0.9931996967497186413),
 ( 0.7223157951917476005, 0.9931996967497186413),
 ( 1.000000000000000000, 1.000000000000000000) ) ) 
 REPRESENTATION_ITEM ( '' )  SURFACE ( )  );
#10287 = VERTEX_POINT ( 'NONE', #35897 ) ;
#10288 = ORIENTED_EDGE ( 'NONE', *, *, #57389, .T. ) ;
#10289 = CARTESIAN_POINT ( 'NONE',  ( 0.1073791018717578927, 41.52698815987152159, 11.62916352156164557 ) ) ;
#10290 = CARTESIAN_POINT ( 'NONE',  ( 0.6029443199889047422, -30.61798795696924813, -38.39370332907843419 ) ) ;
#10291 = CARTESIAN_POINT ( 'NONE',  ( 0.5997462898726536595, -35.63787911784747564, -33.78599121124021565 ) ) ;
#10292 = ORIENTED_EDGE ( 'NONE', *, *, #46186, .F. ) ;
#10293 = CARTESIAN_POINT ( 'NONE',  ( 2.281351352603290472, 22.83955855331517526, 42.18750813859367099 ) ) ;
#10294 = CARTESIAN_POINT ( 'NONE',  ( 0.1119898979215349782, -38.16786793124121147, 22.13989986054947323 ) ) ;
#10295 = CARTESIAN_POINT ( 'NONE',  ( 0.1149546198390367646, -38.57991944330028389, 21.41346260583937067 ) ) ;
#10297 = ORIENTED_EDGE ( 'NONE', *, *, #33638, .F. ) ;
#10296 = EDGE_CURVE ( 'NONE', #36573, #23457, #1039, .T. ) ;
#10298 = EDGE_LOOP ( 'NONE', ( #60407, #35619, #7608, #4103 ) ) ;
#10299 = CARTESIAN_POINT ( 'NONE',  ( 0.9780106845699478857, -30.87035316765414450, -28.34347441228304021 ) ) ;
#10301 = EDGE_CURVE ( 'NONE', #13003, #3705, #46454, .T. ) ;
#10300 = FACE_OUTER_BOUND ( 'NONE', #59110, .T. ) ;
#10302 = CARTESIAN_POINT ( 'NONE',  ( 4.958415959904820980, 33.34645430971423963, 30.84182126257750056 ) ) ;
#10303 = AXIS2_PLACEMENT_3D ( 'NONE', #49928, #45874, #12051 ) ;
#10304 = CARTESIAN_POINT ( 'NONE',  ( 4.549368137175248350, -28.14399996863522446, 32.41327393324091588 ) ) ;
#10305 = CARTESIAN_POINT ( 'NONE',  ( 42.00000000000000711, 7.715020029081011437E-15, -8.088905766426392334E-31 ) ) ;
#10306 = VERTEX_POINT ( 'NONE', #15095 ) ;
#10307 = DIRECTION ( 'NONE',  ( 0.1305261922200468827, -0.9914448613738110483, 0.000000000000000000 ) ) ;
#10308 = ORIENTED_EDGE ( 'NONE', *, *, #42331, .F. ) ;
#10309 = CARTESIAN_POINT ( 'NONE',  ( 0.6023142530420679819, 12.70386526143707684, 46.39979989577485497 ) ) ;
#10310 = CARTESIAN_POINT ( 'NONE',  ( 0.5800708057587377064, -38.37709891224484693, 28.65679888493045269 ) ) ;
#10311 = B_SPLINE_CURVE_WITH_KNOTS ( 'NONE', 3,
 ( #9281, #19019, #13388, #57181, #43135, #47510 ),
 .UNSPECIFIED., .F., .F.,
 ( 4, 2, 4 ),
 ( 4.911328137975851075E-18, 0.0002291459268755708853, 0.0004582918537511368917 ),
 .UNSPECIFIED. ) ;
#10312 = CARTESIAN_POINT ( 'NONE',  ( 0.1157506346131639274, -42.65743773788693716, 11.28200626844061638 ) ) ;
#10313 = CARTESIAN_POINT ( 'NONE',  ( 0.1119899015040012186, -32.08462141187705186, 30.29089594331977153 ) ) ;
#10314 = CARTESIAN_POINT ( 'NONE',  ( -6.016761891674565099, 16.32039929810269996, -9.418621820384323939 ) ) ;
#10315 =( LENGTH_UNIT ( ) NAMED_UNIT ( * ) SI_UNIT ( .MILLI., .METRE. ) );
#10316 = CARTESIAN_POINT ( 'NONE',  ( 0.6026777506516367566, 37.27955795947347895, -31.96530852320179150 ) ) ;
#10317 = CARTESIAN_POINT ( 'NONE',  ( 0.7762783648524387292, 43.90991295203446754, -19.15108798908265442 ) ) ;
#10318 = CARTESIAN_POINT ( 'NONE',  ( 0.8751705887134553219, 19.22545746485597817, 44.08562551107088723 ) ) ;
#10319 = CARTESIAN_POINT ( 'NONE',  ( 0.8560838555295223751, -38.14845555156087187, 27.29593693413575295 ) ) ;
#10320 = CARTESIAN_POINT ( 'NONE',  ( 1.827119703190780653, 34.89020442382223308, 25.21842556008197533 ) ) ;
#10321 = ADVANCED_FACE ( 'NONE', ( #57651 ), #57900, .F. ) ;
#10322 = CARTESIAN_POINT ( 'NONE',  ( -5.995132425357893702, -7.219211173946362692, -17.40647075750124273 ) ) ;
#10323 = CIRCLE ( 'NONE', #26328, 47.09074272231896430 ) ;
#10324 = DIRECTION ( 'NONE',  ( 1.000000000000000000, 0.000000000000000000, 0.000000000000000000 ) ) ;
#10325 = EDGE_CURVE ( 'NONE', #61052, #10228, #6781, .T. ) ;
#10326 = ORIENTED_EDGE ( 'NONE', *, *, #37473, .F. ) ;
#10327 = LINE ( 'NONE', #29423, #30251 ) ;
#10328 = EDGE_CURVE ( 'NONE', #28284, #6126, #28549, .T. ) ;
#10329 = EDGE_CURVE ( 'NONE', #5538, #28574, #33897, .T. ) ;
#10330 = B_SPLINE_CURVE_WITH_KNOTS ( 'NONE', 3,
 ( #10839, #29932, #49039, #59656 ),
 .UNSPECIFIED., .F., .F.,
 ( 4, 4 ),
 ( 0.000000000000000000, 0.005014147105413700387 ),
 .UNSPECIFIED. ) ;
#10331 = CARTESIAN_POINT ( 'NONE',  ( 3.783278058412226752, -31.62921638229648025, -29.18720354295077968 ) ) ;
#10332 = CARTESIAN_POINT ( 'NONE',  ( 5.901764892641307547, 35.14701960959006755, 34.09807149976035134 ) ) ;
#10333 = CARTESIAN_POINT ( 'NONE',  ( 2.528100132419516033, -30.30928330167931861, 29.04481234869007977 ) ) ;
#10334 = CARTESIAN_POINT ( 'NONE',  ( 4.967162193818130511, 38.44485641567099776, -19.45289607368781759 ) ) ;
#10335 = ADVANCED_FACE ( 'NONE', ( #37998 ), #2278, .F. ) ;
#10336 = VERTEX_POINT ( 'NONE', #24477 ) ;
#10337 = CARTESIAN_POINT ( 'NONE',  ( 0.9754642270333693244, -37.24735125696668092, 21.30186789325742325 ) ) ;
#10338 = CARTESIAN_POINT ( 'NONE',  ( 0.5848930533535030563, 10.69427347779456916, 45.66076649783376951 ) ) ;
#10339 = AXIS2_PLACEMENT_3D ( 'NONE', #43193, #23755, #42890 ) ;
#10340 =( BOUNDED_SURFACE ( )  B_SPLINE_SURFACE ( 3, 1, ( 
 ( #30615, #17159 ),
 ( #46290, #59426 ),
 ( #60343, #21851 ),
 ( #16858, #26226 ) ),
 .UNSPECIFIED., .F., .F., .F. ) 
 B_SPLINE_SURFACE_WITH_KNOTS ( ( 4, 4 ),
 ( 2, 2 ),
 ( 0.000000000000000000, 1.000000000000000000 ),
 ( 0.000000000000000000, 1.000000000000000000 ),
 .UNSPECIFIED. ) 
 GEOMETRIC_REPRESENTATION_ITEM ( )  RATIONAL_B_SPLINE_SURFACE ( (
 ( 1.000000000000000000, 1.000000000000000000),
 ( 0.9953390228620291325, 0.8624445117760984880),
 ( 0.9953390228620291325, 0.8624445117760984880),
 ( 1.000000000000000000, 1.000000000000000000) ) ) 
 REPRESENTATION_ITEM ( '' )  SURFACE ( )  );
#10341 = CARTESIAN_POINT ( 'NONE',  ( 0.8554163680231816613, -24.47000373826210051, 40.03029340588521734 ) ) ;
#10342 = B_SPLINE_CURVE_WITH_KNOTS ( 'NONE', 3,
 ( #38393, #23047, #32137, #27418, #28046, #9237 ),
 .UNSPECIFIED., .F., .F.,
 ( 4, 2, 4 ),
 ( 3.511543213478341086E-18, 0.0002445244328975378903, 0.0004890488657950722027 ),
 .UNSPECIFIED. ) ;
#10343 = VERTEX_POINT ( 'NONE', #52662 ) ;
#10344 = FACE_OUTER_BOUND ( 'NONE', #55218, .T. ) ;
#10345 = DIRECTION ( 'NONE',  ( -0.000000000000000000, -0.000000000000000000, -1.000000000000000000 ) ) ;
#10346 = EDGE_LOOP ( 'NONE', ( #17085, #9062, #22073, #17670 ) ) ;
#10347 = CARTESIAN_POINT ( 'NONE',  ( 2.526464513654345545, -27.11556434133527205, -33.34586834545800826 ) ) ;
#10348 = ORIENTED_EDGE ( 'NONE', *, *, #54801, .T. ) ;
#10349 = FACE_BOUND ( 'NONE', #25658, .T. ) ;
#10350 = VERTEX_POINT ( 'NONE', #37 ) ;
#10351 = CARTESIAN_POINT ( 'NONE',  ( 0.1147471544378677460, 29.43420442011967353, -32.87217362189262815 ) ) ;
#10352 = CYLINDRICAL_SURFACE ( 'NONE', #55342, 2.649999999999992806 ) ;
#10353 = ORIENTED_EDGE ( 'NONE', *, *, #37586, .F. ) ;
#10354 = CARTESIAN_POINT ( 'NONE',  ( 0.5804410086790514622, -19.24447200597979801, 42.76879877979338573 ) ) ;
#10355 = PRODUCT_DEFINITION_SHAPE ( 'NONE', 'NONE',  #61998 ) ;
#10356 = B_SPLINE_CURVE_WITH_KNOTS ( 'NONE', 3,
 ( #17145, #27149, #31860, #17445 ),
 .UNSPECIFIED., .F., .F.,
 ( 4, 4 ),
 ( 1.734723475976807094E-18, 0.004042984057420977162 ),
 .UNSPECIFIED. ) ;
#10357 = ORIENTED_EDGE ( 'NONE', *, *, #10418, .F. ) ;
#10359 = B_SPLINE_CURVE_WITH_KNOTS ( 'NONE', 3,
 ( #31923, #13757, #60393, #32862 ),
 .UNSPECIFIED., .F., .F.,
 ( 4, 4 ),
 ( 5.421010862427521207E-19, 0.004444878191957687789 ),
 .UNSPECIFIED. ) ;
#10358 = CARTESIAN_POINT ( 'NONE',  ( 0.9762797500689124330, 19.69530149098714489, -36.99215976885945167 ) ) ;
#10360 = CARTESIAN_POINT ( 'NONE',  ( 0.5807400328401574052, -11.87003418057276072, 46.40483864045141615 ) ) ;
#10361 =( BOUNDED_SURFACE ( )  B_SPLINE_SURFACE ( 3, 1, ( 
 ( #43304, #15716 ),
 ( #33585, #10393 ),
 ( #972, #1270 ),
 ( #15096, #58275 ) ),
 .UNSPECIFIED., .F., .F., .F. ) 
 B_SPLINE_SURFACE_WITH_KNOTS ( ( 4, 4 ),
 ( 2, 2 ),
 ( 0.000000000000000000, 1.000000000000000000 ),
 ( 0.000000000000000000, 1.000000000000000000 ),
 .UNSPECIFIED. ) 
 GEOMETRIC_REPRESENTATION_ITEM ( )  RATIONAL_B_SPLINE_SURFACE ( (
 ( 1.000000000000000000, 1.000000000000000000),
 ( 0.7223157951917476005, 0.9931996967497186413),
 ( 0.7223157951917476005, 0.9931996967497186413),
 ( 1.000000000000000000, 1.000000000000000000) ) ) 
 REPRESENTATION_ITEM ( '' )  SURFACE ( )  );
#10362 = B_SPLINE_CURVE_WITH_KNOTS ( 'NONE', 3,
 ( #29191, #25111, #58924, #16036 ),
 .UNSPECIFIED., .F., .F.,
 ( 4, 4 ),
 ( 1.843143693225357538E-18, 0.004446298630425066754 ),
 .UNSPECIFIED. ) ;
#10363 = CARTESIAN_POINT ( 'NONE',  ( 0.6001305935487422083, 46.60388846085706405, 11.94532529598394177 ) ) ;
#10364 = VERTEX_POINT ( 'NONE', #52353 ) ;
#10365 = CARTESIAN_POINT ( 'NONE',  ( 1.199999999999992628, 0.000000000000000000, 0.000000000000000000 ) ) ;
#10366 = CARTESIAN_POINT ( 'NONE',  ( 2.533389852662419894, -36.19900187127336011, -25.04162125856002774 ) ) ;
#10367 = CARTESIAN_POINT ( 'NONE',  ( 0.5837800005270546988, 32.60172451818726103, -33.70998097124964232 ) ) ;
#10368 = CARTESIAN_POINT ( 'NONE',  ( 0.3676999524040323597, -6.224421213753346116, -43.67158302462387098 ) ) ;
#10369 = ORIENTED_EDGE ( 'NONE', *, *, #36670, .T. ) ;
#10370 = CARTESIAN_POINT ( 'NONE',  ( 1.231276596079881935, 3.353048872156085825, 41.78556968953515849 ) ) ;
#10371 = CARTESIAN_POINT ( 'NONE',  ( 0.1154773475650540948, -17.69611726026696985, 40.42018139440992996 ) ) ;
#10372 = VERTEX_POINT ( 'NONE', #57970 ) ;
#10373 = AXIS2_PLACEMENT_3D ( 'NONE', #14401, #14709, #52901 ) ;
#10374 = LINE ( 'NONE', #47970, #35785 ) ;
#10375 = EDGE_LOOP ( 'NONE', ( #55963, #31004, #46719, #50409 ) ) ;
#10376 = CARTESIAN_POINT ( 'NONE',  ( 2.301529144917015213, -7.543875168382815133, -47.43735140118861437 ) ) ;
#10377 = APPLICATION_CONTEXT ( 'automotive_design' ) ;
#10378 = EDGE_CURVE ( 'NONE', #23031, #29746, #48590, .T. ) ;
#10379 = CARTESIAN_POINT ( 'NONE',  ( 0.9790850452238872847, 40.40622100481030543, -11.12090978174100542 ) ) ;
#10380 = ORIENTED_EDGE ( 'NONE', *, *, #43275, .F. ) ;
#10381 = CARTESIAN_POINT ( 'NONE',  ( 0.9775691876210976794, -12.05521307728244373, -40.13733357675007341 ) ) ;
#10382 = CARTESIAN_POINT ( 'NONE',  ( 4.967162193818130511, 0.000000000000000000, 0.000000000000000000 ) ) ;
#10383 = DIRECTION ( 'NONE',  ( -1.000000000000000000, -0.000000000000000000, -0.000000000000000000 ) ) ;
#10384 = CARTESIAN_POINT ( 'NONE',  ( 0.1064266418746776244, -40.05351192729372656, 15.98292515284391335 ) ) ;
#10385 = B_SPLINE_CURVE_WITH_KNOTS ( 'NONE', 3,
 ( #37601, #61357, #38524, #22865, #61061, #18474, #13793, #32897, #9065, #47288, #4336, #18795, #37921, #34132, #35058, #35368, #40086, #34434 ),
 .UNSPECIFIED., .F., .F.,
 ( 4, 2, 2, 2, 2, 2, 2, 2, 4 ),
 ( 0.008300350213780812239, 0.008819185130678563675, 0.009338020047576315111, 0.009856854964474064812, 0.01037568988137181625, 0.01089452479826956768, 0.01141335971516731912, 0.01193219463206507056, 0.01245102954896282026 ),
 .UNSPECIFIED. ) ;
#10386 = VERTEX_POINT ( 'NONE', #37680 ) ;
#10387 = CARTESIAN_POINT ( 'NONE',  ( 0.1145239942831223490, -41.02090207429923652, 16.25518605600765909 ) ) ;
#10388 = DIRECTION ( 'NONE',  ( 0.000000000000000000, 0.000000000000000000, -1.000000000000000000 ) ) ;
#10389 = CARTESIAN_POINT ( 'NONE',  ( 0.7057020205115037692, -5.417413437617267569, -47.59410670607645955 ) ) ;
#10390 = VECTOR ( 'NONE', #21757, 1000.000000000000114 ) ;
#10391 = CARTESIAN_POINT ( 'NONE',  ( 0.5809828226811553087, -44.03860873105708151, 18.83114015454682999 ) ) ;
#10392 = DIRECTION ( 'NONE',  ( 0.000000000000000000, 0.000000000000000000, 1.000000000000000000 ) ) ;
#10393 = CARTESIAN_POINT ( 'NONE',  ( 4.322998006666179727, -39.32552843303831480, -27.50295597456437591 ) ) ;
#10394 = CARTESIAN_POINT ( 'NONE',  ( 0.5997462898726536595, -47.36625756029543055, 12.96106765957438789 ) ) ;
#10395 = CARTESIAN_POINT ( 'NONE',  ( 5.960721111146673579, 20.35079619394246109, -2.672857320903093914 ) ) ;
#10396 = CARTESIAN_POINT ( 'NONE',  ( 0.3622758884714600280, -33.69533458712325569, -26.89560658783373626 ) ) ;
#10397 = CARTESIAN_POINT ( 'NONE',  ( 0.9754402186311922351, 30.20795797590442433, -30.47320128434230924 ) ) ;
#10398 = CARTESIAN_POINT ( 'NONE',  ( 0.1158816050234199174, -43.76263342502616638, -5.636839274978773240 ) ) ;
#10399 = CARTESIAN_POINT ( 'NONE',  ( 4.549368137175248350, -38.40568845698290801, 19.17571786012255686 ) ) ;
#10400 = CARTESIAN_POINT ( 'NONE',  ( 4.956445790444026223, 2.113652668516905031, -47.04328350079857302 ) ) ;
#10401 = ADVANCED_FACE ( 'NONE', ( #47363 ), #641, .F. ) ;
#10402 = EDGE_CURVE ( 'NONE', #2702, #45432, #9758, .T. ) ;
#10403 = CARTESIAN_POINT ( 'NONE',  ( 0.8751705887134423323, 48.08707113907594533, 0.8911681664090089772 ) ) ;
#10404 = CARTESIAN_POINT ( 'NONE',  ( 0.5997462898726536595, -45.31995669577361951, 18.91172004968117903 ) ) ;
#10405 = ORIENTED_EDGE ( 'NONE', *, *, #19682, .F. ) ;
#10406 = DIRECTION ( 'NONE',  ( 0.09722883295013597105, -0.6264263058867871603, 0.7733929385093892828 ) ) ;
#10407 = CARTESIAN_POINT ( 'NONE',  ( 0.9789233960466696693, -1.531799179696195834, 41.88066759383647053 ) ) ;
#10408 = CARTESIAN_POINT ( 'NONE',  ( -6.016761891674564211, 9.418621820384725396, -16.32039929810246903 ) ) ;
#10409 = EDGE_CURVE ( 'NONE', #43794, #30127, #51738, .T. ) ;
#10410 = ORIENTED_EDGE ( 'NONE', *, *, #53238, .F. ) ;
#10411 = CARTESIAN_POINT ( 'NONE',  ( 5.959828726073459926, -20.35060134307036250, 2.674641840415830085 ) ) ;
#10412 = CARTESIAN_POINT ( 'NONE',  ( 0.9268187852002115479, 26.03038468280454865, 35.58333045365259295 ) ) ;
#10413 = CIRCLE ( 'NONE', #51389, 6.887500000000022382 ) ;
#10414 = VERTEX_POINT ( 'NONE', #48289 ) ;
#10415 = ORIENTED_EDGE ( 'NONE', *, *, #33199, .F. ) ;
#10416 = CARTESIAN_POINT ( 'NONE',  ( 0.1129192098497455998, -43.82135468580280957, 5.161459220629533107 ) ) ;
#10417 = ORIENTED_EDGE ( 'NONE', *, *, #34037, .T. ) ;
#10418 = EDGE_CURVE ( 'NONE', #45083, #58239, #47317, .T. ) ;
#10419 = CARTESIAN_POINT ( 'NONE',  ( 0.5980894510889448457, 24.66136644716821280, -41.31170365136863154 ) ) ;
#10420 = VERTEX_POINT ( 'NONE', #21329 ) ;
#10421 = ORIENTED_EDGE ( 'NONE', *, *, #36102, .T. ) ;
#10422 = CARTESIAN_POINT ( 'NONE',  ( -6.078457390727109555, 7.790511441124012393, 17.60972579352738521 ) ) ;
#10424 = ORIENTED_EDGE ( 'NONE', *, *, #38991, .F. ) ;
#10423 = EDGE_CURVE ( 'NONE', #24845, #45260, #37572, .T. ) ;
#10425 = CARTESIAN_POINT ( 'NONE',  ( 3.240649175237395596, -43.95364737320741710, -1.828059077105528951 ) ) ;
#10426 = LINE ( 'NONE', #24830, #18072 ) ;
#10427 = CIRCLE ( 'NONE', #36470, 0.1000000000000002554 ) ;
#10428 = CARTESIAN_POINT ( 'NONE',  ( 0.9788927965476030835, -17.76925533521107425, -37.95510739628922892 ) ) ;
#10429 = EDGE_LOOP ( 'NONE', ( #5535, #31289, #21635, #60056 ) ) ;
#10430 = CARTESIAN_POINT ( 'NONE',  ( 0.8753041380234465318, 27.35839019124359339, 40.77568900725830758 ) ) ;
#10431 = CARTESIAN_POINT ( 'NONE',  ( 0.9745511491811756910, -33.83313387735770306, -26.39034508612568075 ) ) ;
#10432 = ORIENTED_EDGE ( 'NONE', *, *, #3372, .T. ) ;
#10433 = VERTEX_POINT ( 'NONE', #26027 ) ;
#10434 = CARTESIAN_POINT ( 'NONE',  ( 0.1147471544378677183, 43.25016557451949240, -8.739300100688538464 ) ) ;
#10435 = CARTESIAN_POINT ( 'NONE',  ( -5.995132425357893702, -17.40647075750111483, -7.219211173946675331 ) ) ;
#10436 = CARTESIAN_POINT ( 'NONE',  ( 0.8760168074887076939, 5.394043284319499421, -47.80016357497244428 ) ) ;
#10437 = CARTESIAN_POINT ( 'NONE',  ( 0.9785694773339259633, 35.94433939501183772, 21.54854684592147862 ) ) ;
#10438 = CARTESIAN_POINT ( 'NONE',  ( 0.6064782688330866423, -0.8565416045440378268, -46.88923952143449725 ) ) ;
#10439 = ORIENTED_EDGE ( 'NONE', *, *, #9858, .T. ) ;
#10440 = CARTESIAN_POINT ( 'NONE',  ( 0.1155031312995260795, -1.245823167979823065, -44.10657045345890026 ) ) ;
#10441 = CARTESIAN_POINT ( 'NONE',  ( 1.000110580585050979, 41.44288208944681884, 6.237387826014257897 ) ) ;
#10442 = CARTESIAN_POINT ( 'NONE',  ( 5.901764892641288895, -10.85461099010664654, 47.75111399426337044 ) ) ;
#10443 = EDGE_CURVE ( 'NONE', #23055, #53844, #30107, .T. ) ;
#10444 = LINE ( 'NONE', #12309, #31039 ) ;
#10445 = ORIENTED_EDGE ( 'NONE', *, *, #18274, .T. ) ;
#10446 = CARTESIAN_POINT ( 'NONE',  ( 0.1129192098497455998, -38.20615368646939203, -22.07354996984027196 ) ) ;
#10447 = CARTESIAN_POINT ( 'NONE',  ( 0.6016117650947689910, -14.30605072330158833, -46.97752619015630415 ) ) ;
#10448 = CARTESIAN_POINT ( 'NONE',  ( -1.139999999999998570, 8.422079734756228398E-16, 6.866799999999992465 ) ) ;
#10449 = CARTESIAN_POINT ( 'NONE',  ( 0.9754292589017203863, 41.90451262005537103, -0.5824851679641472879 ) ) ;
#10450 = ORIENTED_EDGE ( 'NONE', *, *, #2958, .T. ) ;
#10451 = ORIENTED_EDGE ( 'NONE', *, *, #1057, .F. ) ;
#10452 = CARTESIAN_POINT ( 'NONE',  ( 5.965394784446460541, 16.27505370423064335, 12.50653125159012902 ) ) ;
#10453 = CARTESIAN_POINT ( 'NONE',  ( 0.9968887458511658251, -20.88287852258416777, -37.48500720268749120 ) ) ;
#10454 = CARTESIAN_POINT ( 'NONE',  ( 0.9790850452238869517, 15.01504043229814833, -39.12653691651804166 ) ) ;
#10456 = B_SPLINE_CURVE_WITH_KNOTS ( 'NONE', 3,
 ( #14634, #818, #52822, #58426, #44086, #11160, #9927, #24324, #38758, #58734, #19639, #34054, #43454, #30241, #48742, #498 ),
 .UNSPECIFIED., .F., .F.,
 ( 4, 3, 3, 3, 3, 4 ),
 ( 1.250973872328959318E-17, 0.0002724568934985488250, 0.0004086836638483747801, 0.0005449104342063555619, 0.0008173270854453591923, 0.001089761613562688792 ),
 .UNSPECIFIED. ) ;
#10455 = LINE ( 'NONE', #10771, #8793 ) ;
#10457 = CARTESIAN_POINT ( 'NONE',  ( 0.8560838555295223751, -20.57050347530454104, -42.15717282805163535 ) ) ;
#10458 = CARTESIAN_POINT ( 'NONE',  ( 0.1140933569871965259, -31.95931914376139105, 30.42288398477553812 ) ) ;
#10459 = CARTESIAN_POINT ( 'NONE',  ( 0.6067375320500718594, 47.57460111700607541, -5.548194933739688750 ) ) ;
#10460 =( BOUNDED_SURFACE ( )  B_SPLINE_SURFACE ( 3, 1, ( 
 ( #13775, #42584 ),
 ( #45588, #40593 ),
 ( #25226, #44668 ),
 ( #26152, #21455 ) ),
 .UNSPECIFIED., .F., .F., .F. ) 
 B_SPLINE_SURFACE_WITH_KNOTS ( ( 4, 4 ),
 ( 2, 2 ),
 ( 0.000000000000000000, 1.000000000000000000 ),
 ( 0.000000000000000000, 1.000000000000000000 ),
 .UNSPECIFIED. ) 
 GEOMETRIC_REPRESENTATION_ITEM ( )  RATIONAL_B_SPLINE_SURFACE ( (
 ( 1.000000000000000000, 1.000000000000000000),
 ( 0.9953390228620291325, 0.8624445117761032620),
 ( 0.9953390228620291325, 0.8624445117761032620),
 ( 1.000000000000000000, 1.000000000000000000) ) ) 
 REPRESENTATION_ITEM ( '' )  SURFACE ( )  );
#10461 = CARTESIAN_POINT ( 'NONE',  ( 0.9722240741986374335, 37.44729083276452997, -20.94823706911160954 ) ) ;
#10462 = CARTESIAN_POINT ( 'NONE',  ( 0.1101816497532063233, 30.39741055095859323, -30.58948775778055662 ) ) ;
#10463 = CARTESIAN_POINT ( 'NONE',  ( 0.5807400328401574052, 33.48217046439112465, 34.25275203086247444 ) ) ;
#10464 = ORIENTED_EDGE ( 'NONE', *, *, #32109, .F. ) ;
#10465 = CARTESIAN_POINT ( 'NONE',  ( 0.9754292580325125694, 15.60437149020586034, -38.89512896622989047 ) ) ;
#10466 = CARTESIAN_POINT ( 'NONE',  ( 0.8557997880470697982, -41.02602466100796619, 24.73961900479237386 ) ) ;
#10467 = CARTESIAN_POINT ( 'NONE',  ( 4.335381028904216727, -43.68634339260488275, -22.16439145674328159 ) ) ;
#10468 = CARTESIAN_POINT ( 'NONE',  ( 3.678748215320120529, -47.80914536661616410, -10.62536745779876313 ) ) ;
#10469 = CIRCLE ( 'NONE', #1449, 2.500000000000002220 ) ;
#10470 = CARTESIAN_POINT ( 'NONE',  ( -6.078726893082806448, 7.791390017580341443, -17.60932374802251132 ) ) ;
#10471 = CARTESIAN_POINT ( 'NONE',  ( 0.3263565795980677420, -4.430380094434308802, -0.2484800633750392507 ) ) ;
#10472 = DIRECTION ( 'NONE',  ( 0.1011922191286468292, 0.8407325376063271571, 0.5319106456895233981 ) ) ;
#10473 = CARTESIAN_POINT ( 'NONE',  ( 0.9752132459055861124, -25.93579301218381161, 34.18286753639630859 ) ) ;
#10474 = B_SPLINE_CURVE_WITH_KNOTS ( 'NONE', 3,
 ( #52311, #43890, #933, #4996, #24125, #43264 ),
 .UNSPECIFIED., .F., .F.,
 ( 4, 2, 4 ),
 ( 9.341771812940338307E-18, 0.0002291978881530153469, 0.0004583957763060213155 ),
 .UNSPECIFIED. ) ;
#10475 = CARTESIAN_POINT ( 'NONE',  ( 5.959828726073459926, -16.28681682518055851, -12.49160845136029252 ) ) ;
#10476 = ADVANCED_FACE ( 'NONE', ( #54191 ), #8696, .F. ) ;
#10477 = CARTESIAN_POINT ( 'NONE',  ( 4.962356264823608143, -25.31392337492896161, 33.62202970123266965 ) ) ;
#10478 = FACE_OUTER_BOUND ( 'NONE', #42129, .T. ) ;
#10480 = ORIENTED_EDGE ( 'NONE', *, *, #36378, .F. ) ;
#10479 = DIRECTION ( 'NONE',  ( 0.000000000000000000, 0.000000000000000000, 1.000000000000000000 ) ) ;
#10481 = ORIENTED_EDGE ( 'NONE', *, *, #61075, .F. ) ;
#10482 = CARTESIAN_POINT ( 'NONE',  ( 0.7056313189692711152, -24.52218711664568218, 39.98013235312978253 ) ) ;
#10483 = CARTESIAN_POINT ( 'NONE',  ( 0.5809828226811560858, -11.86925843957200222, 46.40184912890835278 ) ) ;
#10484 = CARTESIAN_POINT ( 'NONE',  ( 4.962356264823609031, -24.61258717641066696, -34.13877780978592824 ) ) ;
#10485 = ADVANCED_FACE ( 'NONE', ( #49515 ), #266, .F. ) ;
#10486 = ORIENTED_EDGE ( 'NONE', *, *, #39334, .F. ) ;
#10487 = DIRECTION ( 'NONE',  ( -1.000000000000000000, -0.000000000000000000, -0.000000000000000000 ) ) ;
#10488 = CARTESIAN_POINT ( 'NONE',  ( 4.967162193818130511, 0.000000000000000000, 0.000000000000000000 ) ) ;
#10489 = CARTESIAN_POINT ( 'NONE',  ( 5.895596859100789899, -19.39731145114851074, 5.317188324634581242 ) ) ;
#10490 = VERTEX_POINT ( 'NONE', #49208 ) ;
#10491 = ORIENTED_EDGE ( 'NONE', *, *, #1079, .F. ) ;
#10492 = FACE_OUTER_BOUND ( 'NONE', #46819, .T. ) ;
#10493 = DIRECTION ( 'NONE',  ( 0.000000000000000000, 0.000000000000000000, 1.000000000000000000 ) ) ;
#10494 = CARTESIAN_POINT ( 'NONE',  ( 0.5997462898726536595, -1.051648045107538954, 49.09628974305014992 ) ) ;
#10495 = CARTESIAN_POINT ( 'NONE',  ( 0.6253024248130483187, 36.94306049113323809, 32.35204025971334119 ) ) ;
#10496 = ADVANCED_FACE ( 'NONE', ( #11015 ), #15115, .F. ) ;
#10497 = DIRECTION ( 'NONE',  ( 0.09835009131224552170, 0.007732607185417008852, 0.9951218349151971232 ) ) ;
#10498 = CARTESIAN_POINT ( 'NONE',  ( -6.078726893082806448, -16.14009859332552921, 10.50196451462540992 ) ) ;
#10499 = CIRCLE ( 'NONE', #18509, 43.08621763946400307 ) ;
#10500 = CARTESIAN_POINT ( 'NONE',  ( 0.5807400328401637335, -6.791881299635273095, -47.41494605191449807 ) ) ;
#10501 = ORIENTED_EDGE ( 'NONE', *, *, #32217, .T. ) ;
#10502 = ORIENTED_EDGE ( 'NONE', *, *, #30529, .T. ) ;
#10503 = CARTESIAN_POINT ( 'NONE',  ( 0.1129192098497455998, 43.40062318508800843, -7.958498283668546947 ) ) ;
#10504 = CARTESIAN_POINT ( 'NONE',  ( -6.063463321072276813, 19.10058954492596328, 2.447025033736856425 ) ) ;
#10505 = VECTOR ( 'NONE', #12494, 1000.000000000000000 ) ;
#10506 = VERTEX_POINT ( 'NONE', #31033 ) ;
#10507 = CARTESIAN_POINT ( 'NONE',  ( 0.8557997880470599172, 41.93815086860288943, -23.15977007032279289 ) ) ;
#10508 = CARTESIAN_POINT ( 'NONE',  ( 2.648799415243708655, -45.95403142182570377, -17.10977671892458929 ) ) ;
#10509 = CARTESIAN_POINT ( 'NONE',  ( 0.8554163680231816613, 33.26717477998048622, 33.08323677136276331 ) ) ;
#10510 = DIRECTION ( 'NONE',  ( 1.000000000000000000, 0.000000000000000000, 0.000000000000000000 ) ) ;
#10511 = VECTOR ( 'NONE', #23069, 1000.000000000000000 ) ;
#10512 = VERTEX_POINT ( 'NONE', #50142 ) ;
#10513 = CARTESIAN_POINT ( 'NONE',  ( 1.227938101723748288, 25.45152231597057124, 34.55893248994515687 ) ) ;
#10514 = DIRECTION ( 'NONE',  ( -1.000000000000000000, -0.000000000000000000, -0.000000000000000000 ) ) ;
#10515 = CARTESIAN_POINT ( 'NONE',  ( 0.1100053167205930632, -37.43629428538748272, -21.40663161100980005 ) ) ;
#10516 = CARTESIAN_POINT ( 'NONE',  ( 5.960721111146673579, -17.77882586010674260, 10.25731071096551794 ) ) ;
#10517 = ORIENTED_EDGE ( 'NONE', *, *, #53159, .F. ) ;
#10518 = LINE ( 'NONE', #2328, #6493 ) ;
#10519 = ORIENTED_EDGE ( 'NONE', *, *, #44360, .F. ) ;
#10520 = CARTESIAN_POINT ( 'NONE',  ( 0.5804410086790514622, 23.01644811389265399, -40.86273324284467634 ) ) ;
#10521 = B_SPLINE_CURVE_WITH_KNOTS ( 'NONE', 3,
 ( #30872, #27109, #11793, #50290, #6727, #40930, #25869, #60289, #16798, #2044, #12407, #31494, #22102, #54975, #55282, #36843, #50590, #35909, #41229 ),
 .UNSPECIFIED., .F., .F.,
 ( 4, 3, 3, 3, 3, 3, 4 ),
 ( 7.758676801208396025E-18, 0.0002732106629380558725, 0.0004098138914053752694, 0.0005464171197651503760, 0.0006830203481512575007, 0.0008196235766963642835, 0.001011968216111138559 ),
 .UNSPECIFIED. ) ;
#10522 = ORIENTED_EDGE ( 'NONE', *, *, #41062, .F. ) ;
#10523 = CARTESIAN_POINT ( 'NONE',  ( 0.2224561200757607382, 39.54039348282956468, 17.20021002050938463 ) ) ;
#10524 = CARTESIAN_POINT ( 'NONE',  ( 5.896782393890504181, -11.93563916323470764, -16.18847134979303704 ) ) ;
#10525 = CARTESIAN_POINT ( 'NONE',  ( 1.227938101723748288, -39.96870412324346944, 15.63977281655828300 ) ) ;
#10526 = EDGE_CURVE ( 'NONE', #5033, #19687, #45785, .T. ) ;
#10527 = DIRECTION ( 'NONE',  ( -0.07500201931887529039, 0.9899952385360571983, 0.1195162113440108032 ) ) ;
#10528 =( BOUNDED_SURFACE ( )  B_SPLINE_SURFACE ( 3, 1, ( 
 ( #50304, #17729 ),
 ( #40633, #54990 ),
 ( #36231, #45329 ),
 ( #50003, #21188 ) ),
 .UNSPECIFIED., .F., .F., .F. ) 
 B_SPLINE_SURFACE_WITH_KNOTS ( ( 4, 4 ),
 ( 2, 2 ),
 ( 0.000000000000000000, 1.000000000000000000 ),
 ( 0.000000000000000000, 1.000000000000000000 ),
 .UNSPECIFIED. ) 
 GEOMETRIC_REPRESENTATION_ITEM ( )  RATIONAL_B_SPLINE_SURFACE ( (
 ( 1.000000000000000000, 1.000000000000000000),
 ( 0.9732289882329797637, 0.9999525324661233672),
 ( 0.9732289882329797637, 0.9999525324661233672),
 ( 1.000000000000000000, 1.000000000000000000) ) ) 
 REPRESENTATION_ITEM ( '' )  SURFACE ( )  );
#10529 = CARTESIAN_POINT ( 'NONE',  ( 5.910764540655178756, -7.214026563325572461, 18.77389302230083601 ) ) ;
#10530 = DIRECTION ( 'NONE',  ( 0.000000000000000000, 0.000000000000000000, 1.000000000000000000 ) ) ;
#10531 = CARTESIAN_POINT ( 'NONE',  ( 0.8557997880470599172, 47.60865952217007191, -5.347802024196765203 ) ) ;
#10532 = CARTESIAN_POINT ( 'NONE',  ( 40.00000000000000000, 7.347638122934295104E-15, -7.703719777548943412E-31 ) ) ;
#10533 = ORIENTED_EDGE ( 'NONE', *, *, #60624, .F. ) ;
#10534 = EDGE_CURVE ( 'NONE', #18237, #32229, #20405, .T. ) ;
#10535 = CARTESIAN_POINT ( 'NONE',  ( 0.9741495583595158880, 39.79188455996743556, -16.05424148287283614 ) ) ;
#10536 = CARTESIAN_POINT ( 'NONE',  ( 1.092182651088186018, 14.33286397384261690, -39.38692923737020379 ) ) ;
#10537 = CARTESIAN_POINT ( 'NONE',  ( 0.6067375320500736358, -24.55990317723886562, 41.12099578548244239 ) ) ;
#10538 = ORIENTED_EDGE ( 'NONE', *, *, #42818, .T. ) ;
#10540 = MANIFOLD_SOLID_BREP ( 'Move Face1', #53014 ) ;
#10539 = CARTESIAN_POINT ( 'NONE',  ( 4.962356264823608143, 41.96072444189411499, 3.245489512196318316 ) ) ;
#10541 = CARTESIAN_POINT ( 'NONE',  ( -6.010958268070873523, -11.48268200989207877, 14.94067681728545871 ) ) ;
#10542 = CARTESIAN_POINT ( 'NONE',  ( 0.1073791018717578927, -26.63563652260192427, 33.91564619577761874 ) ) ;
#10543 = CARTESIAN_POINT ( 'NONE',  ( 2.624215991343608501, -4.864192649745077368, -47.76052319582220917 ) ) ;
#10544 = B_SPLINE_CURVE_WITH_KNOTS ( 'NONE', 3,
 ( #12466, #12166, #60349, #3647 ),
 .UNSPECIFIED., .F., .F.,
 ( 4, 4 ),
 ( 0.000000000000000000, 0.005004948556313811373 ),
 .UNSPECIFIED. ) ;
#10545 = CARTESIAN_POINT ( 'NONE',  ( 0.6016118706126977189, -20.19594048258466756, 44.76242891988579942 ) ) ;
#10546 = CARTESIAN_POINT ( 'NONE',  ( 0.6031356755773454870, 38.16618524502122511, -29.28597628606506831 ) ) ;
#10547 = CARTESIAN_POINT ( 'NONE',  ( 2.618530812446115519, 23.81615347600926214, 40.52798567416559194 ) ) ;
#10548 = CARTESIAN_POINT ( 'NONE',  ( 0.6027935024548037868, -0.1745403365874843293, 48.10716172909472022 ) ) ;
#10549 = CONICAL_SURFACE ( 'NONE', #53536, 43.08621763946400307, 1.568696531533066763 ) ;
#10550 = ADVANCED_FACE ( 'NONE', ( #61064 ), #53888, .T. ) ;
#10551 = CARTESIAN_POINT ( 'NONE',  ( 0.9784957157296381158, 28.96678784324410927, -30.28627179163612126 ) ) ;
#10553 = EDGE_LOOP ( 'NONE', ( #61787, #10451, #682, #20587 ) ) ;
#10552 = DIRECTION ( 'NONE',  ( -1.000000000000000000, -0.000000000000000000, -0.000000000000000000 ) ) ;
#10554 = VERTEX_POINT ( 'NONE', #40775 ) ;
#10555 = CARTESIAN_POINT ( 'NONE',  ( 4.956653778116975495, -27.17045123668499684, 39.67974989265029961 ) ) ;
#10556 = AXIS2_PLACEMENT_3D ( 'NONE', #46956, #47247, #8392 ) ;
#10557 = CARTESIAN_POINT ( 'NONE',  ( 10.00000000000000533, 1.836909530733574959E-15, -1.925929944387237167E-31 ) ) ;
#10558 = CARTESIAN_POINT ( 'NONE',  ( 4.962356264823608143, -38.57439820587617163, -16.83007429920747811 ) ) ;
#10559 = EDGE_CURVE ( 'NONE', #5852, #43474, #35354, .T. ) ;
#10560 = AXIS2_PLACEMENT_3D ( 'NONE', #40517, #17934, #45518 ) ;
#10561 = CARTESIAN_POINT ( 'NONE',  ( 1.154321485836933503, 0.8253076867718968090, 42.90848031452335221 ) ) ;
#10562 = CARTESIAN_POINT ( 'NONE',  ( 0.5809828226811617480, -47.55412398569210808, 5.711058609465143654 ) ) ;
#10564 = B_SPLINE_CURVE_WITH_KNOTS ( 'NONE', 3,
 ( #10981, #15372, #10044, #5311, #10665, #38883 ),
 .UNSPECIFIED., .F., .F.,
 ( 4, 2, 4 ),
 ( 0.000000000000000000, 0.0002447195606305751256, 0.0004894391212611502512 ),
 .UNSPECIFIED. ) ;
#10563 = CARTESIAN_POINT ( 'NONE',  ( 0.5988103564986357874, 11.86435738293443087, -46.62176022926374941 ) ) ;
#10565 = EDGE_CURVE ( 'NONE', #25757, #37959, #26848, .T. ) ;
#10566 = VERTEX_POINT ( 'NONE', #45464 ) ;
#10567 = ORIENTED_EDGE ( 'NONE', *, *, #28129, .F. ) ;
#10568 = CARTESIAN_POINT ( 'NONE',  ( 4.999999999999986677, 54.69470952478017267, -58.44237546506749936 ) ) ;
#10569 = B_SPLINE_CURVE_WITH_KNOTS ( 'NONE', 3,
 ( #7015, #42057, #32325, #21450 ),
 .UNSPECIFIED., .F., .F.,
 ( 4, 4 ),
 ( 0.000000000000000000, 0.005004741218457419739 ),
 .UNSPECIFIED. ) ;
#10570 = CARTESIAN_POINT ( 'NONE',  ( -18.25036807083938228, -7.723231599531199976, 2.086259205976699338 ) ) ;
#10571 = LINE ( 'NONE', #43487, #3767 ) ;
#10572 = EDGE_LOOP ( 'NONE', ( #49952, #19279, #17902, #12243 ) ) ;
#10573 = EDGE_CURVE ( 'NONE', #7870, #47838, #53781, .T. ) ;
#10574 = CARTESIAN_POINT ( 'NONE',  ( 5.981074661064941900, -12.48781255314277772, -16.28853686865594952 ) ) ;
#10575 = CARTESIAN_POINT ( 'NONE',  ( 4.962356264823596597, -3.779019546647577776, 41.91604238389407300 ) ) ;
#10576 = B_SPLINE_CURVE_WITH_KNOTS ( 'NONE', 3,
 ( #47096, #13895, #12975, #27051, #46480, #55534 ),
 .UNSPECIFIED., .F., .F.,
 ( 4, 2, 4 ),
 ( 0.000000000000000000, 0.0002447195606305753966, 0.0004894391212611507933 ),
 .UNSPECIFIED. ) ;
#10577 = VERTEX_POINT ( 'NONE', #59840 ) ;
#10578 = CARTESIAN_POINT ( 'NONE',  ( 0.5800708057587408151, 28.65679888493058058, 38.37709891224474035 ) ) ;
#10579 = ORIENTED_EDGE ( 'NONE', *, *, #41949, .T. ) ;
#10580 = CARTESIAN_POINT ( 'NONE',  ( 1.000110580585050091, 4.849091690273542810, -41.62816105175947001 ) ) ;
#10581 = CARTESIAN_POINT ( 'NONE',  ( -6.072942160501519915, -1.863502906426155015, -19.16589468839797306 ) ) ;
#10582 = ORIENTED_EDGE ( 'NONE', *, *, #43161, .T. ) ;
#10583 = CARTESIAN_POINT ( 'NONE',  ( 0.5988103622719989083, 23.52668907282285460, 41.96244039798798298 ) ) ;
#10584 = FACE_OUTER_BOUND ( 'NONE', #28680, .T. ) ;
#10585 = CARTESIAN_POINT ( 'NONE',  ( 0.8744876279028263033, 21.91587810745035725, 43.93226988398016886 ) ) ;
#10586 = CARTESIAN_POINT ( 'NONE',  ( 5.571549742892842438, -9.254395351074542475, -1.199999999999999956 ) ) ;
#10587 = VERTEX_POINT ( 'NONE', #16955 ) ;
#10588 = B_SPLINE_CURVE_WITH_KNOTS ( 'NONE', 3,
 ( #24207, #38641, #57695, #19224 ),
 .UNSPECIFIED., .F., .F.,
 ( 4, 4 ),
 ( 2.860979249076398407E-17, 0.005004741218457448362 ),
 .UNSPECIFIED. ) ;
#10589 = CARTESIAN_POINT ( 'NONE',  ( 0.8560838555295223751, -46.14148336882287538, -8.446084690930739214 ) ) ;
#10590 = B_SPLINE_CURVE_WITH_KNOTS ( 'NONE', 3,
 ( #15508, #9020, #56933, #14055 ),
 .UNSPECIFIED., .F., .F.,
 ( 4, 4 ),
 ( 3.469446951953613804E-18, 0.005004741218457419739 ),
 .UNSPECIFIED. ) ;
#10591 = VERTEX_POINT ( 'NONE', #56363 ) ;
#10592 = LINE ( 'NONE', #34713, #40229 ) ;
#10593 = B_SPLINE_CURVE_WITH_KNOTS ( 'NONE', 3,
 ( #44701, #11173, #49678, #34993 ),
 .UNSPECIFIED., .F., .F.,
 ( 4, 4 ),
 ( 0.000000000000000000, 0.004445488388166993383 ),
 .UNSPECIFIED. ) ;
#10594 = VERTEX_POINT ( 'NONE', #17558 ) ;
#10595 = CARTESIAN_POINT ( 'NONE',  ( 4.967162193818130511, 40.93989340068628024, -13.42934394584121094 ) ) ;
#10596 = ORIENTED_EDGE ( 'NONE', *, *, #53503, .T. ) ;
#10597 = CARTESIAN_POINT ( 'NONE',  ( 0.1368894036331262665, 36.62752315710398676, -24.60255826736611340 ) ) ;
#10598 = CARTESIAN_POINT ( 'NONE',  ( 0.9762797500689124330, 36.31338395866826829, -20.92039508843077300 ) ) ;
#10599 = EDGE_CURVE ( 'NONE', #19445, #28616, #53942, .T. ) ;
#10600 = AXIS2_PLACEMENT_3D ( 'NONE', #21436, #25823, #44051 ) ;
#10601 = CARTESIAN_POINT ( 'NONE',  ( 0.8753041380234465318, -42.34096624980154644, -24.86726573039640087 ) ) ;
#10602 = VERTEX_POINT ( 'NONE', #26635 ) ;
#10603 = CARTESIAN_POINT ( 'NONE',  ( 4.549368137175248350, -19.17571786012351254, 38.40568845698243194 ) ) ;
#10604 = EDGE_CURVE ( 'NONE', #49888, #50007, #21634, .T. ) ;
#10605 = CARTESIAN_POINT ( 'NONE',  ( 0.7762777257811892540, 11.53708189756940783, 46.49451973287607132 ) ) ;
#10606 = CARTESIAN_POINT ( 'NONE',  ( -2.601141883200665639, -6.448885681770727629, 13.46132612088575442 ) ) ;
#10607 = VECTOR ( 'NONE', #30253, 1000.000000000000114 ) ;
#10608 = VERTEX_POINT ( 'NONE', #36068 ) ;
#10609 = EDGE_CURVE ( 'NONE', #12769, #17976, #45771, .T. ) ;
#10610 = ORIENTED_EDGE ( 'NONE', *, *, #35583, .F. ) ;
#10611 = CARTESIAN_POINT ( 'NONE',  ( 0.5839880159502333079, 18.28706857028372212, 44.26747004398423257 ) ) ;
#10612 = CARTESIAN_POINT ( 'NONE',  ( 3.238931869106854045, 9.350562014686129686, -41.96286875554259410 ) ) ;
#10613 = CARTESIAN_POINT ( 'NONE',  ( 2.114184763582917181, 7.651710973661706259E-12, 44.03514965515166324 ) ) ;
#10614 = CARTESIAN_POINT ( 'NONE',  ( 5.896782393890504181, -7.234636363571574691, 18.76662259344765715 ) ) ;
#10615 = FACE_OUTER_BOUND ( 'NONE', #16521, .T. ) ;
#10616 = EDGE_LOOP ( 'NONE', ( #45754, #33500, #2973, #32182 ) ) ;
#10617 = EDGE_CURVE ( 'NONE', #31908, #28601, #12253, .T. ) ;
#10618 = CIRCLE ( 'NONE', #8624, 4.000000000000000888 ) ;
#10619 = CARTESIAN_POINT ( 'NONE',  ( 4.967162193818130511, -28.07411493385273715, -32.68434214048198072 ) ) ;
#10620 = ORIENTED_EDGE ( 'NONE', *, *, #20508, .F. ) ;
#10621 = B_SPLINE_CURVE_WITH_KNOTS ( 'NONE', 3,
 ( #4245, #8969, #41576, #47197 ),
 .UNSPECIFIED., .F., .F.,
 ( 4, 4 ),
 ( 0.000000000000000000, 0.004445488388166991649 ),
 .UNSPECIFIED. ) ;
#10622 = CARTESIAN_POINT ( 'NONE',  ( -1.139999999999999902, 6.898680348956876061E-16, 5.633200000000004870 ) ) ;
#10623 = CARTESIAN_POINT ( 'NONE',  ( 4.975610109902397937, 48.43414999183897862, -6.825138951392602849 ) ) ;
#10624 = DIRECTION ( 'NONE',  ( -1.000000000000000000, -0.000000000000000000, -0.000000000000000000 ) ) ;
#10625 = CARTESIAN_POINT ( 'NONE',  ( 0.5998501479064699549, -47.62484632993692912, 6.798102206413326520 ) ) ;
#10626 =( NAMED_UNIT ( * ) SI_UNIT ( $, .STERADIAN. ) SOLID_ANGLE_UNIT ( ) );
#10627 = CARTESIAN_POINT ( 'NONE',  ( 0.6845945791218034371, 31.98229355120833262, 34.31529425661801724 ) ) ;
#10628 = CARTESIAN_POINT ( 'NONE',  ( 0.1135584504625008068, 20.79117989877105899, -38.91887576166853080 ) ) ;
#10629 = CARTESIAN_POINT ( 'NONE',  ( 0.7056555295713284881, 43.92642606846705178, -19.10539864320352521 ) ) ;
#10630 = EDGE_CURVE ( 'NONE', #54620, #57409, #34559, .T. ) ;
#10631 = CARTESIAN_POINT ( 'NONE',  ( 5.896782393890504181, 17.95394716461052909, -9.065421561537322148 ) ) ;
#10632 = CARTESIAN_POINT ( 'NONE',  ( 0.3622758884714600280, 20.83792692158919735, 37.74294673546592804 ) ) ;
#10633 = ADVANCED_FACE ( 'NONE', ( #46084 ), #4769, .T. ) ;
#10634 = CARTESIAN_POINT ( 'NONE',  ( 2.299746137290199499, 3.424328853209327672, -48.91375378757203407 ) ) ;
#10635 = CARTESIAN_POINT ( 'NONE',  ( 4.967162193818129623, -40.65506779172174845, 14.26841313271267886 ) ) ;
#10636 = CARTESIAN_POINT ( 'NONE',  ( 0.8751705887134553219, 41.19904111682508585, -24.81530984069164703 ) ) ;
#10637 = B_SPLINE_CURVE_WITH_KNOTS ( 'NONE', 3,
 ( #35237, #44343, #25817, #39634 ),
 .UNSPECIFIED., .F., .F.,
 ( 4, 4 ),
 ( 4.336808689942017736E-19, 0.004444878191957686922 ),
 .UNSPECIFIED. ) ;
#10638 = ADVANCED_FACE ( 'NONE', ( #55438 ), #28809, .F. ) ;
#10639 = VERTEX_POINT ( 'NONE', #10011 ) ;
#10640 = CARTESIAN_POINT ( 'NONE',  ( 4.967162193818130511, -7.970725651240091025, 42.34252806656591162 ) ) ;
#10641 = CARTESIAN_POINT ( 'NONE',  ( 0.1101816497532062955, 37.41460501058185883, 21.44450189183881861 ) ) ;
#10642 = VECTOR ( 'NONE', #38344, 1000.000000000000114 ) ;
#10643 = CARTESIAN_POINT ( 'NONE',  ( 0.6041374136657475802, 12.28249295041982947, 46.51335992032623068 ) ) ;
#10644 = CARTESIAN_POINT ( 'NONE',  ( 0.5997462898726536595, 22.24958391914565681, -43.77793560195825506 ) ) ;
#10645 = CARTESIAN_POINT ( 'NONE',  ( 0.6845945791218023269, 46.59746449482849329, 5.392849280959315372 ) ) ;
#10646 = AXIS2_PLACEMENT_3D ( 'NONE', #43757, #804, #5483 ) ;
#10647 = VERTEX_POINT ( 'NONE', #29105 ) ;
#10648 = CARTESIAN_POINT ( 'NONE',  ( 4.960156602257182357, -2.524999074837890323, 46.35381625054453281 ) ) ;
#10649 = CARTESIAN_POINT ( 'NONE',  ( 0.9754642270333692133, 16.58255499746128692, -39.57465882553911740 ) ) ;
#10650 = EDGE_CURVE ( 'NONE', #46003, #27817, #61669, .T. ) ;
#10651 = CARTESIAN_POINT ( 'NONE',  ( -99.50001199999974233, 5.000000000000003553, -1.500000000000008216 ) ) ;
#10652 = ORIENTED_EDGE ( 'NONE', *, *, #50482, .T. ) ;
#10653 = CARTESIAN_POINT ( 'NONE',  ( 0.6064515330803530446, -35.25402489989757271, -30.92714122570154345 ) ) ;
#10654 = EDGE_CURVE ( 'NONE', #35248, #31520, #42306, .T. ) ;
#10655 = CARTESIAN_POINT ( 'NONE',  ( 0.9762797500689124330, 25.26481495167912783, -33.43671500974812716 ) ) ;
#10656 = ORIENTED_EDGE ( 'NONE', *, *, #38755, .F. ) ;
#10657 = AXIS2_PLACEMENT_3D ( 'NONE', #7279, #60525, #17638 ) ;
#10658 = CARTESIAN_POINT ( 'NONE',  ( 4.322998006666165516, -14.45630056002971742, 45.75942687572273826 ) ) ;
#10659 = EDGE_LOOP ( 'NONE', ( #45292, #2736, #4613, #16201 ) ) ;
#10660 = CARTESIAN_POINT ( 'NONE',  ( -6.010958268070873523, 17.41463273278788648, -7.197664668556254419 ) ) ;
#10661 = ORIENTED_EDGE ( 'NONE', *, *, #44884, .T. ) ;
#10662 = CARTESIAN_POINT ( 'NONE',  ( 3.783278058412224976, 1.726763838446180976, 43.00370293663099375 ) ) ;
#10663 = CARTESIAN_POINT ( 'NONE',  ( 4.975610109902397937, -48.84566763821283786, 2.559328059280373768 ) ) ;
#10664 = ORIENTED_EDGE ( 'NONE', *, *, #60018, .F. ) ;
#10665 = CARTESIAN_POINT ( 'NONE',  ( 0.7948878604505665857, 3.850400492704748601, -48.94765636212009952 ) ) ;
#10666 = ORIENTED_EDGE ( 'NONE', *, *, #42115, .T. ) ;
#10667 = DIRECTION ( 'NONE',  ( -1.000000000000000000, -0.000000000000000000, -0.000000000000000000 ) ) ;
#10668 = FACE_OUTER_BOUND ( 'NONE', #59726, .T. ) ;
#10669 = ORIENTED_EDGE ( 'NONE', *, *, #21633, .F. ) ;
#10670 = CARTESIAN_POINT ( 'NONE',  ( 2.000000000000027089, 3.464101615137739731, 0.000000000000000000 ) ) ;
#10671 = CARTESIAN_POINT ( 'NONE',  ( 0.8560838555295223751, -30.97734773434455491, -35.22466126774295248 ) ) ;
#10672 = CARTESIAN_POINT ( 'NONE',  ( -6.063463321072276813, 13.84388120595868799, 13.38534294049927631 ) ) ;
#10673 = FACE_OUTER_BOUND ( 'NONE', #9965, .T. ) ;
#10674 = ORIENTED_EDGE ( 'NONE', *, *, #3967, .F. ) ;
#10675 = EDGE_CURVE ( 'NONE', #47799, #37650, #43229, .T. ) ;
#10676 = CARTESIAN_POINT ( 'NONE',  ( 4.975801465491695552, -14.85979367497206205, 45.55012473237727733 ) ) ;
#10677 = CARTESIAN_POINT ( 'NONE',  ( -5.995132425357893702, 16.31525984181046240, -9.429450169547783034 ) ) ;
#10678 = ORIENTED_EDGE ( 'NONE', *, *, #6470, .F. ) ;
#10679 = CARTESIAN_POINT ( 'NONE',  ( 0.5837799406558241699, -46.79736417433153406, -3.041423336563346957 ) ) ;
#10680 = EDGE_CURVE ( 'NONE', #51719, #5333, #32347, .T. ) ;
#10681 = ORIENTED_EDGE ( 'NONE', *, *, #6750, .F. ) ;
#10682 = CARTESIAN_POINT ( 'NONE',  ( 0.9730545539215883499, 33.73144377768594637, -26.52009130076736554 ) ) ;
#10683 = CARTESIAN_POINT ( 'NONE',  ( 2.281448460670576939, 40.87338159040670860, -25.11570011049327533 ) ) ;
#10684 = ORIENTED_EDGE ( 'NONE', *, *, #47986, .F. ) ;
#10685 = CARTESIAN_POINT ( 'NONE',  ( 0.9788927965476027504, -12.55178823826572376, -39.98486244384882582 ) ) ;
#10686 = CARTESIAN_POINT ( 'NONE',  ( -6.078726893082806448, 5.475592473157355755, 18.46109228449450512 ) ) ;
#10687 = CARTESIAN_POINT ( 'NONE',  ( 0.6254087463353913412, -0.6881259009464468779, -48.10157520235525652 ) ) ;
#10688 = CARTESIAN_POINT ( 'NONE',  ( 0.7954196712028467342, 13.28627209367577677, -46.22745629466059825 ) ) ;
#10689 = CIRCLE ( 'NONE', #43708, 48.91267123290010943 ) ;
#10690 = EDGE_CURVE ( 'NONE', #855, #21977, #31867, .T. ) ;
#10691 = EDGE_CURVE ( 'NONE', #26843, #47897, #4671, .T. ) ;
#10692 = PRESENTATION_LAYER_ASSIGNMENT (  '', '', ( #2658 ) ) ;
#10693 = ORIENTED_EDGE ( 'NONE', *, *, #49345, .F. ) ;
#10694 = CARTESIAN_POINT ( 'NONE',  ( 0.1156867017252034419, -40.94616529006326999, 16.44245587842656064 ) ) ;
#10695 = AXIS2_PLACEMENT_3D ( 'NONE', #9803, #37723, #57385 ) ;
#10696 = EDGE_CURVE ( 'NONE', #50538, #29464, #33827, .T. ) ;
#10697 = CARTESIAN_POINT ( 'NONE',  ( 0.6846871229502899947, 41.91507847151797250, 23.20185915381571462 ) ) ;
#10698 = CARTESIAN_POINT ( 'NONE',  ( 0.5797568599927137578, 17.44034498461612159, -43.53228314123417420 ) ) ;
#10699 = B_SPLINE_CURVE_WITH_KNOTS ( 'NONE', 3,
 ( #20728, #31361, #50460, #7527, #26656, #45792 ),
 .UNSPECIFIED., .F., .F.,
 ( 4, 2, 4 ),
 ( 1.188253925084572214E-16, 0.0002448718616795905485, 0.0004897437233590622684 ),
 .UNSPECIFIED. ) ;
#10700 = ADVANCED_FACE ( 'NONE', ( #9684 ), #34334, .F. ) ;
#10701 = FACE_OUTER_BOUND ( 'NONE', #46080, .T. ) ;
#10702 = AXIS2_PLACEMENT_3D ( 'NONE', #4056, #28192, #52296 ) ;
#10703 = CARTESIAN_POINT ( 'NONE',  ( 0.3622758884714730732, 6.444611261694017657, 42.62881903538212924 ) ) ;
#10704 = CARTESIAN_POINT ( 'NONE',  ( 0.5806925824938494740, 46.54710689580857519, 5.708695295225819422 ) ) ;
#10705 = CARTESIAN_POINT ( 'NONE',  ( 3.238018933889920792, -11.82813123897603269, -6.285125596295774386 ) ) ;
#10706 = CARTESIAN_POINT ( 'NONE',  ( -6.016104459813374383, 9.426230926598869075, -16.31603998697559987 ) ) ;
#10707 = CARTESIAN_POINT ( 'NONE',  ( 0.8751705887134423323, -42.09020928323391075, 23.27176129838352736 ) ) ;
#10708 = CARTESIAN_POINT ( 'NONE',  ( 5.910764540655178756, -13.97071922697946533, 14.46790388238978231 ) ) ;
#10709 = VECTOR ( 'NONE', #37218, 1000.000000000000227 ) ;
#10710 = CARTESIAN_POINT ( 'NONE',  ( 5.959547316686252039, 12.49803383497728326, 16.28190225198622443 ) ) ;
#10711 = B_SPLINE_CURVE_WITH_KNOTS ( 'NONE', 3,
 ( #25534, #1708, #39985, #7022, #31472, #26774 ),
 .UNSPECIFIED., .F., .F.,
 ( 4, 2, 4 ),
 ( 1.537985780943912493E-16, 0.0002445252820015181598, 0.0004890505640028825797 ),
 .UNSPECIFIED. ) ;
#10712 =( BOUNDED_SURFACE ( )  B_SPLINE_SURFACE ( 3, 1, ( 
 ( #5498, #31174 ),
 ( #22093, #7344 ),
 ( #21787, #26473 ),
 ( #45000, #2347 ) ),
 .UNSPECIFIED., .F., .F., .F. ) 
 B_SPLINE_SURFACE_WITH_KNOTS ( ( 4, 4 ),
 ( 2, 2 ),
 ( 0.000000000000000000, 1.000000000000000000 ),
 ( 0.000000000000000000, 1.000000000000000000 ),
 .UNSPECIFIED. ) 
 GEOMETRIC_REPRESENTATION_ITEM ( )  RATIONAL_B_SPLINE_SURFACE ( (
 ( 1.000000000000000000, 1.000000000000000000),
 ( 0.9751682680413298332, 0.9999560080971552356),
 ( 0.9751682680413298332, 0.9999560080971552356),
 ( 1.000000000000000000, 1.000000000000000000) ) ) 
 REPRESENTATION_ITEM ( '' )  SURFACE ( )  );
#10713 = B_SPLINE_CURVE_WITH_KNOTS ( 'NONE', 3,
 ( #664, #20718, #16026, #30405, #57978, #29796 ),
 .UNSPECIFIED., .F., .F.,
 ( 4, 2, 4 ),
 ( 1.258037581941437391E-16, 0.0002450741128632354863, 0.0004901482257263450968 ),
 .UNSPECIFIED. ) ;
#10714 = CARTESIAN_POINT ( 'NONE',  ( 0.5839880159502339740, 33.83547574026627558, 33.89965136132159529 ) ) ;
#10715 = CARTESIAN_POINT ( 'NONE',  ( 4.960386119450144626, -43.75174247978073083, 0.4706321868415035969 ) ) ;
#10716 = ORIENTED_EDGE ( 'NONE', *, *, #56353, .F. ) ;
#10717 = CARTESIAN_POINT ( 'NONE',  ( 0.8744876279028263033, -43.20725972823498040, 23.31271664041618052 ) ) ;
#10718 = CARTESIAN_POINT ( 'NONE',  ( 1.479689385636123067, 19.33154860216732018, -39.59640228492652625 ) ) ;
#10719 = CARTESIAN_POINT ( 'NONE',  ( 1.231276596079887931, 5.037240371905710390, 41.61613846158375196 ) ) ;
#10720 = EDGE_LOOP ( 'NONE', ( #39977, #38541, #61337, #42509, #15156 ) ) ;
#10721 = CARTESIAN_POINT ( 'NONE',  ( 0.7948884756798504370, -14.79943981595577185, 46.81533109713159035 ) ) ;
#10722 = CARTESIAN_POINT ( 'NONE',  ( 0.9762797500689124330, 33.20096159360316790, 25.57383300261796677 ) ) ;
#10723 =( BOUNDED_SURFACE ( )  B_SPLINE_SURFACE ( 3, 1, ( 
 ( #36180, #55245 ),
 ( #31458, #7634 ),
 ( #22069, #37734 ),
 ( #384, #47726 ) ),
 .UNSPECIFIED., .F., .F., .F. ) 
 B_SPLINE_SURFACE_WITH_KNOTS ( ( 4, 4 ),
 ( 2, 2 ),
 ( 0.000000000000000000, 1.000000000000000000 ),
 ( 0.000000000000000000, 1.000000000000000000 ),
 .UNSPECIFIED. ) 
 GEOMETRIC_REPRESENTATION_ITEM ( )  RATIONAL_B_SPLINE_SURFACE ( (
 ( 1.000000000000000000, 1.000000000000000000),
 ( 0.9953485035131437453, 0.8621029689291523912),
 ( 0.9953485035131437453, 0.8621029689291523912),
 ( 1.000000000000000000, 1.000000000000000000) ) ) 
 REPRESENTATION_ITEM ( '' )  SURFACE ( )  );
#10724 = ORIENTED_EDGE ( 'NONE', *, *, #44713, .T. ) ;
#10725 = ORIENTED_EDGE ( 'NONE', *, *, #46027, .T. ) ;
#10726 = EDGE_CURVE ( 'NONE', #39562, #20774, #13722, .T. ) ;
#10727 = DIRECTION ( 'NONE',  ( 0.9990097760809872884, 5.448601141172737927E-18, 0.04449120468829269315 ) ) ;
#10728 = AXIS2_PLACEMENT_3D ( 'NONE', #5847, #58472, #15601 ) ;
#10729 = VERTEX_POINT ( 'NONE', #4341 ) ;
#10730 = MECHANICAL_DESIGN_GEOMETRIC_PRESENTATION_REPRESENTATION (  '', ( #21724 ), #35749 ) ;
#10731 = CARTESIAN_POINT ( 'NONE',  ( 1.154321485836934391, 25.46626718279358315, -34.54400167111872832 ) ) ;
#10732 = VECTOR ( 'NONE', #1467, 1000.000000000000000 ) ;
#10733 = ORIENTED_EDGE ( 'NONE', *, *, #14261, .F. ) ;
#10734 = EDGE_LOOP ( 'NONE', ( #5374, #25052, #14817, #8940 ) ) ;
#10735 = CARTESIAN_POINT ( 'NONE',  ( 0.1102144999581332746, 11.03964818279716020, 41.68747259405353844 ) ) ;
#10736 = ORIENTED_EDGE ( 'NONE', *, *, #25764, .T. ) ;
#10737 = CARTESIAN_POINT ( 'NONE',  ( 0.8560838555295158248, 27.08392101972004440, 38.29926965725714894 ) ) ;
#10738 = CARTESIAN_POINT ( 'NONE',  ( 0.8751705887134553219, -23.27176129838455054, 42.09020928323333521 ) ) ;
#10739 = VERTEX_POINT ( 'NONE', #51666 ) ;
#10740 = CARTESIAN_POINT ( 'NONE',  ( 0.5806925824938499181, 45.08220210717423271, 12.91578164539256335 ) ) ;
#10741 = CARTESIAN_POINT ( 'NONE',  ( -6.016489644550737204, 2.463898142943031555, -18.68142234211821773 ) ) ;
#10742 = EDGE_LOOP ( 'NONE', ( #37385, #58414, #55327, #45865 ) ) ;
#10743 = AXIS2_PLACEMENT_3D ( 'NONE', #1840, #30350, #40111 ) ;
#10744 = ORIENTED_EDGE ( 'NONE', *, *, #1898, .T. ) ;
#10745 = CARTESIAN_POINT ( 'NONE',  ( 0.6009452777970412107, -18.00606236585402087, 44.61081509289873281 ) ) ;
#10746 = B_SPLINE_CURVE_WITH_KNOTS ( 'NONE', 3,
 ( #3739, #27262, #17875, #51357, #41089, #54824 ),
 .UNSPECIFIED., .F., .F.,
 ( 4, 2, 4 ),
 ( 7.006328859705253345E-18, 0.0002291472222819939113, 0.0004582944445639808295 ),
 .UNSPECIFIED. ) ;
#10747 = CARTESIAN_POINT ( 'NONE',  ( 0.1064266379913940963, 41.50637574965949028, -11.70292640078110935 ) ) ;
#10748 = CARTESIAN_POINT ( 'NONE',  ( 0.1073791018717578927, -30.83464511437158961, 30.14884492832337060 ) ) ;
#10749 = CARTESIAN_POINT ( 'NONE',  ( 0.9780106845699492180, 35.89738679733209636, 21.62657780551894859 ) ) ;
#10750 = ORIENTED_EDGE ( 'NONE', *, *, #58268, .F. ) ;
#10751 = CARTESIAN_POINT ( 'NONE',  ( 0.9730545539215883499, -25.71816799638755668, -34.34678117142582465 ) ) ;
#10752 = CARTESIAN_POINT ( 'NONE',  ( 0.5980271706414711508, -45.78139539622871013, 17.77956912908273068 ) ) ;
#10753 = EDGE_CURVE ( 'NONE', #10364, #42072, #15928, .T. ) ;
#10754 = CARTESIAN_POINT ( 'NONE',  ( -2.601141883200662974, -13.99736252863761798, -5.183557630747456457 ) ) ;
#10755 = B_SPLINE_CURVE_WITH_KNOTS ( 'NONE', 3,
 ( #48409, #14608, #42811, #58095 ),
 .UNSPECIFIED., .F., .F.,
 ( 4, 4 ),
 ( 0.000000000000000000, 0.005004741218457407596 ),
 .UNSPECIFIED. ) ;
#10756 = CARTESIAN_POINT ( 'NONE',  ( 0.6039202388192953519, -25.60584472520843491, -41.90351332236362936 ) ) ;
#10757 = ORIENTED_EDGE ( 'NONE', *, *, #13296, .F. ) ;
#10758 = CARTESIAN_POINT ( 'NONE',  ( 4.967162193818130511, 42.96271701169385437, 3.259922920617894793 ) ) ;
#10759 = CARTESIAN_POINT ( 'NONE',  ( 4.963659409799330291, -33.96111158240226757, -29.14784479683147467 ) ) ;
#10760 = EDGE_CURVE ( 'NONE', #16502, #22341, #13796, .T. ) ;
#10761 = CARTESIAN_POINT ( 'NONE',  ( -6.063463321072278589, 11.99415941893228421, 15.06521132652004979 ) ) ;
#10762 = CARTESIAN_POINT ( 'NONE',  ( 0.6027444965799114707, -35.18529211318709571, -34.25687864936231364 ) ) ;
#10763 = CONICAL_SURFACE ( 'NONE', #38913, 43.92652462719577500, 1.486293639869522343 ) ;
#10764 = EDGE_CURVE ( 'NONE', #17692, #21442, #9140, .T. ) ;
#10765 = ORIENTED_EDGE ( 'NONE', *, *, #4640, .F. ) ;
#10766 = ORIENTED_EDGE ( 'NONE', *, *, #49050, .F. ) ;
#10767 = DIRECTION ( 'NONE',  ( 1.000000000000000000, 1.836970198721027962E-16, -2.033782021272921061E-31 ) ) ;
#10768 = EDGE_CURVE ( 'NONE', #3462, #29292, #42879, .T. ) ;
#10769 = CARTESIAN_POINT ( 'NONE',  ( -6.016489644550736315, 13.32104266208117771, -13.32727118274423894 ) ) ;
#10770 = CARTESIAN_POINT ( 'NONE',  ( 0.1102144999581332746, -39.88986724628646385, 16.38650952318839060 ) ) ;
#10771 = CARTESIAN_POINT ( 'NONE',  ( -2.601141883200662974, -0.03040527887401129128, 14.92630238834806811 ) ) ;
#10772 = CARTESIAN_POINT ( 'NONE',  ( 0.1100247026804066219, 34.31594964380183654, -26.11768802553209312 ) ) ;
#10773 = CARTESIAN_POINT ( 'NONE',  ( 0.1129192098497455998, -32.03190746135001632, 30.34647742609778831 ) ) ;
#10774 = CARTESIAN_POINT ( 'NONE',  ( 100.0000507999999968, 0.000000000000000000, 0.000000000000000000 ) ) ;
#10775 = CARTESIAN_POINT ( 'NONE',  ( 3.680974057930773924, 27.71659654258243322, 39.15945827951719593 ) ) ;
#10776 = CARTESIAN_POINT ( 'NONE',  ( 0.5848930533535030563, -30.13830825645479550, -35.92986860296690566 ) ) ;
#10777 = CARTESIAN_POINT ( 'NONE',  ( 0.1097557419366048670, 30.33543403792237925, -30.65094619415035737 ) ) ;
#10778 = CARTESIAN_POINT ( 'NONE',  ( 0.6017667736363750963, -6.625250263233982473, 47.64919355032676407 ) ) ;
#10779 = EDGE_CURVE ( 'NONE', #24396, #46146, #1819, .T. ) ;
#10780 = VECTOR ( 'NONE', #33497, 1000.000000000000000 ) ;
#10781 = CARTESIAN_POINT ( 'NONE',  ( 0.1157991065609916270, -6.961833292486440783, -43.57149575978917966 ) ) ;
#10782 = CARTESIAN_POINT ( 'NONE',  ( 5.838029081930957709, 38.95312035650108839, 26.71552867986823188 ) ) ;
#10784 = ADVANCED_FACE ( 'NONE', ( #5884 ), #5023, .F. ) ;
#10783 = CARTESIAN_POINT ( 'NONE',  ( 0.1156495703730067715, -35.28001429893448915, 26.50025555156116397 ) ) ;
#10785 = CARTESIAN_POINT ( 'NONE',  ( 1.231276596079881047, -11.60895935156387537, -40.28037777618035875 ) ) ;
#10786 = CARTESIAN_POINT ( 'NONE',  ( 0.6023142530420679819, -23.82662387835896212, 41.79260242564358663 ) ) ;
#10787 = CARTESIAN_POINT ( 'NONE',  ( 0.6029443449137436017, 33.04717288230519046, -36.32387510261487762 ) ) ;
#10788 = CONTEXT_DEPENDENT_SHAPE_REPRESENTATION ( #32796, #52848 ) ;
#10789 = CARTESIAN_POINT ( 'NONE',  ( 4.691466044806102076, -43.66525414675636085, -9.025781474741316757 ) ) ;
#10790 = CARTESIAN_POINT ( 'NONE',  ( 0.9754642270333685472, -11.27515941577604153, 41.40054989430078081 ) ) ;
#10791 = CARTESIAN_POINT ( 'NONE',  ( 1.231276596079887264, -26.41281459480383376, 32.55211200826430229 ) ) ;
#10792 = CARTESIAN_POINT ( 'NONE',  ( 0.8551540677456715978, -24.74404575822747177, -41.03346287276453097 ) ) ;
#10794 = ORIENTED_EDGE ( 'NONE', *, *, #50904, .F. ) ;
#10793 = FACE_OUTER_BOUND ( 'NONE', #36130, .T. ) ;
#10795 = EDGE_LOOP ( 'NONE', ( #36952, #48411, #50322, #54102 ) ) ;
#10796 = CARTESIAN_POINT ( 'NONE',  ( 0.9754292580325135686, 36.35155301108883208, -20.85406580468192672 ) ) ;
#10797 = CARTESIAN_POINT ( 'NONE',  ( 0.6254087463353920073, -48.10157520235525652, 0.6881259009466142995 ) ) ;
#10798 = LINE ( 'NONE', #49000, #53736 ) ;
#10799 = ORIENTED_EDGE ( 'NONE', *, *, #42104, .F. ) ;
#10800 = ORIENTED_EDGE ( 'NONE', *, *, #25666, .T. ) ;
#10801 = FACE_OUTER_BOUND ( 'NONE', #28315, .T. ) ;
#10802 = PLANE ( 'NONE',  #13161 ) ;
#10803 = CARTESIAN_POINT ( 'NONE',  ( 0.5839254288179566155, -41.43367229384567452, -24.02657516616548605 ) ) ;
#10804 = VECTOR ( 'NONE', #14706, 1000.000000000000114 ) ;
#10805 = EDGE_LOOP ( 'NONE', ( #29708, #60667, #637, #27147 ) ) ;
#10806 = ORIENTED_EDGE ( 'NONE', *, *, #56988, .T. ) ;
#10807 = EDGE_CURVE ( 'NONE', #940, #19546, #39135, .T. ) ;
#10808 = DIRECTION ( 'NONE',  ( 1.000000000000000000, 0.000000000000000000, 0.000000000000000000 ) ) ;
#10809 = CONICAL_SURFACE ( 'NONE', #13811, 42.92674063221959813, 1.485477209440487556 ) ;
#10810 =( BOUNDED_SURFACE ( )  B_SPLINE_SURFACE ( 3, 1, ( 
 ( #16669, #7873 ),
 ( #7550, #60181 ),
 ( #32007, #27293 ),
 ( #40496, #17291 ) ),
 .UNSPECIFIED., .F., .F., .F. ) 
 B_SPLINE_SURFACE_WITH_KNOTS ( ( 4, 4 ),
 ( 2, 2 ),
 ( 0.000000000000000000, 1.000000000000000000 ),
 ( 0.000000000000000000, 1.000000000000000000 ),
 .UNSPECIFIED. ) 
 GEOMETRIC_REPRESENTATION_ITEM ( )  RATIONAL_B_SPLINE_SURFACE ( (
 ( 1.000000000000000000, 1.000000000000000000),
 ( 0.9953485035131437453, 0.8621029689291523912),
 ( 0.9953485035131437453, 0.8621029689291523912),
 ( 1.000000000000000000, 1.000000000000000000) ) ) 
 REPRESENTATION_ITEM ( '' )  SURFACE ( )  );
#10811 = CARTESIAN_POINT ( 'NONE',  ( -6.077587904424778920, -17.35179747939691808, -8.349320069797613542 ) ) ;
#10812 = CARTESIAN_POINT ( 'NONE',  ( 1.088908134280555551, -11.85879120571477863, -41.24246781061831513 ) ) ;
#10813 = CARTESIAN_POINT ( 'NONE',  ( 1.296416391601052487, -11.47028222229313599, 42.55279074064478806 ) ) ;
#10814 = CARTESIAN_POINT ( 'NONE',  ( 0.9789889208857707192, -41.08791942546226750, -8.253349340061184591 ) ) ;
#10815 = CARTESIAN_POINT ( 'NONE',  ( 0.8744876279028263033, 43.84003649649913115, 22.09980204357308153 ) ) ;
#10816 = CARTESIAN_POINT ( 'NONE',  ( -6.016761891674564211, -7.207804629151436160, 17.41015286184800459 ) ) ;
#10817 = ORIENTED_EDGE ( 'NONE', *, *, #25967, .T. ) ;
#10818 = EDGE_LOOP ( 'NONE', ( #51112, #40632, #61833, #58866 ) ) ;
#10819 = CARTESIAN_POINT ( 'NONE',  ( 2.528190830796655852, 36.72068932201717928, -20.34318342514028899 ) ) ;
#10820 = CARTESIAN_POINT ( 'NONE',  ( -6.001507490154111224, 9.435425682281048054, -16.31148204059937257 ) ) ;
#10821 = AXIS2_PLACEMENT_3D ( 'NONE', #50139, #8142, #21631 ) ;
#10822 = ORIENTED_EDGE ( 'NONE', *, *, #50360, .F. ) ;
#10823 = CARTESIAN_POINT ( 'NONE',  ( 0.5809828226811617480, 44.45562576850627323, -17.82437196699632054 ) ) ;
#10824 = CYLINDRICAL_SURFACE ( 'NONE', #48633, 5.000000000000000000 ) ;
#10825 = FACE_OUTER_BOUND ( 'NONE', #40119, .T. ) ;
#10826 = CARTESIAN_POINT ( 'NONE',  ( 0.8554163680231720024, -8.703479761964910466, -46.10265624825630937 ) ) ;
#10827 = ORIENTED_EDGE ( 'NONE', *, *, #41553, .F. ) ;
#10828 = CARTESIAN_POINT ( 'NONE',  ( 0.9756354156337441186, -42.52418499698895005, -5.729847988735796704 ) ) ;
#10829 = B_SPLINE_CURVE_WITH_KNOTS ( 'NONE', 3,
 ( #46674, #36660, #55729, #22853, #41988, #45448 ),
 .UNSPECIFIED., .F., .F.,
 ( 4, 2, 4 ),
 ( 0.000000000000000000, 0.0002447195606305742040, 0.0004894391212611484080 ),
 .UNSPECIFIED. ) ;
#10830 = CARTESIAN_POINT ( 'NONE',  ( 0.1104177457020372732, -37.34931850022154975, -21.55798761925374407 ) ) ;
#10831 = SHAPE_REPRESENTATION ( 'needle roller bearing_nh_iso_ISO 3245 - 2521D - 24,SI,NC,24', ( #14677 ), #31864 ) ;
#10832 = CARTESIAN_POINT ( 'NONE',  ( 0.5809828226811553087, -44.45562576850588243, -17.82437196699728332 ) ) ;
#10833 = ORIENTED_EDGE ( 'NONE', *, *, #6750, .T. ) ;
#10834 = CARTESIAN_POINT ( 'NONE',  ( 0.1119899015040014545, 42.04997222364495713, -13.37015871944657341 ) ) ;
#10835 = ADVANCED_FACE ( 'NONE', ( #2120 ), #47143, .F. ) ;
#10836 = CARTESIAN_POINT ( 'NONE',  ( 0.1119899015040012741, -43.68681032745429604, -6.198702413048826187 ) ) ;
#10837 = VERTEX_POINT ( 'NONE', #34136 ) ;
#10838 = CARTESIAN_POINT ( 'NONE',  ( 0.6845945791218034371, 23.29905063694718592, -40.71315217630433381 ) ) ;
#10839 = CARTESIAN_POINT ( 'NONE',  ( 4.549368137175248350, 13.99871866169305434, 40.58005590356696501 ) ) ;
#10840 = AXIS2_PLACEMENT_3D ( 'NONE', #21247, #45382, #35675 ) ;
#10841 = VERTEX_POINT ( 'NONE', #54429 ) ;
#10842 = CARTESIAN_POINT ( 'NONE',  ( 0.7954190325252784577, -5.415566973723597854, 47.79303692714232454 ) ) ;
#10843 = ADVANCED_FACE ( 'NONE', ( #15949 ), #36721, .F. ) ;
#10844 = CARTESIAN_POINT ( 'NONE',  ( 0.5804410086790514622, 27.37779091616946658, 38.07855586029891271 ) ) ;
#10845 = DIRECTION ( 'NONE',  ( 0.1305261922200498526, 0.9914448613738106042, -0.000000000000000000 ) ) ;
#10846 = CARTESIAN_POINT ( 'NONE',  ( 4.834790513006553603, -32.10612123254752959, 34.66678987626835351 ) ) ;
#10847 = CARTESIAN_POINT ( 'NONE',  ( 0.8744876279028306332, 28.81338721758086052, 39.75095932715638014 ) ) ;
#10849 = CARTESIAN_POINT ( 'NONE',  ( 0.1129192098497447394, -31.35755906439637641, 31.04279751098549056 ) ) ;
#10848 = COLOUR_RGB ( '', 0.72549020, 0.75294118, 0.79215686) ;
#10850 = CARTESIAN_POINT ( 'NONE',  ( 4.694002226626921015, -45.51532087759711942, 2.576885107160884925 ) ) ;
#10851 = CARTESIAN_POINT ( 'NONE',  ( 1.399999999999999467, 6.245698675651501825E-16, 5.100000000000000533 ) ) ;
#10852 = VERTEX_POINT ( 'NONE', #54118 ) ;
#10853 = CARTESIAN_POINT ( 'NONE',  ( 0.9756354156337460060, 39.69194847698950923, -16.29989858042583961 ) ) ;
#10854 =( GEOMETRIC_REPRESENTATION_CONTEXT ( 3 ) GLOBAL_UNCERTAINTY_ASSIGNED_CONTEXT ( ( #41794 ) ) GLOBAL_UNIT_ASSIGNED_CONTEXT ( ( #42001, #22870, #60438 ) ) REPRESENTATION_CONTEXT ( 'NONE', 'WORKASPACE' ) );
#10855 = CARTESIAN_POINT ( 'NONE',  ( 2.500000000000000000, -2.357898499370432166, 3.035766082959412415E-15 ) ) ;
#10856 = CARTESIAN_POINT ( 'NONE',  ( 0.5824935313925935221, 27.52368752571334554, -37.96952464860119392 ) ) ;
#10857 = ORIENTED_EDGE ( 'NONE', *, *, #45093, .F. ) ;
#10859 = MANIFOLD_SOLID_BREP ( 'InnerRace', #36069 ) ;
#10858 = CARTESIAN_POINT ( 'NONE',  ( 4.967162193818130511, 42.34252806656594004, 7.970725651239941811 ) ) ;
#10860 = CARTESIAN_POINT ( 'NONE',  ( -6.078726893082806448, -14.66462719274117887, 12.47969352855413838 ) ) ;
#10862 = EDGE_CURVE ( 'NONE', #1919, #25747, #46913, .T. ) ;
#10861 = CARTESIAN_POINT ( 'NONE',  ( -6.077587904424778920, -14.66646125808240164, -12.47761738310237334 ) ) ;
#10863 = FACE_OUTER_BOUND ( 'NONE', #54293, .T. ) ;
#10864 = FACE_OUTER_BOUND ( 'NONE', #48406, .T. ) ;
#10865 = B_SPLINE_CURVE_WITH_KNOTS ( 'NONE', 3,
 ( #60891, #17380, #32410, #32720, #37426, #36499 ),
 .UNSPECIFIED., .F., .F.,
 ( 4, 2, 4 ),
 ( 0.000000000000000000, 0.0002293801035737106188, 0.0004587602071474212377 ),
 .UNSPECIFIED. ) ;
#10866 = CARTESIAN_POINT ( 'NONE',  ( 2.282816707992315841, -15.16645052872554977, -44.45757241199396503 ) ) ;
#10867 = CARTESIAN_POINT ( 'NONE',  ( 4.960386119450137521, 36.33710775634285284, 24.37316279386549667 ) ) ;
#10868 = CARTESIAN_POINT ( 'NONE',  ( 1.088313998177380615, 29.78798111128829262, 30.89087247895941601 ) ) ;
#10869 = CIRCLE ( 'NONE', #833, 48.09070567114147110 ) ;
#10870 = CARTESIAN_POINT ( 'NONE',  ( 0.2885697896453108813, -6.424755442172918940, 42.63514065501003358 ) ) ;
#10872 = ORIENTED_EDGE ( 'NONE', *, *, #50835, .F. ) ;
#10871 = CARTESIAN_POINT ( 'NONE',  ( 0.5806925824938502512, -29.85799195566318431, 36.16244846134061675 ) ) ;
#10873 = ORIENTED_EDGE ( 'NONE', *, *, #29769, .F. ) ;
#10874 = CARTESIAN_POINT ( 'NONE',  ( 0.8751705887134553219, -44.08562551107095828, 19.22545746485582185 ) ) ;
#10875 = CONICAL_SURFACE ( 'NONE', #23870, 43.92652462719577500, 1.486293639869522343 ) ;
#10876 = CARTESIAN_POINT ( 'NONE',  ( 2.624215991343620935, -47.76052319582213812, -4.864192649745882946 ) ) ;
#10877 = CARTESIAN_POINT ( 'NONE',  ( 0.5848930533535030563, 22.37766167358117286, -41.21302391732853465 ) ) ;
#10878 = PRODUCT_DEFINITION_SHAPE ( 'NONE', 'NONE',  #61987 ) ;
#10879 = CARTESIAN_POINT ( 'NONE',  ( 0.8560838555295158248, -46.14148336882297485, 8.446084690930096173 ) ) ;
#10880 = CARTESIAN_POINT ( 'NONE',  ( 5.917102823773431552, 14.91028373222408732, -13.49715366572951858 ) ) ;
#10881 = CARTESIAN_POINT ( 'NONE',  ( 5.894904586330512508, -11.92958617826559653, 16.19303509775042471 ) ) ;
#10882 = VERTEX_POINT ( 'NONE', #41016 ) ;
#10883 = ORIENTED_EDGE ( 'NONE', *, *, #35781, .F. ) ;
#10884 = EDGE_CURVE ( 'NONE', #47641, #32860, #30726, .T. ) ;
#10885 = FACE_OUTER_BOUND ( 'NONE', #26475, .T. ) ;
#10886 = B_SPLINE_CURVE_WITH_KNOTS ( 'NONE', 3,
 ( #49633, #1088, #20833, #43743 ),
 .UNSPECIFIED., .F., .F.,
 ( 4, 4 ),
 ( 0.000000000000000000, 0.005014147105413700387 ),
 .UNSPECIFIED. ) ;
#10887 = VECTOR ( 'NONE', #31731, 1000.000000000000114 ) ;
#10888 = CARTESIAN_POINT ( 'NONE',  ( 0.6000166863083090663, 28.52380356231424940, -39.97769518177558012 ) ) ;
#10889 = CARTESIAN_POINT ( 'NONE',  ( 4.549368137175248350, -8.582197505784725067, 42.06008734272381133 ) ) ;
#10890 = ORIENTED_EDGE ( 'NONE', *, *, #41797, .T. ) ;
#10891 = CARTESIAN_POINT ( 'NONE',  ( 0.9762797500689124330, -27.44172181261391330, -31.67454323498310842 ) ) ;
#10892 = CARTESIAN_POINT ( 'NONE',  ( 0.6254087463353908971, -11.78492518233843001, 46.64065386173393790 ) ) ;
#10893 = ORIENTED_EDGE ( 'NONE', *, *, #8917, .F. ) ;
#10894 = PRODUCT_DEFINITION_FORMATION_WITH_SPECIFIED_SOURCE ( 'ANY', '', #54756, .NOT_KNOWN. ) ;
#10895 = FACE_OUTER_BOUND ( 'NONE', #24126, .T. ) ;
#10896 = ORIENTED_EDGE ( 'NONE', *, *, #44239, .T. ) ;
#10897 = CARTESIAN_POINT ( 'NONE',  ( 0.5806925824938499181, -35.14454992382352572, 31.04968555388990836 ) ) ;
#10898 = CARTESIAN_POINT ( 'NONE',  ( 4.303969348037258058, -45.86537346639067891, 14.52400616872353289 ) ) ;
#10899 = VERTEX_POINT ( 'NONE', #46018 ) ;
#10900 = CARTESIAN_POINT ( 'NONE',  ( 0.7056555295713264897, -41.89804573586717140, -23.21854706865624962 ) ) ;
#10901 = CARTESIAN_POINT ( 'NONE',  ( -6.079354080745853928, -18.27463532918889300, -6.068826808644588233 ) ) ;
#10902 = CARTESIAN_POINT ( 'NONE',  ( 0.9762797500689124330, 40.28286501695569655, 11.55922018180428168 ) ) ;
#10903 = CARTESIAN_POINT ( 'NONE',  ( -6.079354080745853928, -1.850179728782415545, -19.16689307684906751 ) ) ;
#10904 = B_SPLINE_CURVE_WITH_KNOTS ( 'NONE', 3,
 ( #50929, #2386, #25907, #8025, #21825, #35943 ),
 .UNSPECIFIED., .F., .F.,
 ( 4, 2, 4 ),
 ( 2.114194236346733646E-18, 0.0002293801035737086944, 0.0004587602071474152746 ),
 .UNSPECIFIED. ) ;
#10905 = ORIENTED_EDGE ( 'NONE', *, *, #2477, .F. ) ;
#10906 = CARTESIAN_POINT ( 'NONE',  ( 4.956445790444004018, -46.59545590650535019, -6.811867512257778756 ) ) ;
#10907 = CARTESIAN_POINT ( 'NONE',  ( 2.299652685299201416, -45.91772179304631152, 17.20013227258888477 ) ) ;
#10908 = ORIENTED_EDGE ( 'NONE', *, *, #17560, .F. ) ;
#10909 = CARTESIAN_POINT ( 'NONE',  ( -5.331200000000000827, 0.000000000000000000, 12.55882000000000076 ) ) ;
#10910 =( BOUNDED_SURFACE ( )  B_SPLINE_SURFACE ( 3, 1, ( 
 ( #35286, #59366 ),
 ( #30249, #50287 ),
 ( #7353, #1422 ),
 ( #31181, #40311 ) ),
 .UNSPECIFIED., .F., .F., .F. ) 
 B_SPLINE_SURFACE_WITH_KNOTS ( ( 4, 4 ),
 ( 2, 2 ),
 ( 0.000000000000000000, 1.000000000000000000 ),
 ( 0.000000000000000000, 1.000000000000000000 ),
 .UNSPECIFIED. ) 
 GEOMETRIC_REPRESENTATION_ITEM ( )  RATIONAL_B_SPLINE_SURFACE ( (
 ( 1.000000000000000000, 1.000000000000000000),
 ( 0.9953485035131437453, 0.8621029689291515030),
 ( 0.9953485035131437453, 0.8621029689291515030),
 ( 1.000000000000000000, 1.000000000000000000) ) ) 
 REPRESENTATION_ITEM ( '' )  SURFACE ( )  );
#10911 = ORIENTED_EDGE ( 'NONE', *, *, #58973, .F. ) ;
#10912 = CARTESIAN_POINT ( 'NONE',  ( 1.157643937452370153, -39.86048667108141075, -12.96703038244662842 ) ) ;
#10913 = ADVANCED_FACE ( 'NONE', ( #31579 ), #4646, .F. ) ;
#10914 = ORIENTED_EDGE ( 'NONE', *, *, #49430, .T. ) ;
#10915 = CARTESIAN_POINT ( 'NONE',  ( 0.1119898979215350199, 36.67093969866893133, -24.53983475633885547 ) ) ;
#10916 = CARTESIAN_POINT ( 'NONE',  ( 0.8744876279028263033, 40.65405044375290800, 27.52450240960382644 ) ) ;
#10917 = CIRCLE ( 'NONE', #3855, 7.500000000000022204 ) ;
#10918 = AXIS2_PLACEMENT_3D ( 'NONE', #5559, #58488, #24697 ) ;
#10919 = CARTESIAN_POINT ( 'NONE',  ( 0.8557997880470599172, 41.02602466100778145, 24.73961900479265807 ) ) ;
#10920 = ORIENTED_EDGE ( 'NONE', *, *, #56201, .F. ) ;
#10921 = CARTESIAN_POINT ( 'NONE',  ( -6.017396004339686577, 7.209881890566790297, -17.40926186480771776 ) ) ;
#10922 = EDGE_CURVE ( 'NONE', #36895, #40762, #43561, .T. ) ;
#10923 = CARTESIAN_POINT ( 'NONE',  ( 0.5839879327111947571, -6.161619650335635079, 47.49806740880203648 ) ) ;
#10924 = CARTESIAN_POINT ( 'NONE',  ( 4.694002226626920127, -38.01786027345654162, 25.15804188870963287 ) ) ;
#10925 = ORIENTED_EDGE ( 'NONE', *, *, #3684, .F. ) ;
#10926 = EDGE_CURVE ( 'NONE', #55315, #45625, #42788, .T. ) ;
#10927 = ORIENTED_EDGE ( 'NONE', *, *, #1687, .T. ) ;
#10928 = CARTESIAN_POINT ( 'NONE',  ( 0.5997462898726536595, -45.31995669577334240, -18.91172004968183984 ) ) ;
#10929 = FACE_OUTER_BOUND ( 'NONE', #9355, .T. ) ;
#10930 = CARTESIAN_POINT ( 'NONE',  ( 4.975801465491694664, 40.15204426031534268, -26.14269827151636605 ) ) ;
#10931 = LINE ( 'NONE', #44161, #44968 ) ;
#10932 = CARTESIAN_POINT ( 'NONE',  ( 0.1310142868023667639, 30.03916697317172790, 30.94009702668483186 ) ) ;
#10933 = AXIS2_PLACEMENT_3D ( 'NONE', #15620, #39438, #58490 ) ;
#10934 = ORIENTED_EDGE ( 'NONE', *, *, #36805, .T. ) ;
#10935 = PLANE ( 'NONE',  #20703 ) ;
#10936 = CIRCLE ( 'NONE', #12905, 47.91270532121795611 ) ;
#10937 = ORIENTED_EDGE ( 'NONE', *, *, #38356, .T. ) ;
#10938 = B_SPLINE_CURVE_WITH_KNOTS ( 'NONE', 3,
 ( #59360, #2655, #41221, #31485, #35594, #40923, #50280, #26788, #17096, #50894, #21470, #59671, #17704, #7659, #3265, #54966 ),
 .UNSPECIFIED., .F., .F.,
 ( 4, 3, 3, 3, 3, 4 ),
 ( 2.221635811791082109E-17, 0.0002612764279487775538, 0.0003919131003184807630, 0.0005225497727000644969, 0.0007837925190632461132, 0.001045051706266715433 ),
 .UNSPECIFIED. ) ;
#10939 = CARTESIAN_POINT ( 'NONE',  ( 4.960156602257182357, -46.28683144126597426, 3.546989772329730339 ) ) ;
#10941 = EDGE_CURVE ( 'NONE', #60001, #8147, #927, .T. ) ;
#10940 = CARTESIAN_POINT ( 'NONE',  ( 0.5782707292762442330, -0.8434722838399307809, -46.89376193284147831 ) ) ;
#10942 = CARTESIAN_POINT ( 'NONE',  ( 0.5835226383429302777, -41.93746949518194356, -20.98788047628082509 ) ) ;
#10943 = CARTESIAN_POINT ( 'NONE',  ( 5.958863334805807099, -18.96369761673824783, 7.853699934219561918 ) ) ;
#10944 = CARTESIAN_POINT ( 'NONE',  ( 3.050102900204245682, 11.54593035058338124, 42.45134557958719768 ) ) ;
#10945 = CARTESIAN_POINT ( 'NONE',  ( 4.549368137175248350, -18.79584381673505789, -38.59302160394747006 ) ) ;
#10946 = CARTESIAN_POINT ( 'NONE',  ( 0.9740398440564311811, -39.48175649279244226, 16.80263250099874028 ) ) ;
#10947 = CARTESIAN_POINT ( 'NONE',  ( 0.8760168074886965917, 44.77533136581881479, -17.58183840866353265 ) ) ;
#10948 = CARTESIAN_POINT ( 'NONE',  ( -6.063463321072276813, 3.088760411028184549, 19.00736729804353331 ) ) ;
#10949 = CARTESIAN_POINT ( 'NONE',  ( -6.016489644550737204, -18.20227673842147809, 4.872725758886126357 ) ) ;
#10950 = CARTESIAN_POINT ( 'NONE',  ( 0.7056759521544945235, 40.77723470137082273, -23.17252595696689355 ) ) ;
#10951 = CARTESIAN_POINT ( 'NONE',  ( 1.000110580585050979, 3.539822106476956609, 41.75987478700575650 ) ) ;
#10952 = FACE_OUTER_BOUND ( 'NONE', #24730, .T. ) ;
#10953 = CARTESIAN_POINT ( 'NONE',  ( 0.8557997880470697982, 47.60865952216998664, 5.347802024197403803 ) ) ;
#10954 = CIRCLE ( 'NONE', #25966, 42.92674063221959813 ) ;
#10955 = ORIENTED_EDGE ( 'NONE', *, *, #29340, .T. ) ;
#10956 = CARTESIAN_POINT ( 'NONE',  ( 4.553261556744873317, -41.61700166486752295, 14.05577241741092998 ) ) ;
#10957 = CIRCLE ( 'NONE', #4887, 42.92674063221959813 ) ;
#10958 = CARTESIAN_POINT ( 'NONE',  ( 0.1102847568649952675, 43.12433804869904463, -0.09217763870855683050 ) ) ;
#10959 = CARTESIAN_POINT ( 'NONE',  ( 1.296416391601052265, 24.29467132511798511, -36.77059041245664162 ) ) ;
#10960 = CARTESIAN_POINT ( 'NONE',  ( 0.8557997880470697982, 11.51622788066522851, -46.50333260518546297 ) ) ;
#10961 = CARTESIAN_POINT ( 'NONE',  ( -2.569797478183783568, 0.4487456364276796728, 14.62602397812941568 ) ) ;
#10962 = VERTEX_POINT ( 'NONE', #22488 ) ;
#10963 = EDGE_CURVE ( 'NONE', #34397, #5387, #54726, .T. ) ;
#10964 = CARTESIAN_POINT ( 'NONE',  ( 0.9594984694709473017, -0.4222239975805204826, -44.08486519868079512 ) ) ;
#10965 = CARTESIAN_POINT ( 'NONE',  ( 0.6021448801613057400, 28.30905802261198900, -40.12652953470227857 ) ) ;
#10966 = EDGE_CURVE ( 'NONE', #3479, #38027, #40790, .T. ) ;
#10967 = CARTESIAN_POINT ( 'NONE',  ( -2.569797478183790229, -14.55946937464484847, 1.464172661883917703 ) ) ;
#10968 = ORIENTED_EDGE ( 'NONE', *, *, #58806, .F. ) ;
#10969 = CARTESIAN_POINT ( 'NONE',  ( -6.016489644550737204, -18.68142234211822839, -2.463898142942957836 ) ) ;
#10970 = EDGE_CURVE ( 'NONE', #46146, #17208, #29338, .T. ) ;
#10971 = CARTESIAN_POINT ( 'NONE',  ( 0.9762797500689124330, 15.53330887509081215, 38.92352888134283262 ) ) ;
#10972 = VERTEX_POINT ( 'NONE', #3972 ) ;
#10973 = CARTESIAN_POINT ( 'NONE',  ( -5.995132425357893702, 4.869002713216827871, -18.20425902871262736 ) ) ;
#10974 = CIRCLE ( 'NONE', #9946, 15.99999999999999645 ) ;
#10975 = ORIENTED_EDGE ( 'NONE', *, *, #27473, .T. ) ;
#10976 = DIRECTION ( 'NONE',  ( -1.000000000000000000, -0.000000000000000000, -0.000000000000000000 ) ) ;
#10977 = ORIENTED_EDGE ( 'NONE', *, *, #29906, .T. ) ;
#10978 = CARTESIAN_POINT ( 'NONE',  ( 4.975610109902397937, 48.58133226360775581, 5.683622315980952244 ) ) ;
#10979 = CARTESIAN_POINT ( 'NONE',  ( 4.999999999999998224, -2.649999999999161471, -80.00000000000004263 ) ) ;
#10980 = VERTEX_POINT ( 'NONE', #33755 ) ;
#10981 = CARTESIAN_POINT ( 'NONE',  ( 0.5997462898726536595, 4.195097405483644515, -48.92803682862019343 ) ) ;
#10982 = VERTEX_POINT ( 'NONE', #23112 ) ;
#10983 = CARTESIAN_POINT ( 'NONE',  ( 0.9790724872846768845, 20.17598226788706128, -36.73234200956102313 ) ) ;
#10984 = CARTESIAN_POINT ( 'NONE',  ( 0.5999999999999994227, -11.64055411052240352, -1.199999999999999956 ) ) ;
#10985 = EDGE_CURVE ( 'NONE', #9646, #33299, #33138, .T. ) ;
#10986 =( BOUNDED_SURFACE ( )  B_SPLINE_SURFACE ( 3, 1, ( 
 ( #59800, #6524 ),
 ( #36027, #11586 ),
 ( #39490, #10658 ),
 ( #10973, #5913 ) ),
 .UNSPECIFIED., .F., .F., .F. ) 
 B_SPLINE_SURFACE_WITH_KNOTS ( ( 4, 4 ),
 ( 2, 2 ),
 ( 0.000000000000000000, 1.000000000000000000 ),
 ( 0.000000000000000000, 1.000000000000000000 ),
 .UNSPECIFIED. ) 
 GEOMETRIC_REPRESENTATION_ITEM ( )  RATIONAL_B_SPLINE_SURFACE ( (
 ( 1.000000000000000000, 1.000000000000000000),
 ( 0.7223157951917480446, 0.9931996967497186413),
 ( 0.7223157951917480446, 0.9931996967497186413),
 ( 1.000000000000000000, 1.000000000000000000) ) ) 
 REPRESENTATION_ITEM ( '' )  SURFACE ( )  );
#10987 = EDGE_LOOP ( 'NONE', ( #14158, #38902, #31865, #59387 ) ) ;
#10988 = CARTESIAN_POINT ( 'NONE',  ( 0.5782707292762423457, -39.07253195953412472, -25.94366203871003762 ) ) ;
#10989 = CARTESIAN_POINT ( 'NONE',  ( 0.5839880159502343071, 33.89965136132193635, -33.83547574026591320 ) ) ;
#10990 = CARTESIAN_POINT ( 'NONE',  ( 0.6017666602106489515, 24.35550044372386580, 41.48673504406954038 ) ) ;
#10991 = CARTESIAN_POINT ( 'NONE',  ( 0.6025881611877910160, 44.36157157392728578, 18.61132239451801595 ) ) ;
#10992 = ORIENTED_EDGE ( 'NONE', *, *, #20312, .T. ) ;
#10993 = ADVANCED_FACE ( 'NONE', ( #32832 ), #10763, .F. ) ;
#10994 = DIRECTION ( 'NONE',  ( 0.000000000000000000, 0.000000000000000000, 1.000000000000000000 ) ) ;
#10995 = CARTESIAN_POINT ( 'NONE',  ( -90.00000000000000000, 0.000000000000000000, -5.612499999999999822 ) ) ;
#10996 = ORIENTED_EDGE ( 'NONE', *, *, #45461, .T. ) ;
#10997 = CARTESIAN_POINT ( 'NONE',  ( 3.782625744892852637, -21.14745495448669388, 36.33212425723217365 ) ) ;
#10998 = EDGE_CURVE ( 'NONE', #10972, #43985, #24120, .T. ) ;
#10999 = ORIENTED_EDGE ( 'NONE', *, *, #56070, .T. ) ;
#11000 = CARTESIAN_POINT ( 'NONE',  ( 3.782625744892853525, -3.127219394304327160, -41.92205389714212771 ) ) ;
#11001 = CARTESIAN_POINT ( 'NONE',  ( 0.1129192098497447394, 25.64022107388777272, 35.91003830501040994 ) ) ;
#11002 = VERTEX_POINT ( 'NONE', #47532 ) ;
#11003 = FACE_OUTER_BOUND ( 'NONE', #35337, .T. ) ;
#11004 = CARTESIAN_POINT ( 'NONE',  ( 0.8751705887134423323, -46.21789262997747727, -13.30665218149346529 ) ) ;
#11005 = CARTESIAN_POINT ( 'NONE',  ( 51.35620144615297988, 12.24479674684753761, -2.513874600954978167 ) ) ;
#11006 = FACE_OUTER_BOUND ( 'NONE', #30682, .T. ) ;
#11007 = CIRCLE ( 'NONE', #58952, 42.92674063221959813 ) ;
#11008 = EDGE_LOOP ( 'NONE', ( #28735, #56263, #6443, #24231 ) ) ;
#11009 = CARTESIAN_POINT ( 'NONE',  ( 0.6027935024548037868, 18.57106801640299309, -44.37842839362955516 ) ) ;
#11010 =( NAMED_UNIT ( * ) SI_UNIT ( $, .STERADIAN. ) SOLID_ANGLE_UNIT ( ) );
#11013 = EDGE_CURVE ( 'NONE', #40686, #42210, #37678, .T. ) ;
#11012 = B_SPLINE_CURVE_WITH_KNOTS ( 'NONE', 3,
 ( #33147, #58147, #52221, #33768, #52850, #24350 ),
 .UNSPECIFIED., .F., .F.,
 ( 4, 2, 4 ),
 ( 0.000000000000000000, 0.0002447195606305733366, 0.0004894391212611466733 ),
 .UNSPECIFIED. ) ;
#11011 = CARTESIAN_POINT ( 'NONE',  ( 0.9730545539215883499, 33.73144377768558400, 26.52009130076782739 ) ) ;
#11014 =( NAMED_UNIT ( * ) PLANE_ANGLE_UNIT ( ) SI_UNIT ( $, .RADIAN. ) );
#11015 = FACE_OUTER_BOUND ( 'NONE', #27422, .T. ) ;
#11016 = CARTESIAN_POINT ( 'NONE',  ( 4.553261556744875094, 0.000000000000000000, 0.000000000000000000 ) ) ;
#11017 = CARTESIAN_POINT ( 'NONE',  ( 5.959828726073459926, -17.77343634131849015, 10.26672511661725018 ) ) ;
#11018 = VECTOR ( 'NONE', #58343, 1000.000000000000114 ) ;
#11019 = CARTESIAN_POINT ( 'NONE',  ( -16.29569048063198267, -7.897460783358359215, 1.291753785943115407 ) ) ;
#11020 = CARTESIAN_POINT ( 'NONE',  ( 1.830465331921977912, -2.645429179032414257, 43.97019172504383988 ) ) ;
#11021 = CARTESIAN_POINT ( 'NONE',  ( 4.691466044806103852, 33.30232861642433306, -29.64918311951093699 ) ) ;
#11022 = CARTESIAN_POINT ( 'NONE',  ( 0.8551540677456834771, 41.94570365541202506, 23.16399837394560990 ) ) ;
#11023 = CARTESIAN_POINT ( 'NONE',  ( 5.896782393890504181, -13.97772289704291460, 14.46199673252260354 ) ) ;
#11024 = DIRECTION ( 'NONE',  ( 0.000000000000000000, 0.000000000000000000, 1.000000000000000000 ) ) ;
#11025 = CARTESIAN_POINT ( 'NONE',  ( 0.5827359174754823679, 33.60976280407646755, 34.12345922495620698 ) ) ;
#11026 = DIRECTION ( 'NONE',  ( 0.09835009131224567436, 0.2500873580884576119, 0.9632152266566431642 ) ) ;
#11027 = ORIENTED_EDGE ( 'NONE', *, *, #34529, .F. ) ;
#11028 = CARTESIAN_POINT ( 'NONE',  ( 2.299652685299201416, -43.34123383624062598, 22.93074735830615651 ) ) ;
#11029 = CARTESIAN_POINT ( 'NONE',  ( 0.7948878604505666967, -6.978576542600043453, 48.60039214592296730 ) ) ;
#11030 = DIRECTION ( 'NONE',  ( 0.000000000000000000, 0.000000000000000000, 1.000000000000000000 ) ) ;
#11031 = ORIENTED_EDGE ( 'NONE', *, *, #26734, .T. ) ;
#11032 = EDGE_CURVE ( 'NONE', #59631, #22147, #27748, .T. ) ;
#11033 = CARTESIAN_POINT ( 'NONE',  ( 0.3676999524040323597, -22.15802448779959377, -38.14410221935904843 ) ) ;
#11034 = CARTESIAN_POINT ( 'NONE',  ( 0.1156867017252034419, 4.112540283844289490, 43.93210465808513021 ) ) ;
#11035 = B_SPLINE_CURVE_WITH_KNOTS ( 'NONE', 3,
 ( #21064, #40208, #44280, #59258, #16363, #11675, #49879, #6938, #40506, #59572, #16677, #35801, #54866, #58317, #12003, #39267, #20150, #34554, #10748 ),
 .UNSPECIFIED., .F., .F.,
 ( 4, 3, 3, 3, 3, 3, 4 ),
 ( 1.153344816771540786E-16, 0.0002618519381806261336, 0.0003927759815485985231, 0.0005237000248299446227, 0.0006546240681324982588, 0.0007855481115631335765, 0.0009699050456655117008 ),
 .UNSPECIFIED. ) ;
#11036 = EDGE_CURVE ( 'NONE', #31232, #21995, #12267, .T. ) ;
#11037 = VERTEX_POINT ( 'NONE', #32513 ) ;
#11038 = ORIENTED_EDGE ( 'NONE', *, *, #11476, .T. ) ;
#11039 = LINE ( 'NONE', #11339, #56548 ) ;
#11040 = EDGE_CURVE ( 'NONE', #34042, #46958, #51588, .T. ) ;
#11041 = ORIENTED_EDGE ( 'NONE', *, *, #33591, .T. ) ;
#11042 = EDGE_CURVE ( 'NONE', #44269, #15676, #44458, .T. ) ;
#11044 = CARTESIAN_POINT ( 'NONE',  ( 0.8753041380234530822, 11.79227530596865847, 47.66634631457734628 ) ) ;
#11043 = B_SPLINE_CURVE_WITH_KNOTS ( 'NONE', 3,
 ( #10007, #56666, #23790, #38222, #33822, #57269, #14402, #42918, #27872, #43224, #42301, #61970, #28171, #4033, #33511, #28792, #46683, #260, #19407 ),
 .UNSPECIFIED., .F., .F.,
 ( 4, 3, 3, 3, 3, 3, 4 ),
 ( 1.040890552917501732E-17, 0.0002732106629380587457, 0.0004098138914053709326, 0.0005464171197651407266, 0.0006830203481512488271, 0.0008196235766963528993, 0.001011968216111136607 ),
 .UNSPECIFIED. ) ;
#11045 = EDGE_CURVE ( 'NONE', #7463, #46592, #25258, .T. ) ;
#11046 = ORIENTED_EDGE ( 'NONE', *, *, #41415, .T. ) ;
#11047 = ORIENTED_EDGE ( 'NONE', *, *, #9760, .T. ) ;
#11048 = CARTESIAN_POINT ( 'NONE',  ( 0.6039202388192952409, -48.68192096202334085, -6.452463428513433463 ) ) ;
#11049 = EDGE_LOOP ( 'NONE', ( #29683, #26496, #15309, #10415 ) ) ;
#11050 = LINE ( 'NONE', #43650, #12094 ) ;
#11051 = CARTESIAN_POINT ( 'NONE',  ( 0.5987334363312689645, 41.48360609181539616, -26.28066460520305725 ) ) ;
#11052 = ORIENTED_EDGE ( 'NONE', *, *, #7819, .F. ) ;
#11053 = CARTESIAN_POINT ( 'NONE',  ( 0.8560838555295158248, -2.480523550131575661, 46.84250032821661591 ) ) ;
#11054 = CLOSED_SHELL ( 'NONE', ( #16134, #10550, #43383, #44525, #10003, #33207, #22022, #53580, #21743, #61635, #57359, #12192, #56573, #6910, #14160, #21274, #61922, #39300, #56281, #22127, #57051, #53773, #44022, #56991, #18338, #61290, #18801, #33471, #55309, #46488, #45799, #21069, #49011 ) ) ;
#11055 = EDGE_CURVE ( 'NONE', #37013, #56393, #19041, .T. ) ;
#11056 = FACE_OUTER_BOUND ( 'NONE', #24528, .T. ) ;
#11057 = EDGE_CURVE ( 'NONE', #42620, #28210, #55609, .T. ) ;
#11058 = ORIENTED_EDGE ( 'NONE', *, *, #8973, .F. ) ;
#11059 = DIRECTION ( 'NONE',  ( -0.000000000000000000, -1.000000000000000000, -0.000000000000000000 ) ) ;
#11060 = CIRCLE ( 'NONE', #34058, 11.40403086437694569 ) ;
#11061 = CARTESIAN_POINT ( 'NONE',  ( 4.960386119450151732, -3.911092338298454152, -43.57912139308966459 ) ) ;
#11062 = CARTESIAN_POINT ( 'NONE',  ( 0.5809828226811617480, 24.41822904836982389, -41.20389530892281726 ) ) ;
#11063 = CARTESIAN_POINT ( 'NONE',  ( 5.860006189529234355, 36.27483683749437660, 31.78942168514575073 ) ) ;
#11064 = EDGE_LOOP ( 'NONE', ( #60636, #49572, #52885, #32244 ) ) ;
#11065 = CARTESIAN_POINT ( 'NONE',  ( 3.661933894777873455, -46.77018561706699273, -5.018057621904368659 ) ) ;
#11066 = CARTESIAN_POINT ( 'NONE',  ( 0.6001305935487422083, 5.760103278698015750, -47.76436356026962216 ) ) ;
#11067 = ORIENTED_EDGE ( 'NONE', *, *, #46212, .F. ) ;
#11068 = CARTESIAN_POINT ( 'NONE',  ( 2.879087469061463178, -42.96833078670570671, -9.477564359455300291 ) ) ;
#11069 = CARTESIAN_POINT ( 'NONE',  ( -6.078726893082806448, 9.985094725776445301, -16.46486940689149137 ) ) ;
#11070 = FACE_OUTER_BOUND ( 'NONE', #34164, .T. ) ;
#11071 = CARTESIAN_POINT ( 'NONE',  ( 0.6024113833632039894, -35.12450729357964718, -34.31924906643699558 ) ) ;
#11072 = B_SPLINE_CURVE_WITH_KNOTS ( 'NONE', 3,
 ( #52529, #14043, #9623, #33143, #4907, #4282 ),
 .UNSPECIFIED., .F., .F.,
 ( 4, 2, 4 ),
 ( 4.336808689942017736E-19, 0.0002291459268755708040, 0.0004582918537511411743 ),
 .UNSPECIFIED. ) ;
#11073 = ORIENTED_EDGE ( 'NONE', *, *, #31768, .T. ) ;
#11074 = ORIENTED_EDGE ( 'NONE', *, *, #12320, .T. ) ;
#11075 = LINE ( 'NONE', #5102, #51937 ) ;
#11076 = CARTESIAN_POINT ( 'NONE',  ( 0.5800708057587393718, -13.00144577271073132, 46.09746469244092282 ) ) ;
#11077 = CARTESIAN_POINT ( 'NONE',  ( 0.1073791018717578927, -40.02496097243069784, 16.05399293000745686 ) ) ;
#11079 = ADVANCED_FACE ( 'NONE', ( #24649 ), #60276, .F. ) ;
#11078 = CARTESIAN_POINT ( 'NONE',  ( -6.078075953587585900, -19.21613803895145622, 1.239037172605796489 ) ) ;
#11080 = CARTESIAN_POINT ( 'NONE',  ( 4.975801465491695552, 0.000000000000000000, 0.000000000000000000 ) ) ;
#11081 = CARTESIAN_POINT ( 'NONE',  ( 0.2885697896453111588, -43.10898998017122352, -0.8047882042605032371 ) ) ;
#11082 =( BOUNDED_SURFACE ( )  B_SPLINE_SURFACE ( 3, 1, ( 
 ( #42867, #3370 ),
 ( #61615, #38173 ),
 ( #61920, #14352 ),
 ( #50994, #8091 ) ),
 .UNSPECIFIED., .F., .F., .F. ) 
 B_SPLINE_SURFACE_WITH_KNOTS ( ( 4, 4 ),
 ( 2, 2 ),
 ( 0.000000000000000000, 1.000000000000000000 ),
 ( 0.000000000000000000, 1.000000000000000000 ),
 .UNSPECIFIED. ) 
 GEOMETRIC_REPRESENTATION_ITEM ( )  RATIONAL_B_SPLINE_SURFACE ( (
 ( 1.000000000000000000, 1.000000000000000000),
 ( 0.7269869731126817891, 0.9931720237060910339),
 ( 0.7269869731126817891, 0.9931720237060910339),
 ( 1.000000000000000000, 1.000000000000000000) ) ) 
 REPRESENTATION_ITEM ( '' )  SURFACE ( )  );
#11083 = CARTESIAN_POINT ( 'NONE',  ( -1.200000000000006617, 0.000000000000000000, 0.000000000000000000 ) ) ;
#11084 = EDGE_CURVE ( 'NONE', #6983, #46350, #21234, .T. ) ;
#11085 = DIRECTION ( 'NONE',  ( 0.07836865515943411409, -0.9873352307081171286, -0.1379401902675598812 ) ) ;
#11086 = CARTESIAN_POINT ( 'NONE',  ( 1.112077966505211624, -13.54489572197889302, -41.94718256342459739 ) ) ;
#11087 = CARTESIAN_POINT ( 'NONE',  ( 0.1073791018717578927, 30.83464511437137645, -30.14884492832358731 ) ) ;
#11088 = LINE ( 'NONE', #44926, #17862 ) ;
#11089 = CARTESIAN_POINT ( 'NONE',  ( 0.1157506346131639274, -7.133777142707746322, -43.54365491642857933 ) ) ;
#11090 = CARTESIAN_POINT ( 'NONE',  ( 4.549368137175248350, 40.71620287708344677, -13.59764261105707739 ) ) ;
#11091 = CARTESIAN_POINT ( 'NONE',  ( -2.569797478183790229, -1.464172661884063587, -14.55946937464483248 ) ) ;
#11092 = B_SPLINE_CURVE_WITH_KNOTS ( 'NONE', 3,
 ( #18158, #4021, #33809, #52887 ),
 .UNSPECIFIED., .F., .F.,
 ( 4, 4 ),
 ( 0.000000000000000000, 0.005014147105413695182 ),
 .UNSPECIFIED. ) ;
#11093 = CARTESIAN_POINT ( 'NONE',  ( 5.959828726073459926, 20.34941966491235732, 2.683617577144452593 ) ) ;
#11094 = DIRECTION ( 'NONE',  ( 1.000000000000000000, 0.000000000000000000, 0.000000000000000000 ) ) ;
#11095 = LINE ( 'NONE', #1655, #29647 ) ;
#11096 = CONTEXT_DEPENDENT_SHAPE_REPRESENTATION ( #44094, #5313 ) ;
#11097 = CARTESIAN_POINT ( 'NONE',  ( 0.1119898979215350893, 44.06612418549229915, 2.266717344663642386 ) ) ;
#11098 =( BOUNDED_SURFACE ( )  B_SPLINE_SURFACE ( 3, 1, ( 
 ( #37088, #18897 ),
 ( #61155, #27968 ),
 ( #57067, #13572 ),
 ( #13891, #9782 ) ),
 .UNSPECIFIED., .F., .F., .F. ) 
 B_SPLINE_SURFACE_WITH_KNOTS ( ( 4, 4 ),
 ( 2, 2 ),
 ( 0.000000000000000000, 1.000000000000000000 ),
 ( 0.000000000000000000, 1.000000000000000000 ),
 .UNSPECIFIED. ) 
 GEOMETRIC_REPRESENTATION_ITEM ( )  RATIONAL_B_SPLINE_SURFACE ( (
 ( 1.000000000000000000, 1.000000000000000000),
 ( 0.9732289882329797637, 0.9999525324661233672),
 ( 0.9732289882329797637, 0.9999525324661233672),
 ( 1.000000000000000000, 1.000000000000000000) ) ) 
 REPRESENTATION_ITEM ( '' )  SURFACE ( )  );
#11099 = CIRCLE ( 'NONE', #26065, 13.00000000000000178 ) ;
#11100 = CARTESIAN_POINT ( 'NONE',  ( 0.9747592971366240144, -10.79247637456148645, 41.52905920980982302 ) ) ;
#11101 = CARTESIAN_POINT ( 'NONE',  ( 1.827119703190778877, -22.58367210012866266, -36.65069040194700989 ) ) ;
#11102 = CARTESIAN_POINT ( 'NONE',  ( 5.960721111146673579, 10.25731071096558011, 17.77882586010670707 ) ) ;
#11104 = ORIENTED_EDGE ( 'NONE', *, *, #22563, .T. ) ;
#11103 = CARTESIAN_POINT ( 'NONE',  ( 0.7762783648524412827, 41.03453896757974917, -24.71864151483671890 ) ) ;
#11105 = ORIENTED_EDGE ( 'NONE', *, *, #12614, .T. ) ;
#11106 = CARTESIAN_POINT ( 'NONE',  ( 0.2885700199627509455, -33.71073713194540034, 26.88157179738447056 ) ) ;
#11107 = CARTESIAN_POINT ( 'NONE',  ( 3.221118495291109163, 43.73404891492205593, -4.700466484186104132 ) ) ;
#11108 = CARTESIAN_POINT ( 'NONE',  ( 4.967162193818129623, 40.65506779172164897, 14.26841313271295952 ) ) ;
#11109 = VERTEX_POINT ( 'NONE', #58136 ) ;
#11110 = EDGE_CURVE ( 'NONE', #38885, #17061, #6998, .T. ) ;
#11111 = ORIENTED_EDGE ( 'NONE', *, *, #45565, .T. ) ;
#11112 = CARTESIAN_POINT ( 'NONE',  ( 0.1104177457020373010, -11.15670205480033594, 41.65628910360720027 ) ) ;
#11113 = CARTESIAN_POINT ( 'NONE',  ( 0.8760168074887076939, -28.57146030082009247, 38.69913431881774102 ) ) ;
#11114 = CARTESIAN_POINT ( 'NONE',  ( 0.5806925824938502512, -29.85799195566318431, 36.16244846134061675 ) ) ;
#11115 = ADVANCED_FACE ( 'NONE', ( #57826 ), #49873, .F. ) ;
#11116 = ORIENTED_EDGE ( 'NONE', *, *, #7479, .T. ) ;
#11117 = ORIENTED_EDGE ( 'NONE', *, *, #42375, .F. ) ;
#11118 = CARTESIAN_POINT ( 'NONE',  ( 0.6017666602106488405, -24.35550044372416068, -41.48673504406937695 ) ) ;
#11119 = ADVANCED_FACE ( 'NONE', ( #1736 ), #53512, .F. ) ;
#11120 = CARTESIAN_POINT ( 'NONE',  ( 0.8753041380234465318, 43.84722337925211377, 22.10337824412700058 ) ) ;
#11121 = CARTESIAN_POINT ( 'NONE',  ( 0.5834584762367756028, -38.55966758064684541, -26.69059806529635637 ) ) ;
#11122 = CARTESIAN_POINT ( 'NONE',  ( 2.528190830796655852, 2.996102205408210928, 41.87215671216083734 ) ) ;
#11123 = EDGE_CURVE ( 'NONE', #51919, #55413, #39385, .T. ) ;
#11124 = CARTESIAN_POINT ( 'NONE',  ( 4.956653778116992370, 3.690426056930664611, -47.94889704119048446 ) ) ;
#11125 = FACE_OUTER_BOUND ( 'NONE', #53623, .T. ) ;
#11126 = CARTESIAN_POINT ( 'NONE',  ( 0.1135584504625008484, 15.64364923084964332, -41.25806940317724525 ) ) ;
#11127 = ORIENTED_EDGE ( 'NONE', *, *, #23636, .F. ) ;
#11128 = ORIENTED_EDGE ( 'NONE', *, *, #13882, .F. ) ;
#11129 = CARTESIAN_POINT ( 'NONE',  ( 0.5988103622719986863, 44.67429504351059677, -17.84821742497949515 ) ) ;
#11130 = FACE_OUTER_BOUND ( 'NONE', #38113, .T. ) ;
#11131 = ORIENTED_EDGE ( 'NONE', *, *, #44743, .T. ) ;
#11132 = CARTESIAN_POINT ( 'NONE',  ( -6.010958268070873523, -18.20513189769812357, 4.863021950010583794 ) ) ;
#11133 = CARTESIAN_POINT ( 'NONE',  ( 0.6027444965799114707, -7.966449588082729072, 48.45693136020871350 ) ) ;
#11134 = DIRECTION ( 'NONE',  ( 0.000000000000000000, 0.000000000000000000, 1.000000000000000000 ) ) ;
#11135 = CARTESIAN_POINT ( 'NONE',  ( 0.1156495703730067576, -40.95039897516667082, -16.43191337019942111 ) ) ;
#11136 = VERTEX_POINT ( 'NONE', #35290 ) ;
#11137 = CARTESIAN_POINT ( 'NONE',  ( 0.5817216825391139379, 46.41469338179018678, -6.701581192663303987 ) ) ;
#11138 = CARTESIAN_POINT ( 'NONE',  ( 0.6017667736363749853, 18.08696174077326901, 44.57803721604157943 ) ) ;
#11139 = CARTESIAN_POINT ( 'NONE',  ( 0.5819845901640494645, 44.07435474487846250, 18.74765780149844474 ) ) ;
#11140 = B_SPLINE_CURVE_WITH_KNOTS ( 'NONE', 3,
 ( #40021, #1435, #39705, #20879 ),
 .UNSPECIFIED., .F., .F.,
 ( 4, 4 ),
 ( 0.000000000000000000, 0.005013413432710153717 ),
 .UNSPECIFIED. ) ;
#11141 = CARTESIAN_POINT ( 'NONE',  ( 5.910764540655177868, -19.40170003828502487, 5.298610581423578658 ) ) ;
#11142 = ORIENTED_EDGE ( 'NONE', *, *, #13232, .T. ) ;
#11143 = DIRECTION ( 'NONE',  ( 0.000000000000000000, 0.000000000000000000, 1.000000000000000000 ) ) ;
#11144 = CARTESIAN_POINT ( 'NONE',  ( 2.618530812446111078, -26.46994001813007813, 38.84673814665519131 ) ) ;
#11145 = ORIENTED_EDGE ( 'NONE', *, *, #32909, .F. ) ;
#11146 = CARTESIAN_POINT ( 'NONE',  ( 0.5998501479064699549, 41.92175333043586960, 23.59887241503369282 ) ) ;
#11147 = CARTESIAN_POINT ( 'NONE',  ( -6.015611763856276717, 16.31561949997075445, 9.427003116184231146 ) ) ;
#11148 = ORIENTED_EDGE ( 'NONE', *, *, #4656, .F. ) ;
#11149 = CARTESIAN_POINT ( 'NONE',  ( 0.5997462898726536595, -8.352924653000044941, -48.39194436975655123 ) ) ;
#11150 = CARTESIAN_POINT ( 'NONE',  ( 0.6031357023905874470, -47.70157053127533686, 6.236038527293246148 ) ) ;
#11151 = CARTESIAN_POINT ( 'NONE',  ( 0.3622758884714730732, 0.8252992914322084816, 43.10531414739106282 ) ) ;
#11152 = B_SPLINE_CURVE_WITH_KNOTS ( 'NONE', 3,
 ( #34224, #6282, #44563, #53597 ),
 .UNSPECIFIED., .F., .F.,
 ( 4, 4 ),
 ( 2.504207788927570074E-17, 0.004564976165746191181 ),
 .UNSPECIFIED. ) ;
#11153 = CARTESIAN_POINT ( 'NONE',  ( 0.1129192098497447394, -7.520259262076021578, -43.47870154933693243 ) ) ;
#11154 = CARTESIAN_POINT ( 'NONE',  ( 2.282803330402966235, -37.96809118126141414, -27.65720447746669919 ) ) ;
#11155 = CARTESIAN_POINT ( 'NONE',  ( 3.894904216938898323, 22.27749296280804714, 37.89244832111325678 ) ) ;
#11156 = CARTESIAN_POINT ( 'NONE',  ( 4.322998006666179727, -46.85697641700701155, -10.36018990813296448 ) ) ;
#11157 = ADVANCED_FACE ( 'NONE', ( #5509 ), #13481, .F. ) ;
#11158 = CARTESIAN_POINT ( 'NONE',  ( 4.549368137175248350, 18.79584381673534565, -38.59302160394733505 ) ) ;
#11159 = CARTESIAN_POINT ( 'NONE',  ( 0.7044674535453004927, 48.94804745615595465, -3.986398505018412308 ) ) ;
#11160 = CARTESIAN_POINT ( 'NONE',  ( 0.5836750258453375917, -24.10509086647779853, 41.38803015411996711 ) ) ;
#11161 = CYLINDRICAL_SURFACE ( 'NONE', #8649, 8.000000000000000000 ) ;
#11162 = CARTESIAN_POINT ( 'NONE',  ( 0.9772918015221170318, 15.44874721096192260, 38.95732364219180255 ) ) ;
#11163 = ORIENTED_EDGE ( 'NONE', *, *, #7949, .F. ) ;
#11164 = CARTESIAN_POINT ( 'NONE',  ( 5.981074661064941900, -14.50705827991455976, 14.51919955600710566 ) ) ;
#11165 = FACE_OUTER_BOUND ( 'NONE', #59413, .T. ) ;
#11166 = CARTESIAN_POINT ( 'NONE',  ( 4.975801465491695552, -27.09127437476353251, -39.51822597168487050 ) ) ;
#11167 = FACE_OUTER_BOUND ( 'NONE', #58950, .T. ) ;
#11168 = CARTESIAN_POINT ( 'NONE',  ( 0.6029442701453591180, -19.79821103535463322, 44.93969364557171531 ) ) ;
#11169 = CARTESIAN_POINT ( 'NONE',  ( 0.3622758884714600280, 41.42293301073608802, 11.95365414648511582 ) ) ;
#11170 = DIRECTION ( 'NONE',  ( -1.000000000000000000, -7.166653630759621722E-15, -1.836909530734304951E-16 ) ) ;
#11171 = CARTESIAN_POINT ( 'NONE',  ( 0.8554163680231816613, -46.86440027434175448, -2.221139355847804531 ) ) ;
#11172 = CARTESIAN_POINT ( 'NONE',  ( 0.6031356755852238516, -0.04363310494625852187, 48.10744332413860747 ) ) ;
#11173 = CARTESIAN_POINT ( 'NONE',  ( 3.680974057930773036, -30.65154904503207689, 36.90739001595120072 ) ) ;
#11175 = ORIENTED_EDGE ( 'NONE', *, *, #25863, .T. ) ;
#11174 = CARTESIAN_POINT ( 'NONE',  ( 4.962356264823602814, -33.29728444345256122, -25.73958909062380229 ) ) ;
#11176 = EDGE_LOOP ( 'NONE', ( #35468, #31545 ) ) ;
#11177 = CARTESIAN_POINT ( 'NONE',  ( 1.227938101723756947, 42.43379953535195170, -6.439911493064139236 ) ) ;
#11178 = FACE_BOUND ( 'NONE', #11176, .T. ) ;
#11179 = CARTESIAN_POINT ( 'NONE',  ( -6.015611763856276717, -16.31561949997082905, 9.427003116184113907 ) ) ;
#11180 = CARTESIAN_POINT ( 'NONE',  ( 0.5839254288179555052, -47.49799454719521208, 6.161657890844768559 ) ) ;
#11181 = CARTESIAN_POINT ( 'NONE',  ( 0.5326698147273822848, 0.000000000000000000, 0.000000000000000000 ) ) ;
#11182 = CIRCLE ( 'NONE', #50204, 42.08604991992415023 ) ;
#11183 = EDGE_CURVE ( 'NONE', #6759, #27417, #36901, .T. ) ;
#11184 = CIRCLE ( 'NONE', #56141, 42.08604991992415023 ) ;
#11185 = ORIENTED_EDGE ( 'NONE', *, *, #41468, .F. ) ;
#11186 = EDGE_LOOP ( 'NONE', ( #52947, #9568, #59157, #37040 ) ) ;
#11187 = EDGE_CURVE ( 'NONE', #55039, #48869, #45885, .T. ) ;
#11188 = CARTESIAN_POINT ( 'NONE',  ( 3.678834586032788234, 20.99745812816111723, 44.24611985004418813 ) ) ;
#11189 = CARTESIAN_POINT ( 'NONE',  ( 0.1084644655670283370, -39.99242539812104980, -16.13497904887289636 ) ) ;
#11190 = CARTESIAN_POINT ( 'NONE',  ( 4.553261556744873317, -33.59363643963353496, -28.30206982864260112 ) ) ;
#11191 = ORIENTED_EDGE ( 'NONE', *, *, #9911, .F. ) ;
#11192 = EDGE_CURVE ( 'NONE', #18069, #9258, #4777, .T. ) ;
#11193 = CARTESIAN_POINT ( 'NONE',  ( 0.8551540677456715978, -0.9122407826479158599, 47.90804413217340851 ) ) ;
#11194 = CARTESIAN_POINT ( 'NONE',  ( 5.894904586330512508, 10.82344038793352503, -16.95236119926932972 ) ) ;
#11195 = ORIENTED_EDGE ( 'NONE', *, *, #51799, .F. ) ;
#11196 =( BOUNDED_SURFACE ( )  B_SPLINE_SURFACE ( 3, 1, ( 
 ( #59751, #12169 ),
 ( #32419, #45378 ),
 ( #11539, #30623 ),
 ( #7422, #49741 ) ),
 .UNSPECIFIED., .F., .F., .F. ) 
 B_SPLINE_SURFACE_WITH_KNOTS ( ( 4, 4 ),
 ( 2, 2 ),
 ( 0.000000000000000000, 1.000000000000000000 ),
 ( 0.000000000000000000, 1.000000000000000000 ),
 .UNSPECIFIED. ) 
 GEOMETRIC_REPRESENTATION_ITEM ( )  RATIONAL_B_SPLINE_SURFACE ( (
 ( 1.000000000000000000, 1.000000000000000000),
 ( 0.9729067724841187204, 0.9999501103223794596),
 ( 0.9729067724841187204, 0.9999501103223794596),
 ( 1.000000000000000000, 1.000000000000000000) ) ) 
 REPRESENTATION_ITEM ( '' )  SURFACE ( )  );
#11197 = CARTESIAN_POINT ( 'NONE',  ( 0.9730545539215883499, 41.31259007387247095, -11.59290486963463351 ) ) ;
#11198 = EDGE_LOOP ( 'NONE', ( #45030, #3255, #24839, #49544 ) ) ;
#11199 = DIRECTION ( 'NONE',  ( 0.000000000000000000, 0.000000000000000000, 1.000000000000000000 ) ) ;
#11200 = EDGE_CURVE ( 'NONE', #1947, #14833, #27222, .T. ) ;
#11201 = CARTESIAN_POINT ( 'NONE',  ( 5.960721111146673579, 19.82781442290498219, -5.306302591836375981 ) ) ;
#11202 = EDGE_LOOP ( 'NONE', ( #18023, #25248, #21193, #7901 ) ) ;
#11203 = PLANE ( 'NONE',  #45538 ) ;
#11204 = DIRECTION ( 'NONE',  ( 0.000000000000000000, 0.000000000000000000, 1.000000000000000000 ) ) ;
#11205 = CARTESIAN_POINT ( 'NONE',  ( 0.5839880159502347512, 41.50181427378134913, -23.90868446765435351 ) ) ;
#11206 = CARTESIAN_POINT ( 'NONE',  ( 0.2224561200757619039, 43.11279565427785343, 0.7594684977686744221 ) ) ;
#11207 = EDGE_CURVE ( 'NONE', #10372, #885, #1797, .T. ) ;
#11208 = EDGE_LOOP ( 'NONE', ( #38329, #3191, #58633, #31795 ) ) ;
#11209 = CARTESIAN_POINT ( 'NONE',  ( 0.8554163680231816613, -35.40260165760457056, -30.78735566729940487 ) ) ;
#11210 = CARTESIAN_POINT ( 'NONE',  ( 0.6017666602106489515, 44.31084100715252561, -18.73203020817316045 ) ) ;
#11211 = VERTEX_POINT ( 'NONE', #55911 ) ;
#11212 = CARTESIAN_POINT ( 'NONE',  ( 2.301529144917016101, 47.77346141661144685, 4.990866136406802767 ) ) ;
#11213 = ORIENTED_EDGE ( 'NONE', *, *, #52028, .F. ) ;
#11214 = CARTESIAN_POINT ( 'NONE',  ( 0.5819845901640507968, -18.74765780149859395, 44.07435474487839144 ) ) ;
#11215 = ORIENTED_EDGE ( 'NONE', *, *, #19800, .F. ) ;
#11216 = FACE_OUTER_BOUND ( 'NONE', #6373, .T. ) ;
#11217 = CARTESIAN_POINT ( 'NONE',  ( 0.9787464366903551038, 36.14815773438009217, -21.20482693399881668 ) ) ;
#11218 = CARTESIAN_POINT ( 'NONE',  ( 3.783198216974390515, -41.98529422752523033, 9.462293521184724554 ) ) ;
#11219 = ORIENTED_EDGE ( 'NONE', *, *, #12906, .F. ) ;
#11220 = CARTESIAN_POINT ( 'NONE',  ( 4.967162193818130511, -7.970725651240091025, 42.34252806656591162 ) ) ;
#11221 = CARTESIAN_POINT ( 'NONE',  ( 2.643462169533613793, -44.89050350746140339, -17.09809940585645904 ) ) ;
#11222 = DIRECTION ( 'NONE',  ( 0.000000000000000000, 0.000000000000000000, 1.000000000000000000 ) ) ;
#11223 = ORIENTED_EDGE ( 'NONE', *, *, #7874, .F. ) ;
#11224 = TOROIDAL_SURFACE ( 'NONE', #17217, 15.38217999999999996, 0.05882000000000066342 ) ;
#11225 = ORIENTED_EDGE ( 'NONE', *, *, #20503, .F. ) ;
#11226 = CIRCLE ( 'NONE', #56235, 48.09070567114147110 ) ;
#11227 = CARTESIAN_POINT ( 'NONE',  ( 0.5839879882012675161, 18.32902119196566559, 44.25009266679212061 ) ) ;
#11228 = CARTESIAN_POINT ( 'NONE',  ( 0.7044674535453004927, 48.03641533699669708, -10.21300760708892419 ) ) ;
#11229 = CARTESIAN_POINT ( 'NONE',  ( 0.1101816497532063510, -5.763501205266821081, -42.73758747687828219 ) ) ;
#11230 = EDGE_CURVE ( 'NONE', #26300, #55548, #7049, .T. ) ;
#11231 = CARTESIAN_POINT ( 'NONE',  ( 0.9780106845699474416, -26.81709666672181669, -32.20519481113468885 ) ) ;
#11232 = CARTESIAN_POINT ( 'NONE',  ( 0.5987334363312689645, -45.74238923172318749, 17.86607774094835577 ) ) ;
#11233 = VERTEX_POINT ( 'NONE', #49991 ) ;
#11234 = CARTESIAN_POINT ( 'NONE',  ( 2.528190830796659405, -21.55884404307488822, -36.02041615083565773 ) ) ;
#11235 = VERTEX_POINT ( 'NONE', #54667 ) ;
#11236 = CARTESIAN_POINT ( 'NONE',  ( -4.000000000000000000, -0.3902508023145548899, -5.600000000000000533 ) ) ;
#11237 = CARTESIAN_POINT ( 'NONE',  ( 0.5837157313716030416, 45.20563255473990694, 12.47749369496385441 ) ) ;
#11238 = CARTESIAN_POINT ( 'NONE',  ( -6.079354080745853928, 18.62651132414728394, -4.883239819994009245 ) ) ;
#11239 = CARTESIAN_POINT ( 'NONE',  ( 2.706805983486679779, 11.39999808494296474, 42.50666014853498353 ) ) ;
#11240 =( LENGTH_UNIT ( ) NAMED_UNIT ( * ) SI_UNIT ( .MILLI., .METRE. ) );
#11241 = SURFACE_STYLE_FILL_AREA ( #40387 ) ;
#11242 = CARTESIAN_POINT ( 'NONE',  ( 0.1156495703730067437, 20.28816457620965252, -39.18332976355763719 ) ) ;
#11243 = CARTESIAN_POINT ( 'NONE',  ( 0.6067099128993241886, -5.548253864790723355, 47.57459301987700684 ) ) ;
#11244 = CARTESIAN_POINT ( 'NONE',  ( 0.1149546198390367646, 29.46142209737721984, 32.84769661670956964 ) ) ;
#11245 = CARTESIAN_POINT ( 'NONE',  ( 2.299746137290199943, -29.55404911945319668, 39.12594431232409420 ) ) ;
#11246 =( LENGTH_UNIT ( ) NAMED_UNIT ( * ) SI_UNIT ( .MILLI., .METRE. ) );
#11247 = CARTESIAN_POINT ( 'NONE',  ( 4.691466044806102076, 42.11359095667468466, 14.64802401911244445 ) ) ;
#11248 = DIRECTION ( 'NONE',  ( 0.07500201931887537365, -0.9580968512853003105, -0.2764509371575435970 ) ) ;
#11249 = CARTESIAN_POINT ( 'NONE',  ( 2.528100132419518253, 13.95210196817038018, -39.59283558046644913 ) ) ;
#11250 = CARTESIAN_POINT ( 'NONE',  ( 0.5806925824938502512, -20.23436166722406426, -42.30594485723652554 ) ) ;
#11251 = VERTEX_POINT ( 'NONE', #31820 ) ;
#11252 = EDGE_CURVE ( 'NONE', #9246, #59097, #38454, .T. ) ;
#11253 = CARTESIAN_POINT ( 'NONE',  ( 4.962356264823601926, -38.91448554252674796, -16.02805081171206680 ) ) ;
#11254 = CARTESIAN_POINT ( 'NONE',  ( 2.648799415243696664, -15.27490784895089071, 46.59607980823770390 ) ) ;
#11255 = CARTESIAN_POINT ( 'NONE',  ( 0.9749527285493314599, -25.89384247702547981, -34.21468599366735930 ) ) ;
#11256 = CARTESIAN_POINT ( 'NONE',  ( 0.7056555295713307085, 28.48870155114964220, -38.50897360867654839 ) ) ;
#11257 = CARTESIAN_POINT ( 'NONE',  ( 3.678748215320120973, -5.985490030740792555, 48.60850464056045439 ) ) ;
#11258 = EDGE_LOOP ( 'NONE', ( #39402, #41273, #50705, #26215 ) ) ;
#11259 = EDGE_CURVE ( 'NONE', #59478, #30308, #49622, .T. ) ;
#11260 = CARTESIAN_POINT ( 'NONE',  ( -2.601141883200662974, -6.448885681770537559, -13.46132612088584679 ) ) ;
#11261 = VECTOR ( 'NONE', #49221, 999.9999999999998863 ) ;
#11262 = EDGE_CURVE ( 'NONE', #49895, #52432, #45011, .T. ) ;
#11263 = CARTESIAN_POINT ( 'NONE',  ( 4.975610109902397937, 25.84633036597884725, -41.52609557555889808 ) ) ;
#11264 =( BOUNDED_SURFACE ( )  B_SPLINE_SURFACE ( 3, 1, ( 
 ( #50294, #45614 ),
 ( #61225, #28646 ),
 ( #4509, #33068 ),
 ( #3901, #51514 ) ),
 .UNSPECIFIED., .F., .F., .F. ) 
 B_SPLINE_SURFACE_WITH_KNOTS ( ( 4, 4 ),
 ( 2, 2 ),
 ( 0.000000000000000000, 1.000000000000000000 ),
 ( 0.000000000000000000, 1.000000000000000000 ),
 .UNSPECIFIED. ) 
 GEOMETRIC_REPRESENTATION_ITEM ( )  RATIONAL_B_SPLINE_SURFACE ( (
 ( 1.000000000000000000, 1.000000000000000000),
 ( 0.7282232189291693025, 0.9929344683865674037),
 ( 0.7282232189291693025, 0.9929344683865674037),
 ( 1.000000000000000000, 1.000000000000000000) ) ) 
 REPRESENTATION_ITEM ( '' )  SURFACE ( )  );
#11265 = VECTOR ( 'NONE', #59816, 1000.000000000000227 ) ;
#11266 = VERTEX_POINT ( 'NONE', #40932 ) ;
#11267 = CARTESIAN_POINT ( 'NONE',  ( 2.879087469061463178, -43.96707328741540977, 1.731514747965036349 ) ) ;
#11268 = CARTESIAN_POINT ( 'NONE',  ( 4.975610109902397937, -43.81605102859442979, -21.73943604138302987 ) ) ;
#11269 = ORIENTED_EDGE ( 'NONE', *, *, #58523, .F. ) ;
#11270 = CARTESIAN_POINT ( 'NONE',  ( 4.967162193818130511, -40.65506779172153529, -14.26841313271325795 ) ) ;
#11271 = B_SPLINE_CURVE_WITH_KNOTS ( 'NONE', 3,
 ( #37660, #47654, #18859, #33265, #57033, #5628, #42360, #61414, #9429, #38277, #18532, #13852, #32956, #9124, #5021, #24146 ),
 .UNSPECIFIED., .F., .F.,
 ( 4, 3, 3, 3, 3, 4 ),
 ( 6.939740885162003740E-18, 0.0002732102107931890238, 0.0004098135523333774140, 0.0005464168938824980580, 0.0008195847345945439857, 0.001092771384553105915 ),
 .UNSPECIFIED. ) ;
#11272 = ORIENTED_EDGE ( 'NONE', *, *, #27943, .F. ) ;
#11273 = CARTESIAN_POINT ( 'NONE',  ( 4.553261556744873317, -29.36425772793689859, 32.66925058691941075 ) ) ;
#11274 = ORIENTED_EDGE ( 'NONE', *, *, #38482, .F. ) ;
#11275 = CARTESIAN_POINT ( 'NONE',  ( 4.303969348037246512, -35.51084504003219422, 32.45857549159289590 ) ) ;
#11276 = DIRECTION ( 'NONE',  ( 1.000000000000000000, 0.000000000000000000, 0.000000000000000000 ) ) ;
#11277 = ORIENTED_EDGE ( 'NONE', *, *, #22140, .F. ) ;
#11278 = B_SPLINE_CURVE_WITH_KNOTS ( 'NONE', 3,
 ( #1855, #25060, #53545, #58868, #35098, #15060 ),
 .UNSPECIFIED., .F., .F.,
 ( 4, 2, 4 ),
 ( 3.496446946337351263E-18, 0.0002450742804987318451, 0.0004901485609974602208 ),
 .UNSPECIFIED. ) ;
#11279 = EDGE_CURVE ( 'NONE', #51719, #18847, #19902, .T. ) ;
#11280 = ORIENTED_EDGE ( 'NONE', *, *, #15254, .T. ) ;
#11281 = DIRECTION ( 'NONE',  ( 1.000000000000000000, 0.000000000000000000, 0.000000000000000000 ) ) ;
#11282 = CARTESIAN_POINT ( 'NONE',  ( 0.09136607875274982415, 0.000000000000000000, 0.000000000000000000 ) ) ;
#11283 = ORIENTED_EDGE ( 'NONE', *, *, #59034, .T. ) ;
#11284 = EDGE_LOOP ( 'NONE', ( #50019, #41346, #21219, #36060 ) ) ;
#11285 = CARTESIAN_POINT ( 'NONE',  ( 0.7044674535453004927, 43.87480159924536594, -22.06364673932585774 ) ) ;
#11286 = CARTESIAN_POINT ( 'NONE',  ( 0.3676999524040366896, -35.84016207189403502, -25.71834687500748373 ) ) ;
#11287 = CARTESIAN_POINT ( 'NONE',  ( 0.6017667736363749853, 23.75082673020805402, 41.83584368312199331 ) ) ;
#11288 = CARTESIAN_POINT ( 'NONE',  ( 1.000433927950260538, -18.23650333253261024, -37.73391874501472643 ) ) ;
#11289 = EDGE_LOOP ( 'NONE', ( #41003, #21347, #35177, #1631 ) ) ;
#11290 = CARTESIAN_POINT ( 'NONE',  ( 1.227938101723756947, 25.45152231597106507, -34.55893248994479450 ) ) ;
#11291 = DIRECTION ( 'NONE',  ( 0.000000000000000000, 0.000000000000000000, -1.000000000000000000 ) ) ;
#11292 = ORIENTED_EDGE ( 'NONE', *, *, #22869, .T. ) ;
#11293 = FACE_OUTER_BOUND ( 'NONE', #17447, .T. ) ;
#11294 = VERTEX_POINT ( 'NONE', #57132 ) ;
#11295 = CARTESIAN_POINT ( 'NONE',  ( 0.8560838555295223751, -46.73345513967318965, 4.044379407262076676 ) ) ;
#11296 = CARTESIAN_POINT ( 'NONE',  ( 2.282816707992306515, 28.91046591422454881, 37.02272176691533190 ) ) ;
#11297 = ORIENTED_EDGE ( 'NONE', *, *, #36344, .T. ) ;
#11298 = CARTESIAN_POINT ( 'NONE',  ( 0.8560838555295158248, -30.97734773434503808, 35.22466126774251194 ) ) ;
#11299 = B_SPLINE_CURVE_WITH_KNOTS ( 'NONE', 3,
 ( #24246, #57126, #37450, #56520 ),
 .UNSPECIFIED., .F., .F.,
 ( 4, 4 ),
 ( 7.152448122690996019E-18, 0.005013413432710144176 ),
 .UNSPECIFIED. ) ;
#11300 = CARTESIAN_POINT ( 'NONE',  ( -2.601141883200665639, 4.732256851928614338, 14.15631211003640288 ) ) ;
#11301 = CARTESIAN_POINT ( 'NONE',  ( 53.14993166107466749, 12.49998551214889808, -0.1744414439710397502 ) ) ;
#11302 = CARTESIAN_POINT ( 'NONE',  ( -18.24799997550736919, -12.32233744059949565, -2.099999999999997424 ) ) ;
#11303 = B_SPLINE_CURVE_WITH_KNOTS ( 'NONE', 3,
 ( #38982, #23625, #15163, #34271 ),
 .UNSPECIFIED., .F., .F.,
 ( 4, 4 ),
 ( 0.000000000000000000, 0.004050076154993000749 ),
 .UNSPECIFIED. ) ;
#11304 = EDGE_LOOP ( 'NONE', ( #35503, #30359, #33177, #61699 ) ) ;
#11305 = CARTESIAN_POINT ( 'NONE',  ( 4.967162193818130511, 0.000000000000000000, 0.000000000000000000 ) ) ;
#11306 = ORIENTED_EDGE ( 'NONE', *, *, #3308, .T. ) ;
#11307 = EDGE_CURVE ( 'NONE', #34476, #50243, #54047, .T. ) ;
#11308 = DIRECTION ( 'NONE',  ( 0.9848077530122079093, 0.1736481776669315802, -5.551115123125782086E-17 ) ) ;
#11309 = CARTESIAN_POINT ( 'NONE',  ( 0.9787464366903565471, 41.55793433844984008, -5.410368417358930593 ) ) ;
#11310 = AXIS2_PLACEMENT_3D ( 'NONE', #46254, #52157, #50921 ) ;
#11311 = ADVANCED_FACE ( 'NONE', ( #8292 ), #56746, .T. ) ;
#11312 = CARTESIAN_POINT ( 'NONE',  ( 5.896782393890504181, 17.94821721415871352, -9.076760749925545824 ) ) ;
#11313 = CARTESIAN_POINT ( 'NONE',  ( 0.3676999524040366896, -7.853951980431815194, -43.40813312746713848 ) ) ;
#11314 = EDGE_CURVE ( 'NONE', #37400, #59114, #5843, .T. ) ;
#11315 = CARTESIAN_POINT ( 'NONE',  ( -6.077587904424778920, 18.62472241188249811, 4.890371813497665698 ) ) ;
#11316 = CARTESIAN_POINT ( 'NONE',  ( 1.227938101723756947, 15.63977281655895979, -39.96870412324319943 ) ) ;
#11317 = CARTESIAN_POINT ( 'NONE',  ( 4.956445790444006683, -23.10347171912805564, -41.03373788315033721 ) ) ;
#11318 = CARTESIAN_POINT ( 'NONE',  ( 0.8760168074887076939, -23.27577685234627225, 42.09738177923915003 ) ) ;
#11319 = DIRECTION ( 'NONE',  ( 1.000000000000000000, 1.836909530733573776E-16, 0.000000000000000000 ) ) ;
#11320 = VECTOR ( 'NONE', #18037, 1000.000000000000114 ) ;
#11321 = B_SPLINE_CURVE_WITH_KNOTS ( 'NONE', 3,
 ( #5967, #20417, #35455, #58596 ),
 .UNSPECIFIED., .F., .F.,
 ( 4, 4 ),
 ( 0.000000000000000000, 0.004444103432399266161 ),
 .UNSPECIFIED. ) ;
#11322 = CARTESIAN_POINT ( 'NONE',  ( 0.5797568665920715958, -7.179076188124985158, 46.34313513010278740 ) ) ;
#11323 = ADVANCED_FACE ( 'NONE', ( #38084 ), #16901, .F. ) ;
#11324 = DIRECTION ( 'NONE',  ( -1.718001593797181987E-16, 1.000000000000000000, 0.000000000000000000 ) ) ;
#11325 = CARTESIAN_POINT ( 'NONE',  ( 0.6028777368367060907, -45.55110310871040014, 18.34766565235772262 ) ) ;
#11326 = ORIENTED_EDGE ( 'NONE', *, *, #20245, .F. ) ;
#11327 = CARTESIAN_POINT ( 'NONE',  ( -69.95594261585600293, 0.000000000000000000, 0.000000000000000000 ) ) ;
#11328 = DIRECTION ( 'NONE',  ( 1.000000000000000000, 0.000000000000000000, 0.000000000000000000 ) ) ;
#11329 = CARTESIAN_POINT ( 'NONE',  ( 4.975610109902397937, -44.31543648230385202, -20.70245146161840211 ) ) ;
#11330 = ORIENTED_EDGE ( 'NONE', *, *, #33591, .F. ) ;
#11331 = ADVANCED_FACE ( 'NONE', ( #23039 ), #60862, .F. ) ;
#11332 = CARTESIAN_POINT ( 'NONE',  ( -6.078726893082806448, -18.90026279491055305, -3.684305572565921949 ) ) ;
#11333 = CARTESIAN_POINT ( 'NONE',  ( 0.1073791018717483448, -39.65380858626227223, 16.95003405440244038 ) ) ;
#11334 = B_SPLINE_CURVE_WITH_KNOTS ( 'NONE', 3,
 ( #40266, #29592, #24915, #59016, #16127, #53997 ),
 .UNSPECIFIED., .F., .F.,
 ( 4, 2, 4 ),
 ( 8.131516293641283255E-19, 0.0002293801035737095075, 0.0004587602071474182019 ),
 .UNSPECIFIED. ) ;
#11335 = ADVANCED_FACE ( 'NONE', ( #43081 ), #60642, .F. ) ;
#11336 = CARTESIAN_POINT ( 'NONE',  ( 0.6017667736363749853, -12.11362382130104187, -46.55748817282771057 ) ) ;
#11337 = ORIENTED_EDGE ( 'NONE', *, *, #53081, .F. ) ;
#11338 = CARTESIAN_POINT ( 'NONE',  ( 4.303969348037246512, -27.54579249306183542, -39.44373910178637743 ) ) ;
#11339 = CARTESIAN_POINT ( 'NONE',  ( -2.739355103387247858, 14.08251715046641905, 4.952805029257269176 ) ) ;
#11341 = ORIENTED_EDGE ( 'NONE', *, *, #44443, .F. ) ;
#11340 =( BOUNDED_SURFACE ( )  B_SPLINE_SURFACE ( 3, 1, ( 
 ( #49709, #2700 ),
 ( #6766, #45046 ),
 ( #2074, #6451 ),
 ( #30912, #25911 ) ),
 .UNSPECIFIED., .F., .F., .F. ) 
 B_SPLINE_SURFACE_WITH_KNOTS ( ( 4, 4 ),
 ( 2, 2 ),
 ( 0.000000000000000000, 1.000000000000000000 ),
 ( 0.000000000000000000, 1.000000000000000000 ),
 .UNSPECIFIED. ) 
 GEOMETRIC_REPRESENTATION_ITEM ( )  RATIONAL_B_SPLINE_SURFACE ( (
 ( 1.000000000000000000, 1.000000000000000000),
 ( 0.9754377213608244057, 0.9999580625633939235),
 ( 0.9754377213608244057, 0.9999580625633939235),
 ( 1.000000000000000000, 1.000000000000000000) ) ) 
 REPRESENTATION_ITEM ( '' )  SURFACE ( )  );
#11342 = CARTESIAN_POINT ( 'NONE',  ( -6.010958268070873523, 14.94067681728565589, -11.48268200989181942 ) ) ;
#11343 = VERTEX_POINT ( 'NONE', #23955 ) ;
#11344 = ORIENTED_EDGE ( 'NONE', *, *, #24038, .T. ) ;
#11345 = CARTESIAN_POINT ( 'NONE',  ( 1.227938101723748288, 25.45152231597057124, 34.55893248994515687 ) ) ;
#11346 = ORIENTED_EDGE ( 'NONE', *, *, #46344, .F. ) ;
#11347 = DIRECTION ( 'NONE',  ( -1.000000000000000000, -0.000000000000000000, -0.000000000000000000 ) ) ;
#11348 = EDGE_CURVE ( 'NONE', #6280, #5698, #117, .T. ) ;
#11349 = VECTOR ( 'NONE', #57819, 1000.000000000000000 ) ;
#11350 = CARTESIAN_POINT ( 'NONE',  ( 0.5987334363312691865, 46.79309011824572906, -14.89864502757918174 ) ) ;
#11351 = VERTEX_POINT ( 'NONE', #8929 ) ;
#11352 = CARTESIAN_POINT ( 'NONE',  ( 0.8560838555295158248, 36.24009790160309308, 29.78301761346479282 ) ) ;
#11353 = CARTESIAN_POINT ( 'NONE',  ( 0.9762797500689124330, 41.59901070109194876, 5.084003725032276932 ) ) ;
#11354 = ORIENTED_EDGE ( 'NONE', *, *, #16843, .F. ) ;
#11355 =( BOUNDED_SURFACE ( )  B_SPLINE_SURFACE ( 3, 1, ( 
 ( #17800, #32211 ),
 ( #26257, #36001 ),
 ( #3668, #16886 ),
 ( #60683, #26885 ) ),
 .UNSPECIFIED., .F., .F., .F. ) 
 B_SPLINE_SURFACE_WITH_KNOTS ( ( 4, 4 ),
 ( 2, 2 ),
 ( 0.000000000000000000, 1.000000000000000000 ),
 ( 0.000000000000000000, 1.000000000000000000 ),
 .UNSPECIFIED. ) 
 GEOMETRIC_REPRESENTATION_ITEM ( )  RATIONAL_B_SPLINE_SURFACE ( (
 ( 1.000000000000000000, 1.000000000000000000),
 ( 0.7269869731126817891, 0.9931720237060910339),
 ( 0.7269869731126817891, 0.9931720237060910339),
 ( 1.000000000000000000, 1.000000000000000000) ) ) 
 REPRESENTATION_ITEM ( '' )  SURFACE ( )  );
#11356 = CARTESIAN_POINT ( 'NONE',  ( 0.1129192098497447394, 43.40062318508790895, 7.958498283669150020 ) ) ;
#11357 = CARTESIAN_POINT ( 'NONE',  ( 4.962356264823609031, -3.779019546646985361, -41.91604238389410853 ) ) ;
#11358 = CARTESIAN_POINT ( 'NONE',  ( -2.708315649062910779, 9.116606751444328083, -11.44805714186562895 ) ) ;
#11359 = CARTESIAN_POINT ( 'NONE',  ( 4.549368137175248350, 13.59764261105693350, 40.71620287708348940 ) ) ;
#11360 = EDGE_LOOP ( 'NONE', ( #21861, #38864, #16290, #39729 ) ) ;
#11361 =( BOUNDED_SURFACE ( )  B_SPLINE_SURFACE ( 3, 1, ( 
 ( #6874, #26013 ),
 ( #45148, #2178 ),
 ( #7817, #55730 ),
 ( #21314, #40445 ) ),
 .UNSPECIFIED., .F., .F., .F. ) 
 B_SPLINE_SURFACE_WITH_KNOTS ( ( 4, 4 ),
 ( 2, 2 ),
 ( 0.000000000000000000, 1.000000000000000000 ),
 ( 0.000000000000000000, 1.000000000000000000 ),
 .UNSPECIFIED. ) 
 GEOMETRIC_REPRESENTATION_ITEM ( )  RATIONAL_B_SPLINE_SURFACE ( (
 ( 1.000000000000000000, 1.000000000000000000),
 ( 0.9953485035131437453, 0.8621029689291523912),
 ( 0.9953485035131437453, 0.8621029689291523912),
 ( 1.000000000000000000, 1.000000000000000000) ) ) 
 REPRESENTATION_ITEM ( '' )  SURFACE ( )  );
#11362 = VECTOR ( 'NONE', #58096, 1000.000000000000000 ) ;
#11363 = ORIENTED_EDGE ( 'NONE', *, *, #22362, .F. ) ;
#11364 = CARTESIAN_POINT ( 'NONE',  ( 1.227938101723748288, -0.8460948827228147451, 42.91134962331487657 ) ) ;
#11365 = B_SPLINE_CURVE_WITH_KNOTS ( 'NONE', 3,
 ( #10268, #61928, #854, #52233, #19362, #9961, #48177, #19068, #5231, #53161, #29360, #24669, #24362, #24985, #39102, #33781 ),
 .UNSPECIFIED., .F., .F.,
 ( 4, 3, 3, 3, 3, 4 ),
 ( 1.214354834101861570E-17, 0.0002724568934985572275, 0.0004086836638483815022, 0.0005449104342063627177, 0.0008173270854453656975, 0.001089761613562685756 ),
 .UNSPECIFIED. ) ;
#11366 = CARTESIAN_POINT ( 'NONE',  ( 0.8751705887134553219, 29.98056538504910051, 37.60752970653838645 ) ) ;
#11367 = ORIENTED_EDGE ( 'NONE', *, *, #173, .T. ) ;
#11368 = CARTESIAN_POINT ( 'NONE',  ( 0.6846871229502932144, 41.05093867799185858, 24.69859318104503032 ) ) ;
#11369 = CARTESIAN_POINT ( 'NONE',  ( 0.8744876279028263033, 48.01195819035220325, 10.25679877483054625 ) ) ;
#11370 = CARTESIAN_POINT ( 'NONE',  ( 2.533389852662419894, 8.245621584460703701, -43.23725542191009197 ) ) ;
#11371 = CARTESIAN_POINT ( 'NONE',  ( 0.8751705887134423323, 41.19904111682474479, 24.81530984069222256 ) ) ;
#11372 = EDGE_CURVE ( 'NONE', #9240, #37569, #25661, .T. ) ;
#11373 = VERTEX_POINT ( 'NONE', #23340 ) ;
#11374 = ORIENTED_EDGE ( 'NONE', *, *, #41591, .F. ) ;
#11375 = CARTESIAN_POINT ( 'NONE',  ( 4.956653778116992370, 26.26162724282429650, -40.28700667097652399 ) ) ;
#11376 = CARTESIAN_POINT ( 'NONE',  ( 1.479689385636123067, 42.17416015216831227, 12.76417097687706104 ) ) ;
#11377 = EDGE_CURVE ( 'NONE', #30700, #21629, #18345, .T. ) ;
#11378 = CARTESIAN_POINT ( 'NONE',  ( 0.9789889208857693870, 14.97250939922353297, -39.14280087490587334 ) ) ;
#11379 = CARTESIAN_POINT ( 'NONE',  ( 0.8560838555295158248, 44.99141268455571208, 13.27198623905747432 ) ) ;
#11380 = CARTESIAN_POINT ( 'NONE',  ( -5.720000000000002416, 15.72000000000000064, 0.000000000000000000 ) ) ;
#11381 = ADVANCED_FACE ( 'NONE', ( #18647 ), #56833, .T. ) ;
#11382 = CARTESIAN_POINT ( 'NONE',  ( 3.270143674763207553, 13.53222904135354199, 2.058141141425647191 ) ) ;
#11383 = CARTESIAN_POINT ( 'NONE',  ( 2.359973842542475886, -13.96544505891846200, -41.75047591272259240 ) ) ;
#11384 = CARTESIAN_POINT ( 'NONE',  ( 0.6001305935487422083, -29.70149728382410714, -37.84751346122845206 ) ) ;
#11385 = EDGE_CURVE ( 'NONE', #61878, #43179, #4006, .T. ) ;
#11386 = CARTESIAN_POINT ( 'NONE',  ( 0.3622758884714730732, -6.444611261694294768, -42.62881903538208661 ) ) ;
#11387 = EDGE_CURVE ( 'NONE', #15844, #1609, #1018, .T. ) ;
#11388 = CARTESIAN_POINT ( 'NONE',  ( 0.1129192098497447394, 15.69290830752478882, 41.23935519181615206 ) ) ;
#11389 = B_SPLINE_CURVE_WITH_KNOTS ( 'NONE', 3,
 ( #11440, #54015, #6083, #49959, #2012, #7012, #35572, #16442, #59338, #34951, #15837, #54629, #49331, #30841, #25221, #26146 ),
 .UNSPECIFIED., .F., .F.,
 ( 4, 3, 3, 3, 3, 4 ),
 ( 1.962735358247463844E-17, 0.0002612764279487719702, 0.0003919131003184767514, 0.0005225497727000664484, 0.0007837925190632497995, 0.001045051706266717818 ),
 .UNSPECIFIED. ) ;
#11390 = CARTESIAN_POINT ( 'NONE',  ( 0.9762797500689124330, 15.53330887509137703, -38.92352888134260525 ) ) ;
#11391 = CARTESIAN_POINT ( 'NONE',  ( 4.975610109902397937, 0.9924324126403755164, 48.90260202733708894 ) ) ;
#11392 = CARTESIAN_POINT ( 'NONE',  ( -5.995132425357893702, -14.95525565067266882, -11.46484027925383309 ) ) ;
#11393 = CARTESIAN_POINT ( 'NONE',  ( 0.8551540677456715978, -47.61725548905986471, -5.348818140991393300 ) ) ;
#11394 = CARTESIAN_POINT ( 'NONE',  ( 0.2999999999999897193, -13.49666625504239192, 0.000000000000000000 ) ) ;
#11395 = CARTESIAN_POINT ( 'NONE',  ( 5.959547316686252039, -20.35048796920735015, -2.675599016784462769 ) ) ;
#11396 = CONTEXT_DEPENDENT_SHAPE_REPRESENTATION ( #1223, #34892 ) ;
#11397 = CARTESIAN_POINT ( 'NONE',  ( 0.9780303403264752893, -22.27669849432558991, 35.49772270988660239 ) ) ;
#11398 = CARTESIAN_POINT ( 'NONE',  ( 4.549368137175248350, 8.166781970325150297, 42.14271863032836762 ) ) ;
#11399 = EDGE_CURVE ( 'NONE', #60643, #40797, #24254, .T. ) ;
#11400 = CARTESIAN_POINT ( 'NONE',  ( 3.407937589446178528, 13.34359005742689241, 3.099921468255050439 ) ) ;
#11401 = CARTESIAN_POINT ( 'NONE',  ( 0.5786265663353153954, -24.57327059187369400, -41.11783955080264974 ) ) ;
#11403 = ORIENTED_EDGE ( 'NONE', *, *, #44639, .T. ) ;
#11402 = DIRECTION ( 'NONE',  ( -1.000000000000000000, -0.000000000000000000, -0.000000000000000000 ) ) ;
#11404 = ORIENTED_EDGE ( 'NONE', *, *, #45028, .T. ) ;
#11405 = PLANE ( 'NONE',  #61848 ) ;
#11406 = CARTESIAN_POINT ( 'NONE',  ( 0.9268187852002115479, 43.92278549089876805, -3.813561016834528417 ) ) ;
#11407 = CARTESIAN_POINT ( 'NONE',  ( 0.1158816050234199313, 41.87808310636262377, 13.89849620073145431 ) ) ;
#11408 = ORIENTED_EDGE ( 'NONE', *, *, #6796, .T. ) ;
#11409 = VERTEX_POINT ( 'NONE', #34286 ) ;
#11410 = CARTESIAN_POINT ( 'NONE',  ( 0.7242003506640025678, 36.85244696242455831, -32.44855662441259625 ) ) ;
#11412 = CARTESIAN_POINT ( 'NONE',  ( 0.3622758884714730732, -15.73321244754880688, 40.13994584881756111 ) ) ;
#11411 = COLOUR_RGB ( '', 0.72549020, 0.75294118, 0.79215686) ;
#11413 = DIRECTION ( 'NONE',  ( 0.000000000000000000, 0.000000000000000000, 1.000000000000000000 ) ) ;
#11414 = B_SPLINE_CURVE_WITH_KNOTS ( 'NONE', 3,
 ( #20554, #26474, #40306, #6719 ),
 .UNSPECIFIED., .F., .F.,
 ( 4, 4 ),
 ( 1.084202172485504434E-19, 0.004446298630425104051 ),
 .UNSPECIFIED. ) ;
#11415 = EDGE_CURVE ( 'NONE', #31002, #49359, #34665, .T. ) ;
#11416 = ORIENTED_EDGE ( 'NONE', *, *, #45528, .T. ) ;
#11417 = VERTEX_POINT ( 'NONE', #431 ) ;
#11418 = CARTESIAN_POINT ( 'NONE',  ( -6.057079549204054558, -18.90348671888457588, -3.672794708215112003 ) ) ;
#11419 = B_SPLINE_CURVE_WITH_KNOTS ( 'NONE', 3,
 ( #47428, #28312, #14543, #53032, #716, #47131 ),
 .UNSPECIFIED., .F., .F.,
 ( 4, 2, 4 ),
 ( 1.084202172485504434E-19, 0.0002445244328975358303, 0.0004890488657950715521 ),
 .UNSPECIFIED. ) ;
#11420 = CARTESIAN_POINT ( 'NONE',  ( 0.7044674535452954967, 43.87480159924503198, 22.06364673932647591 ) ) ;
#11421 = CARTESIAN_POINT ( 'NONE',  ( 1.231276596079881935, 41.65019306089989470, -4.747440258479600494 ) ) ;
#11422 = EDGE_LOOP ( 'NONE', ( #12867, #2761, #46049, #39710 ) ) ;
#11423 = CARTESIAN_POINT ( 'NONE',  ( 0.2279481005628795909, -2.172801660577914351, 44.06566032657064369 ) ) ;
#11424 = EDGE_CURVE ( 'NONE', #6671, #9409, #51842, .T. ) ;
#11425 = CARTESIAN_POINT ( 'NONE',  ( -6.016104459813374383, 18.84322058118302223, 0.005335450885132661872 ) ) ;
#11426 = EDGE_CURVE ( 'NONE', #28284, #884, #39614, .T. ) ;
#11427 = CARTESIAN_POINT ( 'NONE',  ( 0.1368894036331281816, 43.98715317849343620, -3.462900688019952877 ) ) ;
#11428 = ORIENTED_EDGE ( 'NONE', *, *, #3675, .F. ) ;
#11429 = ORIENTED_EDGE ( 'NONE', *, *, #44450, .F. ) ;
#11430 = CARTESIAN_POINT ( 'NONE',  ( 0.7056759521544992975, 27.13777475669688144, 38.25297387618083178 ) ) ;
#11431 = CARTESIAN_POINT ( 'NONE',  ( 4.956653778116975495, 20.77844580450561551, 43.37017594958062006 ) ) ;
#11432 = ORIENTED_EDGE ( 'NONE', *, *, #32084, .F. ) ;
#11433 = CARTESIAN_POINT ( 'NONE',  ( 0.5839880159502333079, 44.26747004398443863, -18.28706857028324961 ) ) ;
#11434 = CARTESIAN_POINT ( 'NONE',  ( 0.6016118706126976079, -8.181234200593557659, 48.42126043112642009 ) ) ;
#11435 = CARTESIAN_POINT ( 'NONE',  ( 0.5980271706414734822, -38.93680501037979980, 29.93283244909049756 ) ) ;
#11436 = CARTESIAN_POINT ( 'NONE',  ( 4.553261556744875094, -43.82122302957815663, -3.039733214544628748 ) ) ;
#11437 = AXIS2_PLACEMENT_3D ( 'NONE', #28649, #19579, #121 ) ;
#11438 = VERTEX_POINT ( 'NONE', #44619 ) ;
#11439 = CARTESIAN_POINT ( 'NONE',  ( 0.9756008150404608115, -30.44122083654196587, -30.24019526051575468 ) ) ;
#11440 = CARTESIAN_POINT ( 'NONE',  ( 0.5997462898726536595, -35.63787911784795170, 33.78599121123970406 ) ) ;
#11441 =( BOUNDED_SURFACE ( )  B_SPLINE_SURFACE ( 3, 1, ( 
 ( #53902, #35142 ),
 ( #53291, #19811 ),
 ( #20724, #38931 ),
 ( #57984, #1586 ) ),
 .UNSPECIFIED., .F., .F., .F. ) 
 B_SPLINE_SURFACE_WITH_KNOTS ( ( 4, 4 ),
 ( 2, 2 ),
 ( 0.000000000000000000, 1.000000000000000000 ),
 ( 0.000000000000000000, 1.000000000000000000 ),
 .UNSPECIFIED. ) 
 GEOMETRIC_REPRESENTATION_ITEM ( )  RATIONAL_B_SPLINE_SURFACE ( (
 ( 1.000000000000000000, 1.000000000000000000),
 ( 0.9953485035131437453, 0.8621029689291523912),
 ( 0.9953485035131437453, 0.8621029689291523912),
 ( 1.000000000000000000, 1.000000000000000000) ) ) 
 REPRESENTATION_ITEM ( '' )  SURFACE ( )  );
#11442 = CARTESIAN_POINT ( 'NONE',  ( 3.661921753701998128, 12.72740550795439418, 45.28403993539147621 ) ) ;
#11443 = CIRCLE ( 'NONE', #54432, 2.649999999999985700 ) ;
#11444 = ORIENTED_EDGE ( 'NONE', *, *, #22963, .F. ) ;
#11445 = DIRECTION ( 'NONE',  ( 0.000000000000000000, 0.000000000000000000, -1.000000000000000000 ) ) ;
#11446 = ORIENTED_EDGE ( 'NONE', *, *, #51680, .F. ) ;
#11447 = FACE_OUTER_BOUND ( 'NONE', #41785, .T. ) ;
#11448 = SURFACE_STYLE_FILL_AREA ( #54325 ) ;
#11449 = VERTEX_POINT ( 'NONE', #10163 ) ;
#11450 = CARTESIAN_POINT ( 'NONE',  ( 5.895596859100789899, 0.6756533542673609505, 20.10153416427101192 ) ) ;
#11451 = LINE ( 'NONE', #2962, #15706 ) ;
#11452 = EDGE_CURVE ( 'NONE', #52461, #48862, #22021, .T. ) ;
#11453 = DIRECTION ( 'NONE',  ( -1.000000000000000000, -0.000000000000000000, -0.000000000000000000 ) ) ;
#11454 = AXIS2_PLACEMENT_3D ( 'NONE', #1233, #39492, #50101 ) ;
#11455 = EDGE_CURVE ( 'NONE', #34186, #39947, #26432, .T. ) ;
#11456 = CARTESIAN_POINT ( 'NONE',  ( 0.6029303876144825880, -41.72757124235838688, 23.94027529185480319 ) ) ;
#11457 = CARTESIAN_POINT ( 'NONE',  ( 2.359973842542476330, 21.68887420214251094, 38.31094661420071645 ) ) ;
#11458 =( BOUNDED_SURFACE ( )  B_SPLINE_SURFACE ( 3, 1, ( 
 ( #40708, #51293 ),
 ( #32216, #22805 ),
 ( #41936, #60373 ),
 ( #8376, #59780 ) ),
 .UNSPECIFIED., .F., .F., .F. ) 
 B_SPLINE_SURFACE_WITH_KNOTS ( ( 4, 4 ),
 ( 2, 2 ),
 ( 0.000000000000000000, 1.000000000000000000 ),
 ( 0.000000000000000000, 1.000000000000000000 ),
 .UNSPECIFIED. ) 
 GEOMETRIC_REPRESENTATION_ITEM ( )  RATIONAL_B_SPLINE_SURFACE ( (
 ( 1.000000000000000000, 1.000000000000000000),
 ( 0.9729067724841187204, 0.9999501103223794596),
 ( 0.9729067724841187204, 0.9999501103223794596),
 ( 1.000000000000000000, 1.000000000000000000) ) ) 
 REPRESENTATION_ITEM ( '' )  SURFACE ( )  );
#11459 = CARTESIAN_POINT ( 'NONE',  ( 4.975801465491694664, -2.564218696447152279, -47.84403947906842092 ) ) ;
#11460 = FACE_OUTER_BOUND ( 'NONE', #46351, .T. ) ;
#11461 = CARTESIAN_POINT ( 'NONE',  ( 0.1073791018717578927, -41.52698815987159264, -11.62916352156135780 ) ) ;
#11462 = CARTESIAN_POINT ( 'NONE',  ( 2.648799415243708655, -15.27490784895023879, -46.59607980823791706 ) ) ;
#11463 = EDGE_CURVE ( 'NONE', #34962, #26589, #224, .T. ) ;
#11464 = LINE ( 'NONE', #24325, #24673 ) ;
#11465 = ADVANCED_FACE ( 'NONE', ( #28958 ), #38773, .F. ) ;
#11466 = CARTESIAN_POINT ( 'NONE',  ( 0.8557997880470690211, 47.89938907511594124, -0.9121262075947851322 ) ) ;
#11467 = ORIENTED_EDGE ( 'NONE', *, *, #8204, .F. ) ;
#11468 = B_SPLINE_CURVE_WITH_KNOTS ( 'NONE', 3,
 ( #30364, #1854, #49477, #51318, #27526, #4611, #27838, #52243, #41965, #13140, #36636, #3696, #56327, #32552, #46347, #51630, #37566, #56641, #9032 ),
 .UNSPECIFIED., .F., .F.,
 ( 4, 3, 3, 3, 3, 3, 4 ),
 ( 9.813676791237319219E-18, 0.0002724573126191794418, 0.0004086839781548490193, 0.0005449106435901815947, 0.0006811373090491476632, 0.0008459866663933731691, 0.001010840725717210764 ),
 .UNSPECIFIED. ) ;
#11469 = ADVANCED_FACE ( 'NONE', ( #751 ), #21891, .F. ) ;
#11470 = CARTESIAN_POINT ( 'NONE',  ( -2.708315649062916552, -13.61924161399630329, -5.356004933109414168 ) ) ;
#11471 = CARTESIAN_POINT ( 'NONE',  ( 4.833616638992208614, 2.572717262757989509, -46.17873762321151077 ) ) ;
#11472 = CARTESIAN_POINT ( 'NONE',  ( 4.967162193818130511, -3.259922920617460029, -42.96271701169388280 ) ) ;
#11473 = CARTESIAN_POINT ( 'NONE',  ( 5.838029081930957709, 30.48039787783066146, -36.08338126287580394 ) ) ;
#11474 = DIRECTION ( 'NONE',  ( 0.000000000000000000, 0.000000000000000000, 1.000000000000000000 ) ) ;
#11475 = CARTESIAN_POINT ( 'NONE',  ( 0.8554163680231816613, 23.34472558242442375, 40.69679668712412735 ) ) ;
#11476 = EDGE_CURVE ( 'NONE', #10038, #51030, #48090, .T. ) ;
#11477 = CARTESIAN_POINT ( 'NONE',  ( 0.6017667736363749853, 41.83584368312190804, -23.75082673020819968 ) ) ;
#11478 = CARTESIAN_POINT ( 'NONE',  ( 0.5804410086790514622, -19.24447200597920826, -42.76879877979365574 ) ) ;
#11480 = EDGE_LOOP ( 'NONE', ( #41869, #15061, #56804, #28213 ) ) ;
#11479 = CARTESIAN_POINT ( 'NONE',  ( 0.08486401232817714080, 0.000000000000000000, 0.000000000000000000 ) ) ;
#11481 = ORIENTED_EDGE ( 'NONE', *, *, #61934, .F. ) ;
#11482 = CARTESIAN_POINT ( 'NONE',  ( 4.956653778116991482, -9.917440902360828758, -47.05699031914960528 ) ) ;
#11483 = LINE ( 'NONE', #49377, #28508 ) ;
#11484 = CARTESIAN_POINT ( 'NONE',  ( 0.1095718737110178281, 16.26534146842150719, 39.93945841550381459 ) ) ;
#11485 = ORIENTED_EDGE ( 'NONE', *, *, #16894, .T. ) ;
#11486 = CARTESIAN_POINT ( 'NONE',  ( 0.1157991065609915715, -22.94322095412508133, 37.69019736997796599 ) ) ;
#11487 = CARTESIAN_POINT ( 'NONE',  ( 5.901463166500146684, 3.359582080288941341, 19.83005493150329457 ) ) ;
#11488 = CARTESIAN_POINT ( 'NONE',  ( 0.1081432562775997280, 41.76274004527633110, -10.75186376283298806 ) ) ;
#11489 = B_SPLINE_CURVE_WITH_KNOTS ( 'NONE', 3,
 ( #48420, #38429, #6091, #57177, #43131, #9582 ),
 .UNSPECIFIED., .F., .F.,
 ( 4, 2, 4 ),
 ( 8.699011523299069796E-17, 0.0002293366620881468008, 0.0004586733241762066485 ),
 .UNSPECIFIED. ) ;
#11490 = ORIENTED_EDGE ( 'NONE', *, *, #5149, .F. ) ;
#11491 = ORIENTED_EDGE ( 'NONE', *, *, #33294, .F. ) ;
#11492 = AXIS2_PLACEMENT_3D ( 'NONE', #22551, #50428, #21934 ) ;
#11493 = CARTESIAN_POINT ( 'NONE',  ( 4.962356264823603702, 30.91935898304086550, -28.55221248765493414 ) ) ;
#11495 = CARTESIAN_POINT ( 'NONE',  ( 0.6039202388192952409, 48.23508111734889781, -9.216325865102767523 ) ) ;
#11494 = VECTOR ( 'NONE', #28571, 1000.000000000000114 ) ;
#11496 = CARTESIAN_POINT ( 'NONE',  ( 5.965394784446460541, 7.868087674480955584, -18.95742317323937343 ) ) ;
#11497 = ORIENTED_EDGE ( 'NONE', *, *, #10565, .F. ) ;
#11498 = VECTOR ( 'NONE', #40289, 1000.000000000000114 ) ;
#11499 = ORIENTED_EDGE ( 'NONE', *, *, #38028, .T. ) ;
#11500 = CARTESIAN_POINT ( 'NONE',  ( 0.8753041380234465318, -26.21158409634571740, 41.52217705074212972 ) ) ;
#11501 = CARTESIAN_POINT ( 'NONE',  ( 5.860006189529246790, 48.13093674595585014, -3.137522369585688864 ) ) ;
#11502 = ORIENTED_EDGE ( 'NONE', *, *, #5224, .T. ) ;
#11503 = EDGE_CURVE ( 'NONE', #31302, #60250, #45858, .T. ) ;
#11504 = LINE ( 'NONE', #49703, #1938 ) ;
#11505 = VERTEX_POINT ( 'NONE', #26408 ) ;
#11506 = CARTESIAN_POINT ( 'NONE',  ( 5.965394784446460541, -5.298374383010499677, -19.82972329408683976 ) ) ;
#11507 = CARTESIAN_POINT ( 'NONE',  ( 0.8560838555295158248, -46.85553835019179303, 2.220666565569249684 ) ) ;
#11508 = B_SPLINE_CURVE_WITH_KNOTS ( 'NONE', 3,
 ( #46887, #26829, #36556, #13057, #17741, #46568 ),
 .UNSPECIFIED., .F., .F.,
 ( 4, 2, 4 ),
 ( 1.870559545977334001E-17, 0.0002293319059085090867, 0.0004586638118169994709 ),
 .UNSPECIFIED. ) ;
#11509 = ORIENTED_EDGE ( 'NONE', *, *, #17141, .F. ) ;
#11510 = CARTESIAN_POINT ( 'NONE',  ( 0.7246131072078538793, 23.33689307364193866, 42.06185227555123873 ) ) ;
#11511 = CARTESIAN_POINT ( 'NONE',  ( 0.7948884756798512141, 11.76956421775548378, -47.66734734306368892 ) ) ;
#11512 = CARTESIAN_POINT ( 'NONE',  ( 1.231276596079881047, 5.037240371906286818, -41.61613846158368091 ) ) ;
#11513 = FACE_OUTER_BOUND ( 'NONE', #36912, .T. ) ;
#11514 = ORIENTED_EDGE ( 'NONE', *, *, #11463, .T. ) ;
#11515 = CARTESIAN_POINT ( 'NONE',  ( 2.526552050251863246, -42.96196914573630465, -1.212569781798380486 ) ) ;
#11516 = CARTESIAN_POINT ( 'NONE',  ( -2.569797478183790229, 7.701637110048681123, -12.44213550320645645 ) ) ;
#11517 = VERTEX_POINT ( 'NONE', #54272 ) ;
#11518 = CARTESIAN_POINT ( 'NONE',  ( 0.6000166863083106206, -30.20952222014405919, -38.71961065066481211 ) ) ;
#11519 = B_SPLINE_CURVE_WITH_KNOTS ( 'NONE', 3,
 ( #55512, #2267, #21397, #50818 ),
 .UNSPECIFIED., .F., .F.,
 ( 4, 4 ),
 ( 3.469446951953614189E-18, 0.004042984057420973693 ),
 .UNSPECIFIED. ) ;
#11520 = ORIENTED_EDGE ( 'NONE', *, *, #32118, .T. ) ;
#11521 = CARTESIAN_POINT ( 'NONE',  ( 1.088313998177382391, -36.76812638579213655, -22.12859469727376904 ) ) ;
#11522 = ORIENTED_EDGE ( 'NONE', *, *, #4496, .T. ) ;
#11523 = DIRECTION ( 'NONE',  ( 0.000000000000000000, 0.000000000000000000, 1.000000000000000000 ) ) ;
#11524 = CARTESIAN_POINT ( 'NONE',  ( 0.5997462898726536595, -31.02483596213004091, -38.06587952047387091 ) ) ;
#11526 = CARTESIAN_POINT ( 'NONE',  ( 4.291220156522059348, -45.68901888636781905, -11.48488356522702247 ) ) ;
#11525 = B_SPLINE_CURVE_WITH_KNOTS ( 'NONE', 3,
 ( #32899, #51975, #9067, #28174 ),
 .UNSPECIFIED., .F., .F.,
 ( 4, 4 ),
 ( 0.000000000000000000, 0.005004741218457413668 ),
 .UNSPECIFIED. ) ;
#11527 = ORIENTED_EDGE ( 'NONE', *, *, #34175, .F. ) ;
#11528 = CARTESIAN_POINT ( 'NONE',  ( 4.975801465491695552, 32.01766832630263337, 35.64402118370968964 ) ) ;
#11529 = CARTESIAN_POINT ( 'NONE',  ( 5.965394784446458765, -20.52536205633085231, 0.01447339372446240606 ) ) ;
#11530 = CARTESIAN_POINT ( 'NONE',  ( 0.000000000000000000, 0.000000000000000000, -5.600000000000000533 ) ) ;
#11531 = ORIENTED_EDGE ( 'NONE', *, *, #12516, .F. ) ;
#11532 = B_SPLINE_CURVE_WITH_KNOTS ( 'NONE', 3,
 ( #29170, #40082, #59130, #57967 ),
 .UNSPECIFIED., .F., .F.,
 ( 4, 4 ),
 ( 2.061695315165020171E-17, 0.004444306975806115029 ),
 .UNSPECIFIED. ) ;
#11533 = EDGE_CURVE ( 'NONE', #53953, #40503, #58591, .T. ) ;
#11534 = ORIENTED_EDGE ( 'NONE', *, *, #11503, .T. ) ;
#11535 = CARTESIAN_POINT ( 'NONE',  ( 0.9789889208857693870, -31.14606658136087347, -28.04028235506562083 ) ) ;
#11536 = CARTESIAN_POINT ( 'NONE',  ( 2.533389852662419894, 30.74453978043937141, 31.49958421031297817 ) ) ;
#11537 = CARTESIAN_POINT ( 'NONE',  ( 0.8560838555295223751, 27.08392101972057731, -38.29926965725677235 ) ) ;
#11538 = CARTESIAN_POINT ( 'NONE',  ( 0.1100053167205930216, -5.806749312984825551, -42.73174076921942799 ) ) ;
#11539 = CARTESIAN_POINT ( 'NONE',  ( 5.894904586330512508, 12.98452142685981769, -15.36006560458193704 ) ) ;
#11540 = B_SPLINE_CURVE_WITH_KNOTS ( 'NONE', 3,
 ( #5774, #24925, #39042, #28683 ),
 .UNSPECIFIED., .F., .F.,
 ( 4, 4 ),
 ( 0.000000000000000000, 0.004444103432399269631 ),
 .UNSPECIFIED. ) ;
#11542 = CIRCLE ( 'NONE', #2526, 47.91270532121795611 ) ;
#11541 = CARTESIAN_POINT ( 'NONE',  ( 0.9780106845699474416, 38.45963264927223690, 16.64896101678635532 ) ) ;
#11543 = ORIENTED_EDGE ( 'NONE', *, *, #53350, .T. ) ;
#11544 = EDGE_CURVE ( 'NONE', #28616, #55958, #7795, .T. ) ;
#11545 = B_SPLINE_CURVE_WITH_KNOTS ( 'NONE', 3,
 ( #28233, #61417, #18534, #18861 ),
 .UNSPECIFIED., .F., .F.,
 ( 4, 4 ),
 ( 2.168404344971008868E-19, 0.004048833967417088224 ),
 .UNSPECIFIED. ) ;
#11546 = CARTESIAN_POINT ( 'NONE',  ( 0.6067099128993235224, 6.954009037736147647, 47.38952184036235593 ) ) ;
#11547 = EDGE_CURVE ( 'NONE', #31462, #3804, #57720, .T. ) ;
#11548 = CARTESIAN_POINT ( 'NONE',  ( 5.896782393890504181, 5.952874097602427916, 19.21169895808557371 ) ) ;
#11549 = ORIENTED_EDGE ( 'NONE', *, *, #38288, .F. ) ;
#11550 = AXIS2_PLACEMENT_3D ( 'NONE', #51617, #51004, #13748 ) ;
#11551 = EDGE_CURVE ( 'NONE', #36543, #12367, #35332, .T. ) ;
#11552 = LINE ( 'NONE', #49746, #32374 ) ;
#11553 = CARTESIAN_POINT ( 'NONE',  ( 0.6029442701453591180, 44.28204046225096846, 21.22842711219661993 ) ) ;
#11554 = VECTOR ( 'NONE', #38590, 1000.000000000000000 ) ;
#11555 = CARTESIAN_POINT ( 'NONE',  ( 0.1156867017252034280, -42.71261242789667989, 11.07138414379485170 ) ) ;
#11556 = CARTESIAN_POINT ( 'NONE',  ( 5.981074661064941900, -18.96560215432011631, -7.846517100474756035 ) ) ;
#11557 = CARTESIAN_POINT ( 'NONE',  ( 4.694002226626921015, 32.50760209236001685, 31.96154842386279071 ) ) ;
#11558 =( NAMED_UNIT ( * ) SI_UNIT ( $, .STERADIAN. ) SOLID_ANGLE_UNIT ( ) );
#11559 = CARTESIAN_POINT ( 'NONE',  ( 5.895596859100789899, -13.98490190264553412, -14.45512718677593611 ) ) ;
#11560 = CARTESIAN_POINT ( 'NONE',  ( 0.6027444965799114707, 37.47717969856460485, -31.73325570641842575 ) ) ;
#11561 = CARTESIAN_POINT ( 'NONE',  ( 0.1073791018717578927, -41.77800844988522755, 10.69234304549982895 ) ) ;
#11562 = CARTESIAN_POINT ( 'NONE',  ( 0.1129192098497447394, -27.88830454350447852, -34.19348267541494124 ) ) ;
#11564 = ADVANCED_FACE ( 'NONE', ( #44934 ), #59924, .F. ) ;
#11563 = CARTESIAN_POINT ( 'NONE',  ( 0.08486401232817714080, 12.80000000000000071, 0.000000000000000000 ) ) ;
#11565 = CARTESIAN_POINT ( 'NONE',  ( 0.8557997880470697982, -13.27832040216607190, -46.03118133706039572 ) ) ;
#11566 = CARTESIAN_POINT ( 'NONE',  ( 0.9780303403264780648, 10.03001170075172510, 40.69076650393633088 ) ) ;
#11567 = ADVANCED_FACE ( 'NONE', ( #8221 ), #46771, .F. ) ;
#11568 = CARTESIAN_POINT ( 'NONE',  ( 0.3622758884714730732, -42.62881903538215056, 6.444611261693867554 ) ) ;
#11569 = CARTESIAN_POINT ( 'NONE',  ( 3.270143674763207553, -2.058141141425505527, -13.53222904135356330 ) ) ;
#11570 =( BOUNDED_SURFACE ( )  B_SPLINE_SURFACE ( 3, 1, ( 
 ( #39174, #19434 ),
 ( #24427, #15049 ),
 ( #48853, #34156 ),
 ( #58227, #10341 ) ),
 .UNSPECIFIED., .F., .F., .F. ) 
 B_SPLINE_SURFACE_WITH_KNOTS ( ( 4, 4 ),
 ( 2, 2 ),
 ( 0.000000000000000000, 1.000000000000000000 ),
 ( 0.000000000000000000, 1.000000000000000000 ),
 .UNSPECIFIED. ) 
 GEOMETRIC_REPRESENTATION_ITEM ( )  RATIONAL_B_SPLINE_SURFACE ( (
 ( 1.000000000000000000, 1.000000000000000000),
 ( 0.7282232189291693025, 0.9929344683865674037),
 ( 0.7282232189291693025, 0.9929344683865674037),
 ( 1.000000000000000000, 1.000000000000000000) ) ) 
 REPRESENTATION_ITEM ( '' )  SURFACE ( )  );
#11571 = VERTEX_POINT ( 'NONE', #3511 ) ;
#11572 = CARTESIAN_POINT ( 'NONE',  ( 1.227938101723756947, 37.58536632582779191, 20.72293514920763258 ) ) ;
#11573 = CARTESIAN_POINT ( 'NONE',  ( -6.072942160501519915, 5.465015824219198848, -18.46450011048374051 ) ) ;
#11574 = CARTESIAN_POINT ( 'NONE',  ( 0.1140933569871965259, -38.25874881921380677, -21.98222210951867694 ) ) ;
#11575 = CARTESIAN_POINT ( 'NONE',  ( 0.1100247026804066219, -41.69861001364780861, 10.99745200874623130 ) ) ;
#11576 = VERTEX_POINT ( 'NONE', #17639 ) ;
#11577 = CARTESIAN_POINT ( 'NONE',  ( 3.782625744892851749, -33.65307366127398581, 25.19342646889998250 ) ) ;
#11578 = CARTESIAN_POINT ( 'NONE',  ( 0.1073791018717578927, 41.52698815987152159, 11.62916352156164557 ) ) ;
#11579 = B_SPLINE_CURVE_WITH_KNOTS ( 'NONE', 3,
 ( #25546, #44387, #1413, #57811 ),
 .UNSPECIFIED., .F., .F.,
 ( 4, 4 ),
 ( 2.276721302528256512E-17, 0.004564976165746189446 ),
 .UNSPECIFIED. ) ;
#11580 = CARTESIAN_POINT ( 'NONE',  ( 4.958415959904823644, -15.85236509608435540, 42.56649474273264389 ) ) ;
#11581 = ORIENTED_EDGE ( 'NONE', *, *, #23420, .T. ) ;
#11582 = CARTESIAN_POINT ( 'NONE',  ( 4.060580049360325461, -43.88752239372906416, 2.313670784519497481 ) ) ;
#11583 = EDGE_CURVE ( 'NONE', #29154, #12616, #4123, .T. ) ;
#11584 = CARTESIAN_POINT ( 'NONE',  ( 0.9730545539215883499, 41.31259007387230753, 11.59290486963521971 ) ) ;
#11585 = ORIENTED_EDGE ( 'NONE', *, *, #25606, .T. ) ;
#11586 = CARTESIAN_POINT ( 'NONE',  ( 2.643462169533600914, -13.76277278785592806, 46.02269433264208232 ) ) ;
#11587 = CARTESIAN_POINT ( 'NONE',  ( 0.6031356219577718170, -29.21669799774991461, 38.21934428970563147 ) ) ;
#11588 = B_SPLINE_CURVE_WITH_KNOTS ( 'NONE', 3,
 ( #16922, #17523, #45431, #50709, #46055, #31309, #60719, #40744, #3096, #30681, #31003, #7476, #12844, #7799, #50111, #25995 ),
 .UNSPECIFIED., .F., .F.,
 ( 4, 3, 3, 3, 3, 4 ),
 ( 1.551621725782133590E-17, 0.0002724568934985473071, 0.0004086836638483666486, 0.0005449104342063532851, 0.0008173270854453651554, 0.001089761613562688575 ),
 .UNSPECIFIED. ) ;
#11589 = ORIENTED_EDGE ( 'NONE', *, *, #5811, .T. ) ;
#11590 = CARTESIAN_POINT ( 'NONE',  ( 2.624215991343608501, -30.33228621715059603, 37.21129343241594256 ) ) ;
#11591 = ORIENTED_EDGE ( 'NONE', *, *, #39069, .F. ) ;
#11592 = CARTESIAN_POINT ( 'NONE',  ( 2.528100132419515589, -35.27989545911430724, -22.75044516105213077 ) ) ;
#11593 = CARTESIAN_POINT ( 'NONE',  ( 5.959547316686252039, -17.77392908783926728, -10.26589671991357022 ) ) ;
#11594 = ORIENTED_EDGE ( 'NONE', *, *, #32630, .F. ) ;
#11595 = AXIS2_PLACEMENT_3D ( 'NONE', #29397, #1803, #57570 ) ;
#11596 = ORIENTED_EDGE ( 'NONE', *, *, #58050, .F. ) ;
#11597 = CARTESIAN_POINT ( 'NONE',  ( 1.199999999999992628, 0.000000000000000000, 0.000000000000000000 ) ) ;
#11598 = CARTESIAN_POINT ( 'NONE',  ( 0.1073791018717483448, 11.62916352156094035, 41.52698815987171344 ) ) ;
#11599 = ORIENTED_EDGE ( 'NONE', *, *, #29132, .F. ) ;
#11600 = VERTEX_POINT ( 'NONE', #57060 ) ;
#11601 = CARTESIAN_POINT ( 'NONE',  ( -6.057079549204054558, -4.276794256740849676, 18.77605554916279473 ) ) ;
#11602 = DIRECTION ( 'NONE',  ( 0.000000000000000000, 0.000000000000000000, -1.000000000000000000 ) ) ;
#11603 = CARTESIAN_POINT ( 'NONE',  ( 0.5809828226811544205, 33.48000389720665027, -34.25055090842118233 ) ) ;
#11604 = CARTESIAN_POINT ( 'NONE',  ( -6.057079549204054558, 13.83914966176537398, 13.39063731638631971 ) ) ;
#11605 = CARTESIAN_POINT ( 'NONE',  ( -6.016761891674564211, -13.32172022638601128, 13.32657647165350490 ) ) ;
#11606 = ORIENTED_EDGE ( 'NONE', *, *, #13492, .T. ) ;
#11607 = DIRECTION ( 'NONE',  ( -1.000000000000000000, 0.000000000000000000, 0.000000000000000000 ) ) ;
#11608 = DIRECTION ( 'NONE',  ( -0.000000000000000000, 0.000000000000000000, -1.000000000000000000 ) ) ;
#11609 = ORIENTED_EDGE ( 'NONE', *, *, #49722, .F. ) ;
#11610 = DIRECTION ( 'NONE',  ( 0.000000000000000000, 0.000000000000000000, 1.000000000000000000 ) ) ;
#11611 = B_SPLINE_CURVE_WITH_KNOTS ( 'NONE', 3,
 ( #7496, #41072, #17238, #36360, #31638, #61053, #28464, #42594, #37592, #51964, #37280, #9056, #5260, #4632, #24392, #32574, #47591, #9672, #32890 ),
 .UNSPECIFIED., .F., .F.,
 ( 4, 3, 3, 3, 3, 3, 4 ),
 ( 1.184243374405472686E-16, 0.0002618519381806228268, 0.0003927759815485937526, 0.0005237000248299437553, 0.0006546240681324990178, 0.0007855481115631294566, 0.0009699050456655100745 ),
 .UNSPECIFIED. ) ;
#11612 = ORIENTED_EDGE ( 'NONE', *, *, #34820, .F. ) ;
#11613 = DIRECTION ( 'NONE',  ( -1.000000000000000000, -0.000000000000000000, 1.925929944387235853E-32 ) ) ;
#11614 = CARTESIAN_POINT ( 'NONE',  ( 0.9762797500689124330, 40.28286501695585997, -11.55922018180369548 ) ) ;
#11615 = ORIENTED_EDGE ( 'NONE', *, *, #15386, .T. ) ;
#11616 = DIRECTION ( 'NONE',  ( -1.000000000000000000, -0.000000000000000000, -0.000000000000000000 ) ) ;
#11617 = FACE_OUTER_BOUND ( 'NONE', #52685, .T. ) ;
#11618 = CARTESIAN_POINT ( 'NONE',  ( 0.8751705887134553219, -0.8911681664085087107, -48.08707113907594533 ) ) ;
#11619 = CARTESIAN_POINT ( 'NONE',  ( 0.6009453534118439633, -28.93865405070921426, -38.43042294376904522 ) ) ;
#11620 = EDGE_CURVE ( 'NONE', #8264, #49921, #18126, .T. ) ;
#11621 = VERTEX_POINT ( 'NONE', #13879 ) ;
#11622 = CARTESIAN_POINT ( 'NONE',  ( 2.526464513654345989, -41.18424249084326760, 12.29060355381837155 ) ) ;
#11623 = ORIENTED_EDGE ( 'NONE', *, *, #21432, .F. ) ;
#11624 = EDGE_CURVE ( 'NONE', #14061, #36392, #41776, .T. ) ;
#11625 = CYLINDRICAL_SURFACE ( 'NONE', #47390, 9.500000000000000000 ) ;
#11626 = CARTESIAN_POINT ( 'NONE',  ( 5.719999999999997087, 6.938893903907228378E-15, 0.000000000000000000 ) ) ;
#11627 =( BOUNDED_SURFACE ( )  B_SPLINE_SURFACE ( 3, 1, ( 
 ( #6692, #40895 ),
 ( #50257, #7008 ),
 ( #26141, #1696 ),
 ( #49635, #2319 ) ),
 .UNSPECIFIED., .F., .F., .F. ) 
 B_SPLINE_SURFACE_WITH_KNOTS ( ( 4, 4 ),
 ( 2, 2 ),
 ( 0.000000000000000000, 1.000000000000000000 ),
 ( 0.000000000000000000, 1.000000000000000000 ),
 .UNSPECIFIED. ) 
 GEOMETRIC_REPRESENTATION_ITEM ( )  RATIONAL_B_SPLINE_SURFACE ( (
 ( 1.000000000000000000, 1.000000000000000000),
 ( 0.9729067724841187204, 0.9999501103223794596),
 ( 0.9729067724841187204, 0.9999501103223794596),
 ( 1.000000000000000000, 1.000000000000000000) ) ) 
 REPRESENTATION_ITEM ( '' )  SURFACE ( )  );
#11628 = CARTESIAN_POINT ( 'NONE',  ( 0.6064782688330866423, 17.51648129858323344, -43.50295770789789174 ) ) ;
#11629 = EDGE_LOOP ( 'NONE', ( #21298, #12778, #57965, #54687 ) ) ;
#11630 = CARTESIAN_POINT ( 'NONE',  ( 1.129531546211701931, 0.000000000000000000, 0.000000000000000000 ) ) ;
#11631 = CARTESIAN_POINT ( 'NONE',  ( 0.9722240741986371004, -42.61332881199390954, 5.023189681690606534 ) ) ;
#11632 = VECTOR ( 'NONE', #25139, 1000.000000000000000 ) ;
#11633 = CARTESIAN_POINT ( 'NONE',  ( 0.5807400328401574052, 12.92266817606079421, -46.12278621143483548 ) ) ;
#11634 = CARTESIAN_POINT ( 'NONE',  ( 2.282803330402970232, -24.15824283434179520, -40.28493776356066292 ) ) ;
#11635 = CARTESIAN_POINT ( 'NONE',  ( -6.078457390727109555, -12.94908628767698211, -14.25186567968572326 ) ) ;
#11636 = EDGE_CURVE ( 'NONE', #57072, #61620, #8871, .T. ) ;
#11637 = CARTESIAN_POINT ( 'NONE',  ( 2.299746137290200831, -44.95078339314706284, 19.58847646011585653 ) ) ;
#11638 = CARTESIAN_POINT ( 'NONE',  ( 4.967162193818130511, 28.07411493385340862, -32.68434214048137676 ) ) ;
#11639 = B_SPLINE_CURVE_WITH_KNOTS ( 'NONE', 3,
 ( #35154, #12280, #11336, #54214, #31368, #11651, #31060, #49534, #25735, #50167, #1917, #40183, #21043, #59232, #59550, #35467 ),
 .UNSPECIFIED., .F., .F.,
 ( 4, 3, 3, 3, 3, 4 ),
 ( 2.030557555191247372E-17, 0.0002618515315864420852, 0.0003927756766341980454, 0.0005236998216950584321, 0.0007855159896329918503, 0.001047349442285929605 ),
 .UNSPECIFIED. ) ;
#11640 =( BOUNDED_SURFACE ( )  B_SPLINE_SURFACE ( 3, 1, ( 
 ( #6328, #15782 ),
 ( #1041, #24241 ),
 ( #10150, #1645 ),
 ( #20784, #39919 ) ),
 .UNSPECIFIED., .F., .F., .F. ) 
 B_SPLINE_SURFACE_WITH_KNOTS ( ( 4, 4 ),
 ( 2, 2 ),
 ( 0.000000000000000000, 1.000000000000000000 ),
 ( 0.000000000000000000, 1.000000000000000000 ),
 .UNSPECIFIED. ) 
 GEOMETRIC_REPRESENTATION_ITEM ( )  RATIONAL_B_SPLINE_SURFACE ( (
 ( 1.000000000000000000, 1.000000000000000000),
 ( 0.9953485035131437453, 0.8621029689291523912),
 ( 0.9953485035131437453, 0.8621029689291523912),
 ( 1.000000000000000000, 1.000000000000000000) ) ) 
 REPRESENTATION_ITEM ( '' )  SURFACE ( )  );
#11641 = CARTESIAN_POINT ( 'NONE',  ( -2.601141883200665639, 2.883136076037970064, 14.64523655788587853 ) ) ;
#11642 = CARTESIAN_POINT ( 'NONE',  ( 4.956445790444027999, 20.31112743693101663, -42.48524629068760561 ) ) ;
#11643 = AXIS2_PLACEMENT_3D ( 'NONE', #11630, #6569, #35445 ) ;
#11644 = EDGE_LOOP ( 'NONE', ( #51259, #14923, #46278, #49922 ) ) ;
#11645 = CARTESIAN_POINT ( 'NONE',  ( 5.719999999999993534, 16.00000000000000355, 0.000000000000000000 ) ) ;
#11646 = DIRECTION ( 'NONE',  ( 0.07836865515943411409, 0.1223011693452784876, 0.9893941468723570498 ) ) ;
#11647 = CARTESIAN_POINT ( 'NONE',  ( 0.7057020205114987732, 44.57024707370739236, -17.55108080125399184 ) ) ;
#11648 = EDGE_LOOP ( 'NONE', ( #15008, #49052, #51950, #51240 ) ) ;
#11649 = CARTESIAN_POINT ( 'NONE',  ( 2.301529144917016101, -22.89307126380016300, 42.22700141647002425 ) ) ;
#11650 = CARTESIAN_POINT ( 'NONE',  ( 0.6253024248130503171, 44.53704952457137978, -20.68563383277205148 ) ) ;
#11651 = CARTESIAN_POINT ( 'NONE',  ( 0.6027935024548037868, -12.28245664247814162, -46.51312430684501464 ) ) ;
#11652 = ORIENTED_EDGE ( 'NONE', *, *, #60687, .T. ) ;
#11653 = CARTESIAN_POINT ( 'NONE',  ( 3.240649175237394264, 40.39403302172326704, -17.42374855298310976 ) ) ;
#11654 = ADVANCED_FACE ( 'NONE', ( #52363 ), #4287, .F. ) ;
#11655 = CARTESIAN_POINT ( 'NONE',  ( 0.9756950546413944991, -41.47131842451891970, -11.01205619898762933 ) ) ;
#11656 = ORIENTED_EDGE ( 'NONE', *, *, #27048, .F. ) ;
#11657 = B_SPLINE_CURVE_WITH_KNOTS ( 'NONE', 3,
 ( #23752, #23443, #52241, #4305 ),
 .UNSPECIFIED., .F., .F.,
 ( 4, 4 ),
 ( 5.818439421673296370E-18, 0.004566006591234647236 ),
 .UNSPECIFIED. ) ;
#11658 = CARTESIAN_POINT ( 'NONE',  ( 0.6000166863083090663, 11.43688157230898383, 47.76003791465657144 ) ) ;
#11659 = ORIENTED_EDGE ( 'NONE', *, *, #36136, .T. ) ;
#11660 = ORIENTED_EDGE ( 'NONE', *, *, #40548, .F. ) ;
#11661 = CARTESIAN_POINT ( 'NONE',  ( 0.8751705887134423323, 42.09020928323375443, -23.27176129838382224 ) ) ;
#11662 = ORIENTED_EDGE ( 'NONE', *, *, #3259, .F. ) ;
#11663 = CARTESIAN_POINT ( 'NONE',  ( 0.6846871229502932144, 5.395516691087188121, 47.60345020167353880 ) ) ;
#11664 = EDGE_CURVE ( 'NONE', #61039, #52564, #46534, .T. ) ;
#11665 = CARTESIAN_POINT ( 'NONE',  ( 0.7948884756798506590, 46.86364173482099460, -14.64574094918027747 ) ) ;
#11666 = ORIENTED_EDGE ( 'NONE', *, *, #48568, .T. ) ;
#11667 = DIRECTION ( 'NONE',  ( 0.09835009131224567436, -0.9223318362920814861, 0.3736726418952155404 ) ) ;
#11668 = CARTESIAN_POINT ( 'NONE',  ( 0.6845945791218023269, 46.36658412396726447, -7.109598961194147471 ) ) ;
#11669 = ADVANCED_FACE ( 'NONE', ( #61141 ), #32908, .F. ) ;
#11670 = AXIS2_PLACEMENT_3D ( 'NONE', #820, #38759, #48436 ) ;
#11671 = ORIENTED_EDGE ( 'NONE', *, *, #5421, .F. ) ;
#11672 = CARTESIAN_POINT ( 'NONE',  ( 0.1158816050234199174, 43.30939313556643810, -8.440290725686597995 ) ) ;
#11673 =( GEOMETRIC_REPRESENTATION_CONTEXT ( 3 ) GLOBAL_UNCERTAINTY_ASSIGNED_CONTEXT ( ( #4744 ) ) GLOBAL_UNIT_ASSIGNED_CONTEXT ( ( #37630, #51074, #32298 ) ) REPRESENTATION_CONTEXT ( 'NONE', 'WORKASPACE' ) );
#11674 = CARTESIAN_POINT ( 'NONE',  ( 0.6846871229502932144, 46.04462816497486699, 13.23224427737845232 ) ) ;
#11675 = CARTESIAN_POINT ( 'NONE',  ( 0.1101816497532062955, -30.39741055095880284, 30.58948775778034346 ) ) ;
#11676 = AXIS2_PLACEMENT_3D ( 'NONE', #34718, #29384, #52880 ) ;
#11677 = CARTESIAN_POINT ( 'NONE',  ( 0.5850706913938533704, -37.88789093229785010, -29.30134895053094013 ) ) ;
#11678 = ORIENTED_EDGE ( 'NONE', *, *, #45848, .F. ) ;
#11679 = B_SPLINE_CURVE_WITH_KNOTS ( 'NONE', 3,
 ( #58648, #25458, #25152, #44299, #1328, #29237, #54564, #6629, #50506, #27022, #45840, #17316, #2885, #46147, #16698, #16381, #11694, #12316, #2577 ),
 .UNSPECIFIED., .F., .F.,
 ( 4, 3, 3, 3, 3, 3, 4 ),
 ( 1.250973872328959318E-17, 0.0002732106629380634077, 0.0004098138914053705531, 0.0005464171197651426781, 0.0006830203481512567417, 0.0008196235766963629824, 0.001011968216111134656 ),
 .UNSPECIFIED. ) ;
#11680 = VERTEX_POINT ( 'NONE', #9153 ) ;
#11681 = CARTESIAN_POINT ( 'NONE',  ( 0.5850706913938533704, -24.10530971368318021, 41.38834827854200427 ) ) ;
#11682 = B_SPLINE_CURVE_WITH_KNOTS ( 'NONE', 3,
 ( #55242, #41810, #17994, #41188, #27372, #60251 ),
 .UNSPECIFIED., .F., .F.,
 ( 4, 2, 4 ),
 ( 1.193162889884620877E-16, 0.0002448718616795923374, 0.0004897437233590653041 ),
 .UNSPECIFIED. ) ;
#11683 = CARTESIAN_POINT ( 'NONE',  ( -6.001507490154111224, -16.31148204059940809, -9.435425682280991211 ) ) ;
#11684 = DIRECTION ( 'NONE',  ( -1.000000000000000000, -0.000000000000000000, -0.000000000000000000 ) ) ;
#11685 = ORIENTED_EDGE ( 'NONE', *, *, #47655, .F. ) ;
#11686 = CARTESIAN_POINT ( 'NONE',  ( 5.959547316686252039, 14.51128755440521267, 14.51632612601533801 ) ) ;
#11687 = CARTESIAN_POINT ( 'NONE',  ( 2.282816707992318062, -2.882087820334355843, -46.88486468151364761 ) ) ;
#11688 = CARTESIAN_POINT ( 'NONE',  ( -2.569797478183790229, -10.65947181927846543, 10.02484965418622842 ) ) ;
#11689 = CARTESIAN_POINT ( 'NONE',  ( 0.9730545539215883499, -25.71816799638802920, 34.34678117142546938 ) ) ;
#11690 = EDGE_CURVE ( 'NONE', #32619, #49021, #32670, .T. ) ;
#11691 = AXIS2_PLACEMENT_3D ( 'NONE', #749, #25176, #19885 ) ;
#11692 = ORIENTED_EDGE ( 'NONE', *, *, #32047, .F. ) ;
#11693 = ORIENTED_EDGE ( 'NONE', *, *, #22923, .F. ) ;
#11694 = CARTESIAN_POINT ( 'NONE',  ( 0.9775691876210972353, -39.46427349087333170, -14.10336225258165399 ) ) ;
#11695 = CARTESIAN_POINT ( 'NONE',  ( 0.7245667037590752813, 28.62745028382816415, -38.65590879674357438 ) ) ;
#11696 = EDGE_CURVE ( 'NONE', #21722, #56788, #58474, .T. ) ;
#11697 = CARTESIAN_POINT ( 'NONE',  ( 0.1095718737110178420, -39.93945841550387854, 16.26534146842136508 ) ) ;
#11698 = B_SPLINE_CURVE_WITH_KNOTS ( 'NONE', 3,
 ( #52257, #28456, #18775, #4319 ),
 .UNSPECIFIED., .F., .F.,
 ( 4, 4 ),
 ( 0.000000000000000000, 0.005013413432710138971 ),
 .UNSPECIFIED. ) ;
#11699 = FACE_OUTER_BOUND ( 'NONE', #4458, .T. ) ;
#11700 = CIRCLE ( 'NONE', #40738, 43.92652462719577500 ) ;
#11701 = CARTESIAN_POINT ( 'NONE',  ( 0.1092565886968784594, 34.02318727879963944, -26.49813811968549615 ) ) ;
#11702 = ADVANCED_FACE ( 'NONE', ( #46 ), #29743, .F. ) ;
#11703 = CARTESIAN_POINT ( 'NONE',  ( 4.060580049360325461, -43.23134078854796059, 7.906887376435675741 ) ) ;
#11704 = CARTESIAN_POINT ( 'NONE',  ( 0.5850706913938534814, -37.88789093229826932, 29.30134895053040722 ) ) ;
#11705 = CARTESIAN_POINT ( 'NONE',  ( 0.5804410086790514622, -30.69452151258743555, 35.45935984995644930 ) ) ;
#11706 = CARTESIAN_POINT ( 'NONE',  ( 0.5998501479064708430, 12.95623334615502387, -46.33007877220726556 ) ) ;
#11707 = CARTESIAN_POINT ( 'NONE',  ( 0.8751705887134423323, 38.69254731947834358, -28.56654290188613032 ) ) ;
#11708 = CARTESIAN_POINT ( 'NONE',  ( 1.227938101723756947, 20.72293514920803048, -37.58536632582757875 ) ) ;
#11709 = CARTESIAN_POINT ( 'NONE',  ( 0.1313383488274124100, -11.77600546273740534, -41.48452234694092056 ) ) ;
#11710 = EDGE_CURVE ( 'NONE', #51385, #45191, #32326, .T. ) ;
#11711 = CARTESIAN_POINT ( 'NONE',  ( 5.895881250540457863, 14.91980774178292712, -13.48803241976142075 ) ) ;
#11712 = CARTESIAN_POINT ( 'NONE',  ( 0.6031356755773454870, -34.01711753073234945, -34.01708126935030663 ) ) ;
#11713 = CARTESIAN_POINT ( 'NONE',  ( -31.74999999999995737, 0.000000000000000000, 0.000000000000000000 ) ) ;
#11714 = CARTESIAN_POINT ( 'NONE',  ( 0.6009453534118438522, -5.846398087359047757, -47.75104957283896567 ) ) ;
#11715 = CARTESIAN_POINT ( 'NONE',  ( 4.303969348037258058, 45.22910199346975446, 16.39840148505108886 ) ) ;
#11716 = VECTOR ( 'NONE', #8722, 1000.000000000000000 ) ;
#11718 =( BOUNDED_SURFACE ( )  B_SPLINE_SURFACE ( 3, 1, ( 
 ( #10237, #22101 ),
 ( #26176, #41228 ),
 ( #40007, #12107 ),
 ( #2355, #55281 ) ),
 .UNSPECIFIED., .F., .F., .F. ) 
 B_SPLINE_SURFACE_WITH_KNOTS ( ( 4, 4 ),
 ( 2, 2 ),
 ( 0.000000000000000000, 1.000000000000000000 ),
 ( 0.000000000000000000, 1.000000000000000000 ),
 .UNSPECIFIED. ) 
 GEOMETRIC_REPRESENTATION_ITEM ( )  RATIONAL_B_SPLINE_SURFACE ( (
 ( 1.000000000000000000, 1.000000000000000000),
 ( 0.9953390228620291325, 0.8624445117760984880),
 ( 0.9953390228620291325, 0.8624445117760984880),
 ( 1.000000000000000000, 1.000000000000000000) ) ) 
 REPRESENTATION_ITEM ( '' )  SURFACE ( )  );
#11717 = CARTESIAN_POINT ( 'NONE',  ( 0.5804410086790514622, 46.40460073163221466, 6.792119168064940204 ) ) ;
#11719 = CARTESIAN_POINT ( 'NONE',  ( 4.956445790443998689, -22.15545010017797622, 41.55326799420426198 ) ) ;
#11721 = ORIENTED_EDGE ( 'NONE', *, *, #34182, .F. ) ;
#11720 = CARTESIAN_POINT ( 'NONE',  ( 0.6001305935487422083, 47.62765676940944104, -6.798494447611732383 ) ) ;
#11722 = ORIENTED_EDGE ( 'NONE', *, *, #17980, .T. ) ;
#11723 = STYLED_ITEM ( 'NONE', ( #45770 ), #59429 ) ;
#11724 = CARTESIAN_POINT ( 'NONE',  ( -6.016489644550737204, -18.19999694163060511, -4.881234076340565942 ) ) ;
#11725 = CARTESIAN_POINT ( 'NONE',  ( 4.956653778116990594, -20.77844580450529577, -43.37017594958076927 ) ) ;
#11726 = CIRCLE ( 'NONE', #22712, 48.91267123290010943 ) ;
#11727 = CARTESIAN_POINT ( 'NONE',  ( -6.015611763856276717, 18.68284711750058591, 2.453375430804133117 ) ) ;
#11728 = ORIENTED_EDGE ( 'NONE', *, *, #31621, .F. ) ;
#11729 = ORIENTED_EDGE ( 'NONE', *, *, #47, .F. ) ;
#11730 = FACE_OUTER_BOUND ( 'NONE', #49057, .T. ) ;
#11731 = CARTESIAN_POINT ( 'NONE',  ( 0.7048096507298635682, 33.41730025321754027, -34.61049487267025171 ) ) ;
#11732 = CARTESIAN_POINT ( 'NONE',  ( 0.6025881611877911270, 6.062907795288723811, 47.72390913208167262 ) ) ;
#11733 = ORIENTED_EDGE ( 'NONE', *, *, #34562, .T. ) ;
#11734 = ORIENTED_EDGE ( 'NONE', *, *, #53116, .F. ) ;
#11735 = CARTESIAN_POINT ( 'NONE',  ( 0.8557997880470599172, 47.60865952217007191, -5.347802024196765203 ) ) ;
#11736 =( BOUNDED_SURFACE ( )  B_SPLINE_SURFACE ( 3, 1, ( 
 ( #36135, #12319 ),
 ( #54891, #18247 ),
 ( #12942, #51419 ),
 ( #31413, #22323 ) ),
 .UNSPECIFIED., .F., .F., .F. ) 
 B_SPLINE_SURFACE_WITH_KNOTS ( ( 4, 4 ),
 ( 2, 2 ),
 ( 0.000000000000000000, 1.000000000000000000 ),
 ( 0.000000000000000000, 1.000000000000000000 ),
 .UNSPECIFIED. ) 
 GEOMETRIC_REPRESENTATION_ITEM ( )  RATIONAL_B_SPLINE_SURFACE ( (
 ( 1.000000000000000000, 1.000000000000000000),
 ( 0.9952954269826590483, 0.8620686068821307169),
 ( 0.9952954269826590483, 0.8620686068821307169),
 ( 1.000000000000000000, 1.000000000000000000) ) ) 
 REPRESENTATION_ITEM ( '' )  SURFACE ( )  );
#11737 = CARTESIAN_POINT ( 'NONE',  ( 2.301529144917016101, -38.87759814529798774, -28.20894756932127478 ) ) ;
#11738 = CARTESIAN_POINT ( 'NONE',  ( 0.8560838555295223751, 17.70877843982779609, 43.43698884880053157 ) ) ;
#11739 = EDGE_CURVE ( 'NONE', #58614, #27427, #6887, .T. ) ;
#11740 =( BOUNDED_SURFACE ( )  B_SPLINE_SURFACE ( 3, 1, ( 
 ( #18778, #19697 ),
 ( #13777, #47586 ),
 ( #52260, #48202 ),
 ( #5255, #8739 ) ),
 .UNSPECIFIED., .F., .F., .F. ) 
 B_SPLINE_SURFACE_WITH_KNOTS ( ( 4, 4 ),
 ( 2, 2 ),
 ( 0.000000000000000000, 1.000000000000000000 ),
 ( 0.000000000000000000, 1.000000000000000000 ),
 .UNSPECIFIED. ) 
 GEOMETRIC_REPRESENTATION_ITEM ( )  RATIONAL_B_SPLINE_SURFACE ( (
 ( 1.000000000000000000, 1.000000000000000000),
 ( 0.7223157951917476005, 0.9931996967497186413),
 ( 0.7223157951917476005, 0.9931996967497186413),
 ( 1.000000000000000000, 1.000000000000000000) ) ) 
 REPRESENTATION_ITEM ( '' )  SURFACE ( )  );
#11741 = ORIENTED_EDGE ( 'NONE', *, *, #2878, .T. ) ;
#11742 = DIRECTION ( 'NONE',  ( -0.8660254037844372643, -0.5000000000000024425, 0.000000000000000000 ) ) ;
#11743 = EDGE_CURVE ( 'NONE', #9098, #8039, #15956, .T. ) ;
#11744 = CARTESIAN_POINT ( 'NONE',  ( 5.917102823773431552, 18.99629506471996265, -6.605338134103194925 ) ) ;
#11745 = CARTESIAN_POINT ( 'NONE',  ( 0.9730545539215883499, -42.60426903087349615, -5.099196237955331057 ) ) ;
#11746 = EDGE_LOOP ( 'NONE', ( #54409, #42973, #41859, #26636 ) ) ;
#11747 = EDGE_CURVE ( 'NONE', #18385, #15656, #39116, .T. ) ;
#11748 = VECTOR ( 'NONE', #33293, 1000.000000000000114 ) ;
#11749 = ORIENTED_EDGE ( 'NONE', *, *, #7847, .F. ) ;
#11750 = CARTESIAN_POINT ( 'NONE',  ( 0.7056555295713301534, 13.20840017675017819, 46.04438433984157086 ) ) ;
#11751 = CARTESIAN_POINT ( 'NONE',  ( 0.8744876279028306332, -19.05609938969034545, 45.24616145519679122 ) ) ;
#11752 = ORIENTED_EDGE ( 'NONE', *, *, #1006, .T. ) ;
#11753 = DIRECTION ( 'NONE',  ( -1.000000000000000000, -0.000000000000000000, -0.000000000000000000 ) ) ;
#11754 = DIRECTION ( 'NONE',  ( -1.000000000000000000, -1.836909530733573776E-16, 1.925929944387235853E-32 ) ) ;
#11755 = DIRECTION ( 'NONE',  ( -1.000000000000000000, -0.000000000000000000, -0.000000000000000000 ) ) ;
#11756 = DIRECTION ( 'NONE',  ( 1.000000000000000000, 1.836909530733573776E-16, 0.000000000000000000 ) ) ;
#11757 = B_SPLINE_CURVE_WITH_KNOTS ( 'NONE', 3,
 ( #1640, #44603, #26394, #2886, #20777, #45230, #2578, #49574, #31099, #50200, #40524, #54255, #59589, #22017, #41143, #7266, #49267, #35819, #11376, #45524, #21699, #17317, #17016, #21391, #60205 ),
 .UNSPECIFIED., .F., .F.,
 ( 4, 3, 3, 3, 3, 3, 3, 3, 4 ),
 ( 6.254634441385501517E-18, 0.0005656085177311396400, 0.001131215744874500273, 0.001696821861372766783, 0.002262427090022499018, 0.002828031679238746359, 0.003393635864401605296, 0.003977030878808132490, 0.004561030005651159867 ),
 .UNSPECIFIED. ) ;
#11758 = ORIENTED_EDGE ( 'NONE', *, *, #47885, .F. ) ;
#11759 = FACE_OUTER_BOUND ( 'NONE', #54226, .T. ) ;
#11760 = CARTESIAN_POINT ( 'NONE',  ( 0.5998501479064708430, 17.92509395669044636, 44.64337787626254794 ) ) ;
#11761 = CARTESIAN_POINT ( 'NONE',  ( 0.8554163680231720024, -42.27859581856498750, -20.34025095032602337 ) ) ;
#11762 = ORIENTED_EDGE ( 'NONE', *, *, #46606, .T. ) ;
#11763 = CARTESIAN_POINT ( 'NONE',  ( 4.956445790443996913, 8.365049606151725214, 46.34181691762049127 ) ) ;
#11764 = CIRCLE ( 'NONE', #59771, 2.649999999999985700 ) ;
#11765 = CARTESIAN_POINT ( 'NONE',  ( 0.7954190325252781246, -47.79303692714238139, -5.415566973723075606 ) ) ;
#11766 = CARTESIAN_POINT ( 'NONE',  ( 4.975801465491694664, -47.76942479135482955, -3.702618843597289544 ) ) ;
#11767 = EDGE_CURVE ( 'NONE', #35750, #3477, #10089, .T. ) ;
#11768 = AXIS2_PLACEMENT_3D ( 'NONE', #5092, #57102, #10129 ) ;
#11769 = ORIENTED_EDGE ( 'NONE', *, *, #46640, .F. ) ;
#11770 = CARTESIAN_POINT ( 'NONE',  ( 4.553261556744873317, 42.43205150231990075, -11.36048287389704292 ) ) ;
#11771 = AXIS2_PLACEMENT_3D ( 'NONE', #11597, #11281, #25372 ) ;
#11772 = EDGE_CURVE ( 'NONE', #10837, #873, #38308, .T. ) ;
#11773 = CARTESIAN_POINT ( 'NONE',  ( 0.1092565886968784317, -42.71401356099882918, 5.936467125236308817 ) ) ;
#11774 = DIRECTION ( 'NONE',  ( -1.000000000000000000, -0.000000000000000000, -0.000000000000000000 ) ) ;
#11775 = PRODUCT_DEFINITION_SHAPE ( 'NONE', 'NONE',  #61977 ) ;
#11776 = EDGE_CURVE ( 'NONE', #61479, #5641, #11798, .T. ) ;
#11777 = CARTESIAN_POINT ( 'NONE',  ( 3.238018933889920792, -6.973938193058373258, -11.43554451904476110 ) ) ;
#11778 = CARTESIAN_POINT ( 'NONE',  ( 1.479689385636123067, 21.41596951469469090, 38.50896122999632354 ) ) ;
#11779 = CARTESIAN_POINT ( 'NONE',  ( 0.1129192098497447394, -41.07894348801345075, -16.10814047907924973 ) ) ;
#11780 = CARTESIAN_POINT ( 'NONE',  ( 4.975610109902397937, -28.45381238669816426, 39.78479568629648355 ) ) ;
#11781 = CARTESIAN_POINT ( 'NONE',  ( 4.975801465491695552, -40.15204426031515794, -26.14269827151666092 ) ) ;
#11782 = CARTESIAN_POINT ( 'NONE',  ( 3.376099380956838925, 4.385778397990253374, 12.66780689289938522 ) ) ;
#11783 = CARTESIAN_POINT ( 'NONE',  ( 0.5809828226811553087, 38.32755012159145025, 28.72298383114502229 ) ) ;
#11784 = CARTESIAN_POINT ( 'NONE',  ( 0.9783242366443547500, 14.81179524866698749, 39.20389281331754461 ) ) ;
#11785 = ORIENTED_EDGE ( 'NONE', *, *, #50491, .F. ) ;
#11786 = CARTESIAN_POINT ( 'NONE',  ( -17.29657906255854982, -12.34027659683576772, -1.992589851484418917 ) ) ;
#11787 = CARTESIAN_POINT ( 'NONE',  ( 4.962356264823608143, -28.94323483023595145, -30.55363735178127271 ) ) ;
#11788 = CARTESIAN_POINT ( 'NONE',  ( 4.975801465491695552, 2.564218696447496004, -47.84403947906841381 ) ) ;
#11789 = CARTESIAN_POINT ( 'NONE',  ( 0.5806925824938499181, -34.41156632303712826, -31.86010774524751454 ) ) ;
#11790 = EDGE_CURVE ( 'NONE', #22861, #13203, #57692, .T. ) ;
#11791 = CARTESIAN_POINT ( 'NONE',  ( 5.958863334805807099, -17.77634700750936148, 10.26176968287914093 ) ) ;
#11792 = AXIS2_PLACEMENT_3D ( 'NONE', #10305, #10001, #43528 ) ;
#11793 = CARTESIAN_POINT ( 'NONE',  ( 0.9780303403264750672, -30.86352413661125382, 28.35105802723950319 ) ) ;
#11794 = CARTESIAN_POINT ( 'NONE',  ( 15.00000000000001421, -56.56854249492385378, -56.56854249492376141 ) ) ;
#11795 = CARTESIAN_POINT ( 'NONE',  ( 5.896278296736517710, 17.94863123379898440, -9.075991210191821423 ) ) ;
#11796 = EDGE_CURVE ( 'NONE', #53243, #41822, #26327, .T. ) ;
#11797 = CARTESIAN_POINT ( 'NONE',  ( 0.6017666602106488405, 41.48673504406946932, -24.35550044372401501 ) ) ;
#11798 = CIRCLE ( 'NONE', #46816, 12.55882000000000076 ) ;
#11799 = CARTESIAN_POINT ( 'NONE',  ( 0.9780106845699465534, 29.35917852947671847, -29.90601749698134881 ) ) ;
#11801 = ORIENTED_EDGE ( 'NONE', *, *, #60378, .T. ) ;
#11800 = CARTESIAN_POINT ( 'NONE',  ( 4.958415959904816539, 44.40884735405912664, -9.542443633918582080 ) ) ;
#11802 = EDGE_LOOP ( 'NONE', ( #11806, #39738, #31212, #11722 ) ) ;
#11803 = CARTESIAN_POINT ( 'NONE',  ( 5.860006189529246790, -40.11385274514700683, 26.78264244998084820 ) ) ;
#11804 = CARTESIAN_POINT ( 'NONE',  ( 3.680974057930773480, -8.091325130366769258, 47.28851186370993531 ) ) ;
#11805 = DIRECTION ( 'NONE',  ( -1.000000000000000000, -0.000000000000000000, -0.000000000000000000 ) ) ;
#11806 = ORIENTED_EDGE ( 'NONE', *, *, #16032, .F. ) ;
#11807 = CARTESIAN_POINT ( 'NONE',  ( 0.6253024248130480967, -47.32157158351321868, -13.11918786678801574 ) ) ;
#11808 = CARTESIAN_POINT ( 'NONE',  ( 5.838029081930957709, -4.747847248974175649, -46.99492530745558128 ) ) ;
#11810 = DIRECTION ( 'NONE',  ( -1.685288351013738396E-16, 1.000000000000000000, 0.000000000000000000 ) ) ;
#11809 = B_SPLINE_CURVE_WITH_KNOTS ( 'NONE', 3,
 ( #6707, #39358, #34341, #10523, #16156, #6095 ),
 .UNSPECIFIED., .F., .F.,
 ( 4, 2, 4 ),
 ( 2.196750944941757354E-17, 0.0002293319059085104420, 0.0004586638118169989288 ),
 .UNSPECIFIED. ) ;
#11811 = B_SPLINE_CURVE_WITH_KNOTS ( 'NONE', 3,
 ( #39110, #43188, #24993, #218, #44131, #9968, #48184, #19677, #5236, #14988, #56943, #1159, #34097, #20293, #14064, #52239 ),
 .UNSPECIFIED., .F., .F.,
 ( 4, 3, 3, 3, 3, 4 ),
 ( 1.962735358247464152E-17, 0.0002618515315864398084, 0.0003927756766341925702, 0.0005236998216950552879, 0.0007855159896329908745, 0.001047349442285923317 ),
 .UNSPECIFIED. ) ;
#11812 = B_SPLINE_CURVE_WITH_KNOTS ( 'NONE', 3,
 ( #17657, #21738, #55856, #45263, #8237, #12980 ),
 .UNSPECIFIED., .F., .F.,
 ( 4, 2, 4 ),
 ( 0.000000000000000000, 0.0002291459268755709124, 0.0004582918537511418249 ),
 .UNSPECIFIED. ) ;
#11813 = EDGE_LOOP ( 'NONE', ( #34237, #6478, #11027, #61008 ) ) ;
#11814 = ORIENTED_EDGE ( 'NONE', *, *, #6333, .F. ) ;
#11815 = DIRECTION ( 'NONE',  ( 0.000000000000000000, 0.000000000000000000, -1.000000000000000000 ) ) ;
#11816 = AXIS2_PLACEMENT_3D ( 'NONE', #54730, #44761, #21858 ) ;
#11817 = CARTESIAN_POINT ( 'NONE',  ( 0.1073791018717483448, -40.02496097243048467, -16.05399293000801819 ) ) ;
#11818 = CARTESIAN_POINT ( 'NONE',  ( 0.6067375320500725255, 41.82999795871641169, -23.33187539052085668 ) ) ;
#11819 = EDGE_LOOP ( 'NONE', ( #33452, #27207, #61717, #49182, #46180 ) ) ;
#11820 = ADVANCED_FACE ( 'NONE', ( #31905 ), #11458, .F. ) ;
#11821 = ORIENTED_EDGE ( 'NONE', *, *, #30827, .F. ) ;
#11822 = ADVANCED_FACE ( 'NONE', ( #41619 ), #17873, .F. ) ;
#11823 = DIRECTION ( 'NONE',  ( -1.000000000000000000, -1.836909530733554547E-16, -1.836909530733573529E-16 ) ) ;
#11824 = CARTESIAN_POINT ( 'NONE',  ( 0.7245667037590747261, -11.65533952568384990, 46.66865388241065915 ) ) ;
#11825 =( BOUNDED_SURFACE ( )  B_SPLINE_SURFACE ( 3, 1, ( 
 ( #16884, #17184 ),
 ( #55062, #50372 ),
 ( #21882, #21260 ),
 ( #36303, #12491 ) ),
 .UNSPECIFIED., .F., .F., .F. ) 
 B_SPLINE_SURFACE_WITH_KNOTS ( ( 4, 4 ),
 ( 2, 2 ),
 ( 0.000000000000000000, 1.000000000000000000 ),
 ( 0.000000000000000000, 1.000000000000000000 ),
 .UNSPECIFIED. ) 
 GEOMETRIC_REPRESENTATION_ITEM ( )  RATIONAL_B_SPLINE_SURFACE ( (
 ( 1.000000000000000000, 1.000000000000000000),
 ( 0.9732289882329797637, 0.9999525324661233672),
 ( 0.9732289882329797637, 0.9999525324661233672),
 ( 1.000000000000000000, 1.000000000000000000) ) ) 
 REPRESENTATION_ITEM ( '' )  SURFACE ( )  );
#11826 = ORIENTED_EDGE ( 'NONE', *, *, #60096, .T. ) ;
#11827 = CARTESIAN_POINT ( 'NONE',  ( -6.077587904424778920, -11.01164173315279271, -15.79682777441781738 ) ) ;
#11828 = CARTESIAN_POINT ( 'NONE',  ( 0.9754642270333696574, 41.49150764699772509, -10.93570046136864882 ) ) ;
#11829 = ORIENTED_EDGE ( 'NONE', *, *, #22474, .F. ) ;
#11830 = ADVANCED_FACE ( 'NONE', ( #36309 ), #22194, .F. ) ;
#11831 = EDGE_CURVE ( 'NONE', #33073, #1887, #46628, .T. ) ;
#11832 =( BOUNDED_SURFACE ( )  B_SPLINE_SURFACE ( 3, 1, ( 
 ( #28612, #4474 ),
 ( #5096, #48347 ),
 ( #4783, #24536 ),
 ( #56497, #32719 ) ),
 .UNSPECIFIED., .F., .F., .F. ) 
 B_SPLINE_SURFACE_WITH_KNOTS ( ( 4, 4 ),
 ( 2, 2 ),
 ( 0.000000000000000000, 1.000000000000000000 ),
 ( 0.000000000000000000, 1.000000000000000000 ),
 .UNSPECIFIED. ) 
 GEOMETRIC_REPRESENTATION_ITEM ( )  RATIONAL_B_SPLINE_SURFACE ( (
 ( 1.000000000000000000, 1.000000000000000000),
 ( 0.9953485035131437453, 0.8621029689291523912),
 ( 0.9953485035131437453, 0.8621029689291523912),
 ( 1.000000000000000000, 1.000000000000000000) ) ) 
 REPRESENTATION_ITEM ( '' )  SURFACE ( )  );
#11833 = CARTESIAN_POINT ( 'NONE',  ( 0.5830082357119554803, -34.96314582746199306, 31.25396724875045251 ) ) ;
#11834 = B_SPLINE_CURVE_WITH_KNOTS ( 'NONE', 3,
 ( #55357, #26561, #26246, #60070 ),
 .UNSPECIFIED., .F., .F.,
 ( 4, 4 ),
 ( 2.204559228842524708E-17, 0.004564976165746186844 ),
 .UNSPECIFIED. ) ;
#11835 = CIRCLE ( 'NONE', #45867, 1.000000000000000888 ) ;
#11836 = ORIENTED_EDGE ( 'NONE', *, *, #11636, .T. ) ;
#11837 = CARTESIAN_POINT ( 'NONE',  ( -6.077587904424778920, -11.02178778841139284, 15.78975032548507151 ) ) ;
#11838 = ADVANCED_FACE ( 'NONE', ( #37234 ), #56260, .F. ) ;
#11839 = CARTESIAN_POINT ( 'NONE',  ( 0.5830082357119558134, -19.98760262368099561, 42.42319856276937173 ) ) ;
#11840 = CARTESIAN_POINT ( 'NONE',  ( 0.7764146366350263007, 44.99430970888712267, -13.24962518299705216 ) ) ;
#11841 = CARTESIAN_POINT ( 'NONE',  ( 3.678748215320119197, -41.73555123697755675, 25.62726238296056636 ) ) ;
#11842 = VERTEX_POINT ( 'NONE', #28737 ) ;
#11843 = FACE_BOUND ( 'NONE', #23192, .T. ) ;
#11844 = DIRECTION ( 'NONE',  ( -0.1024043820194934368, -0.5087173657443582186, 0.8548216096550944609 ) ) ;
#11845 = VERTEX_POINT ( 'NONE', #61609 ) ;
#11846 = CARTESIAN_POINT ( 'NONE',  ( -6.078726893082806448, 12.00859800336337280, 15.05282748397580406 ) ) ;
#11847 = MECHANICAL_DESIGN_GEOMETRIC_PRESENTATION_REPRESENTATION (  '', ( #34860 ), #812 ) ;
#11848 = EDGE_CURVE ( 'NONE', #49193, #29773, #27107, .T. ) ;
#11849 = ORIENTED_EDGE ( 'NONE', *, *, #33447, .F. ) ;
#11850 = CARTESIAN_POINT ( 'NONE',  ( 0.9789233960466698914, 4.064014989232912711, 41.71115569005051071 ) ) ;
#11851 = VECTOR ( 'NONE', #42378, 1000.000000000000000 ) ;
#11852 = ORIENTED_EDGE ( 'NONE', *, *, #24431, .F. ) ;
#11853 = CARTESIAN_POINT ( 'NONE',  ( -6.016761891674564211, -0.003433883959652091721, -18.84319130225482297 ) ) ;
#11854 = CARTESIAN_POINT ( 'NONE',  ( 0.5997462898726536595, -25.90236585764290922, 41.72072714036901431 ) ) ;
#11855 = DIRECTION ( 'NONE',  ( -1.000000000000000000, -0.000000000000000000, -0.000000000000000000 ) ) ;
#11856 = VERTEX_POINT ( 'NONE', #27812 ) ;
#11857 = CARTESIAN_POINT ( 'NONE',  ( 0.1135584504625007651, -27.17198796317027742, -34.76542998820209363 ) ) ;
#11858 = CARTESIAN_POINT ( 'NONE',  ( 4.962356264823608143, -41.65024625884313991, -6.040909239515997342 ) ) ;
#11859 = DIRECTION ( 'NONE',  ( 0.000000000000000000, 0.000000000000000000, -1.000000000000000000 ) ) ;
#11860 = ORIENTED_EDGE ( 'NONE', *, *, #21864, .F. ) ;
#11861 = ORIENTED_EDGE ( 'NONE', *, *, #14553, .T. ) ;
#11862 = CARTESIAN_POINT ( 'NONE',  ( 0.2940133293163001982, 29.05872899538194432, 33.19383705977649157 ) ) ;
#11863 = CARTESIAN_POINT ( 'NONE',  ( 2.648799415243708655, 47.84750745855113507, -10.73002764644580687 ) ) ;
#11864 = CARTESIAN_POINT ( 'NONE',  ( 0.6021448801613057400, 32.82111563175431712, 36.52828366230692581 ) ) ;
#11865 = CARTESIAN_POINT ( 'NONE',  ( 0.1103878639767399139, -5.676988162228372659, -42.74915604780179024 ) ) ;
#11866 = CARTESIAN_POINT ( 'NONE',  ( 0.5824935313925948543, -30.55463868283966633, -35.57600640902456490 ) ) ;
#11867 = CARTESIAN_POINT ( 'NONE',  ( 0.5809828226811553087, 23.47450554821769231, -41.74875432577623258 ) ) ;
#11868 = ORIENTED_EDGE ( 'NONE', *, *, #25203, .F. ) ;
#11869 = CARTESIAN_POINT ( 'NONE',  ( 0.5998501479064699549, 17.92509395669108585, -44.64337787626229925 ) ) ;
#11870 = AXIS2_PLACEMENT_3D ( 'NONE', #25671, #49167, #40121 ) ;
#11871 = CARTESIAN_POINT ( 'NONE',  ( 3.783278058412225864, 39.06943705276857060, -18.05212641201930168 ) ) ;
#11872 = ORIENTED_EDGE ( 'NONE', *, *, #28437, .T. ) ;
#11873 = AXIS2_PLACEMENT_3D ( 'NONE', #23417, #28733, #3975 ) ;
#11874 = FACE_OUTER_BOUND ( 'NONE', #58721, .T. ) ;
#11875 = CARTESIAN_POINT ( 'NONE',  ( -2.708315649062910779, -4.041664582652894744, 14.06540004355475837 ) ) ;
#11876 = CARTESIAN_POINT ( 'NONE',  ( 4.999999999999983125, 80.00000000000001421, -3.562970397116383044E-32 ) ) ;
#11877 = CARTESIAN_POINT ( 'NONE',  ( 0.5817216825391123836, 45.34790762631963901, 11.94998854067397787 ) ) ;
#11878 = EDGE_CURVE ( 'NONE', #48571, #57030, #33454, .T. ) ;
#11879 = CARTESIAN_POINT ( 'NONE',  ( -6.072942160501519027, -4.270762779174233970, -18.77670758075122137 ) ) ;
#11880 = CARTESIAN_POINT ( 'NONE',  ( -6.057079549204054558, 9.989941839883096364, -16.46305843807557778 ) ) ;
#11881 = CARTESIAN_POINT ( 'NONE',  ( -2.739355103387247858, 14.60025052884536123, 3.111310245855882339 ) ) ;
#11882 =( NAMED_UNIT ( * ) PLANE_ANGLE_UNIT ( ) SI_UNIT ( $, .RADIAN. ) );
#11883 = CARTESIAN_POINT ( 'NONE',  ( 0.1157991065609915854, -12.47647594550060823, -42.32351490033694574 ) ) ;
#11884 = ADVANCED_FACE ( 'NONE', ( #57840 ), #57519, .F. ) ;
#11885 = CARTESIAN_POINT ( 'NONE',  ( 0.9730545539215883499, -39.83279466599050522, 15.95224156741815236 ) ) ;
#11886 = CARTESIAN_POINT ( 'NONE',  ( 0.2230388203127590674, -40.12182516270790700, -15.79641846944905481 ) ) ;
#11887 = CARTESIAN_POINT ( 'NONE',  ( 5.000000000000007994, -54.69470952477895764, -58.44237546506863623 ) ) ;
#11888 = VECTOR ( 'NONE', #52666, 1000.000000000000000 ) ;
#11889 = CARTESIAN_POINT ( 'NONE',  ( 3.376099380956838925, 13.33943071323252916, -1.329651036526449115 ) ) ;
#11890 = CARTESIAN_POINT ( 'NONE',  ( -2.601141883200662974, -8.117336596316121700, -12.52614362249992830 ) ) ;
#11891 = DIRECTION ( 'NONE',  ( 0.9848077530122080203, 0.1736481776669315524, -2.220446049250313574E-16 ) ) ;
#11892 = CARTESIAN_POINT ( 'NONE',  ( 0.6846871229502932144, -24.69859318104518309, 41.05093867799178042 ) ) ;
#11893 = COLOUR_RGB ( '', 0.08235294, 0.09019608, 0.10196078) ;
#11894 = ORIENTED_EDGE ( 'NONE', *, *, #11183, .F. ) ;
#11895 = CARTESIAN_POINT ( 'NONE',  ( 0.5804410086790514622, 4.150428748652395861, -46.71502748642834746 ) ) ;
#11896 = CARTESIAN_POINT ( 'NONE',  ( 0.1097557419366048670, 43.12388302211984126, -0.2231007852155202087 ) ) ;
#11897 = CARTESIAN_POINT ( 'NONE',  ( 0.9757787079277437936, -39.62711913632688265, -16.45683390770826549 ) ) ;
#11898 = CARTESIAN_POINT ( 'NONE',  ( 0.5800708119828337228, 28.65679933661850498, -38.37709857409239333 ) ) ;
#11899 = CARTESIAN_POINT ( 'NONE',  ( 3.660087539127333311, 16.63102164621095014, -45.06758728829451854 ) ) ;
#11900 = VECTOR ( 'NONE', #31185, 1000.000000000000000 ) ;
#11901 = VERTEX_POINT ( 'NONE', #19347 ) ;
#11902 = CARTESIAN_POINT ( 'NONE',  ( 4.303969348037258058, -36.81598326424571610, 30.97035057417647508 ) ) ;
#11903 = CARTESIAN_POINT ( 'NONE',  ( 0.5809828226811553087, -29.58751527316153940, -37.66417181417581617 ) ) ;
#11904 = ADVANCED_FACE ( 'NONE', ( #28415 ), #43125, .F. ) ;
#11905 = CARTESIAN_POINT ( 'NONE',  ( 0.6029443199889047422, -13.97238921213527263, 47.07770153224356591 ) ) ;
#11906 = VERTEX_POINT ( 'NONE', #28117 ) ;
#11907 = EDGE_CURVE ( 'NONE', #58000, #11842, #32842, .T. ) ;
#11908 = LINE ( 'NONE', #50395, #12982 ) ;
#11909 = ORIENTED_EDGE ( 'NONE', *, *, #10378, .T. ) ;
#11910 = VECTOR ( 'NONE', #44031, 1000.000000000000114 ) ;
#11911 = EDGE_CURVE ( 'NONE', #60182, #36274, #775, .T. ) ;
#11912 = CARTESIAN_POINT ( 'NONE',  ( 5.960721111146673579, -0.006321279846963646747, 20.52557019979492026 ) ) ;
#11913 = CARTESIAN_POINT ( 'NONE',  ( 0.5998501479064708430, -29.69975237324642237, 37.84527566984805702 ) ) ;
#11914 = ORIENTED_EDGE ( 'NONE', *, *, #29335, .T. ) ;
#11915 = CARTESIAN_POINT ( 'NONE',  ( -6.079354080745853928, 13.83171223607755174, -13.39689112691838702 ) ) ;
#11916 = ADVANCED_FACE ( 'NONE', ( #38464 ), #24255, .F. ) ;
#11917 = ORIENTED_EDGE ( 'NONE', *, *, #35439, .T. ) ;
#11918 = DIRECTION ( 'NONE',  ( -3.273063162220391312E-16, 1.000000000000000000, 1.047380211910525220E-14 ) ) ;
#11919 = CARTESIAN_POINT ( 'NONE',  ( 0.1103310638050662013, -26.18709435931501872, -34.26302445194738766 ) ) ;
#11920 = ORIENTED_EDGE ( 'NONE', *, *, #23341, .T. ) ;
#11921 = ORIENTED_EDGE ( 'NONE', *, *, #47380, .F. ) ;
#11922 = CARTESIAN_POINT ( 'NONE',  ( 4.553261556744873317, 6.787618719204111528, -43.39893775135914922 ) ) ;
#11923 = VERTEX_POINT ( 'NONE', #23421 ) ;
#11924 = B_SPLINE_CURVE_WITH_KNOTS ( 'NONE', 3,
 ( #39860, #11637, #6265, #55138 ),
 .UNSPECIFIED., .F., .F.,
 ( 4, 4 ),
 ( 0.000000000000000000, 0.004442905043737217438 ),
 .UNSPECIFIED. ) ;
#11925 = CARTESIAN_POINT ( 'NONE',  ( 0.1100053167205930632, 11.33468317718497964, 41.60823192620011923 ) ) ;
#11926 = ORIENTED_EDGE ( 'NONE', *, *, #50151, .T. ) ;
#11927 = VERTEX_POINT ( 'NONE', #42547 ) ;
#11928 = CARTESIAN_POINT ( 'NONE',  ( 0.9747592971366235703, -0.3237797888851980943, -42.90728926179870228 ) ) ;
#11929 = LINE ( 'NONE', #36043, #28429 ) ;
#11930 = CARTESIAN_POINT ( 'NONE',  ( 3.661933894777864573, 39.48007685360700947, 25.57253793789223550 ) ) ;
#11931 = EDGE_CURVE ( 'NONE', #10343, #60737, #15129, .T. ) ;
#11932 = AXIS2_PLACEMENT_3D ( 'NONE', #22478, #55979, #46611 ) ;
#11933 = CARTESIAN_POINT ( 'NONE',  ( 4.834790513006553603, 1.053669480798183011, 47.23853428663527154 ) ) ;
#11934 = PLANE ( 'NONE',  #1664 ) ;
#11935 = ORIENTED_EDGE ( 'NONE', *, *, #41997, .F. ) ;
#11936 = CARTESIAN_POINT ( 'NONE',  ( 0.1158816050234198897, -1.419926652724121441, -44.10131346803680685 ) ) ;
#11937 = DIRECTION ( 'NONE',  ( -1.000000000000000000, -1.836909530733573776E-16, 1.925929944387235579E-32 ) ) ;
#11938 = CARTESIAN_POINT ( 'NONE',  ( 2.648799415243708655, -48.79107182468955273, -4.893748408692878193 ) ) ;
#11939 = ORIENTED_EDGE ( 'NONE', *, *, #25591, .T. ) ;
#11940 = EDGE_LOOP ( 'NONE', ( #49796, #19700, #57676, #13283 ) ) ;
#11941 =( GEOMETRIC_REPRESENTATION_CONTEXT ( 3 ) GLOBAL_UNCERTAINTY_ASSIGNED_CONTEXT ( ( #359 ) ) GLOBAL_UNIT_ASSIGNED_CONTEXT ( ( #54349, #54050, #49990 ) ) REPRESENTATION_CONTEXT ( 'NONE', 'WORKASPACE' ) );
#11942 = CARTESIAN_POINT ( 'NONE',  ( 4.967162193818130511, 0.000000000000000000, 0.000000000000000000 ) ) ;
#11943 = CARTESIAN_POINT ( 'NONE',  ( 4.549368137175248350, -23.67244292351665536, 35.80950303116058819 ) ) ;
#11944 = CARTESIAN_POINT ( 'NONE',  ( 0.7764146366350244133, 36.25149456319285690, -29.76356187696567801 ) ) ;
#11945 = EDGE_LOOP ( 'NONE', ( #22727, #28585, #17992, #13372 ) ) ;
#11946 = CARTESIAN_POINT ( 'NONE',  ( 0.6000166863083090663, 40.87138819217341279, 27.22780029589465656 ) ) ;
#11947 = CARTESIAN_POINT ( 'NONE',  ( 1.231276596079887264, -37.02495017545888345, 19.65781868679367150 ) ) ;
#11948 = DIRECTION ( 'NONE',  ( 0.000000000000000000, 0.000000000000000000, -1.000000000000000000 ) ) ;
#11949 = VERTEX_POINT ( 'NONE', #18731 ) ;
#11950 = CARTESIAN_POINT ( 'NONE',  ( 2.282816707992323835, 42.71620190746931911, -19.54029326822607260 ) ) ;
#11951 = EDGE_LOOP ( 'NONE', ( #20283, #19938, #17863, #24935 ) ) ;
#11952 = CARTESIAN_POINT ( 'NONE',  ( 0.7954196712028469562, 44.09776749253654060, 19.20650004025017665 ) ) ;
#11953 = CARTESIAN_POINT ( 'NONE',  ( 0.5987334308729319599, -25.97268497059796744, -41.67712252528723127 ) ) ;
#11954 = B_SPLINE_CURVE_WITH_KNOTS ( 'NONE', 3,
 ( #49532, #11649, #16336, #58927 ),
 .UNSPECIFIED., .F., .F.,
 ( 4, 4 ),
 ( 2.071251839531113129E-17, 0.004444306975806116763 ),
 .UNSPECIFIED. ) ;
#11955 = CARTESIAN_POINT ( 'NONE',  ( -6.077587904424778920, -18.27702681447043886, -6.061873655649631765 ) ) ;
#11956 = CIRCLE ( 'NONE', #42982, 15.14599999999999369 ) ;
#11957 =( BOUNDED_SURFACE ( )  B_SPLINE_SURFACE ( 3, 1, ( 
 ( #3474, #55177 ),
 ( #7881, #46127 ),
 ( #21678, #36729 ),
 ( #16998, #45821 ) ),
 .UNSPECIFIED., .F., .F., .F. ) 
 B_SPLINE_SURFACE_WITH_KNOTS ( ( 4, 4 ),
 ( 2, 2 ),
 ( 0.000000000000000000, 1.000000000000000000 ),
 ( 0.000000000000000000, 1.000000000000000000 ),
 .UNSPECIFIED. ) 
 GEOMETRIC_REPRESENTATION_ITEM ( )  RATIONAL_B_SPLINE_SURFACE ( (
 ( 1.000000000000000000, 1.000000000000000000),
 ( 0.7211978278499968642, 0.9934217856018975334),
 ( 0.7211978278499968642, 0.9934217856018975334),
 ( 1.000000000000000000, 1.000000000000000000) ) ) 
 REPRESENTATION_ITEM ( '' )  SURFACE ( )  );
#11958 = EDGE_CURVE ( 'NONE', #873, #2365, #24898, .T. ) ;
#11959 = ORIENTED_EDGE ( 'NONE', *, *, #56272, .T. ) ;
#11960 = CARTESIAN_POINT ( 'NONE',  ( 0.9752570700956787464, 21.65368877244807067, -37.04395688491826633 ) ) ;
#11961 = DIRECTION ( 'NONE',  ( 0.000000000000000000, -0.000000000000000000, 1.000000000000000000 ) ) ;
#11962 = CARTESIAN_POINT ( 'NONE',  ( 4.962356264823608143, 22.27740539909265394, 35.70648129607319277 ) ) ;
#11963 = B_SPLINE_CURVE_WITH_KNOTS ( 'NONE', 3,
 ( #39759, #25018, #34123, #44160, #53494, #15013 ),
 .UNSPECIFIED., .F., .F.,
 ( 4, 2, 4 ),
 ( 1.252479364305869630E-17, 0.0002293755540694283640, 0.0004587511081388442056 ),
 .UNSPECIFIED. ) ;
#11964 = FACE_OUTER_BOUND ( 'NONE', #58808, .T. ) ;
#11965 = CARTESIAN_POINT ( 'NONE',  ( 4.975801465491695552, 2.564218696447496004, -47.84403947906841381 ) ) ;
#11966 = CARTESIAN_POINT ( 'NONE',  ( -6.077587904424778920, -1.842868750311569270, -19.16767738050324610 ) ) ;
#11967 = CARTESIAN_POINT ( 'NONE',  ( 0.8557997880470599172, 37.44587306708097429, 29.88293891557482951 ) ) ;
#11968 = CARTESIAN_POINT ( 'NONE',  ( 5.917102823773431552, -19.39506196288385098, -5.321775033542660793 ) ) ;
#11969 = CARTESIAN_POINT ( 'NONE',  ( 0.5806925824938499181, -13.37132486740634540, -44.94919391528445374 ) ) ;
#11970 = ORIENTED_EDGE ( 'NONE', *, *, #49580, .F. ) ;
#11971 = AXIS2_PLACEMENT_3D ( 'NONE', #54925, #31133, #50241 ) ;
#11972 = CARTESIAN_POINT ( 'NONE',  ( 2.009741617377216460, -2.780860071019173763, -43.95191571352101789 ) ) ;
#11973 = CARTESIAN_POINT ( 'NONE',  ( 0.5836750258453351492, 46.21662382526654511, 12.57171936981178995 ) ) ;
#11974 = CARTESIAN_POINT ( 'NONE',  ( 0.5800708057587394828, 44.48635630048023870, -17.74761804745354254 ) ) ;
#11975 = ORIENTED_EDGE ( 'NONE', *, *, #27473, .F. ) ;
#11976 = CARTESIAN_POINT ( 'NONE',  ( 0.5806925824938502512, -44.11884900496080775, 15.89809815106926116 ) ) ;
#11977 = CARTESIAN_POINT ( 'NONE',  ( 0.5987334363312689645, 44.50372305613552726, -20.76009490861898499 ) ) ;
#11978 = EDGE_CURVE ( 'NONE', #36339, #43965, #18916, .T. ) ;
#11979 = DIRECTION ( 'NONE',  ( 0.000000000000000000, 0.000000000000000000, 1.000000000000000000 ) ) ;
#11980 = VERTEX_POINT ( 'NONE', #53448 ) ;
#11981 = CARTESIAN_POINT ( 'NONE',  ( 4.549368137175248350, 38.40568845698277300, -19.17571786012283042 ) ) ;
#11982 = B_SPLINE_CURVE_WITH_KNOTS ( 'NONE', 3,
 ( #7207, #41094, #50748, #12568 ),
 .UNSPECIFIED., .F., .F.,
 ( 4, 4 ),
 ( 4.470280076681872512E-19, 0.002042055671079073039 ),
 .UNSPECIFIED. ) ;
#11983 = CARTESIAN_POINT ( 'NONE',  ( 0.5980894510889448457, -33.52121017007803516, -34.51330645350390824 ) ) ;
#11984 = EDGE_CURVE ( 'NONE', #18536, #34317, #45113, .T. ) ;
#11985 = ORIENTED_EDGE ( 'NONE', *, *, #24358, .T. ) ;
#11986 = B_SPLINE_CURVE_WITH_KNOTS ( 'NONE', 3,
 ( #13408, #52210, #61901, #32829 ),
 .UNSPECIFIED., .F., .F.,
 ( 4, 4 ),
 ( 2.261237429940862397E-17, 0.004564976165746191181 ),
 .UNSPECIFIED. ) ;
#11987 = CARTESIAN_POINT ( 'NONE',  ( -6.078075953587585900, -4.279696274496690656, -18.77443405392543596 ) ) ;
#11988 = ORIENTED_EDGE ( 'NONE', *, *, #5764, .T. ) ;
#11989 = ADVANCED_FACE ( 'NONE', ( #45022 ), #34697, .F. ) ;
#11990 = ORIENTED_EDGE ( 'NONE', *, *, #36382, .T. ) ;
#11991 = CARTESIAN_POINT ( 'NONE',  ( 2.301430502907646058, 42.22699195640107206, -22.89309745268846186 ) ) ;
#11992 = ORIENTED_EDGE ( 'NONE', *, *, #15032, .T. ) ;
#11993 = LINE ( 'NONE', #21055, #7033 ) ;
#11994 = VERTEX_POINT ( 'NONE', #25885 ) ;
#11995 = CARTESIAN_POINT ( 'NONE',  ( 0.9762797500689124330, -34.26226594605912368, -24.13341909939868657 ) ) ;
#11996 = AXIS2_PLACEMENT_3D ( 'NONE', #47316, #19743, #57295 ) ;
#11997 = CARTESIAN_POINT ( 'NONE',  ( 1.088908134280552664, 39.93902428011489292, 15.69861202536767131 ) ) ;
#11998 = ORIENTED_EDGE ( 'NONE', *, *, #38232, .F. ) ;
#11999 = DIRECTION ( 'NONE',  ( 0.000000000000000000, 0.000000000000000000, -1.000000000000000000 ) ) ;
#12000 = ADVANCED_FACE ( 'NONE', ( #40324 ), #38816, .T. ) ;
#12001 = CIRCLE ( 'NONE', #56990, 0.05882000000000109363 ) ;
#12002 = CARTESIAN_POINT ( 'NONE',  ( 50.50000000000000000, 12.21587082446438011, -2.649999999999992806 ) ) ;
#12003 = CARTESIAN_POINT ( 'NONE',  ( 0.1095718737110178559, -30.67477146794393761, 30.31138510522940877 ) ) ;
#12004 = DIRECTION ( 'NONE',  ( -1.000000000000000000, -1.836909530733554547E-16, -1.836909530733573529E-16 ) ) ;
#12005 = ORIENTED_EDGE ( 'NONE', *, *, #7912, .F. ) ;
#12006 = EDGE_CURVE ( 'NONE', #25025, #37013, #53276, .T. ) ;
#12007 = VERTEX_POINT ( 'NONE', #15883 ) ;
#12008 = CARTESIAN_POINT ( 'NONE',  ( 0.9730545539215883499, -42.90536227157002003, 0.5054011016611185125 ) ) ;
#12009 =( BOUNDED_SURFACE ( )  B_SPLINE_SURFACE ( 3, 1, ( 
 ( #30903, #21202 ),
 ( #11194, #34695 ),
 ( #40337, #16506 ),
 ( #40960, #35317 ) ),
 .UNSPECIFIED., .F., .F., .F. ) 
 B_SPLINE_SURFACE_WITH_KNOTS ( ( 4, 4 ),
 ( 2, 2 ),
 ( 0.000000000000000000, 1.000000000000000000 ),
 ( 0.000000000000000000, 1.000000000000000000 ),
 .UNSPECIFIED. ) 
 GEOMETRIC_REPRESENTATION_ITEM ( )  RATIONAL_B_SPLINE_SURFACE ( (
 ( 1.000000000000000000, 1.000000000000000000),
 ( 0.9729067724841187204, 0.9999501103223794596),
 ( 0.9729067724841187204, 0.9999501103223794596),
 ( 1.000000000000000000, 1.000000000000000000) ) ) 
 REPRESENTATION_ITEM ( '' )  SURFACE ( )  );
#12010 = DIRECTION ( 'NONE',  ( 0.000000000000000000, 0.000000000000000000, 1.000000000000000000 ) ) ;
#12011 = CARTESIAN_POINT ( 'NONE',  ( 1.296416391601052487, 14.17308196082959526, -41.73045796307255983 ) ) ;
#12012 = ORIENTED_EDGE ( 'NONE', *, *, #33136, .T. ) ;
#12013 = DIRECTION ( 'NONE',  ( -1.000000000000000000, -1.836909530733554547E-16, -1.836909530733573529E-16 ) ) ;
#12014 = CARTESIAN_POINT ( 'NONE',  ( 2.618530812446111078, 6.104648047582966974, -46.60965631082621030 ) ) ;
#12015 = CARTESIAN_POINT ( 'NONE',  ( 0.9762797500689124330, -17.18051571332090788, -38.22505284509149703 ) ) ;
#12016 = CARTESIAN_POINT ( 'NONE',  ( -6.010958268070873523, -11.48268200989187271, -14.94067681728561681 ) ) ;
#12017 = CIRCLE ( 'NONE', #20016, 5.612499999999999822 ) ;
#12018 = ORIENTED_EDGE ( 'NONE', *, *, #39603, .T. ) ;
#12019 = VERTEX_POINT ( 'NONE', #58445 ) ;
#12020 = CARTESIAN_POINT ( 'NONE',  ( 4.958415959904820980, 12.97383654754940530, 43.53025980924199700 ) ) ;
#12021 = CARTESIAN_POINT ( 'NONE',  ( 0.5809828226811617480, 12.92184523170268839, -46.11980934799325382 ) ) ;
#12022 = CARTESIAN_POINT ( 'NONE',  ( -6.016761891674565099, -16.31696541414265766, -9.424569481870424426 ) ) ;
#12023 = CARTESIAN_POINT ( 'NONE',  ( 0.6023142530420679819, 6.019593586345300729, -47.72938419887613293 ) ) ;
#12024 = B_SPLINE_CURVE_WITH_KNOTS ( 'NONE', 3,
 ( #40846, #44309, #12322, #40233 ),
 .UNSPECIFIED., .F., .F.,
 ( 4, 4 ),
 ( 2.168404344971008868E-19, 0.004048833967417081285 ),
 .UNSPECIFIED. ) ;
#12025 =( BOUNDED_SURFACE ( )  B_SPLINE_SURFACE ( 3, 1, ( 
 ( #33272, #42987 ),
 ( #10068, #23538 ),
 ( #9435, #28237 ),
 ( #53270, #14469 ) ),
 .UNSPECIFIED., .F., .F., .F. ) 
 B_SPLINE_SURFACE_WITH_KNOTS ( ( 4, 4 ),
 ( 2, 2 ),
 ( 0.000000000000000000, 1.000000000000000000 ),
 ( 0.000000000000000000, 1.000000000000000000 ),
 .UNSPECIFIED. ) 
 GEOMETRIC_REPRESENTATION_ITEM ( )  RATIONAL_B_SPLINE_SURFACE ( (
 ( 1.000000000000000000, 1.000000000000000000),
 ( 0.9953485035131437453, 0.8621029689291515030),
 ( 0.9953485035131437453, 0.8621029689291515030),
 ( 1.000000000000000000, 1.000000000000000000) ) ) 
 REPRESENTATION_ITEM ( '' )  SURFACE ( )  );
#12026 = EDGE_CURVE ( 'NONE', #8116, #46207, #35000, .T. ) ;
#12027 = CARTESIAN_POINT ( 'NONE',  ( 3.270143674763207553, -5.490410281242683155, -12.53844339339240754 ) ) ;
#12028 = CARTESIAN_POINT ( 'NONE',  ( 0.1368894036331273489, 25.76388777123410634, 35.82015372432938705 ) ) ;
#12029 = CARTESIAN_POINT ( 'NONE',  ( 0.6017666602106490625, 12.11361215600179975, -46.55749120190034773 ) ) ;
#12030 = CARTESIAN_POINT ( 'NONE',  ( 2.299652685299200527, -24.30812083016131808, -42.58399918472231604 ) ) ;
#12031 = DIRECTION ( 'NONE',  ( -0.07439287786467650709, -0.7830499462674556099, 0.6174937095821675381 ) ) ;
#12032 = CARTESIAN_POINT ( 'NONE',  ( 3.783198216974391404, 7.325057189011020320, -42.41041696600769484 ) ) ;
#12033 = CARTESIAN_POINT ( 'NONE',  ( 0.6067099128993204138, 29.71710940500729592, 37.56352526808316838 ) ) ;
#12034 = B_SPLINE_CURVE_WITH_KNOTS ( 'NONE', 3,
 ( #44872, #55150, #21972, #21346, #16653, #7530, #36700, #54519, #50462, #35774, #25731, #1912, #21038, #40796, #26658, #40178, #2840, #50163, #45794, #17273, #7220, #59226, #26348, #45479, #35459 ),
 .UNSPECIFIED., .F., .F.,
 ( 4, 3, 3, 3, 3, 3, 3, 3, 4 ),
 ( 5.485677294651095664E-18, 0.0005656085177311396400, 0.001131215744874498972, 0.001696821861372766133, 0.002262427090022498585, 0.002828031679238745925, 0.003393635864401604862, 0.003977030878808131623, 0.004561030005651157265 ),
 .UNSPECIFIED. ) ;
#12035 = CARTESIAN_POINT ( 'NONE',  ( 2.706805983486679335, 41.21557936162371760, -15.42893811010504912 ) ) ;
#12036 = CARTESIAN_POINT ( 'NONE',  ( 4.999999999999986677, 56.56854249492371878, 56.56854249492391062 ) ) ;
#12037 = CARTESIAN_POINT ( 'NONE',  ( 3.771699521203193850, 0.7273600638980093347, -43.95767829216813283 ) ) ;
#12038 = CARTESIAN_POINT ( 'NONE',  ( 1.227938101723756947, 10.28900963485438425, -41.66816631169181306 ) ) ;
#12039 = B_SPLINE_CURVE_WITH_KNOTS ( 'NONE', 3,
 ( #23199, #60164, #46405, #45798, #4060, #17277, #42330, #16980, #46716, #36090, #2843, #41408, #60464, #36398, #51073, #8165 ),
 .UNSPECIFIED., .F., .F.,
 ( 4, 3, 3, 3, 3, 4 ),
 ( 2.194378057379452319E-17, 0.0002612764279487728375, 0.0003919131003184776188, 0.0005225497727000641716, 0.0007837925190632419933, 0.001045051706266716084 ),
 .UNSPECIFIED. ) ;
#12040 = LINE ( 'NONE', #12648, #7460 ) ;
#12041 = DIRECTION ( 'NONE',  ( -1.000000000000000000, -0.000000000000000000, -0.000000000000000000 ) ) ;
#12042 = CARTESIAN_POINT ( 'NONE',  ( 0.9762797500689124330, -27.44172181261435739, 31.67454323498272117 ) ) ;
#12044 = EDGE_LOOP ( 'NONE', ( #23332, #38944, #2800, #41973 ) ) ;
#12043 = CARTESIAN_POINT ( 'NONE',  ( -17.97369999999976642, 0.000000000000000000, 2.099999999999994760 ) ) ;
#12045 = ORIENTED_EDGE ( 'NONE', *, *, #14501, .T. ) ;
#12046 = CARTESIAN_POINT ( 'NONE',  ( 0.6026777506516368677, 16.79643818398497501, -46.14570462100229520 ) ) ;
#12047 = CARTESIAN_POINT ( 'NONE',  ( 3.660176727303401822, -14.24118031989626232, 45.87883389004763757 ) ) ;
#12048 = CARTESIAN_POINT ( 'NONE',  ( 4.833616638992208614, 41.67905425467677816, 20.04871863793823650 ) ) ;
#12049 = EDGE_LOOP ( 'NONE', ( #45558, #43277, #15693, #7256 ) ) ;
#12050 = ORIENTED_EDGE ( 'NONE', *, *, #5352, .T. ) ;
#12051 = DIRECTION ( 'NONE',  ( 0.000000000000000000, 0.000000000000000000, 1.000000000000000000 ) ) ;
#12052 = CARTESIAN_POINT ( 'NONE',  ( 0.6846871229502899947, -13.23224427737796915, -46.04462816497500910 ) ) ;
#12053 = ORIENTED_EDGE ( 'NONE', *, *, #22087, .F. ) ;
#12054 = ORIENTED_EDGE ( 'NONE', *, *, #2082, .F. ) ;
#12055 = CARTESIAN_POINT ( 'NONE',  ( 4.975610109902397937, -28.45381238669758872, -39.78479568629688856 ) ) ;
#12056 = ADVANCED_FACE ( 'NONE', ( #20276 ), #32683, .F. ) ;
#12057 = CIRCLE ( 'NONE', #10024, 2.649999999999985700 ) ;
#12058 = CARTESIAN_POINT ( 'NONE',  ( 3.783278058412225864, -3.901118461247123470, 42.86118820526429829 ) ) ;
#12059 = CARTESIAN_POINT ( 'NONE',  ( 0.5806925824938506953, -38.96949031362410665, -26.08833430941730924 ) ) ;
#12060 = EDGE_CURVE ( 'NONE', #9726, #34790, #37556, .T. ) ;
#12061 = ORIENTED_EDGE ( 'NONE', *, *, #35203, .F. ) ;
#12062 = CARTESIAN_POINT ( 'NONE',  ( 5.965394784446460541, -20.34787558161485066, -2.693446924985554602 ) ) ;
#12063 = CARTESIAN_POINT ( 'NONE',  ( -6.078075953587585900, 16.78075473395873374, -9.444651650847566415 ) ) ;
#12064 = EDGE_CURVE ( 'NONE', #28734, #12846, #22730, .T. ) ;
#12065 = DIRECTION ( 'NONE',  ( 1.000000000000000000, -0.000000000000000000, -0.000000000000000000 ) ) ;
#12066 = ORIENTED_EDGE ( 'NONE', *, *, #59468, .T. ) ;
#12067 = ORIENTED_EDGE ( 'NONE', *, *, #29256, .T. ) ;
#12068 = FACE_OUTER_BOUND ( 'NONE', #13214, .T. ) ;
#12069 = CARTESIAN_POINT ( 'NONE',  ( 4.962356264823608143, 0.000000000000000000, 0.000000000000000000 ) ) ;
#12070 = B_SPLINE_CURVE_WITH_KNOTS ( 'NONE', 3,
 ( #44221, #30381, #1251, #20388 ),
 .UNSPECIFIED., .F., .F.,
 ( 4, 4 ),
 ( 2.787728152484798234E-17, 0.005004948556313835659 ),
 .UNSPECIFIED. ) ;
#12071 = ORIENTED_EDGE ( 'NONE', *, *, #9742, .T. ) ;
#12072 = CARTESIAN_POINT ( 'NONE',  ( 0.3676999524040366896, 37.41430475689384139, 23.36921870497834774 ) ) ;
#12073 = CARTESIAN_POINT ( 'NONE',  ( 4.956445790444027111, 14.46717203539434671, -44.81337951368921324 ) ) ;
#12074 = CARTESIAN_POINT ( 'NONE',  ( 0.5839879882012687373, 12.39635945869026834, -46.26395995854822729 ) ) ;
#12075 = B_SPLINE_CURVE_WITH_KNOTS ( 'NONE', 3,
 ( #44818, #19758, #38881, #10663 ),
 .UNSPECIFIED., .F., .F.,
 ( 4, 4 ),
 ( 0.000000000000000000, 0.004442905043737216571 ),
 .UNSPECIFIED. ) ;
#12076 = EDGE_CURVE ( 'NONE', #33012, #9955, #23763, .T. ) ;
#12077 = EDGE_LOOP ( 'NONE', ( #14003, #24435, #15988, #1699 ) ) ;
#12078 = CARTESIAN_POINT ( 'NONE',  ( 3.661933894777890330, 12.72741214118793529, -45.28403852506967553 ) ) ;
#12079 = CARTESIAN_POINT ( 'NONE',  ( 0.6030672727741701600, 18.32928433899690290, 44.47882233696930854 ) ) ;
#12080 = CARTESIAN_POINT ( 'NONE',  ( 4.833616638992208614, -34.47248434257934235, 30.83411269743503880 ) ) ;
#12081 = CARTESIAN_POINT ( 'NONE',  ( 4.956653778116975495, 14.93973939759886704, 45.71126949320255761 ) ) ;
#12082 = ORIENTED_EDGE ( 'NONE', *, *, #51837, .F. ) ;
#12083 = DIRECTION ( 'NONE',  ( 0.000000000000000000, 0.5000000000000011102, 0.8660254037844379305 ) ) ;
#12084 = CARTESIAN_POINT ( 'NONE',  ( 5.901764892641288895, -46.48816889762525761, -15.38965951493231898 ) ) ;
#12085 = CARTESIAN_POINT ( 'NONE',  ( 4.967162193818130511, -42.96271701169384016, -3.259922920618186115 ) ) ;
#12086 = CARTESIAN_POINT ( 'NONE',  ( 0.9730545539215883499, 36.90443313492330901, 21.89037132892449478 ) ) ;
#12087 = B_SPLINE_CURVE_WITH_KNOTS ( 'NONE', 3,
 ( #39007, #43707, #11100, #57435, #48991, #15488, #43394, #48373, #33991, #38387, #28961, #49289, #10790, #1352, #34913, #24574, #14573, #5436, #755 ),
 .UNSPECIFIED., .F., .F.,
 ( 4, 3, 3, 3, 3, 3, 4 ),
 ( 6.938893903907227607E-18, 0.0002724573126191799839, 0.0004086839781548505914, 0.0005449106435901909188, 0.0006811373090491549273, 0.0008459866663933714344, 0.001010840725717212282 ),
 .UNSPECIFIED. ) ;
#12088 = ORIENTED_EDGE ( 'NONE', *, *, #31753, .F. ) ;
#12089 = DIRECTION ( 'NONE',  ( -0.1736481776669314137, 0.9848077530122079093, -5.551115123125779004E-17 ) ) ;
#12090 = CARTESIAN_POINT ( 'NONE',  ( 1.231276596079881047, 20.88402890667877898, -36.34740854095476692 ) ) ;
#12091 = CARTESIAN_POINT ( 'NONE',  ( 4.975610109902397937, 47.16372689271670993, -12.96272628450527264 ) ) ;
#12092 = CARTESIAN_POINT ( 'NONE',  ( 4.962356264823608143, 0.000000000000000000, 0.000000000000000000 ) ) ;
#12093 = CARTESIAN_POINT ( 'NONE',  ( 0.5804410086790514622, 22.05813747677438741, 41.38790189066267544 ) ) ;
#12094 = VECTOR ( 'NONE', #48624, 1000.000000000000114 ) ;
#12095 = CARTESIAN_POINT ( 'NONE',  ( 0.5819845079324661441, 46.14435090135493311, -12.83441846783082418 ) ) ;
#12096 = CARTESIAN_POINT ( 'NONE',  ( -6.077587904424778920, -18.27312872431374657, -6.073614082125261326 ) ) ;
#12097 = CARTESIAN_POINT ( 'NONE',  ( 0.1104177457020373149, -41.65628910360730686, -11.15670205479989896 ) ) ;
#12098 = CARTESIAN_POINT ( 'NONE',  ( 0.5809828226811617480, 37.66417181417551774, 29.58751527316192664 ) ) ;
#12099 =( BOUNDED_SURFACE ( )  B_SPLINE_SURFACE ( 3, 1, ( 
 ( #61513, #17392 ),
 ( #28028, #4188 ),
 ( #22705, #56821 ),
 ( #13950, #33051 ) ),
 .UNSPECIFIED., .F., .F., .F. ) 
 B_SPLINE_SURFACE_WITH_KNOTS ( ( 4, 4 ),
 ( 2, 2 ),
 ( 0.000000000000000000, 1.000000000000000000 ),
 ( 0.000000000000000000, 1.000000000000000000 ),
 .UNSPECIFIED. ) 
 GEOMETRIC_REPRESENTATION_ITEM ( )  RATIONAL_B_SPLINE_SURFACE ( (
 ( 1.000000000000000000, 1.000000000000000000),
 ( 0.7282232189291693025, 0.9929344683865674037),
 ( 0.7282232189291693025, 0.9929344683865674037),
 ( 1.000000000000000000, 1.000000000000000000) ) ) 
 REPRESENTATION_ITEM ( '' )  SURFACE ( )  );
#12100 = CARTESIAN_POINT ( 'NONE',  ( 0.5834584762367746036, 27.96416347290652382, -37.64626874304744319 ) ) ;
#12101 = VERTEX_POINT ( 'NONE', #46244 ) ;
#12102 = EDGE_CURVE ( 'NONE', #44660, #4479, #16682, .T. ) ;
#12103 = DIRECTION ( 'NONE',  ( 0.07836865515943411409, -0.8672783706145228422, 0.4916162952473402958 ) ) ;
#12104 = CARTESIAN_POINT ( 'NONE',  ( -6.010958268070873523, 4.891065400978640731, -18.19761767765824700 ) ) ;
#12105 = CARTESIAN_POINT ( 'NONE',  ( 4.553261556744873317, -39.47791437445913942, 19.26223877088302672 ) ) ;
#12106 = CARTESIAN_POINT ( 'NONE',  ( 6.999999999999995559, 56.56854249492371878, 56.56854249492391062 ) ) ;
#12107 = CARTESIAN_POINT ( 'NONE',  ( 0.5786265663353153954, -46.45062944555884599, -11.69877690266703851 ) ) ;
#12108 = CARTESIAN_POINT ( 'NONE',  ( 4.291220156522060236, -11.88564107118090973, 45.58640733412488544 ) ) ;
#12109 = EDGE_CURVE ( 'NONE', #6804, #56628, #41547, .T. ) ;
#12110 = SHAPE_DEFINITION_REPRESENTATION ( #50273, #362 ) ;
#12111 = CARTESIAN_POINT ( 'NONE',  ( 4.553261556744873317, -14.95853073564509828, 41.30111286702087625 ) ) ;
#12112 = CARTESIAN_POINT ( 'NONE',  ( 0.6025881611877910160, 41.77096849334450468, -23.86454577211521411 ) ) ;
#12113 = EDGE_CURVE ( 'NONE', #33819, #13208, #9917, .T. ) ;
#12114 = CARTESIAN_POINT ( 'NONE',  ( 0.1310142868023695673, -6.259743112235846674, 42.66681113736507314 ) ) ;
#12115 = VERTEX_POINT ( 'NONE', #13046 ) ;
#12116 = ORIENTED_EDGE ( 'NONE', *, *, #3210, .F. ) ;
#12117 = CARTESIAN_POINT ( 'NONE',  ( 4.322998006666165516, -16.38761975793177683, -45.10383234877027547 ) ) ;
#12118 = CARTESIAN_POINT ( 'NONE',  ( 1.227938101723748288, 41.23019537246709376, 11.92353943227963597 ) ) ;
#12119 =( BOUNDED_SURFACE ( )  B_SPLINE_SURFACE ( 3, 1, ( 
 ( #14291, #783 ),
 ( #460, #53392 ),
 ( #24600, #53089 ),
 ( #61854, #10500 ) ),
 .UNSPECIFIED., .F., .F., .F. ) 
 B_SPLINE_SURFACE_WITH_KNOTS ( ( 4, 4 ),
 ( 2, 2 ),
 ( 0.000000000000000000, 1.000000000000000000 ),
 ( 0.000000000000000000, 1.000000000000000000 ),
 .UNSPECIFIED. ) 
 GEOMETRIC_REPRESENTATION_ITEM ( )  RATIONAL_B_SPLINE_SURFACE ( (
 ( 1.000000000000000000, 1.000000000000000000),
 ( 0.9953390228620291325, 0.8624445117760984880),
 ( 0.9953390228620291325, 0.8624445117760984880),
 ( 1.000000000000000000, 1.000000000000000000) ) ) 
 REPRESENTATION_ITEM ( '' )  SURFACE ( )  );
#12120 = ORIENTED_EDGE ( 'NONE', *, *, #55504, .F. ) ;
#12121 = DIRECTION ( 'NONE',  ( 0.000000000000000000, 0.000000000000000000, -1.000000000000000000 ) ) ;
#12122 = CARTESIAN_POINT ( 'NONE',  ( 5.959828726073459926, -18.96145866559666615, -7.858992891710077089 ) ) ;
#12123 = CARTESIAN_POINT ( 'NONE',  ( 0.1103310638050662013, 41.67627416617914093, -11.08182869403250947 ) ) ;
#12124 = EDGE_LOOP ( 'NONE', ( #19912, #19211, #22237, #55809 ) ) ;
#12125 = ORIENTED_EDGE ( 'NONE', *, *, #25159, .F. ) ;
#12126 = CARTESIAN_POINT ( 'NONE',  ( 2.299652685299201860, 21.52981099345398519, 44.05393244018406307 ) ) ;
#12127 = EDGE_CURVE ( 'NONE', #59574, #33107, #17414, .T. ) ;
#12128 = CARTESIAN_POINT ( 'NONE',  ( 3.660087539126826606, -22.37124151181825127, 42.51124390328611469 ) ) ;
#12129 = CARTESIAN_POINT ( 'NONE',  ( 0.8560838555295223751, -42.27062166135446120, -20.33635607586480631 ) ) ;
#12130 = ORIENTED_EDGE ( 'NONE', *, *, #1264, .F. ) ;
#12131 = B_SPLINE_CURVE_WITH_KNOTS ( 'NONE', 3,
 ( #33392, #142, #38406, #57452 ),
 .UNSPECIFIED., .F., .F.,
 ( 4, 4 ),
 ( 2.501853776554200607E-17, 0.005004948556313833924 ),
 .UNSPECIFIED. ) ;
#12132 = ORIENTED_EDGE ( 'NONE', *, *, #10753, .F. ) ;
#12133 = FACE_OUTER_BOUND ( 'NONE', #11422, .T. ) ;
#12134 = EDGE_CURVE ( 'NONE', #53679, #60046, #47791, .T. ) ;
#12135 = CARTESIAN_POINT ( 'NONE',  ( 4.958415959904818315, 24.86570830293410594, 38.01184689561967645 ) ) ;
#12136 = ORIENTED_EDGE ( 'NONE', *, *, #53041, .F. ) ;
#12137 = VECTOR ( 'NONE', #2273, 1000.000000000000000 ) ;
#12138 = FACE_OUTER_BOUND ( 'NONE', #59901, .T. ) ;
#12139 = FACE_OUTER_BOUND ( 'NONE', #48808, .T. ) ;
#12140 = VERTEX_POINT ( 'NONE', #8300 ) ;
#12141 = DIRECTION ( 'NONE',  ( 1.000000000000000000, 1.836909530733573776E-16, 0.000000000000000000 ) ) ;
#12142 = CARTESIAN_POINT ( 'NONE',  ( 5.958863334805807099, 0.001220270595885530451, 20.52565293643016275 ) ) ;
#12143 = B_SPLINE_CURVE_WITH_KNOTS ( 'NONE', 3,
 ( #58908, #6893, #20407, #19799, #15097, #16023 ),
 .UNSPECIFIED., .F., .F.,
 ( 4, 2, 4 ),
 ( 1.167014589833948395E-16, 0.0002448718616795945600, 0.0004897437233590723514 ),
 .UNSPECIFIED. ) ;
#12144 = EDGE_LOOP ( 'NONE', ( #49020, #49610, #43695, #37166 ) ) ;
#12145 = CARTESIAN_POINT ( 'NONE',  ( 2.526552050251863690, -27.11558601691289638, 33.34585601411856715 ) ) ;
#12146 = CARTESIAN_POINT ( 'NONE',  ( 0.5830081025819928708, -19.49199439610001150, 42.65318497890458360 ) ) ;
#12147 = CARTESIAN_POINT ( 'NONE',  ( -6.203732170862584994, -1.182048853166489222, 5.744326400484686099E-14 ) ) ;
#12148 = EDGE_CURVE ( 'NONE', #46817, #1532, #47302, .T. ) ;
#12149 = VERTEX_POINT ( 'NONE', #27420 ) ;
#12150 = CARTESIAN_POINT ( 'NONE',  ( 2.624215991343608501, 19.66774719433037788, -43.79392271049049867 ) ) ;
#12151 = CARTESIAN_POINT ( 'NONE',  ( 0.1073791018717578927, -42.81622261970997556, 5.147744207006151207 ) ) ;
#12152 = ORIENTED_EDGE ( 'NONE', *, *, #13665, .T. ) ;
#12153 = ORIENTED_EDGE ( 'NONE', *, *, #30185, .F. ) ;
#12154 = CARTESIAN_POINT ( 'NONE',  ( 0.9784957157296387820, 4.426412977119490222, 41.67421175197387129 ) ) ;
#12155 = ORIENTED_EDGE ( 'NONE', *, *, #8954, .F. ) ;
#12156 = DIRECTION ( 'NONE',  ( 0.09835009131224566048, 0.4908642831975245091, 0.8656670924898630659 ) ) ;
#12157 = CARTESIAN_POINT ( 'NONE',  ( 0.5998501479064708430, -17.92509395669076966, -44.64337787626241294 ) ) ;
#12158 = CARTESIAN_POINT ( 'NONE',  ( 0.1154773475650539977, -43.73856127446700981, 5.820815036214034954 ) ) ;
#12159 = VERTEX_POINT ( 'NONE', #46550 ) ;
#12160 = CARTESIAN_POINT ( 'NONE',  ( 0.5987334308729318488, -8.434467990461143927, -48.37791496424389948 ) ) ;
#12161 = CARTESIAN_POINT ( 'NONE',  ( 3.270143674763207553, 8.548517033725252290, 10.69018354892890876 ) ) ;
#12162 = FACE_OUTER_BOUND ( 'NONE', #37238, .T. ) ;
#12163 = ORIENTED_EDGE ( 'NONE', *, *, #22100, .F. ) ;
#12164 = ORIENTED_EDGE ( 'NONE', *, *, #9425, .T. ) ;
#12165 = DIRECTION ( 'NONE',  ( 1.000000000000000000, 0.000000000000000000, 0.000000000000000000 ) ) ;
#12166 = CARTESIAN_POINT ( 'NONE',  ( 4.960386119450145515, 23.14534831554981764, -37.13124447179514931 ) ) ;
#12167 = DIRECTION ( 'NONE',  ( 0.07439287786467665975, -0.8701500408883711124, 0.4871392060437932936 ) ) ;
#12168 = CARTESIAN_POINT ( 'NONE',  ( 0.1097557419366048670, -5.849988371690785449, -42.72583172879051716 ) ) ;
#12169 = CARTESIAN_POINT ( 'NONE',  ( 0.5804410086790514622, -29.86002002114410558, 36.16488706179337953 ) ) ;
#12170 = CARTESIAN_POINT ( 'NONE',  ( 0.1313383488274126321, 41.81465294768271690, 10.54394128763572702 ) ) ;
#12171 = ORIENTED_EDGE ( 'NONE', *, *, #37160, .T. ) ;
#12172 = CARTESIAN_POINT ( 'NONE',  ( 2.528190830796657629, -40.03694634880724124, 12.62129403887486134 ) ) ;
#12173 = FACE_OUTER_BOUND ( 'NONE', #56944, .T. ) ;
#12174 = VERTEX_POINT ( 'NONE', #7057 ) ;
#12175 = EDGE_CURVE ( 'NONE', #48936, #41808, #22112, .T. ) ;
#12176 = CYLINDRICAL_SURFACE ( 'NONE', #18940, 10.00000000000000000 ) ;
#12177 = CARTESIAN_POINT ( 'NONE',  ( 0.1368894036331290698, -38.75424303169170059, -21.09431138871115508 ) ) ;
#12178 = CARTESIAN_POINT ( 'NONE',  ( 0.6029443449137436017, 44.22536370377634540, 21.34611775597693395 ) ) ;
#12179 = CARTESIAN_POINT ( 'NONE',  ( 4.975801465491695552, -31.15993731089151808, 36.39623109580413285 ) ) ;
#12180 = FACE_OUTER_BOUND ( 'NONE', #43213, .T. ) ;
#12181 = DIRECTION ( 'NONE',  ( 0.000000000000000000, 0.000000000000000000, -1.000000000000000000 ) ) ;
#12182 = VECTOR ( 'NONE', #4246, 1000.000000000000000 ) ;
#12183 = CARTESIAN_POINT ( 'NONE',  ( 5.917102823773431552, -2.021675920617120870, 20.01006108245896442 ) ) ;
#12184 = ADVANCED_FACE ( 'NONE', ( #3596 ), #27791, .T. ) ;
#12185 = CARTESIAN_POINT ( 'NONE',  ( 0.6017666602106490625, 38.37783452831165931, 29.00829887116083583 ) ) ;
#12186 = AXIS2_PLACEMENT_3D ( 'NONE', #10488, #29583, #5748 ) ;
#12187 = CARTESIAN_POINT ( 'NONE',  ( 0.5850706913938533704, -33.73916126769427848, -33.99603398296626011 ) ) ;
#12188 = CARTESIAN_POINT ( 'NONE',  ( 0.7048096507298635682, -46.24547838151377732, 13.26491767067435390 ) ) ;
#12189 = EDGE_CURVE ( 'NONE', #35220, #57870, #35815, .T. ) ;
#12190 = CARTESIAN_POINT ( 'NONE',  ( 4.967162193818130511, -8.839793687085512275, 42.16965968614191240 ) ) ;
#12191 = DIRECTION ( 'NONE',  ( 1.000000000000000000, 0.000000000000000000, 0.000000000000000000 ) ) ;
#12192 = ADVANCED_FACE ( 'NONE', ( #2369 ), #21809, .F. ) ;
#12193 = CARTESIAN_POINT ( 'NONE',  ( 5.917102823773431552, 3.336722021764624291, -19.83320458728778135 ) ) ;
#12194 = CARTESIAN_POINT ( 'NONE',  ( 3.727782113643637096, 17.17182055185172374, 40.47105576632487356 ) ) ;
#12195 = CARTESIAN_POINT ( 'NONE',  ( 1.000433927950262092, -7.619417497986461285, -41.21120181023874096 ) ) ;
#12196 = LINE ( 'NONE', #7136, #22678 ) ;
#12197 =( BOUNDED_SURFACE ( )  B_SPLINE_SURFACE ( 3, 1, ( 
 ( #44312, #21400 ),
 ( #39607, #49279 ),
 ( #16708, #30470 ),
 ( #35827, #35208 ) ),
 .UNSPECIFIED., .F., .F., .F. ) 
 B_SPLINE_SURFACE_WITH_KNOTS ( ( 4, 4 ),
 ( 2, 2 ),
 ( 0.000000000000000000, 1.000000000000000000 ),
 ( 0.000000000000000000, 1.000000000000000000 ),
 .UNSPECIFIED. ) 
 GEOMETRIC_REPRESENTATION_ITEM ( )  RATIONAL_B_SPLINE_SURFACE ( (
 ( 1.000000000000000000, 1.000000000000000000),
 ( 0.7211978278499970862, 0.9934217856018976445),
 ( 0.7211978278499970862, 0.9934217856018976445),
 ( 1.000000000000000000, 1.000000000000000000) ) ) 
 REPRESENTATION_ITEM ( '' )  SURFACE ( )  );
#12198 = EDGE_CURVE ( 'NONE', #61727, #4551, #16810, .T. ) ;
#12199 = VERTEX_POINT ( 'NONE', #40945 ) ;
#12200 = CARTESIAN_POINT ( 'NONE',  ( 5.896278296736517710, -2.018661446113838132, 20.01129644926478335 ) ) ;
#12201 = EDGE_CURVE ( 'NONE', #50810, #12769, #38332, .T. ) ;
#12202 = CARTESIAN_POINT ( 'NONE',  ( 0.1095718737110177865, 43.12372487139541732, 0.2569529612659335327 ) ) ;
#12203 = CARTESIAN_POINT ( 'NONE',  ( 0.9740398440564312921, -26.44872719679347739, -33.78760696452732049 ) ) ;
#12204 = CARTESIAN_POINT ( 'NONE',  ( 0.5998501479064708430, 18.89267974119668025, -44.24259072156067418 ) ) ;
#12205 = VERTEX_POINT ( 'NONE', #60006 ) ;
#12206 = CARTESIAN_POINT ( 'NONE',  ( 4.975801465491695552, 14.85979367497174408, -45.55012473237738391 ) ) ;
#12207 = CARTESIAN_POINT ( 'NONE',  ( 0.3676999524040366896, -26.85386693986640338, 34.99743438737744583 ) ) ;
#12208 = B_SPLINE_CURVE_WITH_KNOTS ( 'NONE', 3,
 ( #32119, #13323, #60590, #36833 ),
 .UNSPECIFIED., .F., .F.,
 ( 4, 4 ),
 ( 0.000000000000000000, 0.004446298630425082367 ),
 .UNSPECIFIED. ) ;
#12209 = CARTESIAN_POINT ( 'NONE',  ( 0.1129192098497455998, 43.99990943031669843, 3.310552508129313232 ) ) ;
#12210 = EDGE_LOOP ( 'NONE', ( #13364, #61000, #45200, #41573 ) ) ;
#12211 = B_SPLINE_CURVE_WITH_KNOTS ( 'NONE', 3,
 ( #32561, #22840, #18773, #13449 ),
 .UNSPECIFIED., .F., .F.,
 ( 4, 4 ),
 ( 0.000000000000000000, 0.005014147105413704723 ),
 .UNSPECIFIED. ) ;
#12212 = CARTESIAN_POINT ( 'NONE',  ( 4.549368137175248350, 8.166781970325150297, 42.14271863032836762 ) ) ;
#12213 = EDGE_LOOP ( 'NONE', ( #28458, #2286 ) ) ;
#12214 = CARTESIAN_POINT ( 'NONE',  ( 0.6001305935487315502, 29.70149728382386201, 37.84751346122865101 ) ) ;
#12215 = CARTESIAN_POINT ( 'NONE',  ( 0.6041374136657476912, 34.14050483116091783, 33.89363087703058852 ) ) ;
#12216 = EDGE_LOOP ( 'NONE', ( #20680, #47590, #34927, #1288 ) ) ;
#12217 = CARTESIAN_POINT ( 'NONE',  ( -6.078726893082806448, 13.83492043373111180, -13.39361854993076406 ) ) ;
#12218 = ORIENTED_EDGE ( 'NONE', *, *, #36955, .F. ) ;
#12219 = CARTESIAN_POINT ( 'NONE',  ( 0.6064782688330849769, 42.89335125862529452, 18.96034979168258516 ) ) ;
#12220 = CARTESIAN_POINT ( 'NONE',  ( 1.000110580585051201, 41.61827148400551835, -4.933250597274972726 ) ) ;
#12221 = ADVANCED_FACE ( 'NONE', ( #38096 ), #15487, .F. ) ;
#12222 = ORIENTED_EDGE ( 'NONE', *, *, #41831, .T. ) ;
#12223 = CARTESIAN_POINT ( 'NONE',  ( 2.648799415243708655, -34.24682227764526488, 35.09519379021831043 ) ) ;
#12224 = ORIENTED_EDGE ( 'NONE', *, *, #35105, .F. ) ;
#12225 = CARTESIAN_POINT ( 'NONE',  ( 0.1152809850208375703, -1.635316795157891745, 44.09388870885884160 ) ) ;
#12226 = ADVANCED_FACE ( 'NONE', ( #43093 ), #37093, .F. ) ;
#12227 = ORIENTED_EDGE ( 'NONE', *, *, #55119, .T. ) ;
#12228 = ORIENTED_EDGE ( 'NONE', *, *, #27751, .T. ) ;
#12229 = CARTESIAN_POINT ( 'NONE',  ( 0.9754402186311946776, -0.1875553420608594424, -42.90805920318128130 ) ) ;
#12230 = CARTESIAN_POINT ( 'NONE',  ( -2.739355103387248747, -13.93362462427441706, -5.357394122223096744 ) ) ;
#12231 = CARTESIAN_POINT ( 'NONE',  ( 0.5997462898726536595, -25.90236585764231947, -41.72072714036939090 ) ) ;
#12232 = CARTESIAN_POINT ( 'NONE',  ( -31.75000000000000000, -15.43999999999999240, 1.890854657883512518E-15 ) ) ;
#12233 = CARTESIAN_POINT ( 'NONE',  ( 0.8551540677456715978, 33.23105123575899711, 34.52115452272941098 ) ) ;
#12234 = ORIENTED_EDGE ( 'NONE', *, *, #21236, .F. ) ;
#12235 = CARTESIAN_POINT ( 'NONE',  ( 3.894904216938897878, 6.429595949874166827, 43.48315338608232850 ) ) ;
#12236 = CARTESIAN_POINT ( 'NONE',  ( 5.974727161628367256, 19.82156119440445607, -5.327229920347220649 ) ) ;
#12237 = FACE_OUTER_BOUND ( 'NONE', #61933, .T. ) ;
#12238 = EDGE_LOOP ( 'NONE', ( #42457, #52541, #7305, #39555 ) ) ;
#12239 = EDGE_LOOP ( 'NONE', ( #34703, #37985, #42407, #50597 ) ) ;
#12240 = DIRECTION ( 'NONE',  ( -1.000000000000000000, -0.000000000000000000, -0.000000000000000000 ) ) ;
#12241 = FACE_OUTER_BOUND ( 'NONE', #5817, .T. ) ;
#12242 = CARTESIAN_POINT ( 'NONE',  ( 0.5806925824938499181, -44.47729014209976128, 14.86583411581871772 ) ) ;
#12243 = ORIENTED_EDGE ( 'NONE', *, *, #50824, .F. ) ;
#12244 = CARTESIAN_POINT ( 'NONE',  ( 4.962356264823608143, 0.000000000000000000, 0.000000000000000000 ) ) ;
#12245 = CARTESIAN_POINT ( 'NONE',  ( 1.479689385636123067, -34.59735853788245663, 27.28748114921756596 ) ) ;
#12246 = ORIENTED_EDGE ( 'NONE', *, *, #14261, .T. ) ;
#12247 = LINE ( 'NONE', #40159, #30933 ) ;
#12248 = ORIENTED_EDGE ( 'NONE', *, *, #18718, .F. ) ;
#12249 = FACE_OUTER_BOUND ( 'NONE', #6946, .T. ) ;
#12250 = CARTESIAN_POINT ( 'NONE',  ( 0.9730545539215883499, -34.34678117142574649, 25.71816799638765971 ) ) ;
#12251 = DIRECTION ( 'NONE',  ( -1.000000000000000000, 0.000000000000000000, 0.000000000000000000 ) ) ;
#12252 = EDGE_CURVE ( 'NONE', #48937, #20219, #5755, .T. ) ;
#12253 = LINE ( 'NONE', #55746, #31822 ) ;
#12254 = ORIENTED_EDGE ( 'NONE', *, *, #9533, .T. ) ;
#12255 = CARTESIAN_POINT ( 'NONE',  ( 1.157643937452368821, 10.51841477362188471, 40.57542637169456157 ) ) ;
#12256 = CARTESIAN_POINT ( 'NONE',  ( 3.782625744892851749, -10.79728826547640530, 40.62827427060136642 ) ) ;
#12257 = EDGE_CURVE ( 'NONE', #56898, #58292, #6099, .T. ) ;
#12258 = CARTESIAN_POINT ( 'NONE',  ( 2.624215991343620935, 37.21129343241644705, -30.33228621714997431 ) ) ;
#12259 = ADVANCED_FACE ( 'NONE', ( #9548 ), #49500, .F. ) ;
#12260 = CARTESIAN_POINT ( 'NONE',  ( 0.1103878639767399417, -16.54784522866442842, -39.82320122342697744 ) ) ;
#12261 = B_SPLINE_CURVE_WITH_KNOTS ( 'NONE', 3,
 ( #18762, #36957, #37889, #23754 ),
 .UNSPECIFIED., .F., .F.,
 ( 4, 4 ),
 ( 0.000000000000000000, 0.005013413432710145910 ),
 .UNSPECIFIED. ) ;
#12262 = EDGE_CURVE ( 'NONE', #23932, #1177, #7743, .T. ) ;
#12263 = CARTESIAN_POINT ( 'NONE',  ( 4.694002226626920127, -45.51532087759709810, -2.576885107160872490 ) ) ;
#12264 = CARTESIAN_POINT ( 'NONE',  ( 0.9730545539215883499, 41.57420493492384850, 10.61654491617579055 ) ) ;
#12265 = CARTESIAN_POINT ( 'NONE',  ( 0.5786265663353196143, -44.52624106864154641, 17.66171603226064590 ) ) ;
#12266 = CARTESIAN_POINT ( 'NONE',  ( 5.965394784446460541, -17.76824826579347416, -10.27521535480980219 ) ) ;
#12267 = B_SPLINE_CURVE_WITH_KNOTS ( 'NONE', 3,
 ( #29040, #38457, #5206, #24337, #37222, #13409 ),
 .UNSPECIFIED., .F., .F.,
 ( 4, 2, 4 ),
 ( 1.192622389734054877E-18, 0.0002293801035737094533, 0.0004587602071474177140 ),
 .UNSPECIFIED. ) ;
#12268 = DIRECTION ( 'NONE',  ( 0.000000000000000000, 0.000000000000000000, 1.000000000000000000 ) ) ;
#12269 = VECTOR ( 'NONE', #36730, 1000.000000000000000 ) ;
#12270 = ADVANCED_FACE ( 'NONE', ( #18355 ), #10809, .F. ) ;
#12271 = CARTESIAN_POINT ( 'NONE',  ( 0.9762797500689124330, 19.69530149098714489, -36.99215976885945167 ) ) ;
#12272 = CARTESIAN_POINT ( 'NONE',  ( 0.6039202388192952409, 28.23800208753110752, -40.17684595576886153 ) ) ;
#12273 = VERTEX_POINT ( 'NONE', #4826 ) ;
#12274 = CARTESIAN_POINT ( 'NONE',  ( 3.238018933889920792, 12.84302458974300443, 3.803184422942107901 ) ) ;
#12275 = DIRECTION ( 'NONE',  ( -0.07500201931887527651, -0.01982172072489229997, 0.9969863572213991665 ) ) ;
#12276 = CARTESIAN_POINT ( 'NONE',  ( 0.1129192098497455998, -18.30288010335110016, 40.14917642626692640 ) ) ;
#12277 = VERTEX_POINT ( 'NONE', #52766 ) ;
#12278 = CARTESIAN_POINT ( 'NONE',  ( 0.5809828226811553087, -46.11980934799348830, 12.92184523170186594 ) ) ;
#12279 = CARTESIAN_POINT ( 'NONE',  ( 0.1140933569871964010, 3.859258926286197156, 43.95515977247479356 ) ) ;
#12280 = CARTESIAN_POINT ( 'NONE',  ( 0.6009453534118439633, -12.02914401651140786, -46.57942464365170565 ) ) ;
#12281 = ORIENTED_EDGE ( 'NONE', *, *, #60017, .F. ) ;
#12282 = CARTESIAN_POINT ( 'NONE',  ( 0.9730545539215883499, 10.61654491617563423, 41.57420493492389113 ) ) ;
#12283 = B_SPLINE_CURVE_WITH_KNOTS ( 'NONE', 3,
 ( #30956, #50064, #22176, #4268, #31571, #46612 ),
 .UNSPECIFIED., .F., .F.,
 ( 4, 2, 4 ),
 ( 0.000000000000000000, 0.0002291966416970788345, 0.0004583932833941576691 ),
 .UNSPECIFIED. ) ;
#12284 = CARTESIAN_POINT ( 'NONE',  ( 5.901463166500146684, -18.51103891486777542, 7.865068889265228513 ) ) ;
#12285 = CARTESIAN_POINT ( 'NONE',  ( 3.376099380956838925, 13.21675742563009770, 2.241808819707602041 ) ) ;
#12286 = ORIENTED_EDGE ( 'NONE', *, *, #35859, .F. ) ;
#12287 = CARTESIAN_POINT ( 'NONE',  ( 5.959828726073459926, 12.49160845136013265, 16.28681682518067930 ) ) ;
#12288 = VERTEX_POINT ( 'NONE', #28970 ) ;
#12289 = ORIENTED_EDGE ( 'NONE', *, *, #40543, .F. ) ;
#12290 = CARTESIAN_POINT ( 'NONE',  ( 0.8560838555295158248, 21.73747136795142154, 41.56747734237938374 ) ) ;
#12291 = ORIENTED_EDGE ( 'NONE', *, *, #2251, .F. ) ;
#12292 = CARTESIAN_POINT ( 'NONE',  ( 5.958863334805807099, 0.001220270596169137139, -20.52565293643016275 ) ) ;
#12293 = ORIENTED_EDGE ( 'NONE', *, *, #19755, .T. ) ;
#12294 = DIRECTION ( 'NONE',  ( 0.1024043820194936033, -0.9239750460186124670, -0.3684880688409171157 ) ) ;
#12295 = ADVANCED_FACE ( 'NONE', ( #37161 ), #43493, .F. ) ;
#12296 = CARTESIAN_POINT ( 'NONE',  ( 0.8744876279028306332, 40.65405044375329879, -27.52450240960324024 ) ) ;
#12297 = ORIENTED_EDGE ( 'NONE', *, *, #19731, .F. ) ;
#12298 = CARTESIAN_POINT ( 'NONE',  ( 10.00000000000000533, 1.836909530733574959E-15, -1.925929944387237167E-31 ) ) ;
#12299 = CARTESIAN_POINT ( 'NONE',  ( 0.8551540677456715978, 46.03951182599426772, 13.28067116677218529 ) ) ;
#12300 = CARTESIAN_POINT ( 'NONE',  ( 3.376099380956842921, -4.408915724532880276, -12.65977273753497379 ) ) ;
#12301 = CARTESIAN_POINT ( 'NONE',  ( 0.6000166863083090663, -7.321729200002740967, -48.56146376737711989 ) ) ;
#12302 = EDGE_LOOP ( 'NONE', ( #20306, #18435, #56648, #34130 ) ) ;
#12303 = CARTESIAN_POINT ( 'NONE',  ( 0.7056313189692702270, 43.50197882008412620, 17.53072966805745381 ) ) ;
#12304 = ORIENTED_EDGE ( 'NONE', *, *, #24690, .F. ) ;
#12305 = PRESENTATION_LAYER_ASSIGNMENT (  '', '', ( #61275 ) ) ;
#12306 = CARTESIAN_POINT ( 'NONE',  ( 5.981074661064941900, 12.48781255314267113, 16.28853686865603123 ) ) ;
#12307 = CARTESIAN_POINT ( 'NONE',  ( 0.9758171775293912331, 26.12572690811914455, 34.03798695362321070 ) ) ;
#12308 =( BOUNDED_SURFACE ( )  B_SPLINE_SURFACE ( 3, 1, ( 
 ( #6690, #44970 ),
 ( #59332, #30834 ),
 ( #11132, #15520 ),
 ( #39652, #25215 ) ),
 .UNSPECIFIED., .F., .F., .F. ) 
 B_SPLINE_SURFACE_WITH_KNOTS ( ( 4, 4 ),
 ( 2, 2 ),
 ( 0.000000000000000000, 1.000000000000000000 ),
 ( 0.000000000000000000, 1.000000000000000000 ),
 .UNSPECIFIED. ) 
 GEOMETRIC_REPRESENTATION_ITEM ( )  RATIONAL_B_SPLINE_SURFACE ( (
 ( 1.000000000000000000, 1.000000000000000000),
 ( 0.7223157951917476005, 0.9931996967497186413),
 ( 0.7223157951917476005, 0.9931996967497186413),
 ( 1.000000000000000000, 1.000000000000000000) ) ) 
 REPRESENTATION_ITEM ( '' )  SURFACE ( )  );
#12309 = CARTESIAN_POINT ( 'NONE',  ( -2.708315649062910779, -10.53288422393062795, 10.16016146078271198 ) ) ;
#12310 = ORIENTED_EDGE ( 'NONE', *, *, #37099, .F. ) ;
#12311 = CARTESIAN_POINT ( 'NONE',  ( 3.783278058412224976, -29.18720354295066599, 31.62921638229657262 ) ) ;
#12312 = CARTESIAN_POINT ( 'NONE',  ( 0.6000166863083106206, -1.051715750664326876, 49.09905676984292455 ) ) ;
#12313 = CARTESIAN_POINT ( 'NONE',  ( 4.226256110419179812, 7.420606375272879696, -43.31006639351232934 ) ) ;
#12314 = ORIENTED_EDGE ( 'NONE', *, *, #27036, .T. ) ;
#12315 = ORIENTED_EDGE ( 'NONE', *, *, #47815, .T. ) ;
#12316 = CARTESIAN_POINT ( 'NONE',  ( 0.9769922540276048117, -39.44262731837918068, -14.16371085943138297 ) ) ;
#12317 = CARTESIAN_POINT ( 'NONE',  ( 0.1103878639767399139, 34.24245495762985314, 26.21398130517529168 ) ) ;
#12318 = CARTESIAN_POINT ( 'NONE',  ( 0.9756008150404607004, -16.28894658522360217, 39.69644259322203084 ) ) ;
#12319 = CARTESIAN_POINT ( 'NONE',  ( 0.8554163680231720024, 44.99993935735625428, -13.27444654010398928 ) ) ;
#12320 = EDGE_CURVE ( 'NONE', #9811, #3346, #47968, .T. ) ;
#12321 = AXIS2_PLACEMENT_3D ( 'NONE', #38939, #10098, #25416 ) ;
#12322 = CARTESIAN_POINT ( 'NONE',  ( 3.783198216974386963, -12.79806054635163370, 41.09147814699338852 ) ) ;
#12323 = B_SPLINE_CURVE_WITH_KNOTS ( 'NONE', 3,
 ( #30262, #58139, #5816, #49373 ),
 .UNSPECIFIED., .F., .F.,
 ( 4, 4 ),
 ( 6.254634441385501517E-18, 0.004566006591234645501 ),
 .UNSPECIFIED. ) ;
#12324 = CARTESIAN_POINT ( 'NONE',  ( 3.319141568766058814, -12.31039395171775830, -1.199999999999999956 ) ) ;
#12325 = EDGE_CURVE ( 'NONE', #55726, #516, #61534, .T. ) ;
#12326 = CARTESIAN_POINT ( 'NONE',  ( 0.6025881611877910160, 12.66175293297402504, -46.41131722377296853 ) ) ;
#12327 = CARTESIAN_POINT ( 'NONE',  ( 5.896782393890504181, -15.78847575145224447, 12.45994062280461634 ) ) ;
#12328 = EDGE_CURVE ( 'NONE', #31835, #8537, #39788, .T. ) ;
#12329 = EDGE_CURVE ( 'NONE', #30486, #61495, #60582, .T. ) ;
#12330 = CARTESIAN_POINT ( 'NONE',  ( 0.8744876279028263033, 43.84003649649913115, 22.09980204357308153 ) ) ;
#12331 = CARTESIAN_POINT ( 'NONE',  ( 4.553261556744875094, 0.000000000000000000, 0.000000000000000000 ) ) ;
#12332 = CARTESIAN_POINT ( 'NONE',  ( 0.5786265663353196143, -11.69877690266622317, -46.45062944555905204 ) ) ;
#12333 = CARTESIAN_POINT ( 'NONE',  ( 3.390910168358336918, 41.07524454790360124, -15.71373354310021142 ) ) ;
#12334 = CARTESIAN_POINT ( 'NONE',  ( 4.962356264823608143, 0.000000000000000000, 0.000000000000000000 ) ) ;
#12335 = CARTESIAN_POINT ( 'NONE',  ( 5.960721111146673579, 20.34914600876575363, -2.685391721745826299 ) ) ;
#12336 = CARTESIAN_POINT ( 'NONE',  ( 0.9788927965476029724, -22.43074396039533269, 35.40054149324505062 ) ) ;
#12337 = CARTESIAN_POINT ( 'NONE',  ( 5.960721111146673579, -18.96073515164543011, -7.860635756377828187 ) ) ;
#12338 = CARTESIAN_POINT ( 'NONE',  ( 0.6024113833632039894, 16.75552346327387809, 46.16052753784931895 ) ) ;
#12339 = CARTESIAN_POINT ( 'NONE',  ( 0.6028618097248863439, 46.42282207635403068, -12.61968633793867411 ) ) ;
#12341 = ORIENTED_EDGE ( 'NONE', *, *, #45144, .T. ) ;
#12340 = CARTESIAN_POINT ( 'NONE',  ( 5.894904586330512508, 17.95171060118299522, 9.070032996247425316 ) ) ;
#12342 = ORIENTED_EDGE ( 'NONE', *, *, #54399, .T. ) ;
#12343 = EDGE_CURVE ( 'NONE', #23714, #25486, #21000, .T. ) ;
#12344 = DIRECTION ( 'NONE',  ( -0.07500201931887527651, -0.4319596767211244526, -0.8987688995426313943 ) ) ;
#12345 = CARTESIAN_POINT ( 'NONE',  ( 2.185380717157383135, 2.793969434617936010, -43.94329912359357593 ) ) ;
#12346 = CARTESIAN_POINT ( 'NONE',  ( 0.6254311100348668440, 34.49956326955417296, -33.52633430496194933 ) ) ;
#12347 = ORIENTED_EDGE ( 'NONE', *, *, #18676, .F. ) ;
#12348 = EDGE_CURVE ( 'NONE', #41175, #1146, #38999, .T. ) ;
#12349 = ORIENTED_EDGE ( 'NONE', *, *, #47053, .F. ) ;
#12350 = CARTESIAN_POINT ( 'NONE',  ( 4.956445790443998689, -10.39006634428300835, 45.93021414603936847 ) ) ;
#12352 = CARTESIAN_POINT ( 'NONE',  ( 4.956445790443988031, 0.000000000000000000, 0.000000000000000000 ) ) ;
#12351 = B_SPLINE_CURVE_WITH_KNOTS ( 'NONE', 3,
 ( #20101, #48897, #19479, #9753, #15400, #11009, #5949, #44233, #25087, #30090, #43609, #43295, #20399, #28860, #5642, #6251 ),
 .UNSPECIFIED., .F., .F.,
 ( 4, 3, 3, 3, 3, 4 ),
 ( 2.194378057379452319E-17, 0.0002618515315864391037, 0.0003927756766341967986, 0.0005236998216950561552, 0.0007855159896329881640, 0.001047349442285927653 ),
 .UNSPECIFIED. ) ;
#12353 = AXIS2_PLACEMENT_3D ( 'NONE', #49691, #36237, #11815 ) ;
#12354 = UNCERTAINTY_MEASURE_WITH_UNIT (LENGTH_MEASURE( 1.000000000000000082E-05 ), #30532, 'distance_accuracy_value', 'NONE');
#12355 = EDGE_LOOP ( 'NONE', ( #23619, #5783, #18210, #61785 ) ) ;
#12356 = VERTEX_POINT ( 'NONE', #34295 ) ;
#12357 = CARTESIAN_POINT ( 'NONE',  ( 4.967162193818130511, 0.000000000000000000, 0.000000000000000000 ) ) ;
#12358 = CARTESIAN_POINT ( 'NONE',  ( 0.5850706913938534814, 44.31965802246106279, 18.16120156791897244 ) ) ;
#12359 = CARTESIAN_POINT ( 'NONE',  ( 5.917102823773431552, -11.93691330175311194, 16.18640846136571199 ) ) ;
#12360 = EDGE_LOOP ( 'NONE', ( #41549, #17525, #27601, #25517 ) ) ;
#12361 = CARTESIAN_POINT ( 'NONE',  ( 4.975801465491694664, -32.01766832630337944, 35.64402118370901462 ) ) ;
#12362 = AXIS2_PLACEMENT_3D ( 'NONE', #1062, #24577, #34916 ) ;
#12363 = CARTESIAN_POINT ( 'NONE',  ( -6.015611763856276717, 18.20278301740936655, 4.870987357968240339 ) ) ;
#12364 =( BOUNDED_SURFACE ( )  B_SPLINE_SURFACE ( 3, 1, ( 
 ( #20910, #36263 ),
 ( #40663, #12451 ),
 ( #31541, #60335 ),
 ( #57171, #38125 ) ),
 .UNSPECIFIED., .F., .F., .F. ) 
 B_SPLINE_SURFACE_WITH_KNOTS ( ( 4, 4 ),
 ( 2, 2 ),
 ( 0.000000000000000000, 1.000000000000000000 ),
 ( 0.000000000000000000, 1.000000000000000000 ),
 .UNSPECIFIED. ) 
 GEOMETRIC_REPRESENTATION_ITEM ( )  RATIONAL_B_SPLINE_SURFACE ( (
 ( 1.000000000000000000, 1.000000000000000000),
 ( 0.9952954269826590483, 0.8620686068821339365),
 ( 0.9952954269826590483, 0.8620686068821339365),
 ( 1.000000000000000000, 1.000000000000000000) ) ) 
 REPRESENTATION_ITEM ( '' )  SURFACE ( )  );
#12365 = EDGE_CURVE ( 'NONE', #55302, #12174, #8329, .T. ) ;
#12366 = DIRECTION ( 'NONE',  ( 0.000000000000000000, 0.000000000000000000, 1.000000000000000000 ) ) ;
#12367 = VERTEX_POINT ( 'NONE', #58071 ) ;
#12368 = ORIENTED_EDGE ( 'NONE', *, *, #34617, .F. ) ;
#12369 = CARTESIAN_POINT ( 'NONE',  ( 1.154321485836935723, -29.75729673892721650, 30.92445806269068242 ) ) ;
#12370 = B_SPLINE_CURVE_WITH_KNOTS ( 'NONE', 3,
 ( #35789, #31691, #60477, #55786, #12909, #40494, #40192, #32005, #36408, #55474, #26059, #2854, #30747, #46117, #41117, #54534, #2549, #49865, #6925 ),
 .UNSPECIFIED., .F., .F.,
 ( 4, 3, 3, 3, 3, 3, 4 ),
 ( 1.301113191146877164E-18, 0.0002612768053151710043, 0.0003919133833142906544, 0.0005225499612322604282, 0.0006531865391693357416, 0.0008112755173415182311, 0.0009693688056799726815 ),
 .UNSPECIFIED. ) ;
#12371 = ORIENTED_EDGE ( 'NONE', *, *, #15288, .T. ) ;
#12372 = DIRECTION ( 'NONE',  ( -1.000000000000000000, 0.000000000000000000, 0.000000000000000000 ) ) ;
#12373 = CARTESIAN_POINT ( 'NONE',  ( 0.6028618097248862329, 33.89350006451827824, -34.14037999462335193 ) ) ;
#12374 = CARTESIAN_POINT ( 'NONE',  ( 4.956445790443998689, -23.10347171912865250, 41.03373788314999615 ) ) ;
#12375 = LINE ( 'NONE', #59963, #31394 ) ;
#12376 = ORIENTED_EDGE ( 'NONE', *, *, #34050, .T. ) ;
#12377 = CARTESIAN_POINT ( 'NONE',  ( 0.9730545539215883499, -30.69604515769629316, -29.98130006528894498 ) ) ;
#12378 = CARTESIAN_POINT ( 'NONE',  ( 0.6027935024548038978, 18.24855952726166564, 44.51201578381234469 ) ) ;
#12379 =( BOUNDED_SURFACE ( )  B_SPLINE_SURFACE ( 3, 1, ( 
 ( #15811, #11113 ),
 ( #30196, #1990 ),
 ( #36699, #6360 ),
 ( #46102, #25494 ) ),
 .UNSPECIFIED., .F., .F., .F. ) 
 B_SPLINE_SURFACE_WITH_KNOTS ( ( 4, 4 ),
 ( 2, 2 ),
 ( 0.000000000000000000, 1.000000000000000000 ),
 ( 0.000000000000000000, 1.000000000000000000 ),
 .UNSPECIFIED. ) 
 GEOMETRIC_REPRESENTATION_ITEM ( )  RATIONAL_B_SPLINE_SURFACE ( (
 ( 1.000000000000000000, 1.000000000000000000),
 ( 0.9953040768229005630, 0.8617119497784937465),
 ( 0.9953040768229005630, 0.8617119497784937465),
 ( 1.000000000000000000, 1.000000000000000000) ) ) 
 REPRESENTATION_ITEM ( '' )  SURFACE ( )  );
#12380 = CARTESIAN_POINT ( 'NONE',  ( 0.1092355843206037486, 39.95589129953367546, -16.22491322981586492 ) ) ;
#12381 = ORIENTED_EDGE ( 'NONE', *, *, #54682, .T. ) ;
#12382 = CARTESIAN_POINT ( 'NONE',  ( 0.3676999524040323597, 16.00695768809450215, -41.10629986868669761 ) ) ;
#12383 = CARTESIAN_POINT ( 'NONE',  ( 0.8554163680231720024, -29.58718577084438905, 36.41159034254562954 ) ) ;
#12384 = CARTESIAN_POINT ( 'NONE',  ( 4.960156602257181468, -46.28683144126593874, -3.546989772330372492 ) ) ;
#12385 = PRESENTATION_STYLE_ASSIGNMENT (( #12696 ) ) ;
#12386 = ORIENTED_EDGE ( 'NONE', *, *, #59594, .T. ) ;
#12387 = CARTESIAN_POINT ( 'NONE',  ( -1.200000000000006617, 8.239576745513313235E-16, 6.728125000000022560 ) ) ;
#12388 = CARTESIAN_POINT ( 'NONE',  ( 0.8554163680231708922, 37.37991192211431724, -28.35397075908055697 ) ) ;
#12389 = CARTESIAN_POINT ( 'NONE',  ( -0.2999999999999999889, -13.49666625504239015, 0.000000000000000000 ) ) ;
#12390 = AXIS2_PLACEMENT_3D ( 'NONE', #16459, #20548, #10530 ) ;
#12391 = CARTESIAN_POINT ( 'NONE',  ( 5.959828726073459926, -19.82738831247216993, 5.308046411394905739 ) ) ;
#12392 = CARTESIAN_POINT ( 'NONE',  ( 0.5824936645240089694, -46.81422852104944354, 2.768788005476148673 ) ) ;
#12393 =( REPRESENTATION_RELATIONSHIP ('NONE','NONE', #44881, #53251 ) REPRESENTATION_RELATIONSHIP_WITH_TRANSFORMATION ( #44319 )SHAPE_REPRESENTATION_RELATIONSHIP( ) );
#12394 = CARTESIAN_POINT ( 'NONE',  ( 3.782625744892853525, -24.05484086317139614, -34.47611833055603370 ) ) ;
#12395 = CARTESIAN_POINT ( 'NONE',  ( 0.9736507210033057413, -5.153758453069271717, -42.59776535855984747 ) ) ;
#12396 = EDGE_CURVE ( 'NONE', #35884, #40578, #21777, .T. ) ;
#12397 = CARTESIAN_POINT ( 'NONE',  ( 0.5839879882012686263, 37.99844431214167884, 29.15719377327458872 ) ) ;
#12398 = CARTESIAN_POINT ( 'NONE',  ( 0.5804410086790514622, 10.33990028284759966, 45.74501408892737686 ) ) ;
#12399 = ORIENTED_EDGE ( 'NONE', *, *, #257, .T. ) ;
#12400 = EDGE_CURVE ( 'NONE', #17235, #10372, #10798, .T. ) ;
#12401 = CARTESIAN_POINT ( 'NONE',  ( 0.1129192098497447394, -43.82135468580274562, -5.161459220630158384 ) ) ;
#12402 = CARTESIAN_POINT ( 'NONE',  ( 0.7948878604505692502, 32.36187211755012783, -36.92435348581946641 ) ) ;
#12403 = CARTESIAN_POINT ( 'NONE',  ( 2.528190830796654964, 41.42606007575643901, 6.792325283202126585 ) ) ;
#12404 = DIRECTION ( 'NONE',  ( 1.000000000000000000, 0.000000000000000000, 0.000000000000000000 ) ) ;
#12405 = VECTOR ( 'NONE', #30373, 1000.000000000000227 ) ;
#12406 = DIRECTION ( 'NONE',  ( 0.000000000000000000, 0.000000000000000000, 1.000000000000000000 ) ) ;
#12407 = CARTESIAN_POINT ( 'NONE',  ( 0.9790320750461900534, -31.13925818481557073, 28.04788284775852603 ) ) ;
#12408 = APPLICATION_PROTOCOL_DEFINITION ( 'draft international standard', 'automotive_design', 1998, #26741 ) ;
#12409 = CARTESIAN_POINT ( 'NONE',  ( 4.967162193818130511, 3.259922920617742914, 42.96271701169386859 ) ) ;
#12410 = CARTESIAN_POINT ( 'NONE',  ( 0.9785694773339252972, -7.190011144658855713, 41.28727582990130429 ) ) ;
#12411 = CARTESIAN_POINT ( 'NONE',  ( 0.6000166863083106206, -43.04473087058023850, 23.64264422580037461 ) ) ;
#12412 = ORIENTED_EDGE ( 'NONE', *, *, #27510, .T. ) ;
#12413 = ORIENTED_EDGE ( 'NONE', *, *, #37228, .F. ) ;
#12414 = FACE_OUTER_BOUND ( 'NONE', #49191, .T. ) ;
#12415 = CARTESIAN_POINT ( 'NONE',  ( 4.553261556744875094, -20.11719049292643646, -39.04917684785361587 ) ) ;
#12416 = CARTESIAN_POINT ( 'NONE',  ( 0.5835871038041858805, -7.934817416658265010, 46.21983476242418476 ) ) ;
#12417 = CARTESIAN_POINT ( 'NONE',  ( 2.299652685299201860, 38.15857472714130694, -30.79293587255566322 ) ) ;
#12418 = EDGE_CURVE ( 'NONE', #30761, #45872, #33000, .T. ) ;
#12419 = CARTESIAN_POINT ( 'NONE',  ( 5.272379999999998290, 1.538011871406776419E-15, -12.55882000000000076 ) ) ;
#12420 = DIRECTION ( 'NONE',  ( -1.000000000000000000, -0.000000000000000000, -0.000000000000000000 ) ) ;
#12421 = CARTESIAN_POINT ( 'NONE',  ( 0.1073791018717578927, 41.77800844988514939, -10.69234304550012027 ) ) ;
#12422 = ORIENTED_EDGE ( 'NONE', *, *, #36799, .T. ) ;
#12423 = ORIENTED_EDGE ( 'NONE', *, *, #52292, .T. ) ;
#12424 = DIRECTION ( 'NONE',  ( 0.000000000000000000, 0.000000000000000000, -1.000000000000000000 ) ) ;
#12425 = CARTESIAN_POINT ( 'NONE',  ( 0.1098349054025746230, -39.75970464594254139, -16.69989664087441028 ) ) ;
#12426 = CARTESIAN_POINT ( 'NONE',  ( 0.6029303876144825880, 41.59667219751848677, 24.16699908817976450 ) ) ;
#12427 = VERTEX_POINT ( 'NONE', #43718 ) ;
#12428 = AXIS2_PLACEMENT_3D ( 'NONE', #25100, #1274, #39536 ) ;
#12429 = CARTESIAN_POINT ( 'NONE',  ( 2.299746137290199499, 26.98651929683142114, -40.93909029189441640 ) ) ;
#12430 = CARTESIAN_POINT ( 'NONE',  ( 4.960386119450136633, 28.60674280242237799, 33.10726099979272874 ) ) ;
#12431 = ORIENTED_EDGE ( 'NONE', *, *, #22921, .F. ) ;
#12432 = B_SPLINE_CURVE_WITH_KNOTS ( 'NONE', 3,
 ( #1509, #11245, #58518, #49143 ),
 .UNSPECIFIED., .F., .F.,
 ( 4, 4 ),
 ( 0.000000000000000000, 0.004442905043737218305 ),
 .UNSPECIFIED. ) ;
#12433 = CARTESIAN_POINT ( 'NONE',  ( 4.975801465491694664, -9.906103548668557579, 46.87746200127438101 ) ) ;
#12434 = CARTESIAN_POINT ( 'NONE',  ( 0.1157506346131639274, 33.65821932553335927, 28.53182313903419143 ) ) ;
#12435 = ORIENTED_EDGE ( 'NONE', *, *, #55490, .T. ) ;
#12436 = CARTESIAN_POINT ( 'NONE',  ( 0.1129192098497447394, -12.08918212651769686, 42.43587472053614817 ) ) ;
#12437 = CARTESIAN_POINT ( 'NONE',  ( 3.407937589446174087, 7.970324840161956637, 11.14158115674376148 ) ) ;
#12438 = ORIENTED_EDGE ( 'NONE', *, *, #12348, .T. ) ;
#12439 = LINE ( 'NONE', #2704, #10511 ) ;
#12440 = CARTESIAN_POINT ( 'NONE',  ( 5.965394784446458765, 20.52536205633085231, -0.01447339372431907453 ) ) ;
#12441 = CARTESIAN_POINT ( 'NONE',  ( 0.5819845901640494645, 41.70428411658559043, -23.55368560422299140 ) ) ;
#12442 = CARTESIAN_POINT ( 'NONE',  ( -5.995132425357893702, 16.32377331145333699, -9.414704407577630718 ) ) ;
#12443 = B_SPLINE_CURVE_WITH_KNOTS ( 'NONE', 3,
 ( #47861, #29349, #53450, #14348, #34080, #4910 ),
 .UNSPECIFIED., .F., .F.,
 ( 4, 2, 4 ),
 ( 8.558167549966216424E-17, 0.0002293366620881469092, 0.0004586733241762082748 ),
 .UNSPECIFIED. ) ;
#12444 = AXIS2_PLACEMENT_3D ( 'NONE', #8503, #42666, #13861 ) ;
#12445 = ORIENTED_EDGE ( 'NONE', *, *, #34037, .F. ) ;
#12447 = EDGE_CURVE ( 'NONE', #11449, #45029, #25490, .T. ) ;
#12446 = ORIENTED_EDGE ( 'NONE', *, *, #28361, .F. ) ;
#12448 = CARTESIAN_POINT ( 'NONE',  ( 1.214306433183764966E-14, 4.618802153517020059, 0.000000000000000000 ) ) ;
#12449 = CARTESIAN_POINT ( 'NONE',  ( 0.6009453534118439633, 44.61081284455531204, -18.00606795643230029 ) ) ;
#12450 = ORIENTED_EDGE ( 'NONE', *, *, #29300, .F. ) ;
#12451 = CARTESIAN_POINT ( 'NONE',  ( 0.5782707292762442330, -19.08336439318344802, -42.84345407579313303 ) ) ;
#12452 = VERTEX_POINT ( 'NONE', #6663 ) ;
#12453 = DIRECTION ( 'NONE',  ( -0.07500201931887529039, 0.08636880102339446197, -0.9934360207420870337 ) ) ;
#12454 = ADVANCED_FACE ( 'NONE', ( #44944 ), #19585, .T. ) ;
#12455 = ORIENTED_EDGE ( 'NONE', *, *, #7507, .F. ) ;
#12456 = CARTESIAN_POINT ( 'NONE',  ( 4.967162193818130511, -40.93989340068600313, -13.42934394584206359 ) ) ;
#12457 = CARTESIAN_POINT ( 'NONE',  ( 0.6027444965799114707, -48.68737225085462939, -6.409235460969727960 ) ) ;
#12458 = CARTESIAN_POINT ( 'NONE',  ( 0.1092565886968785566, -26.00565248013079156, 34.40108480122206203 ) ) ;
#12459 = ORIENTED_EDGE ( 'NONE', *, *, #51327, .T. ) ;
#12460 = CARTESIAN_POINT ( 'NONE',  ( -6.016489644550737204, 17.41053539857209742, -7.206912786933101778 ) ) ;
#12461 = CARTESIAN_POINT ( 'NONE',  ( 4.962356264823608143, 0.000000000000000000, 0.000000000000000000 ) ) ;
#12462 = CARTESIAN_POINT ( 'NONE',  ( -6.063463321072278589, 0.6327935495819126954, -19.24629898975586073 ) ) ;
#12463 = ORIENTED_EDGE ( 'NONE', *, *, #32042, .F. ) ;
#12464 = EDGE_LOOP ( 'NONE', ( #16584, #53415 ) ) ;
#12465 = CARTESIAN_POINT ( 'NONE',  ( -1.400000000000000799, 0.000000000000000000, -7.400000000000021672 ) ) ;
#12466 = CARTESIAN_POINT ( 'NONE',  ( 4.962356264823602814, 22.27740539909316198, -35.70648129607287302 ) ) ;
#12467 = B_SPLINE_CURVE_WITH_KNOTS ( 'NONE', 3,
 ( #7148, #50094, #49780, #30051, #26276, #54144, #21587, #45414, #40725, #11905, #6214, #21280, #15973, #30662, #1526, #59795 ),
 .UNSPECIFIED., .F., .F.,
 ( 4, 3, 3, 3, 3, 4 ),
 ( 2.194378057379452319E-17, 0.0002612764279487737591, 0.0003919131003184764261, 0.0005225497727000642800, 0.0007837925190632450290, 0.001045051706266714132 ),
 .UNSPECIFIED. ) ;
#12468 = CARTESIAN_POINT ( 'NONE',  ( 0.9791128995231602739, 38.58122919918244520, -16.36539604550769411 ) ) ;
#12469 = AXIS2_PLACEMENT_3D ( 'NONE', #6821, #45098, #49147 ) ;
#12470 = CARTESIAN_POINT ( 'NONE',  ( 0.1098349054025746369, -5.417317591399518406, -42.78286259078961962 ) ) ;
#12471 = CARTESIAN_POINT ( 'NONE',  ( 0.6254311100348641794, -11.78487556908975264, -46.64066536338336988 ) ) ;
#12472 = ORIENTED_EDGE ( 'NONE', *, *, #21522, .T. ) ;
#12473 = EDGE_CURVE ( 'NONE', #28574, #37964, #58354, .T. ) ;
#12474 = CARTESIAN_POINT ( 'NONE',  ( 0.1103878639767399694, 37.32258098927768231, -21.60424693647518168 ) ) ;
#12475 = DIRECTION ( 'NONE',  ( 0.000000000000000000, -1.000000000000000000, 1.224646799147349509E-16 ) ) ;
#12476 = ORIENTED_EDGE ( 'NONE', *, *, #42809, .T. ) ;
#12477 = ADVANCED_FACE ( 'NONE', ( #16727 ), #28273, .F. ) ;
#12478 = CARTESIAN_POINT ( 'NONE',  ( 0.9730545539215883499, -29.98130006528883129, 30.69604515769640329 ) ) ;
#12479 = CARTESIAN_POINT ( 'NONE',  ( 0.9769922540276050338, -27.39328719377936494, 31.71654728694862158 ) ) ;
#12480 = CARTESIAN_POINT ( 'NONE',  ( 7.000000000000016875, -54.69470952477976766, 58.44237546506786884 ) ) ;
#12481 = CARTESIAN_POINT ( 'NONE',  ( 0.1158816050234199313, -42.67963805895574581, 11.19779158859894252 ) ) ;
#12482 = CARTESIAN_POINT ( 'NONE',  ( 0.7056555295713289322, -47.37451042924659106, 7.085402321211620169 ) ) ;
#12483 = CARTESIAN_POINT ( 'NONE',  ( -6.072942160501519027, 9.994728154871472370, -16.45933083084606352 ) ) ;
#12484 = CARTESIAN_POINT ( 'NONE',  ( 0.6026777506516367566, 4.888802969756627981, 48.86354465406822811 ) ) ;
#12485 = ADVANCED_FACE ( 'NONE', ( #31751 ), #2606, .F. ) ;
#12486 = CARTESIAN_POINT ( 'NONE',  ( 0.1149546198390367924, -12.29174268441242113, -42.37758401328954250 ) ) ;
#12487 =( BOUNDED_SURFACE ( )  B_SPLINE_SURFACE ( 3, 1, ( 
 ( #4320, #37583 ),
 ( #38202, #13454 ),
 ( #9663, #18155 ),
 ( #32566, #51643 ) ),
 .UNSPECIFIED., .F., .F., .F. ) 
 B_SPLINE_SURFACE_WITH_KNOTS ( ( 4, 4 ),
 ( 2, 2 ),
 ( 0.000000000000000000, 1.000000000000000000 ),
 ( 0.000000000000000000, 1.000000000000000000 ),
 .UNSPECIFIED. ) 
 GEOMETRIC_REPRESENTATION_ITEM ( )  RATIONAL_B_SPLINE_SURFACE ( (
 ( 1.000000000000000000, 1.000000000000000000),
 ( 0.9953390228620291325, 0.8624445117761032620),
 ( 0.9953390228620291325, 0.8624445117761032620),
 ( 1.000000000000000000, 1.000000000000000000) ) ) 
 REPRESENTATION_ITEM ( '' )  SURFACE ( )  );
#12488 = CARTESIAN_POINT ( 'NONE',  ( 0.9756008150404598123, -39.58764833544687889, 16.55159915785265667 ) ) ;
#12489 = CARTESIAN_POINT ( 'NONE',  ( 0.6000166863083106206, -34.91285637184653012, -34.53861522509651394 ) ) ;
#12490 = CONICAL_SURFACE ( 'NONE', #18469, 43.92652462719577500, 1.486293639869522343 ) ;
#12491 = CARTESIAN_POINT ( 'NONE',  ( 0.5807400328401574052, -18.83234461715214181, 44.04145271122558825 ) ) ;
#12492 = DIRECTION ( 'NONE',  ( 0.09835009131224567436, 0.7847759187265459513, 0.6119264800004807769 ) ) ;
#12493 = VECTOR ( 'NONE', #21098, 1000.000000000000000 ) ;
#12494 = DIRECTION ( 'NONE',  ( 0.09722883295013597105, -0.9952333609815530169, -0.007557197398263266856 ) ) ;
#12495 = FILL_AREA_STYLE ('',( #38852 ) ) ;
#12496 = CARTESIAN_POINT ( 'NONE',  ( 0.5837374860065631665, -24.10515569139019831, -41.38807031854337737 ) ) ;
#12497 = EDGE_CURVE ( 'NONE', #26349, #44905, #61359, .T. ) ;
#12498 = AXIS2_PLACEMENT_3D ( 'NONE', #22776, #35746, #11948 ) ;
#12499 = CARTESIAN_POINT ( 'NONE',  ( -48.95476116535499500, 1.530808498934191127E-15, 12.50000000000000000 ) ) ;
#12500 = CARTESIAN_POINT ( 'NONE',  ( 0.9762797500689124330, 38.77779312671030709, 15.89363222827819300 ) ) ;
#12501 = ORIENTED_EDGE ( 'NONE', *, *, #9381, .F. ) ;
#12502 = CARTESIAN_POINT ( 'NONE',  ( 0.8554163680231720024, 3.785871848717075494, -46.76401017296218043 ) ) ;
#12503 = CARTESIAN_POINT ( 'NONE',  ( 4.322998006666165516, 30.86725474310359729, -36.74401119231377777 ) ) ;
#12504 = CARTESIAN_POINT ( 'NONE',  ( 0.5997462898726536595, -47.63132954987522538, -11.95023328037962251 ) ) ;
#12505 = CARTESIAN_POINT ( 'NONE',  ( -2.739355103387247858, -12.87605224490601330, -7.553465796405506971 ) ) ;
#12506 = ORIENTED_EDGE ( 'NONE', *, *, #26342, .F. ) ;
#12507 = CARTESIAN_POINT ( 'NONE',  ( 2.879087469061463178, -40.10403664819293112, 18.10436194136033450 ) ) ;
#12508 = CARTESIAN_POINT ( 'NONE',  ( 6.559176281257887098, -8.489993063321520594, 3.632288619156076459E-16 ) ) ;
#12509 = B_SPLINE_CURVE_WITH_KNOTS ( 'NONE', 3,
 ( #746, #38998, #19264, #38381, #5429, #9852 ),
 .UNSPECIFIED., .F., .F.,
 ( 4, 2, 4 ),
 ( 2.224043620450101781E-17, 0.0002293755540694328906, 0.0004587511081388435008 ),
 .UNSPECIFIED. ) ;
#12510 = CARTESIAN_POINT ( 'NONE',  ( 5.917102823773431552, 16.58597737984205622, 11.37519548874259279 ) ) ;
#12511 = ORIENTED_EDGE ( 'NONE', *, *, #44454, .T. ) ;
#12512 = AXIS2_PLACEMENT_3D ( 'NONE', #28417, #47547, #56615 ) ;
#12513 = B_SPLINE_CURVE_WITH_KNOTS ( 'NONE', 3,
 ( #8834, #53716, #30237, #16162 ),
 .UNSPECIFIED., .F., .F.,
 ( 4, 4 ),
 ( 0.000000000000000000, 0.005004948556313809638 ),
 .UNSPECIFIED. ) ;
#12514 = CARTESIAN_POINT ( 'NONE',  ( 7.000000000000016875, -54.69470952477895764, -58.44237546506863623 ) ) ;
#12515 = ORIENTED_EDGE ( 'NONE', *, *, #40707, .F. ) ;
#12516 = EDGE_CURVE ( 'NONE', #41236, #22780, #14356, .T. ) ;
#12517 = FACE_OUTER_BOUND ( 'NONE', #56422, .T. ) ;
#12518 = DIRECTION ( 'NONE',  ( -1.000000000000000000, -0.000000000000000000, -0.000000000000000000 ) ) ;
#12519 = VERTEX_POINT ( 'NONE', #26418 ) ;
#12520 = DIRECTION ( 'NONE',  ( 0.000000000000000000, 0.7071067811865395791, 0.7071067811865553443 ) ) ;
#12521 = ORIENTED_EDGE ( 'NONE', *, *, #58285, .F. ) ;
#12522 = DIRECTION ( 'NONE',  ( -1.000000000000000000, -0.000000000000000000, -0.000000000000000000 ) ) ;
#12523 = CARTESIAN_POINT ( 'NONE',  ( 1.091591847532195070, 41.63653874899925711, -4.812237728845413898 ) ) ;
#12524 = ADVANCED_FACE ( 'NONE', ( #50232 ), #41121, .F. ) ;
#12525 = ORIENTED_EDGE ( 'NONE', *, *, #1966, .T. ) ;
#12526 = EDGE_CURVE ( 'NONE', #46592, #22531, #7551, .T. ) ;
#12527 = CARTESIAN_POINT ( 'NONE',  ( 2.643462169533600914, -25.20536747735808447, 40.89244134039068257 ) ) ;
#12528 = ORIENTED_EDGE ( 'NONE', *, *, #48528, .F. ) ;
#12529 = CARTESIAN_POINT ( 'NONE',  ( 0.1140933569871964287, -1.793286609244197027, 44.08779959604483878 ) ) ;
#12530 = AXIS2_PLACEMENT_3D ( 'NONE', #569, #59122, #48501 ) ;
#12531 = VERTEX_POINT ( 'NONE', #17043 ) ;
#12532 = EDGE_CURVE ( 'NONE', #40338, #32714, #31434, .T. ) ;
#12533 = ORIENTED_EDGE ( 'NONE', *, *, #7334, .F. ) ;
#12534 = CARTESIAN_POINT ( 'NONE',  ( 0.7954190325252802340, 34.61997719899436987, 33.39101560460813545 ) ) ;
#12535 = CARTESIAN_POINT ( 'NONE',  ( 0.7762777257811902532, 43.90991299786900015, 19.15108781300947172 ) ) ;
#12536 = CARTESIAN_POINT ( 'NONE',  ( 2.301529144917015213, -4.990866136406990172, 47.77346141661142553 ) ) ;
#12537 = FACE_OUTER_BOUND ( 'NONE', #56777, .T. ) ;
#12538 = DIRECTION ( 'NONE',  ( 0.09835009131224552170, -0.7847759187265582748, 0.6119264800004649008 ) ) ;
#12539 = VERTEX_POINT ( 'NONE', #55846 ) ;
#12540 = CARTESIAN_POINT ( 'NONE',  ( 0.9730545539215883499, 10.61654491617563423, 41.57420493492389113 ) ) ;
#12541 = CARTESIAN_POINT ( 'NONE',  ( 0.8554163680231816613, -42.27859581856498750, -20.34025095032602692 ) ) ;
#12542 = CARTESIAN_POINT ( 'NONE',  ( 0.5797568665920712627, -34.35528743026003440, 31.92083229156293811 ) ) ;
#12543 = VECTOR ( 'NONE', #2016, 1000.000000000000000 ) ;
#12544 = ORIENTED_EDGE ( 'NONE', *, *, #11476, .F. ) ;
#12545 = VERTEX_POINT ( 'NONE', #36156 ) ;
#12546 = CARTESIAN_POINT ( 'NONE',  ( 0.3622758884714600280, -33.69533458712325569, -26.89560658783373626 ) ) ;
#12547 = CARTESIAN_POINT ( 'NONE',  ( 4.335381028904216727, 24.52155563981566289, 42.40813785899788968 ) ) ;
#12548 = CARTESIAN_POINT ( 'NONE',  ( 1.000433927950263868, 40.24156067008907200, -11.70621512224969329 ) ) ;
#12549 = EDGE_LOOP ( 'NONE', ( #12555, #47018, #38484, #13893 ) ) ;
#12550 = CARTESIAN_POINT ( 'NONE',  ( 0.1073791018717483448, -42.81622261970991161, -5.147744207006710759 ) ) ;
#12551 = FACE_OUTER_BOUND ( 'NONE', #23797, .T. ) ;
#12552 = EDGE_CURVE ( 'NONE', #6090, #43360, #46421, .T. ) ;
#12553 = VERTEX_POINT ( 'NONE', #32066 ) ;
#12554 = CARTESIAN_POINT ( 'NONE',  ( 5.880360259849752858, -31.66572319753586839, 36.03610316515328549 ) ) ;
#12555 = ORIENTED_EDGE ( 'NONE', *, *, #49779, .F. ) ;
#12556 = ADVANCED_FACE ( 'NONE', ( #51144 ), #47720, .T. ) ;
#12557 = CARTESIAN_POINT ( 'NONE',  ( 5.958863334805807099, 14.51296551801802970, -14.51469124124464827 ) ) ;
#12558 = CARTESIAN_POINT ( 'NONE',  ( 0.6252788684277231779, -26.04119143542666848, -41.63292783119062790 ) ) ;
#12559 = CARTESIAN_POINT ( 'NONE',  ( 0.8551540677456834771, 47.37911285756630519, -7.157691013573882266 ) ) ;
#12560 = EDGE_CURVE ( 'NONE', #5530, #12519, #22044, .T. ) ;
#12561 = CARTESIAN_POINT ( 'NONE',  ( 4.975610109902397937, 35.53430708602537891, 33.61193875773635398 ) ) ;
#12562 =( BOUNDED_SURFACE ( )  B_SPLINE_SURFACE ( 3, 1, ( 
 ( #46761, #56740 ),
 ( #61127, #8831 ),
 ( #47669, #14174 ),
 ( #22947, #33278 ) ),
 .UNSPECIFIED., .F., .F., .F. ) 
 B_SPLINE_SURFACE_WITH_KNOTS ( ( 4, 4 ),
 ( 2, 2 ),
 ( 0.000000000000000000, 1.000000000000000000 ),
 ( 0.000000000000000000, 1.000000000000000000 ),
 .UNSPECIFIED. ) 
 GEOMETRIC_REPRESENTATION_ITEM ( )  RATIONAL_B_SPLINE_SURFACE ( (
 ( 1.000000000000000000, 1.000000000000000000),
 ( 0.9953390228620291325, 0.8624445117760984880),
 ( 0.9953390228620291325, 0.8624445117760984880),
 ( 1.000000000000000000, 1.000000000000000000) ) ) 
 REPRESENTATION_ITEM ( '' )  SURFACE ( )  );
#12563 = EDGE_LOOP ( 'NONE', ( #40733, #47878, #24085, #56657 ) ) ;
#12564 = CARTESIAN_POINT ( 'NONE',  ( 0.7246131072078569879, 37.65685186358352610, 29.92944207473665585 ) ) ;
#12565 = CARTESIAN_POINT ( 'NONE',  ( 0.5807400328401637335, 38.33001520688989672, -28.72484455891601840 ) ) ;
#12566 = LINE ( 'NONE', #3134, #36874 ) ;
#12567 = CARTESIAN_POINT ( 'NONE',  ( -6.078726893082806448, -1.852420388636412119, -19.16670498475114570 ) ) ;
#12568 = CARTESIAN_POINT ( 'NONE',  ( 2.788021980263895028, 5.971756191165462832E-15, 46.99417130740431503 ) ) ;
#12569 = CARTESIAN_POINT ( 'NONE',  ( 0.5804410086790514622, -45.84731009780866628, 9.876437042312842252 ) ) ;
#12570 = CARTESIAN_POINT ( 'NONE',  ( -1.500000000000001332, 0.000000000000000000, 0.000000000000000000 ) ) ;
#12571 = ADVANCED_FACE ( 'NONE', ( #56764 ), #11098, .F. ) ;
#12572 = DIRECTION ( 'NONE',  ( 0.000000000000000000, 0.7071067811865421326, 0.7071067811865527908 ) ) ;
#12573 = CARTESIAN_POINT ( 'NONE',  ( -1.129531546211723025, 0.000000000000000000, -5.612499999999999822 ) ) ;
#12574 = B_SPLINE_CURVE_WITH_KNOTS ( 'NONE', 3,
 ( #27118, #34756, #10951, #46242, #20647, #50600 ),
 .UNSPECIFIED., .F., .F.,
 ( 4, 2, 4 ),
 ( 4.336808689942017736E-19, 0.0002291459268755700993, 0.0004582918537511397649 ),
 .UNSPECIFIED. ) ;
#12575 = EDGE_CURVE ( 'NONE', #38564, #21005, #37699, .T. ) ;
#12576 = VECTOR ( 'NONE', #32464, 1000.000000000000114 ) ;
#12577 = CARTESIAN_POINT ( 'NONE',  ( 0.8554163680231816613, 45.48289776771366633, 11.51136324522541443 ) ) ;
#12578 = CARTESIAN_POINT ( 'NONE',  ( 0.5827357941260215002, -29.44458568814485488, -37.77622264066042135 ) ) ;
#12579 = ORIENTED_EDGE ( 'NONE', *, *, #25585, .T. ) ;
#12580 = CARTESIAN_POINT ( 'NONE',  ( 2.282803330402961794, 31.69834785191134330, 34.66571290073540723 ) ) ;
#12581 = VECTOR ( 'NONE', #40261, 1000.000000000000000 ) ;
#12582 = CARTESIAN_POINT ( 'NONE',  ( 5.896278296736517710, -4.667894692254015432, 19.56368418157506994 ) ) ;
#12583 = DIRECTION ( 'NONE',  ( 0.9848077530122079093, 0.1736481776669315524, -5.551115123125781470E-17 ) ) ;
#12584 = VERTEX_POINT ( 'NONE', #14499 ) ;
#12585 = CARTESIAN_POINT ( 'NONE',  ( 3.782625744892854414, -40.24479482953532283, -12.14885151870784874 ) ) ;
#12586 = CIRCLE ( 'NONE', #5522, 43.92652462719577500 ) ;
#12587 = CARTESIAN_POINT ( 'NONE',  ( 0.1155031312995260795, 4.069181162214699832, 43.93612860961791711 ) ) ;
#12588 = B_SPLINE_CURVE_WITH_KNOTS ( 'NONE', 3,
 ( #46912, #38432, #27778, #13697 ),
 .UNSPECIFIED., .F., .F.,
 ( 4, 4 ),
 ( 4.336808689942017736E-19, 0.004446298630425048540 ),
 .UNSPECIFIED. ) ;
#12589 = CARTESIAN_POINT ( 'NONE',  ( 0.6064515330803578186, -14.57163282274000871, -44.57579895993265495 ) ) ;
#12590 = ORIENTED_EDGE ( 'NONE', *, *, #51270, .T. ) ;
#12591 = CARTESIAN_POINT ( 'NONE',  ( 4.553261556744873317, 40.63093864075514006, -16.69330377710856084 ) ) ;
#12592 = CARTESIAN_POINT ( 'NONE',  ( 0.1073791018717578927, 41.77800844988514939, -10.69234304550012027 ) ) ;
#12593 = CARTESIAN_POINT ( 'NONE',  ( 1.834102595619085507, -11.27825010024307595, 42.57932385012767895 ) ) ;
#12594 = ORIENTED_EDGE ( 'NONE', *, *, #28006, .F. ) ;
#12595 = CARTESIAN_POINT ( 'NONE',  ( 0.8554163680231708922, 5.604726001789484435, -46.58103175710778743 ) ) ;
#12596 = EDGE_LOOP ( 'NONE', ( #52795, #42106, #12741, #48092 ) ) ;
#12597 = VERTEX_POINT ( 'NONE', #46793 ) ;
#12598 = ADVANCED_FACE ( 'NONE', ( #52370 ), #17499, .F. ) ;
#12599 = VERTEX_POINT ( 'NONE', #32369 ) ;
#12600 = CARTESIAN_POINT ( 'NONE',  ( 0.8551540677456715978, 5.348818140990894143, 47.61725548905992866 ) ) ;
#12601 = B_SPLINE_CURVE_WITH_KNOTS ( 'NONE', 3,
 ( #41499, #55875, #23301, #12998, #32091, #7960 ),
 .UNSPECIFIED., .F., .F.,
 ( 4, 2, 4 ),
 ( 8.148123767742043513E-18, 0.0002291978881530167022, 0.0004583957763060252186 ),
 .UNSPECIFIED. ) ;
#12602 = ORIENTED_EDGE ( 'NONE', *, *, #48182, .T. ) ;
#12603 = EDGE_CURVE ( 'NONE', #18917, #29558, #47092, .T. ) ;
#12604 = CARTESIAN_POINT ( 'NONE',  ( 2.881901169982995725, 1.330622528702777754E-16, 49.00591519830862808 ) ) ;
#12605 = CARTESIAN_POINT ( 'NONE',  ( 0.8753041380234530822, 37.96023374381034188, 31.14737520222631417 ) ) ;
#12606 = EDGE_CURVE ( 'NONE', #58891, #21001, #9162, .T. ) ;
#12607 = EDGE_LOOP ( 'NONE', ( #58524, #4288, #44446, #61322 ) ) ;
#12608 = EDGE_CURVE ( 'NONE', #61948, #59796, #34720, .T. ) ;
#12609 = B_SPLINE_CURVE_WITH_KNOTS ( 'NONE', 3,
 ( #48217, #6492, #15637, #29403, #44771, #20035, #48514, #54114, #49134, #1813, #20942, #59133, #16244, #54424, #29099, #578 ),
 .UNSPECIFIED., .F., .F.,
 ( 4, 3, 3, 3, 3, 4 ),
 ( 1.868480190406682863E-17, 0.0002612764279487741928, 0.0003919131003184782693, 0.0005225497727000676411, 0.0007837925190632453543, 0.001045051706266716951 ),
 .UNSPECIFIED. ) ;
#12610 = CARTESIAN_POINT ( 'NONE',  ( 5.917102823773431552, 20.06759006498877795, 1.334746056486321164 ) ) ;
#12611 = CARTESIAN_POINT ( 'NONE',  ( 3.894904216938897878, -37.15895100125024442, 23.48055989457843395 ) ) ;
#12612 = CARTESIAN_POINT ( 'NONE',  ( 0.5837800304671211249, -30.31211522357351384, 35.78285906481343659 ) ) ;
#12614 = EDGE_CURVE ( 'NONE', #56393, #45060, #13577, .T. ) ;
#12613 = ORIENTED_EDGE ( 'NONE', *, *, #24008, .T. ) ;
#12615 = CARTESIAN_POINT ( 'NONE',  ( 0.5797568665920711517, 43.41643168312820222, 17.72678110955651931 ) ) ;
#12616 = VERTEX_POINT ( 'NONE', #23272 ) ;
#12617 = CARTESIAN_POINT ( 'NONE',  ( 0.9754642270333672149, -42.90808635884414457, -0.1757168848623658075 ) ) ;
#12618 = ORIENTED_EDGE ( 'NONE', *, *, #43178, .F. ) ;
#12619 = CARTESIAN_POINT ( 'NONE',  ( 4.967162193818130511, 3.259922920617742914, 42.96271701169386859 ) ) ;
#12620 = ADVANCED_FACE ( 'NONE', ( #32678 ), #50695, .T. ) ;
#12621 = CARTESIAN_POINT ( 'NONE',  ( 2.281351352603241622, -17.13758816714718591, -44.80774876812576935 ) ) ;
#12622 = ORIENTED_EDGE ( 'NONE', *, *, #4226, .F. ) ;
#12623 = CARTESIAN_POINT ( 'NONE',  ( 4.553261556744875094, 0.000000000000000000, 0.000000000000000000 ) ) ;
#12624 = CARTESIAN_POINT ( 'NONE',  ( 4.967162193818130511, 7.970725651240403664, -42.34252806656584056 ) ) ;
#12625 = CARTESIAN_POINT ( 'NONE',  ( 0.6016118706126976079, 27.80884168916806942, 40.47492283736583829 ) ) ;
#12626 = CARTESIAN_POINT ( 'NONE',  ( 0.6023143664670691511, -41.53077189784247736, -24.28012784216863551 ) ) ;
#12628 = ORIENTED_EDGE ( 'NONE', *, *, #1987, .F. ) ;
#12627 = CIRCLE ( 'NONE', #32600, 10.00000000000000355 ) ;
#12629 = EDGE_LOOP ( 'NONE', ( #45549, #49163, #10666, #27346 ) ) ;
#12630 = DIRECTION ( 'NONE',  ( -1.000000000000000000, -0.000000000000000000, -0.000000000000000000 ) ) ;
#12631 = CARTESIAN_POINT ( 'NONE',  ( 0.9780106845699476636, -41.83479645273218495, 2.486172201176787500 ) ) ;
#12632 = CARTESIAN_POINT ( 'NONE',  ( -5.571549742892843327, -9.254395351074540699, -1.199999999999999956 ) ) ;
#12633 = AXIS2_PLACEMENT_3D ( 'NONE', #60676, #7754, #32203 ) ;
#12634 = CARTESIAN_POINT ( 'NONE',  ( 0.6009452777970409887, 5.846392105360529001, -47.75105029762386266 ) ) ;
#12635 = B_SPLINE_CURVE_WITH_KNOTS ( 'NONE', 3,
 ( #48739, #24632, #57492, #10531 ),
 .UNSPECIFIED., .F., .F.,
 ( 4, 4 ),
 ( 0.000000000000000000, 0.004446090762761387670 ),
 .UNSPECIFIED. ) ;
#12636 = CARTESIAN_POINT ( 'NONE',  ( 4.226256110419178924, 12.10579822316747922, 42.24070192796447287 ) ) ;
#12637 = CARTESIAN_POINT ( 'NONE',  ( 4.956653778116488773, 2.599733001513538255, 48.02038484091099235 ) ) ;
#12639 = CIRCLE ( 'NONE', #29597, 6.728125000000022560 ) ;
#12638 = B_SPLINE_CURVE_WITH_KNOTS ( 'NONE', 3,
 ( #10399, #10087, #39233, #30104 ),
 .UNSPECIFIED., .F., .F.,
 ( 4, 4 ),
 ( 0.000000000000000000, 0.005014147105413701254 ),
 .UNSPECIFIED. ) ;
#12640 = CARTESIAN_POINT ( 'NONE',  ( 2.643462169533600914, -4.896978544601818584, -47.78621045426874048 ) ) ;
#12641 = DIRECTION ( 'NONE',  ( 0.09722883295013597105, -0.1513788123411373143, -0.9836823721188365788 ) ) ;
#12642 = CARTESIAN_POINT ( 'NONE',  ( 0.9762797500689124330, 33.20096159360316790, 25.57383300261796677 ) ) ;
#12643 = CARTESIAN_POINT ( 'NONE',  ( 1.092182651088183354, 35.65846785729959123, -22.02804699723095183 ) ) ;
#12644 = DIRECTION ( 'NONE',  ( -1.000000000000000000, -0.000000000000000000, -0.000000000000000000 ) ) ;
#12645 = CARTESIAN_POINT ( 'NONE',  ( 0.8751705887134553219, -19.22545746485630502, -44.08562551107074512 ) ) ;
#12646 = CARTESIAN_POINT ( 'NONE',  ( 5.958863334805807099, -2.680345151634763834, 20.34989385289152963 ) ) ;
#12647 = EDGE_CURVE ( 'NONE', #42943, #10214, #57576, .T. ) ;
#12648 = CARTESIAN_POINT ( 'NONE',  ( 4.999999999999986677, 58.44237546506882808, -54.69470952477875869 ) ) ;
#12649 = CARTESIAN_POINT ( 'NONE',  ( 0.6027444965799114707, 16.83735020315194220, 46.13070727859980025 ) ) ;
#12650 = CARTESIAN_POINT ( 'NONE',  ( 4.833616638992208614, -25.31740731790925025, 38.70560126501819553 ) ) ;
#12652 = VERTEX_POINT ( 'NONE', #38017 ) ;
#12651 = CARTESIAN_POINT ( 'NONE',  ( 5.960721111146673579, -16.28018152803684515, -12.50019045452732591 ) ) ;
#12653 = ORIENTED_EDGE ( 'NONE', *, *, #54361, .T. ) ;
#12654 = FACE_BOUND ( 'NONE', #9123, .T. ) ;
#12655 = CARTESIAN_POINT ( 'NONE',  ( 0.5782707292762442330, -8.514009628394607176, 46.12209875705161721 ) ) ;
#12656 = CARTESIAN_POINT ( 'NONE',  ( -6.001507490154111224, -13.31361390284150659, -13.33564355450122285 ) ) ;
#12657 = VERTEX_POINT ( 'NONE', #47695 ) ;
#12658 = PRODUCT_DEFINITION ( 'UNKNOWN', '', #58888, #56162 ) ;
#12659 = EDGE_LOOP ( 'NONE', ( #24209, #61259, #48562, #29278 ) ) ;
#12660 = CARTESIAN_POINT ( 'NONE',  ( 1.399999999999999023, 0.000000000000000000, -7.400000000000022560 ) ) ;
#12661 = CARTESIAN_POINT ( 'NONE',  ( 0.2279481005628784251, 43.15403823156285057, 9.177824980992246751 ) ) ;
#12662 = EDGE_LOOP ( 'NONE', ( #58487, #60313, #44710, #37752 ) ) ;
#12663 = VERTEX_POINT ( 'NONE', #56154 ) ;
#12664 = DIRECTION ( 'NONE',  ( 0.07906939808003035641, -0.3658060745126776592, 0.9273262350094960693 ) ) ;
#12665 = AXIS2_PLACEMENT_3D ( 'NONE', #51720, #9738, #48272 ) ;
#12666 = CARTESIAN_POINT ( 'NONE',  ( -6.016761891674565099, 13.32657647165373760, -13.32172022638577680 ) ) ;
#12667 = VECTOR ( 'NONE', #8891, 1000.000000000000114 ) ;
#12668 = CARTESIAN_POINT ( 'NONE',  ( 0.7948884756798508811, 48.93475817450405430, 4.010995762022314004 ) ) ;
#12669 = CIRCLE ( 'NONE', #1623, 48.09070567114147110 ) ;
#12670 = ORIENTED_EDGE ( 'NONE', *, *, #32454, .T. ) ;
#12671 = CARTESIAN_POINT ( 'NONE',  ( 4.834790513006553603, 19.54670848745993439, -43.01761881172228641 ) ) ;
#12672 = B_SPLINE_CURVE_WITH_KNOTS ( 'NONE', 3,
 ( #46535, #42166, #52439, #8288 ),
 .UNSPECIFIED., .F., .F.,
 ( 4, 4 ),
 ( 0.000000000000000000, 0.004447772540403789436 ),
 .UNSPECIFIED. ) ;
#12673 = CARTESIAN_POINT ( 'NONE',  ( 0.8560838555295223751, -41.44626783305086093, 21.96769712083507287 ) ) ;
#12674 = EDGE_CURVE ( 'NONE', #36543, #46057, #17720, .T. ) ;
#12675 = CARTESIAN_POINT ( 'NONE',  ( 0.1103936448916685020, 0.01291577404961429323, -43.12443171339901227 ) ) ;
#12676 = EDGE_CURVE ( 'NONE', #34042, #14204, #8536, .T. ) ;
#12677 = ORIENTED_EDGE ( 'NONE', *, *, #24352, .F. ) ;
#12678 = AXIS2_PLACEMENT_3D ( 'NONE', #5124, #6038, #5731 ) ;
#12679 = ORIENTED_EDGE ( 'NONE', *, *, #38134, .F. ) ;
#12680 = EDGE_CURVE ( 'NONE', #10980, #57884, #28572, .T. ) ;
#12681 = DIRECTION ( 'NONE',  ( 1.850371707708593823E-16, -1.000000000000000000, 0.000000000000000000 ) ) ;
#12682 = ORIENTED_EDGE ( 'NONE', *, *, #54946, .F. ) ;
#12683 = CARTESIAN_POINT ( 'NONE',  ( 0.6021448801613057400, -48.73699182459426993, 6.020528757208808202 ) ) ;
#12684 = FACE_OUTER_BOUND ( 'NONE', #51273, .T. ) ;
#12685 = CARTESIAN_POINT ( 'NONE',  ( 3.238018933889920792, 6.676852487596914187, 11.61150865419837963 ) ) ;
#12686 = ADVANCED_FACE ( 'NONE', ( #28885 ), #23892, .F. ) ;
#12687 = CARTESIAN_POINT ( 'NONE',  ( -6.015611763856276717, 11.46610900684722623, 14.95313250337433963 ) ) ;
#12688 = CARTESIAN_POINT ( 'NONE',  ( 3.660087539127315992, 47.83637163185232311, 4.399983418616303155 ) ) ;
#12689 = VERTEX_POINT ( 'NONE', #48308 ) ;
#12690 = CARTESIAN_POINT ( 'NONE',  ( 4.967162193818130511, 0.000000000000000000, 0.000000000000000000 ) ) ;
#12691 = CARTESIAN_POINT ( 'NONE',  ( 0.7246131072078536572, 24.75818606403450417, -41.24126838495074310 ) ) ;
#12692 = ORIENTED_EDGE ( 'NONE', *, *, #55036, .T. ) ;
#12693 = CARTESIAN_POINT ( 'NONE',  ( 0.6846871229502899947, -19.12907057981172088, -43.92355552798057516 ) ) ;
#12694 = DIRECTION ( 'NONE',  ( 0.000000000000000000, 0.000000000000000000, -1.000000000000000000 ) ) ;
#12695 = CARTESIAN_POINT ( 'NONE',  ( 0.9752570700956790795, 30.17732761204941738, 30.50353876750642357 ) ) ;
#12696 = SURFACE_STYLE_USAGE ( .BOTH. , #55261 ) ;
#12697 = EDGE_CURVE ( 'NONE', #57388, #25265, #41213, .T. ) ;
#12698 = ORIENTED_EDGE ( 'NONE', *, *, #52702, .F. ) ;
#12699 = CARTESIAN_POINT ( 'NONE',  ( 0.8753041380234471980, -39.87785955339043653, 28.65125905284175190 ) ) ;
#12700 = LINE ( 'NONE', #35582, #41693 ) ;
#12701 = ADVANCED_FACE ( 'NONE', ( #20122 ), #40388, .F. ) ;
#12702 = CARTESIAN_POINT ( 'NONE',  ( 0.9754292589017241610, 40.56950062075481611, 10.50919056244812566 ) ) ;
#12703 = B_SPLINE_CURVE_WITH_KNOTS ( 'NONE', 3,
 ( #39649, #5767, #24920, #30510, #1085, #49630 ),
 .UNSPECIFIED., .F., .F.,
 ( 4, 2, 4 ),
 ( 8.542522420166516410E-18, 0.0002291472222819935318, 0.0004582944445639785527 ),
 .UNSPECIFIED. ) ;
#12704 = CARTESIAN_POINT ( 'NONE',  ( 0.5848930533535030563, 32.73270734968657791, 33.58337314724851552 ) ) ;
#12705 = FACE_OUTER_BOUND ( 'NONE', #31364, .T. ) ;
#12706 = CARTESIAN_POINT ( 'NONE',  ( 0.6846871229502899947, 11.56285438919697306, -46.49193983736579128 ) ) ;
#12707 = DIRECTION ( 'NONE',  ( 0.000000000000000000, 0.000000000000000000, 1.000000000000000000 ) ) ;
#12708 = CARTESIAN_POINT ( 'NONE',  ( 0.9968887458511662691, -22.02152923727777178, 36.82760690604620635 ) ) ;
#12709 = VECTOR ( 'NONE', #19865, 1000.000000000000114 ) ;
#12710 = CARTESIAN_POINT ( 'NONE',  ( 5.901463166500145796, -18.52233187494223188, 7.838436850235891207 ) ) ;
#12711 = CARTESIAN_POINT ( 'NONE',  ( 0.5806925824938499181, 11.40214825760356376, -45.48860711711441240 ) ) ;
#12712 = ORIENTED_EDGE ( 'NONE', *, *, #6733, .T. ) ;
#12713 = VECTOR ( 'NONE', #7971, 1000.000000000000114 ) ;
#12714 = AXIS2_PLACEMENT_3D ( 'NONE', #60020, #16199, #40037 ) ;
#12715 = CARTESIAN_POINT ( 'NONE',  ( 0.6041374136657475802, -6.452348380036255548, 47.67304777898688428 ) ) ;
#12716 = CARTESIAN_POINT ( 'NONE',  ( 3.407937589446174087, 10.00592723328973932, -9.356405769958946905 ) ) ;
#12717 = CARTESIAN_POINT ( 'NONE',  ( 0.5809828226811553087, -12.92184523170170607, -46.11980934799353093 ) ) ;
#12718 = CARTESIAN_POINT ( 'NONE',  ( 3.407937589446178528, 11.62731850632894215, -7.243367523630903193 ) ) ;
#12719 = B_SPLINE_CURVE_WITH_KNOTS ( 'NONE', 3,
 ( #53146, #10561, #48764, #10254, #35001, #24658 ),
 .UNSPECIFIED., .F., .F.,
 ( 4, 2, 4 ),
 ( 9.875171458978167205E-18, 0.0002291978881530160788, 0.0004583957763060222913 ),
 .UNSPECIFIED. ) ;
#12720 = CARTESIAN_POINT ( 'NONE',  ( 4.322998006666179727, 2.120302895115615538, 47.94177812210865142 ) ) ;
#12721 = CARTESIAN_POINT ( 'NONE',  ( 0.5809828226811553087, -41.20389530892325070, 24.41822904836909203 ) ) ;
#12722 = PRODUCT_CONTEXT ( 'NONE', #9535, 'mechanical' ) ;
#12723 = CARTESIAN_POINT ( 'NONE',  ( 0.5998501479064699549, -44.24259072156099393, 18.89267974119588445 ) ) ;
#12724 = EDGE_CURVE ( 'NONE', #11600, #10306, #43953, .T. ) ;
#12725 = CARTESIAN_POINT ( 'NONE',  ( 0.9775691876210976794, -7.342838859687320863, 41.26034932560141044 ) ) ;
#12726 = CONICAL_SURFACE ( 'NONE', #20715, 43.92652462719577500, 1.486293639869522343 ) ;
#12727 = CARTESIAN_POINT ( 'NONE',  ( 0.3622758884714600280, 6.444611261694588755, -42.62881903538203687 ) ) ;
#12729 = ORIENTED_EDGE ( 'NONE', *, *, #24867, .T. ) ;
#12728 = CARTESIAN_POINT ( 'NONE',  ( 4.956653778116990594, -39.67974989265022145, -27.17045123668512474 ) ) ;
#12730 = VERTEX_POINT ( 'NONE', #987 ) ;
#12731 = B_SPLINE_CURVE_WITH_KNOTS ( 'NONE', 3,
 ( #52422, #52118, #47436, #48056, #38366, #24235 ),
 .UNSPECIFIED., .F., .F.,
 ( 4, 2, 4 ),
 ( 7.007167689862070887E-18, 0.0002448709889506557472, 0.0004897419779013045555 ),
 .UNSPECIFIED. ) ;
#12732 = CARTESIAN_POINT ( 'NONE',  ( 3.894904216938897878, -19.80394396472108554, -39.24191809683094334 ) ) ;
#12733 = CARTESIAN_POINT ( 'NONE',  ( 2.643462169533600914, -17.09809940585630272, -44.89050350746145313 ) ) ;
#12734 = DIRECTION ( 'NONE',  ( 0.07906939808003035641, 0.8264033190538777607, -0.5574994031781526083 ) ) ;
#12735 = ORIENTED_EDGE ( 'NONE', *, *, #2970, .T. ) ;
#12736 = CARTESIAN_POINT ( 'NONE',  ( 3.240649175237396484, 43.98046403787316905, -0.9918167224828714490 ) ) ;
#12737 = CARTESIAN_POINT ( 'NONE',  ( 4.956653778116966613, 0.000000000000000000, 0.000000000000000000 ) ) ;
#12738 = FACE_OUTER_BOUND ( 'NONE', #55249, .T. ) ;
#12739 = AXIS2_PLACEMENT_3D ( 'NONE', #56297, #61905, #8684 ) ;
#12740 =( BOUNDED_SURFACE ( )  B_SPLINE_SURFACE ( 3, 1, ( 
 ( #50357, #7744 ),
 ( #26556, #2734 ),
 ( #26866, #3047 ),
 ( #22172, #22783 ) ),
 .UNSPECIFIED., .F., .F., .F. ) 
 B_SPLINE_SURFACE_WITH_KNOTS ( ( 4, 4 ),
 ( 2, 2 ),
 ( 0.000000000000000000, 1.000000000000000000 ),
 ( 0.000000000000000000, 1.000000000000000000 ),
 .UNSPECIFIED. ) 
 GEOMETRIC_REPRESENTATION_ITEM ( )  RATIONAL_B_SPLINE_SURFACE ( (
 ( 1.000000000000000000, 1.000000000000000000),
 ( 0.7282232189291693025, 0.9929344683865674037),
 ( 0.7282232189291693025, 0.9929344683865674037),
 ( 1.000000000000000000, 1.000000000000000000) ) ) 
 REPRESENTATION_ITEM ( '' )  SURFACE ( )  );
#12741 = ORIENTED_EDGE ( 'NONE', *, *, #21077, .T. ) ;
#12742 = ORIENTED_EDGE ( 'NONE', *, *, #25464, .F. ) ;
#12743 = CARTESIAN_POINT ( 'NONE',  ( 0.9784957157296357844, 24.67156637886485626, -33.87693713141196383 ) ) ;
#12744 = CARTESIAN_POINT ( 'NONE',  ( 7.000000000000006217, -2.780326704359372228E-13, 80.00000000000001421 ) ) ;
#12745 = CARTESIAN_POINT ( 'NONE',  ( 0.9790320750461900534, 32.94311240808050201, -25.90537545396250607 ) ) ;
#12746 = ORIENTED_EDGE ( 'NONE', *, *, #25395, .T. ) ;
#12747 = CARTESIAN_POINT ( 'NONE',  ( 0.6252788684277231779, 43.94110077395946945, -21.92313832338802371 ) ) ;
#12748 = CARTESIAN_POINT ( 'NONE',  ( 0.6016117650947689910, 49.02773486208430143, 2.798619041181271694 ) ) ;
#12749 =( BOUNDED_SURFACE ( )  B_SPLINE_SURFACE ( 3, 1, ( 
 ( #7142, #26271 ),
 ( #45715, #40718 ),
 ( #55384, #40404 ),
 ( #35080, #2455 ) ),
 .UNSPECIFIED., .F., .F., .F. ) 
 B_SPLINE_SURFACE_WITH_KNOTS ( ( 4, 4 ),
 ( 2, 2 ),
 ( 0.000000000000000000, 1.000000000000000000 ),
 ( 0.000000000000000000, 1.000000000000000000 ),
 .UNSPECIFIED. ) 
 GEOMETRIC_REPRESENTATION_ITEM ( )  RATIONAL_B_SPLINE_SURFACE ( (
 ( 1.000000000000000000, 1.000000000000000000),
 ( 0.7211978278499968642, 0.9934217856018975334),
 ( 0.7211978278499968642, 0.9934217856018975334),
 ( 1.000000000000000000, 1.000000000000000000) ) ) 
 REPRESENTATION_ITEM ( '' )  SURFACE ( )  );
#12750 = CARTESIAN_POINT ( 'NONE',  ( -6.078457390727109555, -11.01309887717671288, -15.79576412077101644 ) ) ;
#12751 = CARTESIAN_POINT ( 'NONE',  ( 0.6001305935487315502, 17.92615948558540850, -44.64600790884038162 ) ) ;
#12752 = EDGE_CURVE ( 'NONE', #5070, #10104, #59148, .T. ) ;
#12753 = VECTOR ( 'NONE', #44513, 1000.000000000000114 ) ;
#12754 = VERTEX_POINT ( 'NONE', #19818 ) ;
#12755 = B_SPLINE_CURVE_WITH_KNOTS ( 'NONE', 3,
 ( #41014, #41309, #45694, #16556 ),
 .UNSPECIFIED., .F., .F.,
 ( 4, 4 ),
 ( 0.000000000000000000, 0.004447772540403837141 ),
 .UNSPECIFIED. ) ;
#12756 = FACE_OUTER_BOUND ( 'NONE', #19671, .T. ) ;
#12757 = FACE_OUTER_BOUND ( 'NONE', #1772, .T. ) ;
#12758 = AXIS2_PLACEMENT_3D ( 'NONE', #18311, #48342, #52103 ) ;
#12759 = EDGE_LOOP ( 'NONE', ( #53486, #7234, #10432 ) ) ;
#12760 = VECTOR ( 'NONE', #36340, 1000.000000000000000 ) ;
#12761 = CARTESIAN_POINT ( 'NONE',  ( 4.553261556744873317, -43.15908619232978083, -8.175135770535248980 ) ) ;
#12762 = EDGE_CURVE ( 'NONE', #37909, #3915, #52375, .T. ) ;
#12763 = CARTESIAN_POINT ( 'NONE',  ( 0.9789889208857696090, 4.099175781249488004, -41.70769300688767345 ) ) ;
#12764 = CARTESIAN_POINT ( 'NONE',  ( -6.057079549204054558, 16.78313491342506936, 9.442330939842715765 ) ) ;
#12765 = VERTEX_POINT ( 'NONE', #52993 ) ;
#12766 = EDGE_LOOP ( 'NONE', ( #45213, #10326, #60421, #22581 ) ) ;
#12767 = CARTESIAN_POINT ( 'NONE',  ( 5.896278296736517710, -15.78795198421094170, 12.46064010228340280 ) ) ;
#12768 = CARTESIAN_POINT ( 'NONE',  ( -6.077587904424778920, -14.65844225831517633, 12.48703695652296553 ) ) ;
#12769 = VERTEX_POINT ( 'NONE', #58291 ) ;
#12770 = CARTESIAN_POINT ( 'NONE',  ( 0.1064266379913941518, 42.82540706760016747, 5.071708164747208869 ) ) ;
#12771 = ORIENTED_EDGE ( 'NONE', *, *, #46076, .F. ) ;
#12772 = CARTESIAN_POINT ( 'NONE',  ( 0.6041374136657476912, -18.57118264377508865, -44.37863742124660149 ) ) ;
#12773 = ORIENTED_EDGE ( 'NONE', *, *, #57139, .F. ) ;
#12774 = DIRECTION ( 'NONE',  ( 1.000000000000000000, 1.836909530733573776E-16, 0.000000000000000000 ) ) ;
#12775 = CARTESIAN_POINT ( 'NONE',  ( 0.6029443449137436017, -48.69867271451428792, -6.322880184532521319 ) ) ;
#12776 = EDGE_CURVE ( 'NONE', #9477, #24263, #49389, .T. ) ;
#12777 = CARTESIAN_POINT ( 'NONE',  ( 2.281351352603289584, -7.562287671717538906, 47.37344280316143852 ) ) ;
#12778 = ORIENTED_EDGE ( 'NONE', *, *, #37191, .F. ) ;
#12779 = CARTESIAN_POINT ( 'NONE',  ( 0.1154773475650540393, -27.65137296628978802, -34.38524688184250522 ) ) ;
#12780 = CARTESIAN_POINT ( 'NONE',  ( 2.624215991343608501, 47.98682984381861161, 1.411420423865641149 ) ) ;
#12781 = EDGE_CURVE ( 'NONE', #58714, #2462, #46757, .T. ) ;
#12782 = CARTESIAN_POINT ( 'NONE',  ( 0.5837800304671199036, -41.87608985909586323, 21.10996045217588701 ) ) ;
#12783 = B_SPLINE_CURVE_WITH_KNOTS ( 'NONE', 3,
 ( #54090, #11212, #30299, #49410 ),
 .UNSPECIFIED., .F., .F.,
 ( 4, 4 ),
 ( 1.992131139712224140E-17, 0.004444306975806115896 ),
 .UNSPECIFIED. ) ;
#12784 = CONICAL_SURFACE ( 'NONE', #20763, 43.92652462719577500, 1.486293639869522343 ) ;
#12785 = ORIENTED_EDGE ( 'NONE', *, *, #685, .F. ) ;
#12786 = DIRECTION ( 'NONE',  ( -0.07906939808003035641, 0.1078133555909867869, 0.9910218517487257017 ) ) ;
#12787 = CARTESIAN_POINT ( 'NONE',  ( 1.092182651088184242, -26.45970545413510777, 32.50607899643846110 ) ) ;
#12788 = CARTESIAN_POINT ( 'NONE',  ( 5.917102823773431552, -19.93362549613927115, 2.672132599892532046 ) ) ;
#12789 = CARTESIAN_POINT ( 'NONE',  ( 0.7246131072078533242, -11.65529928397605808, -46.66866179549012372 ) ) ;
#12790 = ORIENTED_EDGE ( 'NONE', *, *, #36628, .T. ) ;
#12791 = AXIS2_PLACEMENT_3D ( 'NONE', #2054, #16488, #21186 ) ;
#12792 = CARTESIAN_POINT ( 'NONE',  ( 0.1102847568649952675, 37.30068345220691839, -21.64199720113203895 ) ) ;
#12793 = CARTESIAN_POINT ( 'NONE',  ( 4.962356264823608143, 0.000000000000000000, 0.000000000000000000 ) ) ;
#12794 = EDGE_LOOP ( 'NONE', ( #30607, #10664, #1521, #5469 ) ) ;
#12795 = CARTESIAN_POINT ( 'NONE',  ( 0.5807400328401637335, 18.83234461715243313, -44.04145271122544614 ) ) ;
#12796 = CARTESIAN_POINT ( 'NONE',  ( 0.9787284016396617936, -26.91414329176047815, 32.12421033736727338 ) ) ;
#12797 = FACE_OUTER_BOUND ( 'NONE', #61203, .T. ) ;
#12798 = CARTESIAN_POINT ( 'NONE',  ( 0.2940135542859017570, 19.68859029487963141, -39.47910790395081193 ) ) ;
#12799 = CARTESIAN_POINT ( 'NONE',  ( 0.8760168074886965917, -47.80016357497253665, 5.394043284318689402 ) ) ;
#12800 = CARTESIAN_POINT ( 'NONE',  ( 4.975801465491695552, 0.000000000000000000, 0.000000000000000000 ) ) ;
#12801 = CARTESIAN_POINT ( 'NONE',  ( 0.6026112563231247332, 4.542062193711753793, 48.89693922867424902 ) ) ;
#12802 = CARTESIAN_POINT ( 'NONE',  ( 0.5834584762367747146, 10.69421303378797994, 45.66037446847265358 ) ) ;
#12803 = ADVANCED_FACE ( 'NONE', ( #30115 ), #55158, .F. ) ;
#12804 = CARTESIAN_POINT ( 'NONE',  ( 0.9752132459055852243, -39.55248938404429992, 16.63533515462565404 ) ) ;
#12805 = CARTESIAN_POINT ( 'NONE',  ( 0.9754292580325140127, 19.62773382990652138, 37.02809111480564042 ) ) ;
#12806 = DIRECTION ( 'NONE',  ( -1.000000000000000000, -1.836909530733573776E-16, 1.103352205049209901E-32 ) ) ;
#12807 = FACE_OUTER_BOUND ( 'NONE', #61834, .T. ) ;
#12808 = VECTOR ( 'NONE', #39528, 1000.000000000000227 ) ;
#12809 = CIRCLE ( 'NONE', #28647, 47.91270532121795611 ) ;
#12810 = CARTESIAN_POINT ( 'NONE',  ( 0.6254087463353906751, -46.64065386173405869, -11.78492518233793795 ) ) ;
#12811 = CARTESIAN_POINT ( 'NONE',  ( 0.6026112563231247332, -1.399892387035774233, -49.08748614676582633 ) ) ;
#12812 = CARTESIAN_POINT ( 'NONE',  ( 2.359973842542475442, 16.61171373028292919, 40.76992594518206658 ) ) ;
#12813 = CARTESIAN_POINT ( 'NONE',  ( -2.739355103387248747, -11.80442426703895897, 9.138004961410270965 ) ) ;
#12814 = CARTESIAN_POINT ( 'NONE',  ( 4.956445790444005794, -27.49627641100061837, -38.22947597953034204 ) ) ;
#12815 = B_SPLINE_CURVE_WITH_KNOTS ( 'NONE', 3,
 ( #21894, #34762, #21578, #15966, #40108, #35386, #40715, #53829, #54762, #49152, #54445, #59787, #54136, #16897, #36012, #55077 ),
 .UNSPECIFIED., .F., .F.,
 ( 4, 3, 3, 3, 3, 4 ),
 ( 1.868385820337156008E-17, 0.0002732102107931905959, 0.0004098135523333825640, 0.0005464168938825052137, 0.0008195847345945452868, 0.001092771384553100928 ),
 .UNSPECIFIED. ) ;
#12816 = ORIENTED_EDGE ( 'NONE', *, *, #21515, .T. ) ;
#12817 = CARTESIAN_POINT ( 'NONE',  ( 5.896782393890504181, -2.019528367549592307, 20.01118667272569951 ) ) ;
#12818 = CARTESIAN_POINT ( 'NONE',  ( -6.057079549204054558, 5.470993133660704721, -18.46346298046971768 ) ) ;
#12820 = AXIS2_PLACEMENT_3D ( 'NONE', #46925, #55353, #8064 ) ;
#12819 = CARTESIAN_POINT ( 'NONE',  ( 5.838029081930957709, 25.43272996496265748, 39.80252887295241493 ) ) ;
#12821 = CARTESIAN_POINT ( 'NONE',  ( 0.3676999524040323597, -18.60775935196367925, 39.99627326667132365 ) ) ;
#12822 = EDGE_LOOP ( 'NONE', ( #40863, #20372, #46472, #50472 ) ) ;
#12823 = CARTESIAN_POINT ( 'NONE',  ( 0.5807400328401637335, -34.25275203086259523, 33.48217046439098965 ) ) ;
#12824 = CARTESIAN_POINT ( 'NONE',  ( 0.6030672727741701600, 24.12926094633986196, -41.61859040196959114 ) ) ;
#12825 = ORIENTED_EDGE ( 'NONE', *, *, #11424, .T. ) ;
#12826 = B_SPLINE_CURVE_WITH_KNOTS ( 'NONE', 3,
 ( #43162, #19969, #58138, #34367 ),
 .UNSPECIFIED., .F., .F.,
 ( 4, 4 ),
 ( 0.000000000000000000, 0.004048833967417087357 ),
 .UNSPECIFIED. ) ;
#12827 = CARTESIAN_POINT ( 'NONE',  ( 0.6000166863083090663, 17.45040302316585112, 45.90541270958728148 ) ) ;
#12828 = EDGE_CURVE ( 'NONE', #25918, #2384, #58689, .T. ) ;
#12829 = AXIS2_PLACEMENT_3D ( 'NONE', #3129, #46381, #23178 ) ;
#12830 = EDGE_LOOP ( 'NONE', ( #47025, #9048, #56256, #21291 ) ) ;
#12831 = CARTESIAN_POINT ( 'NONE',  ( -5.995132425357893702, -18.84415457712583475, -0.008513469643004962714 ) ) ;
#12832 = FACE_OUTER_BOUND ( 'NONE', #39808, .T. ) ;
#12833 = ORIENTED_EDGE ( 'NONE', *, *, #31635, .T. ) ;
#12834 = CARTESIAN_POINT ( 'NONE',  ( 4.999999999999986677, 56.56854249492450037, -56.56854249492312192 ) ) ;
#12835 = CARTESIAN_POINT ( 'NONE',  ( 0.1095718737110178836, 26.04820588677147697, 34.36877422441008179 ) ) ;
#12837 = ORIENTED_EDGE ( 'NONE', *, *, #47536, .F. ) ;
#12836 = EDGE_CURVE ( 'NONE', #55315, #20695, #46103, .T. ) ;
#12838 = CARTESIAN_POINT ( 'NONE',  ( 4.549368137175248350, -40.58005590356700765, 13.99871866169291579 ) ) ;
#12839 = LINE ( 'NONE', #31929, #59324 ) ;
#12840 = ORIENTED_EDGE ( 'NONE', *, *, #43546, .F. ) ;
#12841 = CARTESIAN_POINT ( 'NONE',  ( 0.5998501479064708430, -29.69975237324642237, 37.84527566984805702 ) ) ;
#12842 = EDGE_CURVE ( 'NONE', #38501, #36669, #6909, .T. ) ;
#12843 = ORIENTED_EDGE ( 'NONE', *, *, #60431, .F. ) ;
#12844 = CARTESIAN_POINT ( 'NONE',  ( 0.5832366564991507962, -38.16363840618235770, -28.94058080282821166 ) ) ;
#12845 = ORIENTED_EDGE ( 'NONE', *, *, #46455, .F. ) ;
#12846 = VERTEX_POINT ( 'NONE', #54841 ) ;
#12847 = CARTESIAN_POINT ( 'NONE',  ( -6.063463321072276813, -4.269814012169966588, 18.77735712982385863 ) ) ;
#12848 = CARTESIAN_POINT ( 'NONE',  ( 0.5806925824938494740, 36.46274162637944016, -29.49052111156159128 ) ) ;
#12849 = CIRCLE ( 'NONE', #20827, 2.055000000000000160 ) ;
#12850 = CARTESIAN_POINT ( 'NONE',  ( 0.000000000000000000, 0.000000000000000000, -1.199999999999999956 ) ) ;
#12851 = AXIS2_PLACEMENT_3D ( 'NONE', #43854, #34742, #897 ) ;
#12852 = CARTESIAN_POINT ( 'NONE',  ( -2.601141883200662974, -13.21958573851844143, -6.930943685483855532 ) ) ;
#12853 = CARTESIAN_POINT ( 'NONE',  ( -6.016104459813371719, -16.32137543786076250, -9.416989654584476455 ) ) ;
#12854 = ORIENTED_EDGE ( 'NONE', *, *, #10764, .F. ) ;
#12855 = CARTESIAN_POINT ( 'NONE',  ( 1.092182651088184020, -39.33161120148861301, 14.48397544658308078 ) ) ;
#12856 = CARTESIAN_POINT ( 'NONE',  ( 5.917102823773431552, 17.94639498788064813, 9.078360258918703352 ) ) ;
#12857 = EDGE_CURVE ( 'NONE', #30264, #28594, #41999, .T. ) ;
#12858 = CARTESIAN_POINT ( 'NONE',  ( 0.8560838555295223751, -34.16988317699956923, 32.13708010619405542 ) ) ;
#12859 = ORIENTED_EDGE ( 'NONE', *, *, #4413, .T. ) ;
#12860 = ORIENTED_EDGE ( 'NONE', *, *, #61435, .T. ) ;
#12861 =( BOUNDED_SURFACE ( )  B_SPLINE_SURFACE ( 3, 1, ( 
 ( #57394, #4464 ),
 ( #23603, #28918 ),
 ( #35802, #11677 ),
 ( #44586, #30760 ) ),
 .UNSPECIFIED., .F., .F., .F. ) 
 B_SPLINE_SURFACE_WITH_KNOTS ( ( 4, 4 ),
 ( 2, 2 ),
 ( 0.000000000000000000, 1.000000000000000000 ),
 ( 0.000000000000000000, 1.000000000000000000 ),
 .UNSPECIFIED. ) 
 GEOMETRIC_REPRESENTATION_ITEM ( )  RATIONAL_B_SPLINE_SURFACE ( (
 ( 1.000000000000000000, 1.000000000000000000),
 ( 0.9732289882329797637, 0.9999525324661233672),
 ( 0.9732289882329797637, 0.9999525324661233672),
 ( 1.000000000000000000, 1.000000000000000000) ) ) 
 REPRESENTATION_ITEM ( '' )  SURFACE ( )  );
#12862 = CARTESIAN_POINT ( 'NONE',  ( 10.00000000000001599, -54.69470952477895764, -58.44237546506863623 ) ) ;
#12863 = CARTESIAN_POINT ( 'NONE',  ( 0.2885700199627513340, -42.63514063525633446, 6.424755504217515067 ) ) ;
#12864 = ORIENTED_EDGE ( 'NONE', *, *, #7979, .T. ) ;
#12865 = CARTESIAN_POINT ( 'NONE',  ( 4.694002226626920127, 18.13772657221557694, -41.82472529781492909 ) ) ;
#12866 = VECTOR ( 'NONE', #5042, 1000.000000000000114 ) ;
#12867 = ORIENTED_EDGE ( 'NONE', *, *, #49712, .T. ) ;
#12868 = CARTESIAN_POINT ( 'NONE',  ( 4.963659409799330291, 42.53037318520993182, 13.93274247732036031 ) ) ;
#12869 = CARTESIAN_POINT ( 'NONE',  ( -6.063463321072276813, 7.780528881867387447, -17.61487504349370425 ) ) ;
#12870 = CARTESIAN_POINT ( 'NONE',  ( 4.962356264823608143, 12.05238263218917716, 40.32338863178108568 ) ) ;
#12871 = CARTESIAN_POINT ( 'NONE',  ( 0.9789889208857700531, 9.621692253337958078, -40.78918896257224702 ) ) ;
#12872 = CARTESIAN_POINT ( 'NONE',  ( 0.9722240750034573109, 21.95618656574004746, 36.86535092060686480 ) ) ;
#12873 = ORIENTED_EDGE ( 'NONE', *, *, #42077, .T. ) ;
#12874 = DIRECTION ( 'NONE',  ( -0.9990097760809875105, 5.448601141172015318E-18, -0.04449120468828680897 ) ) ;
#12875 = AXIS2_PLACEMENT_3D ( 'NONE', #58827, #48831, #43858 ) ;
#12876 = CARTESIAN_POINT ( 'NONE',  ( 5.960221823109900008, -2.673723662181486826, 20.35070456576729825 ) ) ;
#12877 = CARTESIAN_POINT ( 'NONE',  ( 4.975801465491694664, -21.70134120755230711, 42.71626295676225027 ) ) ;
#12878 = CARTESIAN_POINT ( 'NONE',  ( 5.895596859100789899, 19.70914391261467102, 4.009716878325924050 ) ) ;
#12879 = EDGE_CURVE ( 'NONE', #22472, #57080, #27733, .T. ) ;
#12880 = CARTESIAN_POINT ( 'NONE',  ( 43.00000000000000000, 5.682605120120046040E-15, -2.995852231480065614E-16 ) ) ;
#12881 = CARTESIAN_POINT ( 'NONE',  ( 0.6029443199889047422, -49.10740923581496986, 2.443331554578143732E-05 ) ) ;
#12882 = CARTESIAN_POINT ( 'NONE',  ( 0.5817217712918323347, 22.93558036730663829, -40.90469541780249330 ) ) ;
#12883 = EDGE_CURVE ( 'NONE', #817, #42473, #36782, .T. ) ;
#12884 = EDGE_CURVE ( 'NONE', #38412, #27210, #16566, .T. ) ;
#12885 = CARTESIAN_POINT ( 'NONE',  ( 5.901463166500145796, -19.39418503693765317, -5.327612701169281983 ) ) ;
#12886 = DIRECTION ( 'NONE',  ( -0.000000000000000000, -0.000000000000000000, -1.000000000000000000 ) ) ;
#12887 = AXIS2_PLACEMENT_3D ( 'NONE', #36774, #13264, #55844 ) ;
#12888 = ORIENTED_EDGE ( 'NONE', *, *, #31410, .T. ) ;
#12889 = AXIS2_PLACEMENT_3D ( 'NONE', #49266, #43999, #19554 ) ;
#12890 = CARTESIAN_POINT ( 'NONE',  ( 0.5800708119828333897, 47.89175345941821149, -0.6275298934116645411 ) ) ;
#12891 = CARTESIAN_POINT ( 'NONE',  ( 0.9788927965476025284, 20.26469601834873657, 36.68349367107364145 ) ) ;
#12892 = CARTESIAN_POINT ( 'NONE',  ( -6.016104459813374383, -13.32794178585006861, 13.32039631884679842 ) ) ;
#12893 = CARTESIAN_POINT ( 'NONE',  ( 5.974727161628367256, -17.76736931401867281, 10.27590650342006384 ) ) ;
#12894 = ORIENTED_EDGE ( 'NONE', *, *, #56986, .F. ) ;
#12895 = CARTESIAN_POINT ( 'NONE',  ( 4.999999999999997335, 9.184547653667864935E-16, -9.629649721936170507E-32 ) ) ;
#12896 = CARTESIAN_POINT ( 'NONE',  ( 0.1135584504625008623, 3.806764484040820129, 43.95976110374461854 ) ) ;
#12897 = SURFACE_STYLE_USAGE ( .BOTH. , #46107 ) ;
#12898 = ORIENTED_EDGE ( 'NONE', *, *, #17816, .F. ) ;
#12899 = CARTESIAN_POINT ( 'NONE',  ( 0.6039202388192953519, -49.10736577297868166, 0.1741829149863364512 ) ) ;
#12900 = CARTESIAN_POINT ( 'NONE',  ( 5.910764540655178756, -18.51025558288811013, 7.865855117234400673 ) ) ;
#12901 = CARTESIAN_POINT ( 'NONE',  ( 0.3676999524040366896, -11.75791688508890331, 42.51707861373098041 ) ) ;
#12902 = EDGE_CURVE ( 'NONE', #46350, #46904, #39745, .T. ) ;
#12903 = ORIENTED_EDGE ( 'NONE', *, *, #58325, .T. ) ;
#12904 = CARTESIAN_POINT ( 'NONE',  ( 3.661921753702030102, 31.32117497468681933, -35.09437450702161954 ) ) ;
#12905 = AXIS2_PLACEMENT_3D ( 'NONE', #47524, #48145, #10233 ) ;
#12907 = ORIENTED_EDGE ( 'NONE', *, *, #32191, .T. ) ;
#12906 = EDGE_CURVE ( 'NONE', #6528, #16502, #2216, .T. ) ;
#12908 = EDGE_LOOP ( 'NONE', ( #39960, #12932, #18583, #41105 ) ) ;
#12909 = CARTESIAN_POINT ( 'NONE',  ( 0.1154773475650540671, 44.04468435281491878, 2.647529094650572734 ) ) ;
#12910 = ORIENTED_EDGE ( 'NONE', *, *, #53724, .T. ) ;
#12911 = CARTESIAN_POINT ( 'NONE',  ( 4.962356264823608143, 0.000000000000000000, 0.000000000000000000 ) ) ;
#12912 = EDGE_LOOP ( 'NONE', ( #47118, #692, #21016, #27741 ) ) ;
#12913 = DIRECTION ( 'NONE',  ( 0.1024043820194936311, 0.9239750460186099135, 0.3684880688409236105 ) ) ;
#12914 = EDGE_CURVE ( 'NONE', #1029, #35847, #703, .T. ) ;
#12915 =( GEOMETRIC_REPRESENTATION_CONTEXT ( 3 ) GLOBAL_UNCERTAINTY_ASSIGNED_CONTEXT ( ( #2296 ) ) GLOBAL_UNIT_ASSIGNED_CONTEXT ( ( #22184, #36604, #50977 ) ) REPRESENTATION_CONTEXT ( 'NONE', 'WORKASPACE' ) );
#12916 = CARTESIAN_POINT ( 'NONE',  ( 4.833616638992205949, 46.17873762321152498, -2.572717262757493906 ) ) ;
#12917 = ORIENTED_EDGE ( 'NONE', *, *, #25997, .T. ) ;
#12918 = CARTESIAN_POINT ( 'NONE',  ( 0.1152809850208375148, 43.35225507947838253, -8.217497308402093026 ) ) ;
#12919 = B_SPLINE_CURVE_WITH_KNOTS ( 'NONE', 3,
 ( #10703, #49835, #57974, #44549, #20716, #48906 ),
 .UNSPECIFIED., .F., .F.,
 ( 4, 2, 4 ),
 ( 8.594572927133164801E-17, 0.0002293366620881456082, 0.0004586733241762052391 ),
 .UNSPECIFIED. ) ;
#12920 = CARTESIAN_POINT ( 'NONE',  ( 5.896782393890504181, 20.06834277495332941, 1.337050913387667350 ) ) ;
#12921 = CARTESIAN_POINT ( 'NONE',  ( 0.3676999524040366896, -38.02468164711607557, 22.36233818182511257 ) ) ;
#12922 = DIRECTION ( 'NONE',  ( 0.09835009131224552170, 0.9223318362920736035, 0.3736726418952349693 ) ) ;
#12923 = VERTEX_POINT ( 'NONE', #60160 ) ;
#12924 = CARTESIAN_POINT ( 'NONE',  ( 1.084202172485504434E-14, 4.618802153517020059, -0.3572655899081733644 ) ) ;
#12925 = EDGE_CURVE ( 'NONE', #7194, #35355, #12034, .T. ) ;
#12926 = ORIENTED_EDGE ( 'NONE', *, *, #10573, .T. ) ;
#12927 = CARTESIAN_POINT ( 'NONE',  ( 4.962356264823608143, 0.000000000000000000, 0.000000000000000000 ) ) ;
#12928 =( BOUNDED_SURFACE ( )  B_SPLINE_SURFACE ( 3, 1, ( 
 ( #34075, #34677 ),
 ( #19658, #517 ),
 ( #4046, #53741 ),
 ( #58142, #43475 ) ),
 .UNSPECIFIED., .F., .F., .F. ) 
 B_SPLINE_SURFACE_WITH_KNOTS ( ( 4, 4 ),
 ( 2, 2 ),
 ( 0.000000000000000000, 1.000000000000000000 ),
 ( 0.000000000000000000, 1.000000000000000000 ),
 .UNSPECIFIED. ) 
 GEOMETRIC_REPRESENTATION_ITEM ( )  RATIONAL_B_SPLINE_SURFACE ( (
 ( 1.000000000000000000, 1.000000000000000000),
 ( 0.9953485035131437453, 0.8621029689291523912),
 ( 0.9953485035131437453, 0.8621029689291523912),
 ( 1.000000000000000000, 1.000000000000000000) ) ) 
 REPRESENTATION_ITEM ( '' )  SURFACE ( )  );
#12929 = EDGE_LOOP ( 'NONE', ( #34777, #1456, #44769, #9187 ) ) ;
#12930 = CARTESIAN_POINT ( 'NONE',  ( -2.500000000000002220, 3.061616997868386099E-16, -25.03750572909317285 ) ) ;
#12931 = CARTESIAN_POINT ( 'NONE',  ( 0.9762797500689124330, 41.46413394121043439, -6.086902470967093137 ) ) ;
#12932 = ORIENTED_EDGE ( 'NONE', *, *, #27087, .T. ) ;
#12933 = CYLINDRICAL_SURFACE ( 'NONE', #38608, 2.649999999999992806 ) ;
#12934 = CARTESIAN_POINT ( 'NONE',  ( 0.3622758884714600280, -17.25816669465019615, 39.50828911766968332 ) ) ;
#12935 = CARTESIAN_POINT ( 'NONE',  ( 0.6039202388192953519, 46.55074123944901743, -15.63944381705600684 ) ) ;
#12936 = AXIS2_PLACEMENT_3D ( 'NONE', #35312, #50612, #2690 ) ;
#12937 = ORIENTED_EDGE ( 'NONE', *, *, #25020, .T. ) ;
#12938 = ORIENTED_EDGE ( 'NONE', *, *, #22213, .F. ) ;
#12939 = CARTESIAN_POINT ( 'NONE',  ( 1.827119703190777988, -27.17434071502579229, -33.38937793923678043 ) ) ;
#12940 = CARTESIAN_POINT ( 'NONE',  ( 0.3622758884714730732, -37.74294673546571488, -20.83792692158958815 ) ) ;
#12941 = LINE ( 'NONE', #12632, #49822 ) ;
#12942 = CARTESIAN_POINT ( 'NONE',  ( 5.895881250540457863, -19.39944854657663242, 5.309338725022799466 ) ) ;
#12943 = B_SPLINE_CURVE_WITH_KNOTS ( 'NONE', 3,
 ( #6704, #54637, #50268, #30531, #21767, #17082 ),
 .UNSPECIFIED., .F., .F.,
 ( 4, 2, 4 ),
 ( 0.000000000000000000, 0.0002447195606305745293, 0.0004894391212611490585 ),
 .UNSPECIFIED. ) ;
#12944 = CARTESIAN_POINT ( 'NONE',  ( 0.6067375320500691949, -29.71715680108759727, 37.56348932307251687 ) ) ;
#12945 = CARTESIAN_POINT ( 'NONE',  ( 4.975610109902397937, 48.58133226360784818, -5.683622315980244366 ) ) ;
#12946 = CARTESIAN_POINT ( 'NONE',  ( 0.5837800304671207918, 4.739362457610067025, -46.65592969467970619 ) ) ;
#12947 = CIRCLE ( 'NONE', #37954, 42.92674063221959813 ) ;
#12948 = CARTESIAN_POINT ( 'NONE',  ( 0.9754292580325126805, -12.97161693114786019, 39.85052849204841863 ) ) ;
#12949 = CARTESIAN_POINT ( 'NONE',  ( 4.975801465491694664, -45.18341283946446651, -15.94009207553035523 ) ) ;
#12950 = VECTOR ( 'NONE', #56350, 1000.000000000000000 ) ;
#12951 = CARTESIAN_POINT ( 'NONE',  ( 0.6253024248130456542, 43.94107594871452704, 21.92318571483041012 ) ) ;
#12952 = DIRECTION ( 'NONE',  ( 0.000000000000000000, 0.000000000000000000, -1.000000000000000000 ) ) ;
#12953 = ADVANCED_FACE ( 'NONE', ( #30732 ), #7967, .F. ) ;
#12954 = CARTESIAN_POINT ( 'NONE',  ( 2.528190830796658517, -36.90586700523726194, -20.00527722239178985 ) ) ;
#12955 = CARTESIAN_POINT ( 'NONE',  ( -5.995132425357893702, -7.219211173946615823, 17.40647075750114325 ) ) ;
#12956 = CARTESIAN_POINT ( 'NONE',  ( 5.894904586330512508, -19.93362243062210482, 2.679572513488333474 ) ) ;
#12957 = CARTESIAN_POINT ( 'NONE',  ( 5.965394784446458765, 20.34787558161486842, -2.693446924985416491 ) ) ;
#12959 = EDGE_CURVE ( 'NONE', #29761, #18772, #48612, .T. ) ;
#12958 = CARTESIAN_POINT ( 'NONE',  ( 4.553261556744875094, -20.51767157960516741, 38.84024612145369559 ) ) ;
#12960 = FACE_OUTER_BOUND ( 'NONE', #31283, .T. ) ;
#12961 = ADVANCED_FACE ( 'NONE', ( #51688 ), #44778, .F. ) ;
#12962 = CARTESIAN_POINT ( 'NONE',  ( 2.643462169533600914, 11.09243630552468218, 46.73820883660209802 ) ) ;
#12963 = CARTESIAN_POINT ( 'NONE',  ( 0.6031356219577718170, 46.44562759437254584, -12.53544563195251271 ) ) ;
#12964 = EDGE_CURVE ( 'NONE', #58751, #33696, #61686, .T. ) ;
#12966 = VERTEX_POINT ( 'NONE', #27278 ) ;
#12965 = DIRECTION ( 'NONE',  ( 0.07906939808003035641, 0.7447223275783754204, -0.6626738904570698141 ) ) ;
#12967 = ORIENTED_EDGE ( 'NONE', *, *, #61957, .F. ) ;
#12968 = CARTESIAN_POINT ( 'NONE',  ( 5.895881250540457863, -18.51513737938377346, 7.856040314996277196 ) ) ;
#12969 = CARTESIAN_POINT ( 'NONE',  ( 5.895596859100789899, 3.341829471547073549, -19.83331437242869910 ) ) ;
#12970 = EDGE_CURVE ( 'NONE', #56562, #26742, #35759, .T. ) ;
#12971 = CARTESIAN_POINT ( 'NONE',  ( 0.7954196712028447358, 34.61997730204581813, -33.39101545667300286 ) ) ;
#12972 = VERTEX_POINT ( 'NONE', #14124 ) ;
#12973 = ORIENTED_EDGE ( 'NONE', *, *, #18619, .F. ) ;
#12974 = CARTESIAN_POINT ( 'NONE',  ( 0.3622758884714730732, -31.06363466427707820, -29.89648521331620756 ) ) ;
#12975 = CARTESIAN_POINT ( 'NONE',  ( 0.6252788684277207354, 5.398452368597682849, 48.80882136661001880 ) ) ;
#12976 = UNCERTAINTY_MEASURE_WITH_UNIT (LENGTH_MEASURE( 1.000000000000000082E-05 ), #29104, 'distance_accuracy_value', 'NONE');
#12977 = VERTEX_POINT ( 'NONE', #37946 ) ;
#12978 = ORIENTED_EDGE ( 'NONE', *, *, #38375, .T. ) ;
#12979 = ADVANCED_FACE ( 'NONE', ( #9088 ), #12726, .F. ) ;
#12980 = CARTESIAN_POINT ( 'NONE',  ( 1.231276596079881047, -37.78837162824498819, 18.14705873423338289 ) ) ;
#12981 = EDGE_CURVE ( 'NONE', #42702, #16409, #794, .T. ) ;
#12982 = VECTOR ( 'NONE', #2464, 999.9999999999998863 ) ;
#12983 = CARTESIAN_POINT ( 'NONE',  ( 0.8557997880470690211, -34.51495345639526136, -33.22501220301936797 ) ) ;
#12984 = CARTESIAN_POINT ( 'NONE',  ( 5.896782393890504181, -11.93563916323493146, 16.18847134979287361 ) ) ;
#12985 = B_SPLINE_CURVE_WITH_KNOTS ( 'NONE', 3,
 ( #14110, #9376, #28480, #33518, #9686, #11242, #54121, #20949, #15336, #49754, #44779, #1820, #6498, #44477, #53212, #35065, #43860, #10628, #6813 ),
 .UNSPECIFIED., .F., .F.,
 ( 4, 3, 3, 3, 3, 3, 4 ),
 ( 0.000000000000000000, 0.0002612768053151712211, 0.0003919133833142921181, 0.0005225499612322617293, 0.0006531865391693382353, 0.0008112755173415196405, 0.0009693688056799733320 ),
 .UNSPECIFIED. ) ;
#12986 = EDGE_LOOP ( 'NONE', ( #52, #25000, #55850, #16081 ) ) ;
#12987 = CARTESIAN_POINT ( 'NONE',  ( 3.680882792899936806, 25.57189948075129848, 40.59250320379022270 ) ) ;
#12988 = B_SPLINE_CURVE_WITH_KNOTS ( 'NONE', 3,
 ( #53428, #57816, #24326, #38760, #52199, #43457 ),
 .UNSPECIFIED., .F., .F.,
 ( 4, 2, 4 ),
 ( 1.196130537910465800E-16, 0.0002448718616795930421, 0.0004897437233590655210 ),
 .UNSPECIFIED. ) ;
#12989 = LINE ( 'NONE', #8555, #40627 ) ;
#12990 = B_SPLINE_CURVE_WITH_KNOTS ( 'NONE', 3,
 ( #12374, #32402, #17371, #55556 ),
 .UNSPECIFIED., .F., .F.,
 ( 4, 4 ),
 ( 5.594315114139762021E-17, 0.005004948556313858210 ),
 .UNSPECIFIED. ) ;
#12991 = CARTESIAN_POINT ( 'NONE',  ( 0.1095718737110178281, 0.2569529612657829865, -43.12372487139541732 ) ) ;
#12992 = ORIENTED_EDGE ( 'NONE', *, *, #27825, .T. ) ;
#12993 = ORIENTED_EDGE ( 'NONE', *, *, #23451, .T. ) ;
#12994 = CARTESIAN_POINT ( 'NONE',  ( 5.860006189529234355, -21.31760477694612987, 43.26650951066862660 ) ) ;
#12995 = AXIS2_PLACEMENT_3D ( 'NONE', #9935, #52832, #33750 ) ;
#12996 = ORIENTED_EDGE ( 'NONE', *, *, #15986, .T. ) ;
#12997 = CARTESIAN_POINT ( 'NONE',  ( 5.959547316686252039, 14.51632612601528827, -14.51128755440526241 ) ) ;
#12998 = CARTESIAN_POINT ( 'NONE',  ( 0.9972139404380309102, 17.02682566833184552, 39.38665787682671038 ) ) ;
#12999 = CARTESIAN_POINT ( 'NONE',  ( 0.6009453534118438522, 34.32439302680967330, -33.70725662590621852 ) ) ;
#13000 = CARTESIAN_POINT ( 'NONE',  ( 0.8753041380234530822, -31.30612550145381334, -37.82941757363182234 ) ) ;
#13001 = CARTESIAN_POINT ( 'NONE',  ( -2.601141883200662974, 6.503674101141085018, -13.43494140871240639 ) ) ;
#13002 = EDGE_CURVE ( 'NONE', #22082, #57516, #9010, .T. ) ;
#13003 = VERTEX_POINT ( 'NONE', #41711 ) ;
#13004 = CARTESIAN_POINT ( 'NONE',  ( 4.956653778116966613, 0.000000000000000000, 0.000000000000000000 ) ) ;
#13005 = CARTESIAN_POINT ( 'NONE',  ( 0.7954196712028464011, 24.79809944608775396, -41.21355366240439366 ) ) ;
#13006 = EDGE_CURVE ( 'NONE', #41352, #4083, #53043, .T. ) ;
#13007 = CARTESIAN_POINT ( 'NONE',  ( -6.057079549204054558, 3.065021114850809081, -19.01149327815301504 ) ) ;
#13008 = ORIENTED_EDGE ( 'NONE', *, *, #9405, .T. ) ;
#13009 = DIRECTION ( 'NONE',  ( 0.000000000000000000, -0.7071067811865461294, -0.7071067811865487940 ) ) ;
#13010 = CARTESIAN_POINT ( 'NONE',  ( 0.3676999524040366896, 44.06746933160592050, 2.002181318165502599 ) ) ;
#13011 = CARTESIAN_POINT ( 'NONE',  ( -6.072942160501519027, 12.01744408475444992, -15.04610248399301398 ) ) ;
#13012 = CARTESIAN_POINT ( 'NONE',  ( 0.8744876279028263033, -24.68559978112701714, -42.43785119236734715 ) ) ;
#13013 =( BOUNDED_SURFACE ( )  B_SPLINE_SURFACE ( 3, 1, ( 
 ( #36872, #3614 ),
 ( #41262, #50320 ),
 ( #36558, #8634 ),
 ( #7390, #40966 ) ),
 .UNSPECIFIED., .F., .F., .F. ) 
 B_SPLINE_SURFACE_WITH_KNOTS ( ( 4, 4 ),
 ( 2, 2 ),
 ( 0.000000000000000000, 1.000000000000000000 ),
 ( 0.000000000000000000, 1.000000000000000000 ),
 .UNSPECIFIED. ) 
 GEOMETRIC_REPRESENTATION_ITEM ( )  RATIONAL_B_SPLINE_SURFACE ( (
 ( 1.000000000000000000, 1.000000000000000000),
 ( 0.9953485035131437453, 0.8621029689291515030),
 ( 0.9953485035131437453, 0.8621029689291515030),
 ( 1.000000000000000000, 1.000000000000000000) ) ) 
 REPRESENTATION_ITEM ( '' )  SURFACE ( )  );
#13014 = ORIENTED_EDGE ( 'NONE', *, *, #31196, .T. ) ;
#13015 = CARTESIAN_POINT ( 'NONE',  ( 0.1129192098497447394, -12.08918212651769686, 42.43587472053614817 ) ) ;
#13016 = CARTESIAN_POINT ( 'NONE',  ( 3.270143674763207553, -11.98875605389984500, 6.605065939546772569 ) ) ;
#13017 = CARTESIAN_POINT ( 'NONE',  ( 4.833616638992208614, -45.44786513329592736, -8.578242093415591185 ) ) ;
#13018 = FACE_OUTER_BOUND ( 'NONE', #23658, .T. ) ;
#13019 = CARTESIAN_POINT ( 'NONE',  ( 0.6026112563231247332, -42.87342733809637707, 23.94598553388809492 ) ) ;
#13020 = FACE_OUTER_BOUND ( 'NONE', #52106, .T. ) ;
#13021 = CARTESIAN_POINT ( 'NONE',  ( 0.6067099128993225232, -6.954009037735842114, -47.38952184036241277 ) ) ;
#13022 = CARTESIAN_POINT ( 'NONE',  ( 1.227938101723748288, -22.18841447410744649, 36.73927144310504644 ) ) ;
#13023 = CARTESIAN_POINT ( 'NONE',  ( 8.000000000000012434, -80.00000000000001421, 2.649999999999992806 ) ) ;
#13024 = CARTESIAN_POINT ( 'NONE',  ( 4.691466044806103852, -44.51344083442437238, -2.583163953528327283 ) ) ;
#13025 = ORIENTED_EDGE ( 'NONE', *, *, #15942, .T. ) ;
#13026 = VECTOR ( 'NONE', #58623, 1000.000000000000114 ) ;
#13027 = CARTESIAN_POINT ( 'NONE',  ( 5.960221823109900008, 17.77295928189541740, 10.26751639438374397 ) ) ;
#13028 = CARTESIAN_POINT ( 'NONE',  ( 0.8557997880470697982, -17.48760788519248521, 44.60232077416680596 ) ) ;
#13029 = CARTESIAN_POINT ( 'NONE',  ( 0.1145239942831223490, -35.16543549781121669, -26.65215989284831011 ) ) ;
#13030 = CARTESIAN_POINT ( 'NONE',  ( 0.5830081025819920937, -34.96316152485596973, -31.25394967950578007 ) ) ;
#13031 = CARTESIAN_POINT ( 'NONE',  ( 0.7413678028165010536, -23.65209160105352382, -37.21645677204664793 ) ) ;
#13032 = CARTESIAN_POINT ( 'NONE',  ( 0.1129192098497455998, -38.68182264534154058, 21.22895156665764915 ) ) ;
#13033 = PRODUCT_CONTEXT ( 'NONE', #51153, 'mechanical' ) ;
#13035 = ADVANCED_FACE ( 'NONE', ( #47022, #42023 ), #32922, .T. ) ;
#13034 = CARTESIAN_POINT ( 'NONE',  ( 2.681483223904246760, -3.070647092368467668, -2.072929885643508434E-14 ) ) ;
#13036 = CARTESIAN_POINT ( 'NONE',  ( 3.661933894777873455, -45.01796196593215171, 13.63870468136689240 ) ) ;
#13037 = CARTESIAN_POINT ( 'NONE',  ( 0.6029443199889047422, -1.573945515703186748, 49.08217942764971298 ) ) ;
#13038 = EDGE_CURVE ( 'NONE', #31868, #47280, #34436, .T. ) ;
#13040 = EDGE_LOOP ( 'NONE', ( #29972, #17063 ) ) ;
#13039 = CARTESIAN_POINT ( 'NONE',  ( 0.5997462898726536595, -45.31995669577361951, 18.91172004968117903 ) ) ;
#13041 = VERTEX_POINT ( 'NONE', #24115 ) ;
#13042 = CONICAL_SURFACE ( 'NONE', #19073, 43.08621763946400307, 1.568696531533066763 ) ;
#13043 = CARTESIAN_POINT ( 'NONE',  ( 4.975610109902397937, -27.50982196586548412, -40.44328253918266824 ) ) ;
#13044 = CARTESIAN_POINT ( 'NONE',  ( 3.407937589446178528, 12.82481284928203813, 4.815089211105102684 ) ) ;
#13045 = EDGE_CURVE ( 'NONE', #45706, #11842, #53809, .T. ) ;
#13046 = CARTESIAN_POINT ( 'NONE',  ( 0.8557997880470599172, -41.93815086860273311, 23.15977007032308421 ) ) ;
#13047 = ORIENTED_EDGE ( 'NONE', *, *, #32341, .F. ) ;
#13048 = CARTESIAN_POINT ( 'NONE',  ( 0.5998501479064699549, -38.48283596222010061, -28.86886762351111457 ) ) ;
#13049 = CARTESIAN_POINT ( 'NONE',  ( 0.5809828226811565299, -23.47450554821739743, 41.74875432577639600 ) ) ;
#13050 = CARTESIAN_POINT ( 'NONE',  ( 0.5998501479064708430, -44.24259072156073813, -18.89267974119652749 ) ) ;
#13051 = ORIENTED_EDGE ( 'NONE', *, *, #11348, .F. ) ;
#13052 = ORIENTED_EDGE ( 'NONE', *, *, #12262, .F. ) ;
#13053 = CARTESIAN_POINT ( 'NONE',  ( 3.407937589446174087, -12.47329436636624678, -5.663729899985203708 ) ) ;
#13054 = CARTESIAN_POINT ( 'NONE',  ( 1.834102595619085507, 37.61045569671126998, 22.92708806506842834 ) ) ;
#13055 = LINE ( 'NONE', #37170, #49937 ) ;
#13056 = CARTESIAN_POINT ( 'NONE',  ( 5.960721111146673579, -20.34914600876573587, -2.685391721745965299 ) ) ;
#13057 = CARTESIAN_POINT ( 'NONE',  ( 0.2224561200757611545, 11.89200283918790646, -41.44719785461218464 ) ) ;
#13058 = ORIENTED_EDGE ( 'NONE', *, *, #13701, .T. ) ;
#13059 = AXIS2_PLACEMENT_3D ( 'NONE', #35850, #15812, #11413 ) ;
#13060 = CARTESIAN_POINT ( 'NONE',  ( -6.077587904424778920, 12.00112336472187025, -15.05885318935865236 ) ) ;
#13061 = ORIENTED_EDGE ( 'NONE', *, *, #24473, .F. ) ;
#13062 = CARTESIAN_POINT ( 'NONE',  ( -6.077587904424778920, 17.85108912406252912, -7.220432014686311462 ) ) ;
#13063 = DIRECTION ( 'NONE',  ( 1.000000000000000000, 0.000000000000000000, 0.000000000000000000 ) ) ;
#13064 = CARTESIAN_POINT ( 'NONE',  ( 0.9780106845699481077, 4.506814239222374674, -41.66557178137100692 ) ) ;
#13065 = CARTESIAN_POINT ( 'NONE',  ( 4.956653778116975495, -14.93973939759918323, 45.71126949320244393 ) ) ;
#13066 = ORIENTED_EDGE ( 'NONE', *, *, #14558, .F. ) ;
#13067 = ORIENTED_EDGE ( 'NONE', *, *, #56551, .F. ) ;
#13068 = CARTESIAN_POINT ( 'NONE',  ( 4.553261556744875094, 43.92594400279101308, 0.2258523573163287723 ) ) ;
#13069 = DIRECTION ( 'NONE',  ( 1.000000000000000000, 0.000000000000000000, 0.000000000000000000 ) ) ;
#13070 = ORIENTED_EDGE ( 'NONE', *, *, #39777, .F. ) ;
#13071 = DIRECTION ( 'NONE',  ( -1.000000000000000000, -0.000000000000000000, -0.000000000000000000 ) ) ;
#13072 = VECTOR ( 'NONE', #39176, 1000.000000000000114 ) ;
#13073 = EDGE_CURVE ( 'NONE', #5057, #35775, #2671, .T. ) ;
#13074 = ORIENTED_EDGE ( 'NONE', *, *, #35820, .T. ) ;
#13075 = CARTESIAN_POINT ( 'NONE',  ( 4.303969348037246512, 30.97035057417713588, -36.81598326424517609 ) ) ;
#13076 = ORIENTED_EDGE ( 'NONE', *, *, #181, .T. ) ;
#13077 = CARTESIAN_POINT ( 'NONE',  ( -6.010958268070873523, -18.20513189769804896, -4.863021950010837813 ) ) ;
#13078 = CARTESIAN_POINT ( 'NONE',  ( 0.7954196712028472893, -17.60078400783993047, -44.76287685048079368 ) ) ;
#13079 = CIRCLE ( 'NONE', #40107, 48.09070567114147110 ) ;
#13080 = CARTESIAN_POINT ( 'NONE',  ( 0.1095718737110177865, -26.45591486700782369, 34.05592812063336083 ) ) ;
#13081 = ORIENTED_EDGE ( 'NONE', *, *, #12828, .F. ) ;
#13082 = B_SPLINE_CURVE_WITH_KNOTS ( 'NONE', 3,
 ( #38182, #52863, #39107, #24672 ),
 .UNSPECIFIED., .F., .F.,
 ( 4, 4 ),
 ( 0.000000000000000000, 0.004444103432399267896 ),
 .UNSPECIFIED. ) ;
#13083 = CARTESIAN_POINT ( 'NONE',  ( 0.1158816050234198897, -27.51540855527343865, -34.49412027203399589 ) ) ;
#13084 = CARTESIAN_POINT ( 'NONE',  ( 0.1147471544378677183, -27.26760129513139930, 34.69049016781103489 ) ) ;
#13085 = CARTESIAN_POINT ( 'NONE',  ( 0.5837799406558212834, -41.81448599028684754, 21.23187017069644611 ) ) ;
#13086 = ORIENTED_EDGE ( 'NONE', *, *, #51253, .T. ) ;
#13087 = CARTESIAN_POINT ( 'NONE',  ( 0.9769922540276050338, -22.17659144084161582, -35.56023547661229145 ) ) ;
#13088 = CARTESIAN_POINT ( 'NONE',  ( 0.8744876279028263033, -38.80702141274021955, -30.07266432244763621 ) ) ;
#13089 = DIRECTION ( 'NONE',  ( 0.07500201931887538753, 0.6334382584228924751, 0.7701497710603204538 ) ) ;
#13090 = LINE ( 'NONE', #23096, #57928 ) ;
#13091 = DIRECTION ( 'NONE',  ( -0.1011922191286467043, -0.08272061902645741482, -0.9914219253051141933 ) ) ;
#13092 = EDGE_LOOP ( 'NONE', ( #36741, #22358 ) ) ;
#13093 = CARTESIAN_POINT ( 'NONE',  ( 5.965394784446460541, -2.664747781315973896, -20.35165389555757187 ) ) ;
#13094 = DIRECTION ( 'NONE',  ( -1.000000000000000000, -3.135800716341489291E-16, 1.298891185607901956E-16 ) ) ;
#13095 = ORIENTED_EDGE ( 'NONE', *, *, #28488, .T. ) ;
#13096 = CARTESIAN_POINT ( 'NONE',  ( 4.303969348037258058, -46.98258166031682492, -10.35452842635891990 ) ) ;
#13097 = CARTESIAN_POINT ( 'NONE',  ( 4.335381028904216727, 45.77817886910109024, -17.43889867775290625 ) ) ;
#13098 = CARTESIAN_POINT ( 'NONE',  ( 0.2940135542858993145, -34.86814986296420926, 27.02688797892369976 ) ) ;
#13099 = CARTESIAN_POINT ( 'NONE',  ( 0.1368894036331293751, 19.84133884650108115, -39.41043768726326135 ) ) ;
#13100 = CARTESIAN_POINT ( 'NONE',  ( 5.958863334805807099, 2.680345151634340617, 20.34989385289158648 ) ) ;
#13101 = CARTESIAN_POINT ( 'NONE',  ( 0.1073791018717483448, -41.52698815987176317, 11.62916352156079824 ) ) ;
#13103 = B_SPLINE_CURVE_WITH_KNOTS ( 'NONE', 3,
 ( #5793, #21461, #20247, #30853, #7028, #29938 ),
 .UNSPECIFIED., .F., .F.,
 ( 4, 2, 4 ),
 ( 8.541065402288461036E-17, 0.0002293366620881459063, 0.0004586733241762064317 ),
 .UNSPECIFIED. ) ;
#13102 = DIRECTION ( 'NONE',  ( 0.09722883295013592941, -0.9607671998409492709, 0.2597555422949351933 ) ) ;
#13104 =( NAMED_UNIT ( * ) PLANE_ANGLE_UNIT ( ) SI_UNIT ( $, .RADIAN. ) );
#13106 = EDGE_CURVE ( 'NONE', #49884, #23849, #13460, .T. ) ;
#13105 = CARTESIAN_POINT ( 'NONE',  ( 0.9722240750034576440, -42.61332880321396033, -5.023189755349382501 ) ) ;
#13107 =( BOUNDED_SURFACE ( )  B_SPLINE_SURFACE ( 3, 1, ( 
 ( #22849, #32885 ),
 ( #18779, #51959 ),
 ( #42287, #37587 ),
 ( #9357, #56655 ) ),
 .UNSPECIFIED., .F., .F., .F. ) 
 B_SPLINE_SURFACE_WITH_KNOTS ( ( 4, 4 ),
 ( 2, 2 ),
 ( 0.000000000000000000, 1.000000000000000000 ),
 ( 0.000000000000000000, 1.000000000000000000 ),
 .UNSPECIFIED. ) 
 GEOMETRIC_REPRESENTATION_ITEM ( )  RATIONAL_B_SPLINE_SURFACE ( (
 ( 1.000000000000000000, 1.000000000000000000),
 ( 0.9729067724841187204, 0.9999501103223794596),
 ( 0.9729067724841187204, 0.9999501103223794596),
 ( 1.000000000000000000, 1.000000000000000000) ) ) 
 REPRESENTATION_ITEM ( '' )  SURFACE ( )  );
#13108 = CARTESIAN_POINT ( 'NONE',  ( 0.6039202388192952409, 27.95228209933733865, 40.37615185091387815 ) ) ;
#13109 = CARTESIAN_POINT ( 'NONE',  ( 4.834790513006555379, -4.995710817784499547, -46.98544683568999858 ) ) ;
#13110 = ADVANCED_FACE ( 'NONE', ( #39475 ), #36746, .T. ) ;
#13111 = CARTESIAN_POINT ( 'NONE',  ( 4.553261556744875094, -25.31600221269659201, 35.89762663172006540 ) ) ;
#13112 = DIRECTION ( 'NONE',  ( 1.836766033387207149E-16, -1.000000000000000000, 0.000000000000000000 ) ) ;
#13113 = CARTESIAN_POINT ( 'NONE',  ( 0.1313383488274142974, 30.94058105930520952, 30.03864748494556736 ) ) ;
#13114 = CARTESIAN_POINT ( 'NONE',  ( 0.5786265663353153954, -44.52624106864131193, -17.66171603226127829 ) ) ;
#13115 = EDGE_CURVE ( 'NONE', #11251, #26923, #28713, .T. ) ;
#13116 = CARTESIAN_POINT ( 'NONE',  ( 0.9268187852002115479, 16.15318250627089469, 41.02229915335962573 ) ) ;
#13117 = LINE ( 'NONE', #31906, #36480 ) ;
#13118 = CARTESIAN_POINT ( 'NONE',  ( 0.5817216825391118284, 46.53606797270585815, 5.799080086286046765 ) ) ;
#13119 = CARTESIAN_POINT ( 'NONE',  ( 0.7954190325252780136, -42.08256085583556683, -23.29293489839720976 ) ) ;
#13120 =( BOUNDED_SURFACE ( )  B_SPLINE_SURFACE ( 3, 1, ( 
 ( #14222, #13599 ),
 ( #9494, #9190 ),
 ( #52713, #28297 ),
 ( #5081, #28599 ) ),
 .UNSPECIFIED., .F., .F., .F. ) 
 B_SPLINE_SURFACE_WITH_KNOTS ( ( 4, 4 ),
 ( 2, 2 ),
 ( 0.000000000000000000, 1.000000000000000000 ),
 ( 0.000000000000000000, 1.000000000000000000 ),
 .UNSPECIFIED. ) 
 GEOMETRIC_REPRESENTATION_ITEM ( )  RATIONAL_B_SPLINE_SURFACE ( (
 ( 1.000000000000000000, 1.000000000000000000),
 ( 0.9732289882329797637, 0.9999525324661233672),
 ( 0.9732289882329797637, 0.9999525324661233672),
 ( 1.000000000000000000, 1.000000000000000000) ) ) 
 REPRESENTATION_ITEM ( '' )  SURFACE ( )  );
#13121 = ORIENTED_EDGE ( 'NONE', *, *, #12060, .T. ) ;
#13122 = CARTESIAN_POINT ( 'NONE',  ( 0.8557997880470697982, 47.37054680076715840, -7.156447707085226817 ) ) ;
#13123 = EDGE_CURVE ( 'NONE', #23728, #24678, #45639, .T. ) ;
#13124 = FACE_OUTER_BOUND ( 'NONE', #53760, .T. ) ;
#13125 = CARTESIAN_POINT ( 'NONE',  ( 3.390910168358336918, 28.07862399391833819, -33.84801340022468708 ) ) ;
#13126 = CARTESIAN_POINT ( 'NONE',  ( 0.8554163680231720024, -26.01084021241217314, -39.04666009476586908 ) ) ;
#13127 = ORIENTED_EDGE ( 'NONE', *, *, #57754, .F. ) ;
#13128 = EDGE_CURVE ( 'NONE', #9574, #60249, #5975, .T. ) ;
#13129 = FACE_OUTER_BOUND ( 'NONE', #24353, .T. ) ;
#13130 = B_SPLINE_CURVE_WITH_KNOTS ( 'NONE', 3,
 ( #52349, #51734, #8829, #42370, #39219, #19177, #53886, #33580, #34198, #53571, #24472, #10694, #58270, #58578, #14780, #10387, #15090, #652, #33893 ),
 .UNSPECIFIED., .F., .F.,
 ( 4, 3, 3, 3, 3, 3, 4 ),
 ( 0.000000000000000000, 0.0002612768053151668301, 0.0003919133833142900581, 0.0005225499612322602114, 0.0006531865391693349827, 0.0008112755173415168216, 0.0009693688056799697542 ),
 .UNSPECIFIED. ) ;
#13131 = ORIENTED_EDGE ( 'NONE', *, *, #14610, .F. ) ;
#13132 = CARTESIAN_POINT ( 'NONE',  ( 1.479689385636123067, -26.54425251156986576, 35.17081892520713637 ) ) ;
#13133 = ORIENTED_EDGE ( 'NONE', *, *, #47160, .T. ) ;
#13134 = CARTESIAN_POINT ( 'NONE',  ( 3.407937589446178528, 7.243367523631024874, 11.62731850632886754 ) ) ;
#13135 = CARTESIAN_POINT ( 'NONE',  ( -6.016489644550737204, 18.19999694163064063, 4.881234076340438932 ) ) ;
#13136 = ORIENTED_EDGE ( 'NONE', *, *, #31544, .T. ) ;
#13137 = FACE_OUTER_BOUND ( 'NONE', #56021, .T. ) ;
#13138 = CARTESIAN_POINT ( 'NONE',  ( -6.072942160501519027, -14.65319399899845543, -12.49352103759128596 ) ) ;
#13139 = VERTEX_POINT ( 'NONE', #48847 ) ;
#13140 = CARTESIAN_POINT ( 'NONE',  ( 0.9757787079277449038, 21.42002160630820384, 37.17954582422744636 ) ) ;
#13141 = DIRECTION ( 'NONE',  ( -0.07500201931887527651, 0.4673421949333779746, -0.8808893062882211522 ) ) ;
#13142 = B_SPLINE_CURVE_WITH_KNOTS ( 'NONE', 3,
 ( #13859, #38591, #33576, #28537, #47978, #28855, #57640, #4708, #14775, #33887, #52650, #5029, #24154, #326, #52964, #29165, #19787, #5335, #52035 ),
 .UNSPECIFIED., .F., .F.,
 ( 4, 3, 3, 3, 3, 3, 4 ),
 ( 1.355252715606880543E-20, 0.0002612768053151681854, 0.0003919133833142889739, 0.0005225499612322556577, 0.0006531865391693332480, 0.0008112755173415167132, 0.0009693688056799707299 ),
 .UNSPECIFIED. ) ;
#13143 = EDGE_LOOP ( 'NONE', ( #42590, #35543, #60478, #36483 ) ) ;
#13144 = CARTESIAN_POINT ( 'NONE',  ( -6.077587904424778920, 13.83688374988438241, -13.39166417911216911 ) ) ;
#13145 = EDGE_LOOP ( 'NONE', ( #57183, #58309, #12234, #47416 ) ) ;
#13146 = CARTESIAN_POINT ( 'NONE',  ( 5.958863334805807099, -20.35021240744037030, 2.677925489610294196 ) ) ;
#13147 = EDGE_CURVE ( 'NONE', #5867, #25607, #43556, .T. ) ;
#13148 = VERTEX_POINT ( 'NONE', #19740 ) ;
#13149 = VERTEX_POINT ( 'NONE', #49155 ) ;
#13150 = DIRECTION ( 'NONE',  ( 0.000000000000000000, 0.000000000000000000, -1.000000000000000000 ) ) ;
#13151 = LINE ( 'NONE', #32250, #57381 ) ;
#13152 = CARTESIAN_POINT ( 'NONE',  ( 0.7056759521545000746, -44.57577085471505285, 14.58593438299126177 ) ) ;
#13153 = CARTESIAN_POINT ( 'NONE',  ( 0.1092565886968784594, -16.21587544131350000, 39.95965440403619340 ) ) ;
#13154 = CARTESIAN_POINT ( 'NONE',  ( 0.6031356755773454870, 44.44549206087155824, 18.40989784469875801 ) ) ;
#13155 = ORIENTED_EDGE ( 'NONE', *, *, #181, .F. ) ;
#13156 = CARTESIAN_POINT ( 'NONE',  ( 0.5549461598389365813, 5.107917383263871791, 43.80784034248385694 ) ) ;
#13157 = DIRECTION ( 'NONE',  ( -1.000000000000000000, -0.000000000000000000, -0.000000000000000000 ) ) ;
#13158 = CARTESIAN_POINT ( 'NONE',  ( 0.5804410086790514622, -46.82762660194602944, 2.587129429331442854 ) ) ;
#13159 = EDGE_LOOP ( 'NONE', ( #46438, #10040, #35648, #40443 ) ) ;
#13160 = ORIENTED_EDGE ( 'NONE', *, *, #57829, .F. ) ;
#13161 = AXIS2_PLACEMENT_3D ( 'NONE', #58376, #58684, #39316 ) ;
#13162 = VECTOR ( 'NONE', #35140, 1000.000000000000114 ) ;
#13163 = FACE_OUTER_BOUND ( 'NONE', #35100, .T. ) ;
#13164 = DIRECTION ( 'NONE',  ( -1.000000000000000000, -0.000000000000000000, -0.000000000000000000 ) ) ;
#13165 = DIRECTION ( 'NONE',  ( -0.07906939808003035641, -0.9390317839750951245, 0.3346152103115038190 ) ) ;
#13166 = CARTESIAN_POINT ( 'NONE',  ( 3.270143674763207553, -6.605065939546730824, -11.98875605389986454 ) ) ;
#13167 = CARTESIAN_POINT ( 'NONE',  ( 1.157643937452369487, 8.912044576298065124, -40.95824381079869880 ) ) ;
#13168 = ORIENTED_EDGE ( 'NONE', *, *, #58806, .T. ) ;
#13169 = CARTESIAN_POINT ( 'NONE',  ( 4.694002226626921015, 36.74006825548360666, -26.98985283451062855 ) ) ;
#13170 = CARTESIAN_POINT ( 'NONE',  ( -5.995132425357893702, -11.46484027925357729, -14.95525565067286600 ) ) ;
#13171 = DIRECTION ( 'NONE',  ( 0.000000000000000000, 1.000000000000000000, -1.224646799147353207E-16 ) ) ;
#13173 = CARTESIAN_POINT ( 'NONE',  ( 3.727782113643637096, -39.30990089286451195, -19.68526016335944107 ) ) ;
#13172 = B_SPLINE_CURVE_WITH_KNOTS ( 'NONE', 3,
 ( #55187, #31712, #60496, #1946, #25769, #59266 ),
 .UNSPECIFIED., .F., .F.,
 ( 4, 2, 4 ),
 ( 1.710438460654249876E-17, 0.0002293319059085093036, 0.0004586638118170015309 ),
 .UNSPECIFIED. ) ;
#13174 = CARTESIAN_POINT ( 'NONE',  ( 3.894904216938897878, -41.52606794860570005, -14.41214811206100599 ) ) ;
#13175 = DIRECTION ( 'NONE',  ( 0.07836865515943411409, 0.9608836331491523719, 0.2656332009267416416 ) ) ;
#13176 = ORIENTED_EDGE ( 'NONE', *, *, #51332, .F. ) ;
#13177 = CARTESIAN_POINT ( 'NONE',  ( 0.9756950546413931669, 21.37039651692549924, -37.20808764646317002 ) ) ;
#13178 = CARTESIAN_POINT ( 'NONE',  ( 4.962356264823608143, 0.000000000000000000, 0.000000000000000000 ) ) ;
#13179 = ADVANCED_FACE ( 'NONE', ( #44491 ), #16387, .F. ) ;
#13180 = CARTESIAN_POINT ( 'NONE',  ( 0.9730545539215883499, -6.101350888304943432, 42.47233286818615028 ) ) ;
#13181 = CARTESIAN_POINT ( 'NONE',  ( 0.1103744047535531458, 21.59576373962417151, -37.32746539760798754 ) ) ;
#13182 = CARTESIAN_POINT ( 'NONE',  ( 0.9790850452238875068, 29.17097364564380868, 30.08972626708911946 ) ) ;
#13183 = EDGE_CURVE ( 'NONE', #4007, #49007, #2720, .T. ) ;
#13184 = CARTESIAN_POINT ( 'NONE',  ( 0.5827359174754822568, 6.611633125157481139, -47.43746338751526537 ) ) ;
#13185 = CARTESIAN_POINT ( 'NONE',  ( 0.5807400328401637335, -46.12278621143487811, -12.92266817606064322 ) ) ;
#13186 = CARTESIAN_POINT ( 'NONE',  ( -6.063463321072276813, -12.95783560055426697, -14.24482183210721509 ) ) ;
#13187 = ORIENTED_EDGE ( 'NONE', *, *, #4568, .T. ) ;
#13188 = CARTESIAN_POINT ( 'NONE',  ( -6.063463321072276813, 19.25669258467947387, -0.01559418547018221260 ) ) ;
#13189 = CARTESIAN_POINT ( 'NONE',  ( 3.221118495291108719, 23.59276081282231274, -37.12334921435170543 ) ) ;
#13190 = DIRECTION ( 'NONE',  ( 0.000000000000000000, 0.000000000000000000, -1.000000000000000000 ) ) ;
#13191 = CARTESIAN_POINT ( 'NONE',  ( -6.016761891674565099, 16.32039929810269996, -9.418621820384323939 ) ) ;
#13192 = ORIENTED_EDGE ( 'NONE', *, *, #20997, .T. ) ;
#13193 = EDGE_CURVE ( 'NONE', #47724, #58012, #3004, .T. ) ;
#13194 = CARTESIAN_POINT ( 'NONE',  ( 0.7056555295713289322, 46.04438433984174139, -13.20840017674969857 ) ) ;
#13195 = CARTESIAN_POINT ( 'NONE',  ( 0.9783242366443573035, -41.79629446811009075, -3.066636421480622765 ) ) ;
#13196 = VECTOR ( 'NONE', #35649, 1000.000000000000000 ) ;
#13197 =( NAMED_UNIT ( * ) PLANE_ANGLE_UNIT ( ) SI_UNIT ( $, .RADIAN. ) );
#13198 = CIRCLE ( 'NONE', #46205, 42.08604991992415023 ) ;
#13199 = EDGE_LOOP ( 'NONE', ( #26353, #34243, #7054, #22416 ) ) ;
#13200 = CARTESIAN_POINT ( 'NONE',  ( 1.231276596079887264, 19.39962232756291272, -37.16088568059149111 ) ) ;
#13201 = CARTESIAN_POINT ( 'NONE',  ( 0.5817217712918333339, -45.86342913730425863, -9.786767687844841745 ) ) ;
#13202 = CARTESIAN_POINT ( 'NONE',  ( 0.8753041380234471980, 49.05142151719384458, -2.257515230414626206 ) ) ;
#13203 = VERTEX_POINT ( 'NONE', #25353 ) ;
#13204 = CARTESIAN_POINT ( 'NONE',  ( 0.5998501479064699549, 29.69975237324562656, 37.84527566984866809 ) ) ;
#13205 = VERTEX_POINT ( 'NONE', #52609 ) ;
#13206 = ORIENTED_EDGE ( 'NONE', *, *, #23040, .F. ) ;
#13207 = CARTESIAN_POINT ( 'NONE',  ( -6.077587904424778920, -8.901182807328959612, 17.07527352707539592 ) ) ;
#13208 = VERTEX_POINT ( 'NONE', #38243 ) ;
#13209 = CARTESIAN_POINT ( 'NONE',  ( -6.016489644550737204, 4.872725758886191194, 18.20227673842146032 ) ) ;
#13210 = ORIENTED_EDGE ( 'NONE', *, *, #21424, .F. ) ;
#13211 = CARTESIAN_POINT ( 'NONE',  ( 0.8554163680231816613, 17.71207986799935696, 43.44522643353848679 ) ) ;
#13212 = CARTESIAN_POINT ( 'NONE',  ( 0.6067099128993235224, 13.08009036336202513, 46.07641759122967784 ) ) ;
#13213 = CARTESIAN_POINT ( 'NONE',  ( 0.9745511491811748028, 16.10518088436905870, 39.77127619790144308 ) ) ;
#13214 = EDGE_LOOP ( 'NONE', ( #33408, #16109, #4688, #32339 ) ) ;
#13215 = DIRECTION ( 'NONE',  ( -1.000000000000000000, -1.836909530733573776E-16, 1.925929944387235853E-32 ) ) ;
#13216 = CARTESIAN_POINT ( 'NONE',  ( 0.9730545539215883499, 30.69604515769692554, -29.98130006528829483 ) ) ;
#13217 = CARTESIAN_POINT ( 'NONE',  ( 0.7413678028165008316, -37.95542240817268009, 22.44709338839723500 ) ) ;
#13218 = CARTESIAN_POINT ( 'NONE',  ( 0.7954196712028465122, -41.21355366240445761, -24.79809944608760475 ) ) ;
#13219 = VERTEX_POINT ( 'NONE', #5591 ) ;
#13220 = ADVANCED_FACE ( 'NONE', ( #919 ), #35623, .F. ) ;
#13221 = CARTESIAN_POINT ( 'NONE',  ( 1.318516776095788545, 3.857556137907071747, 2.454790609853964971E-15 ) ) ;
#13222 = CARTESIAN_POINT ( 'NONE',  ( 4.549368137175248350, -32.13400537129945178, 28.46244473166616729 ) ) ;
#13223 = ORIENTED_EDGE ( 'NONE', *, *, #58886, .T. ) ;
#13224 = CARTESIAN_POINT ( 'NONE',  ( 0.9757402383260949108, -42.90839848328079853, -0.08489923450683498074 ) ) ;
#13225 = EDGE_CURVE ( 'NONE', #27212, #9094, #22434, .T. ) ;
#13226 = VERTEX_POINT ( 'NONE', #44801 ) ;
#13227 = CARTESIAN_POINT ( 'NONE',  ( 4.967162193818130511, 0.000000000000000000, 0.000000000000000000 ) ) ;
#13228 = CARTESIAN_POINT ( 'NONE',  ( 0.5832655196449132440, 11.09274990485192269, -45.56518498285437602 ) ) ;
#13229 = ORIENTED_EDGE ( 'NONE', *, *, #53017, .T. ) ;
#13230 = DIRECTION ( 'NONE',  ( -1.000000000000000000, -0.000000000000000000, -0.000000000000000000 ) ) ;
#13231 = CARTESIAN_POINT ( 'NONE',  ( 4.956445790444004906, -46.59545590650544966, 6.811867512257108181 ) ) ;
#13232 = EDGE_CURVE ( 'NONE', #37323, #32724, #13754, .T. ) ;
#13233 = CARTESIAN_POINT ( 'NONE',  ( 0.5800708119828335008, 24.48933355903764308, 41.16171018093167788 ) ) ;
#13234 = DIRECTION ( 'NONE',  ( -1.000000000000000000, -0.000000000000000000, -0.000000000000000000 ) ) ;
#13235 = VERTEX_POINT ( 'NONE', #20967 ) ;
#13236 = LINE ( 'NONE', #14172, #16963 ) ;
#13237 = CARTESIAN_POINT ( 'NONE',  ( 0.9787284016396609054, -41.80215183015796043, 2.985984142163401689 ) ) ;
#13238 = CARTESIAN_POINT ( 'NONE',  ( 4.956653778116991482, -14.93973939759855263, -45.71126949320266419 ) ) ;
#13239 = CARTESIAN_POINT ( 'NONE',  ( -6.017396004339687465, 18.68211039806567086, -2.458362590802601222 ) ) ;
#13240 = AXIS2_PLACEMENT_3D ( 'NONE', #39465, #58519, #10017 ) ;
#13241 = CARTESIAN_POINT ( 'NONE',  ( 120.0000507999999968, 0.000000000000000000, 0.000000000000000000 ) ) ;
#13242 = CARTESIAN_POINT ( 'NONE',  ( -4.908599999999998964, 0.000000000000000000, 48.35291015139245019 ) ) ;
#13243 = VECTOR ( 'NONE', #30784, 1000.000000000000114 ) ;
#13244 = B_SPLINE_CURVE_WITH_KNOTS ( 'NONE', 3,
 ( #25663, #15668, #25357, #34771 ),
 .UNSPECIFIED., .F., .F.,
 ( 4, 4 ),
 ( 0.000000000000000000, 0.005014147105413706458 ),
 .UNSPECIFIED. ) ;
#13245 = CARTESIAN_POINT ( 'NONE',  ( 0.5998501479064699549, 28.86886762351124958, -38.48283596222000114 ) ) ;
#13246 = CARTESIAN_POINT ( 'NONE',  ( -6.016761891674564211, 11.47373234755503013, 14.94721834528419002 ) ) ;
#13247 = EDGE_CURVE ( 'NONE', #2081, #13939, #42643, .T. ) ;
#13248 = CARTESIAN_POINT ( 'NONE',  ( 4.322998006666165516, -4.155494336618380302, -47.80838462754064011 ) ) ;
#13249 = CARTESIAN_POINT ( 'NONE',  ( 0.5834584762367753807, 40.44190349954094899, -23.74212354333551644 ) ) ;
#13250 = EDGE_CURVE ( 'NONE', #19512, #14527, #45776, .T. ) ;
#13251 = CARTESIAN_POINT ( 'NONE',  ( 0.9790724872846768845, 32.86481170631836335, 26.00460269817044434 ) ) ;
#13252 = CARTESIAN_POINT ( 'NONE',  ( -2.708315649062910779, -7.544341609840062191, 12.54007339125002041 ) ) ;
#13253 = CARTESIAN_POINT ( 'NONE',  ( 4.956653778116975495, -2.599733001514665798, 48.02038484091099235 ) ) ;
#13254 = DIRECTION ( 'NONE',  ( 0.000000000000000000, 0.000000000000000000, 1.000000000000000000 ) ) ;
#13255 = CARTESIAN_POINT ( 'NONE',  ( 0.5807400328401574052, 17.82553128098408735, 44.45848844984448789 ) ) ;
#13256 = CARTESIAN_POINT ( 'NONE',  ( 3.240649175237394708, -16.12010403042567575, -40.93173785030273137 ) ) ;
#13257 = EDGE_CURVE ( 'NONE', #22938, #53786, #37436, .T. ) ;
#13258 = CARTESIAN_POINT ( 'NONE',  ( 2.301529144917015213, 46.71331407887422671, 11.18385659262694531 ) ) ;
#13259 = CARTESIAN_POINT ( 'NONE',  ( 4.967162193818130511, 8.839793687085215623, 42.16965968614196925 ) ) ;
#13260 = CARTESIAN_POINT ( 'NONE',  ( 0.6009453534118438522, 46.57942464365174118, -12.02914401651124443 ) ) ;
#13262 = EDGE_LOOP ( 'NONE', ( #42285, #21849, #48684, #61867 ) ) ;
#13261 = CYLINDRICAL_SURFACE ( 'NONE', #21338, 5.612499999999999822 ) ;
#13263 = ORIENTED_EDGE ( 'NONE', *, *, #44191, .T. ) ;
#13264 = DIRECTION ( 'NONE',  ( -1.000000000000000000, -0.000000000000000000, -0.000000000000000000 ) ) ;
#13265 = CARTESIAN_POINT ( 'NONE',  ( -6.001507490154111224, 18.20581304543304668, -4.862106078787734376 ) ) ;
#13266 = DIRECTION ( 'NONE',  ( 0.000000000000000000, 0.000000000000000000, 1.000000000000000000 ) ) ;
#13267 = ORIENTED_EDGE ( 'NONE', *, *, #54076, .T. ) ;
#13268 = EDGE_CURVE ( 'NONE', #4433, #22519, #17234, .T. ) ;
#13269 = VERTEX_POINT ( 'NONE', #20552 ) ;
#13270 = CARTESIAN_POINT ( 'NONE',  ( 0.5832366564991505742, -33.67434452455936622, 34.05963937630789928 ) ) ;
#13271 = CARTESIAN_POINT ( 'NONE',  ( 4.963659409799332067, -20.22157859941758318, 39.92545197189544837 ) ) ;
#13272 = ORIENTED_EDGE ( 'NONE', *, *, #42970, .T. ) ;
#13273 = ORIENTED_EDGE ( 'NONE', *, *, #34200, .T. ) ;
#13274 = CARTESIAN_POINT ( 'NONE',  ( 5.439999999999996838, 15.14599999999999902, 0.000000000000000000 ) ) ;
#13275 = CARTESIAN_POINT ( 'NONE',  ( 0.5807400328401574052, -17.82553128098376050, -44.45848844984462289 ) ) ;
#13276 = CARTESIAN_POINT ( 'NONE',  ( 1.000433927950261870, -2.058517538525916457, -41.85906333395944756 ) ) ;
#13277 = ORIENTED_EDGE ( 'NONE', *, *, #48499, .T. ) ;
#13278 = EDGE_LOOP ( 'NONE', ( #43888, #12067, #33557, #15498 ) ) ;
#13279 = CARTESIAN_POINT ( 'NONE',  ( 0.8744876279028306332, -26.20733431478126008, -41.51536677536140729 ) ) ;
#13280 = B_SPLINE_CURVE_WITH_KNOTS ( 'NONE', 3,
 ( #29331, #15253, #53433, #53729, #14957, #6114 ),
 .UNSPECIFIED., .F., .F.,
 ( 4, 2, 4 ),
 ( 5.294859796737922701E-18, 0.0002448709889506563977, 0.0004897419779013074828 ),
 .UNSPECIFIED. ) ;
#13281 = CIRCLE ( 'NONE', #51264, 43.92652462719577500 ) ;
#13282 = CARTESIAN_POINT ( 'NONE',  ( 4.956653778116975495, 9.917440902361160937, 47.05699031914952712 ) ) ;
#13283 = ORIENTED_EDGE ( 'NONE', *, *, #15908, .F. ) ;
#13284 =( BOUNDED_SURFACE ( )  B_SPLINE_SURFACE ( 3, 1, ( 
 ( #20510, #15817 ),
 ( #34932, #48701 ),
 ( #39323, #11420 ),
 ( #10811, #11120 ) ),
 .UNSPECIFIED., .F., .F., .F. ) 
 B_SPLINE_SURFACE_WITH_KNOTS ( ( 4, 4 ),
 ( 2, 2 ),
 ( 0.000000000000000000, 1.000000000000000000 ),
 ( 0.000000000000000000, 1.000000000000000000 ),
 .UNSPECIFIED. ) 
 GEOMETRIC_REPRESENTATION_ITEM ( )  RATIONAL_B_SPLINE_SURFACE ( (
 ( 1.000000000000000000, 1.000000000000000000),
 ( 0.9953485035131437453, 0.8621029689291523912),
 ( 0.9953485035131437453, 0.8621029689291523912),
 ( 1.000000000000000000, 1.000000000000000000) ) ) 
 REPRESENTATION_ITEM ( '' )  SURFACE ( )  );
#13285 = CARTESIAN_POINT ( 'NONE',  ( 0.1092355843206037486, 21.30139719602319559, 37.49628696754466262 ) ) ;
#13286 = ORIENTED_EDGE ( 'NONE', *, *, #37430, .F. ) ;
#13287 = ORIENTED_EDGE ( 'NONE', *, *, #47782, .F. ) ;
#13288 = ADVANCED_FACE ( 'NONE', ( #1115 ), #20859, .F. ) ;
#13289 = CARTESIAN_POINT ( 'NONE',  ( -6.078726893082806448, 0.6205993875984882058, -19.24600991553398188 ) ) ;
#13290 = ORIENTED_EDGE ( 'NONE', *, *, #10760, .F. ) ;
#13291 = CARTESIAN_POINT ( 'NONE',  ( 0.5827357941260210561, 44.10984861950480962, -18.66407988912442306 ) ) ;
#13292 = CARTESIAN_POINT ( 'NONE',  ( 4.975801465491694664, 15.94009207553051510, -45.18341283946441678 ) ) ;
#13293 = FACE_OUTER_BOUND ( 'NONE', #37322, .T. ) ;
#13294 = CARTESIAN_POINT ( 'NONE',  ( 0.5997462898726536595, -30.20781297212619165, 38.71743361310707598 ) ) ;
#13295 = CARTESIAN_POINT ( 'NONE',  ( 1.112077966505211624, -43.83978140853107419, -4.593897166977904511 ) ) ;
#13296 = EDGE_CURVE ( 'NONE', #11901, #51356, #10456, .T. ) ;
#13297 = ORIENTED_EDGE ( 'NONE', *, *, #30939, .T. ) ;
#13298 = CARTESIAN_POINT ( 'NONE',  ( -6.010958268070873523, -4.863021950010776528, 18.20513189769807028 ) ) ;
#13299 = CARTESIAN_POINT ( 'NONE',  ( 0.1310142868023689011, -10.54463319394704435, -41.81449350725025482 ) ) ;
#13300 = ADVANCED_FACE ( 'NONE', ( #43774 ), #43680, .T. ) ;
#13301 = CARTESIAN_POINT ( 'NONE',  ( 0.9730545539215883499, -21.01499094264522682, -37.40983423658496321 ) ) ;
#13302 = CONICAL_SURFACE ( 'NONE', #10303, 42.08604991992415023, 1.569615340895231137 ) ;
#13303 = ORIENTED_EDGE ( 'NONE', *, *, #10443, .T. ) ;
#13304 = CARTESIAN_POINT ( 'NONE',  ( 1.231276596079881047, -21.83837404314779462, -35.78214904347746739 ) ) ;
#13305 = CARTESIAN_POINT ( 'NONE',  ( 5.895881250540457863, 12.98890680526564267, -15.35630103939177360 ) ) ;
#13306 = ADVANCED_FACE ( 'NONE', ( #5800 ), #52781, .F. ) ;
#13307 = CARTESIAN_POINT ( 'NONE',  ( 4.335381028904216727, -28.85261930641616956, 39.58892783119247127 ) ) ;
#13308 = DIRECTION ( 'NONE',  ( -0.8191520442889896891, 1.003171929053522158E-16, 0.5735764363510490460 ) ) ;
#13309 = ADVANCED_FACE ( 'NONE', ( #15857 ), #34975, .F. ) ;
#13310 = ORIENTED_EDGE ( 'NONE', *, *, #16811, .F. ) ;
#13311 = CARTESIAN_POINT ( 'NONE',  ( 4.975610109902397937, -46.59897809419055648, 14.86555238512586463 ) ) ;
#13312 = CARTESIAN_POINT ( 'NONE',  ( 4.694002226626921015, 7.615834493547636974, -44.94756763622505247 ) ) ;
#13313 = CARTESIAN_POINT ( 'NONE',  ( 0.5807400328401574052, 24.41979442053169080, 41.20655774452978193 ) ) ;
#13314 = PRODUCT ( 'straight bevel gear(static)_iso_ISO - Straight bevel gear 2M 48GT 49PT 20PA 5FW ---48O25H100MD16.0N', 'straight bevel gear(static)_iso_ISO - Straight bevel gear 2M 48GT 49PT 20PA 5FW ---48O25H100MD16.0N', '', ( #17104 ) ) ;
#13315 = CARTESIAN_POINT ( 'NONE',  ( 0.5824936645240094135, -29.99832043048538210, -36.04634448026914839 ) ) ;
#13316 = CARTESIAN_POINT ( 'NONE',  ( 0.9741495583595186636, -42.59115242362810250, 5.208308905147964296 ) ) ;
#13317 = CARTESIAN_POINT ( 'NONE',  ( 5.894904586330512508, -9.664823957841305102, -17.63861077085095630 ) ) ;
#13318 = CARTESIAN_POINT ( 'NONE',  ( 0.3622758884714730732, 42.62881903538210793, -6.444611261694146442 ) ) ;
#13319 = CARTESIAN_POINT ( 'NONE',  ( 1.154321713695928286, 20.73950268329824809, 37.57248787340945739 ) ) ;
#13320 = FACE_OUTER_BOUND ( 'NONE', #9657, .T. ) ;
#13321 = EDGE_CURVE ( 'NONE', #59308, #2462, #44877, .T. ) ;
#13322 = CARTESIAN_POINT ( 'NONE',  ( 0.9783242366443558602, 41.90778699278978792, 0.2681036618207567890 ) ) ;
#13323 = CARTESIAN_POINT ( 'NONE',  ( 2.282816707992316729, -9.105513224129030192, -46.08238921033910174 ) ) ;
#13324 = ORIENTED_EDGE ( 'NONE', *, *, #15910, .T. ) ;
#13325 = FACE_OUTER_BOUND ( 'NONE', #38813, .T. ) ;
#13326 = CARTESIAN_POINT ( 'NONE',  ( 1.231276596079881047, -18.40965318903201364, 37.66113965983544887 ) ) ;
#13327 = CARTESIAN_POINT ( 'NONE',  ( 5.965394784446458765, 5.298374383010636457, -19.82972329408680778 ) ) ;
#13328 = FACE_OUTER_BOUND ( 'NONE', #31328, .T. ) ;
#13329 = B_SPLINE_CURVE_WITH_KNOTS ( 'NONE', 3,
 ( #50468, #59235, #40483, #26982 ),
 .UNSPECIFIED., .F., .F.,
 ( 4, 4 ),
 ( 0.000000000000000000, 0.005014147105413696917 ),
 .UNSPECIFIED. ) ;
#13330 = CARTESIAN_POINT ( 'NONE',  ( 0.1129192098497455998, -1.898585089632445433, 44.08341142019953907 ) ) ;
#13331 = AXIS2_PLACEMENT_3D ( 'NONE', #25969, #19060, #17810 ) ;
#13332 = CARTESIAN_POINT ( 'NONE',  ( 1.660531772554323604, -3.660093687634888848, -2.106514470958295182E-14 ) ) ;
#13333 = APPLICATION_PROTOCOL_DEFINITION ( 'draft international standard', 'automotive_design', 1998, #23534 ) ;
#13334 = CARTESIAN_POINT ( 'NONE',  ( 0.5824936645240085253, -25.54018381715007990, 39.33112240486524769 ) ) ;
#13335 = EDGE_CURVE ( 'NONE', #37250, #55180, #1722, .T. ) ;
#13336 = CARTESIAN_POINT ( 'NONE',  ( 0.5839879327111903162, 12.48412918464437915, 46.24044206955228731 ) ) ;
#13337 = DIRECTION ( 'NONE',  ( 0.1011922191286468015, -0.1460712814909308488, 0.9840850143719378496 ) ) ;
#13339 = ORIENTED_EDGE ( 'NONE', *, *, #24913, .T. ) ;
#13338 = CARTESIAN_POINT ( 'NONE',  ( 0.1368894036331279040, -35.73859056403340873, -25.87690998592599456 ) ) ;
#13341 = ORIENTED_EDGE ( 'NONE', *, *, #44909, .T. ) ;
#13340 = B_SPLINE_CURVE_WITH_KNOTS ( 'NONE', 3,
 ( #35654, #45665, #55642, #35966, #25927, #27159, #7096, #40985, #32174, #46285, #22460, #41584, #45062, #2093, #21224, #50042, #59422, #59736, #16852 ),
 .UNSPECIFIED., .F., .F.,
 ( 4, 3, 3, 3, 3, 3, 4 ),
 ( 1.250973872328959318E-17, 0.0002732106629380675819, 0.0004098138914053775462, 0.0005464171197651557970, 0.0006830203481512715953, 0.0008196235766963839075, 0.001011968216111141594 ),
 .UNSPECIFIED. ) ;
#13342 = DIRECTION ( 'NONE',  ( 1.000000000000000000, 0.000000000000000000, 0.000000000000000000 ) ) ;
#13343 = CARTESIAN_POINT ( 'NONE',  ( 4.303969348037258058, 10.35452842635908510, -46.98258166031678940 ) ) ;
#13344 = ADVANCED_FACE ( 'NONE', ( #49053 ), #38665, .T. ) ;
#13345 = VERTEX_POINT ( 'NONE', #4721 ) ;
#13346 = CARTESIAN_POINT ( 'NONE',  ( 0.5997462898726536595, 11.43624519451716992, -47.75734421002901797 ) ) ;
#13348 = DIRECTION ( 'NONE',  ( 1.000000000000000000, 0.000000000000000000, 0.000000000000000000 ) ) ;
#13347 = VECTOR ( 'NONE', #47381, 1000.000000000000000 ) ;
#13349 = CARTESIAN_POINT ( 'NONE',  ( 2.643462169533600914, 32.97543604874627476, 34.93025802711738237 ) ) ;
#13351 = EDGE_CURVE ( 'NONE', #59557, #37326, #50610, .T. ) ;
#13350 = ORIENTED_EDGE ( 'NONE', *, *, #25260, .T. ) ;
#13352 = ORIENTED_EDGE ( 'NONE', *, *, #59905, .F. ) ;
#13353 = DIRECTION ( 'NONE',  ( 0.02222222222222222307, -0.9997530559290660479, 0.000000000000000000 ) ) ;
#13354 = CARTESIAN_POINT ( 'NONE',  ( 4.553261556744875094, 38.16266689001181334, 21.75202109381179483 ) ) ;
#13355 = CARTESIAN_POINT ( 'NONE',  ( 0.5806925824938499181, 46.89268439822727430, 0.5463627657667635695 ) ) ;
#13356 = CARTESIAN_POINT ( 'NONE',  ( 5.959828726073459926, -20.34941966491237508, -2.683617577144310484 ) ) ;
#13357 = B_SPLINE_CURVE_WITH_KNOTS ( 'NONE', 3,
 ( #31222, #36251, #53093, #61252, #47187, #10197 ),
 .UNSPECIFIED., .F., .F.,
 ( 4, 2, 4 ),
 ( 7.564592850777163085E-18, 0.0002291978881530175695, 0.0004583957763060276039 ),
 .UNSPECIFIED. ) ;
#13358 = CARTESIAN_POINT ( 'NONE',  ( 0.5804410086790514622, 43.38796872094628299, -17.80460676694616851 ) ) ;
#13359 = CARTESIAN_POINT ( 'NONE',  ( 0.7044674535452954967, 17.74870190915637025, -45.79067921914693073 ) ) ;
#13360 = ORIENTED_EDGE ( 'NONE', *, *, #5688, .T. ) ;
#13361 =( BOUNDED_SURFACE ( )  B_SPLINE_SURFACE ( 3, 1, ( 
 ( #42955, #37957 ),
 ( #24748, #19752 ),
 ( #3, #18832 ),
 ( #14137, #10037 ) ),
 .UNSPECIFIED., .F., .F., .F. ) 
 B_SPLINE_SURFACE_WITH_KNOTS ( ( 4, 4 ),
 ( 2, 2 ),
 ( 0.000000000000000000, 1.000000000000000000 ),
 ( 0.000000000000000000, 1.000000000000000000 ),
 .UNSPECIFIED. ) 
 GEOMETRIC_REPRESENTATION_ITEM ( )  RATIONAL_B_SPLINE_SURFACE ( (
 ( 1.000000000000000000, 1.000000000000000000),
 ( 0.9751682680413298332, 0.9999560080971552356),
 ( 0.9751682680413298332, 0.9999560080971552356),
 ( 1.000000000000000000, 1.000000000000000000) ) ) 
 REPRESENTATION_ITEM ( '' )  SURFACE ( )  );
#13362 = CARTESIAN_POINT ( 'NONE',  ( 0.8557997880470697982, 46.50333260518559086, 11.51622788066474534 ) ) ;
#13363 = FACE_OUTER_BOUND ( 'NONE', #49862, .T. ) ;
#13364 = ORIENTED_EDGE ( 'NONE', *, *, #9538, .T. ) ;
#13365 = CARTESIAN_POINT ( 'NONE',  ( 6.999999999999991118, 80.00000000000001421, 2.649999999999992806 ) ) ;
#13366 = CARTESIAN_POINT ( 'NONE',  ( 7.999999999999996447, -2.778489794828638662E-13, 80.00000000000001421 ) ) ;
#13367 = CARTESIAN_POINT ( 'NONE',  ( 0.8751705887134423323, -7.160166390004656378, 47.55935879196458416 ) ) ;
#13368 = EDGE_CURVE ( 'NONE', #6110, #22076, #37637, .T. ) ;
#13369 = B_SPLINE_CURVE_WITH_KNOTS ( 'NONE', 3,
 ( #25810, #45555, #55533, #50236 ),
 .UNSPECIFIED., .F., .F.,
 ( 4, 4 ),
 ( 6.254634441385501517E-18, 0.004566006591234647236 ),
 .UNSPECIFIED. ) ;
#13370 = AXIS2_PLACEMENT_3D ( 'NONE', #15636, #2113, #39767 ) ;
#13371 = ORIENTED_EDGE ( 'NONE', *, *, #54120, .T. ) ;
#13372 = ORIENTED_EDGE ( 'NONE', *, *, #50640, .T. ) ;
#13373 = CARTESIAN_POINT ( 'NONE',  ( 0.9756008150404595902, 0.1421465480002861714, 42.90824081423206593 ) ) ;
#13374 = FACE_OUTER_BOUND ( 'NONE', #10177, .T. ) ;
#13375 = EDGE_CURVE ( 'NONE', #2228, #51399, #24166, .T. ) ;
#13376 = DIRECTION ( 'NONE',  ( 0.000000000000000000, 0.000000000000000000, 1.000000000000000000 ) ) ;
#13377 = ORIENTED_EDGE ( 'NONE', *, *, #22018, .F. ) ;
#13378 = CARTESIAN_POINT ( 'NONE',  ( 7.000000000000021316, -80.00000000000001421, -1.954818893553044610E-31 ) ) ;
#13380 = ORIENTED_EDGE ( 'NONE', *, *, #46624, .F. ) ;
#13379 = EDGE_CURVE ( 'NONE', #19517, #53916, #41877, .T. ) ;
#13381 = CARTESIAN_POINT ( 'NONE',  ( 3.390910168358336918, 43.50063370814297770, 6.464673504796084380 ) ) ;
#13382 = CARTESIAN_POINT ( 'NONE',  ( 0.5997462898726536595, -25.00873172704263325, 42.26245340191598387 ) ) ;
#13383 = ADVANCED_FACE ( 'NONE', ( #10701 ), #10361, .F. ) ;
#13384 = CARTESIAN_POINT ( 'NONE',  ( 4.967162193818130511, -23.56777426397153974, -36.06913038482822742 ) ) ;
#13385 = ORIENTED_EDGE ( 'NONE', *, *, #42997, .T. ) ;
#13386 = CARTESIAN_POINT ( 'NONE',  ( 0.5988103564986355654, -33.58571500783082797, 34.44345003622193246 ) ) ;
#13387 = EDGE_CURVE ( 'NONE', #33079, #33083, #16649, .T. ) ;
#13388 = CARTESIAN_POINT ( 'NONE',  ( 1.000110580585052533, -30.63720285853708347, -28.59684045094404325 ) ) ;
#13389 = CARTESIAN_POINT ( 'NONE',  ( 5.894904586330512508, -18.51743364446310025, -7.850736480391433680 ) ) ;
#13390 = CIRCLE ( 'NONE', #60387, 8.000000000000000000 ) ;
#13391 = ORIENTED_EDGE ( 'NONE', *, *, #18274, .F. ) ;
#13392 = CARTESIAN_POINT ( 'NONE',  ( 2.500000000000000000, 0.000000000000000000, 0.000000000000000000 ) ) ;
#13393 = FACE_OUTER_BOUND ( 'NONE', #8533, .T. ) ;
#13394 = CARTESIAN_POINT ( 'NONE',  ( 0.8554163680231816613, -26.01084021241216604, -39.04666009476586908 ) ) ;
#13395 = EDGE_CURVE ( 'NONE', #52432, #34503, #18014, .T. ) ;
#13396 = CARTESIAN_POINT ( 'NONE',  ( 4.956653778117001252, 47.05699031914963371, -9.917440902360649346 ) ) ;
#13397 = CARTESIAN_POINT ( 'NONE',  ( 0.6064782688330846439, 36.36007787089019416, 29.61889909570526669 ) ) ;
#13398 = ORIENTED_EDGE ( 'NONE', *, *, #8342, .F. ) ;
#13399 = CARTESIAN_POINT ( 'NONE',  ( 0.6000166863083106206, -13.47152005829862276, 47.22649287240490423 ) ) ;
#13400 = LINE ( 'NONE', #18405, #31811 ) ;
#13401 = ORIENTED_EDGE ( 'NONE', *, *, #20926, .F. ) ;
#13402 = FACE_OUTER_BOUND ( 'NONE', #6526, .T. ) ;
#13403 = CARTESIAN_POINT ( 'NONE',  ( -49.49999999999975842, 1.232595164407830946E-29, 1.078520768856852078E-29 ) ) ;
#13404 = CARTESIAN_POINT ( 'NONE',  ( 0.8557997880470690211, 19.17299735372009550, 43.90420959842187187 ) ) ;
#13405 = CARTESIAN_POINT ( 'NONE',  ( 0.9741495583595178864, 5.992561317325774795, -42.48790363482595467 ) ) ;
#13406 = CARTESIAN_POINT ( 'NONE',  ( -6.015611763856276717, 18.68122482568283260, -2.465697960550860657 ) ) ;
#13407 = CARTESIAN_POINT ( 'NONE',  ( -6.078726893082806448, -4.288195875146425529, -18.77246434022707788 ) ) ;
#13408 = CARTESIAN_POINT ( 'NONE',  ( 0.3622758884714600280, -25.58609868863743841, -34.70015533914819628 ) ) ;
#13409 = CARTESIAN_POINT ( 'NONE',  ( 0.1129192098497447394, 39.54191224844646513, -19.58032082273713570 ) ) ;
#13410 = CARTESIAN_POINT ( 'NONE',  ( 5.960221823109900008, -17.77840967225727553, 10.25807604135590978 ) ) ;
#13411 = CARTESIAN_POINT ( 'NONE',  ( 0.7954196712028467342, -44.09776749253668271, -19.20650004024986401 ) ) ;
#13412 = CARTESIAN_POINT ( 'NONE',  ( 0.1081432562775997835, -6.048481838666351251, 42.69830087850301226 ) ) ;
#13413 = ORIENTED_EDGE ( 'NONE', *, *, #526, .T. ) ;
#13414 = CARTESIAN_POINT ( 'NONE',  ( 5.895881250540457863, 17.95317081027896577, 9.067046898811559785 ) ) ;
#13415 = LINE ( 'NONE', #22496, #19236 ) ;
#13416 = VECTOR ( 'NONE', #28559, 1000.000000000000227 ) ;
#13417 = CARTESIAN_POINT ( 'NONE',  ( 0.9730545539215883499, 30.69604515769650632, 29.98130006528872826 ) ) ;
#13418 = CARTESIAN_POINT ( 'NONE',  ( 4.958415959904821868, 1.012370948441741358, -45.41122172861453521 ) ) ;
#13419 = CARTESIAN_POINT ( 'NONE',  ( 4.226256110419179812, 31.85118181789737335, -30.27093435608539096 ) ) ;
#13420 = EDGE_CURVE ( 'NONE', #32705, #53183, #55614, .T. ) ;
#13421 = ORIENTED_EDGE ( 'NONE', *, *, #3840, .F. ) ;
#13422 = CARTESIAN_POINT ( 'NONE',  ( 0.9752570700956808558, 11.32817567195968955, -41.38610171411344396 ) ) ;
#13423 = CARTESIAN_POINT ( 'NONE',  ( 5.901764892641288895, -16.87177170878354104, 45.97102116384157000 ) ) ;
#13424 = CARTESIAN_POINT ( 'NONE',  ( 1.296416391601052487, 28.79733114477846101, -33.36197076034524400 ) ) ;
#13425 = CARTESIAN_POINT ( 'NONE',  ( -19.85946183287803635, -7.946284510655257094, -0.9343843706440355668 ) ) ;
#13426 = ORIENTED_EDGE ( 'NONE', *, *, #34759, .T. ) ;
#13427 = CYLINDRICAL_SURFACE ( 'NONE', #37981, 10.00000000000000711 ) ;
#13428 = CIRCLE ( 'NONE', #14460, 2.649999999999985700 ) ;
#13429 = CARTESIAN_POINT ( 'NONE',  ( 0.6009452777970410997, 23.67489783211094334, -41.87890062806012281 ) ) ;
#13430 = ORIENTED_EDGE ( 'NONE', *, *, #6796, .F. ) ;
#13431 = CARTESIAN_POINT ( 'NONE',  ( 1.154321713695928953, 41.23280394713393093, 11.90271797554028232 ) ) ;
#13432 = ORIENTED_EDGE ( 'NONE', *, *, #8099, .T. ) ;
#13433 = DIRECTION ( 'NONE',  ( 0.000000000000000000, 0.000000000000000000, -1.000000000000000000 ) ) ;
#13434 = CARTESIAN_POINT ( 'NONE',  ( 5.960221823109900008, 14.51763960716758106, 14.50993159119815701 ) ) ;
#13435 = ORIENTED_EDGE ( 'NONE', *, *, #39603, .F. ) ;
#13436 = CARTESIAN_POINT ( 'NONE',  ( 4.975610109902397937, -10.32228546579698403, -47.81108480154335183 ) ) ;
#13437 = CARTESIAN_POINT ( 'NONE',  ( 0.8751705887134423323, 44.08562551107055327, 19.22545746485676688 ) ) ;
#13438 = ORIENTED_EDGE ( 'NONE', *, *, #49569, .F. ) ;
#13439 = CARTESIAN_POINT ( 'NONE',  ( 0.5824936645240087474, -7.440785221794779858, -46.30197505855910123 ) ) ;
#13440 = FACE_OUTER_BOUND ( 'NONE', #44457, .T. ) ;
#13441 = ORIENTED_EDGE ( 'NONE', *, *, #561, .F. ) ;
#13442 = CARTESIAN_POINT ( 'NONE',  ( 0.5997462898726536595, -39.04071682475809268, 29.78882441375220580 ) ) ;
#13443 = EDGE_CURVE ( 'NONE', #1361, #462, #30633, .T. ) ;
#13444 = ORIENTED_EDGE ( 'NONE', *, *, #15200, .T. ) ;
#13445 = CARTESIAN_POINT ( 'NONE',  ( 0.8751705887134553219, 24.81530984069150136, 41.19904111682516401 ) ) ;
#13447 = EDGE_CURVE ( 'NONE', #47186, #43343, #12639, .T. ) ;
#13446 = EDGE_LOOP ( 'NONE', ( #57143, #49411, #13831, #9865 ) ) ;
#13448 = ORIENTED_EDGE ( 'NONE', *, *, #22786, .F. ) ;
#13449 = CARTESIAN_POINT ( 'NONE',  ( 4.549368137175248350, 42.06008734272383975, 8.582197505784577629 ) ) ;
#13450 = CARTESIAN_POINT ( 'NONE',  ( 0.9790850452238877288, -37.38141985983193649, 18.94641864643972085 ) ) ;
#13451 = CARTESIAN_POINT ( 'NONE',  ( 2.624215991343620935, 40.85210347989567481, -25.21574086439663276 ) ) ;
#13452 = EDGE_CURVE ( 'NONE', #11409, #21723, #54579, .T. ) ;
#13453 = CARTESIAN_POINT ( 'NONE',  ( 0.1073791018717578927, -16.95003405440338895, 39.65380858626186722 ) ) ;
#13454 = CARTESIAN_POINT ( 'NONE',  ( 0.5786265663353196143, -37.55861529268533161, -29.72999788434331592 ) ) ;
#13455 = ORIENTED_EDGE ( 'NONE', *, *, #24282, .F. ) ;
#13456 = CARTESIAN_POINT ( 'NONE',  ( 0.9752132459055854463, 11.33038172416152634, 41.38545930839050868 ) ) ;
#13457 = EDGE_CURVE ( 'NONE', #42659, #22425, #51598, .T. ) ;
#13458 = LINE ( 'NONE', #23459, #10780 ) ;
#13459 = CARTESIAN_POINT ( 'NONE',  ( 0.7056313189692728916, -34.21346071282268042, 32.08095618914278191 ) ) ;
#13461 = ORIENTED_EDGE ( 'NONE', *, *, #53167, .F. ) ;
#13460 = B_SPLINE_CURVE_WITH_KNOTS ( 'NONE', 3,
 ( #10334, #29427, #44189, #38547 ),
 .UNSPECIFIED., .F., .F.,
 ( 4, 4 ),
 ( 0.000000000000000000, 0.005004741218457418872 ),
 .UNSPECIFIED. ) ;
#13462 =( BOUNDED_SURFACE ( )  B_SPLINE_SURFACE ( 3, 1, ( 
 ( #2363, #6122 ),
 ( #35293, #21482 ),
 ( #44404, #25565 ),
 ( #1741, #11478 ) ),
 .UNSPECIFIED., .F., .F., .F. ) 
 B_SPLINE_SURFACE_WITH_KNOTS ( ( 4, 4 ),
 ( 2, 2 ),
 ( 0.000000000000000000, 1.000000000000000000 ),
 ( 0.000000000000000000, 1.000000000000000000 ),
 .UNSPECIFIED. ) 
 GEOMETRIC_REPRESENTATION_ITEM ( )  RATIONAL_B_SPLINE_SURFACE ( (
 ( 1.000000000000000000, 1.000000000000000000),
 ( 0.9729067724841187204, 0.9999501103223794596),
 ( 0.9729067724841187204, 0.9999501103223794596),
 ( 1.000000000000000000, 1.000000000000000000) ) ) 
 REPRESENTATION_ITEM ( '' )  SURFACE ( )  );
#13463 = B_SPLINE_CURVE_WITH_KNOTS ( 'NONE', 3,
 ( #3078, #41334, #24911, #42557, #44344, #4596 ),
 .UNSPECIFIED., .F., .F.,
 ( 4, 2, 4 ),
 ( 6.106282077343214115E-18, 0.0002291472222819936945, 0.0004582944445639813174 ),
 .UNSPECIFIED. ) ;
#13464 = ORIENTED_EDGE ( 'NONE', *, *, #55742, .T. ) ;
#13465 = FACE_OUTER_BOUND ( 'NONE', #38244, .T. ) ;
#13466 = DIRECTION ( 'NONE',  ( 0.07500201931887537365, -0.6834640454944218568, -0.7261209235481992375 ) ) ;
#13467 = CARTESIAN_POINT ( 'NONE',  ( 0.9762797500689124330, 40.28286501695569655, 11.55922018180428168 ) ) ;
#13468 = CARTESIAN_POINT ( 'NONE',  ( 0.1102144999581333162, -34.28951223307547025, 26.15241010112966435 ) ) ;
#13470 = AXIS2_PLACEMENT_3D ( 'NONE', #34635, #44665, #1702 ) ;
#13469 = CARTESIAN_POINT ( 'NONE',  ( 2.879087469061463178, -34.20017424174309895, 27.68482903356619929 ) ) ;
#13471 = ADVANCED_FACE ( 'NONE', ( #21953 ), #36359, .F. ) ;
#13472 = ORIENTED_EDGE ( 'NONE', *, *, #42954, .F. ) ;
#13473 = CARTESIAN_POINT ( 'NONE',  ( 0.5839254288179566155, 47.47429404163007405, 6.341681103464710922 ) ) ;
#13474 = EDGE_CURVE ( 'NONE', #940, #3592, #40640, .T. ) ;
#13475 = CARTESIAN_POINT ( 'NONE',  ( 1.231276596079887264, -16.87422718933211030, 38.37365278131431268 ) ) ;
#13476 = CARTESIAN_POINT ( 'NONE',  ( 1.657374760986086493, 42.98942532183876608, -9.633263089436098880 ) ) ;
#13477 = AXIS2_PLACEMENT_3D ( 'NONE', #12834, #13760, #12520 ) ;
#13478 = LINE ( 'NONE', #14103, #975 ) ;
#13479 = CARTESIAN_POINT ( 'NONE',  ( 3.221118495291108719, -41.44247251342186189, -14.74051870308588441 ) ) ;
#13480 = CARTESIAN_POINT ( 'NONE',  ( 0.6254311100348660668, -5.596225872411697111, -47.77988293940227749 ) ) ;
#13481 =( BOUNDED_SURFACE ( )  B_SPLINE_SURFACE ( 3, 1, ( 
 ( #3277, #41231 ),
 ( #54977, #46236 ),
 ( #11795, #35910 ),
 ( #22104, #27111 ) ),
 .UNSPECIFIED., .F., .F., .F. ) 
 B_SPLINE_SURFACE_WITH_KNOTS ( ( 4, 4 ),
 ( 2, 2 ),
 ( 0.000000000000000000, 1.000000000000000000 ),
 ( 0.000000000000000000, 1.000000000000000000 ),
 .UNSPECIFIED. ) 
 GEOMETRIC_REPRESENTATION_ITEM ( )  RATIONAL_B_SPLINE_SURFACE ( (
 ( 1.000000000000000000, 1.000000000000000000),
 ( 0.9952954269826590483, 0.8620686068821339365),
 ( 0.9952954269826590483, 0.8620686068821339365),
 ( 1.000000000000000000, 1.000000000000000000) ) ) 
 REPRESENTATION_ITEM ( '' )  SURFACE ( )  );
#13482 = ORIENTED_EDGE ( 'NONE', *, *, #41406, .T. ) ;
#13483 = CARTESIAN_POINT ( 'NONE',  ( -6.079354080745853928, -19.21634661680158374, -1.234899976152050272 ) ) ;
#13484 = CARTESIAN_POINT ( 'NONE',  ( 0.6846871229502932144, 38.52803883689338704, -28.47437962186088001 ) ) ;
#13485 = CARTESIAN_POINT ( 'NONE',  ( 0.6039202388192952409, -8.009480623390196286, 48.45009734760630948 ) ) ;
#13486 = CARTESIAN_POINT ( 'NONE',  ( 4.975610109902397937, -5.269241389991576874, 48.62802178077752302 ) ) ;
#13487 = CARTESIAN_POINT ( 'NONE',  ( 5.974727161628369032, -7.840226266082411577, -18.96851388233655200 ) ) ;
#13488 = CARTESIAN_POINT ( 'NONE',  ( 0.5839879327111905383, 6.161619650335993903, -47.49806740880204359 ) ) ;
#13489 = CARTESIAN_POINT ( 'NONE',  ( 3.782542959838397945, 18.67355142067374985, 37.66346148106973146 ) ) ;
#13490 = CARTESIAN_POINT ( 'NONE',  ( 4.975801465491694664, 40.15204426031534268, -26.14269827151636605 ) ) ;
#13491 = VECTOR ( 'NONE', #23263, 999.9999999999998863 ) ;
#13492 = EDGE_CURVE ( 'NONE', #40053, #11576, #28615, .T. ) ;
#13493 = CARTESIAN_POINT ( 'NONE',  ( 5.896782393890504181, -13.98685533979004347, -14.45316451791091161 ) ) ;
#13494 = EDGE_LOOP ( 'NONE', ( #28921, #57633, #48781, #525 ) ) ;
#13495 = FACE_OUTER_BOUND ( 'NONE', #2417, .T. ) ;
#13496 = B_SPLINE_CURVE_WITH_KNOTS ( 'NONE', 3,
 ( #2803, #35741, #16940, #11943 ),
 .UNSPECIFIED., .F., .F.,
 ( 4, 4 ),
 ( 2.414736334504793811E-17, 0.004564976165746186844 ),
 .UNSPECIFIED. ) ;
#13497 = CARTESIAN_POINT ( 'NONE',  ( 0.5839880159502339740, 46.25220722086348957, 12.44022138820703205 ) ) ;
#13498 = CARTESIAN_POINT ( 'NONE',  ( 4.962356264823596597, 39.89814050050772920, 13.39305724859313429 ) ) ;
#13499 = CARTESIAN_POINT ( 'NONE',  ( 0.7056759521544998526, -2.409567365275814943, 46.83954327519839467 ) ) ;
#13500 = EDGE_LOOP ( 'NONE', ( #17290, #5080, #3560, #11939 ) ) ;
#13501 = CARTESIAN_POINT ( 'NONE',  ( 4.691466044806103852, 9.025781474740853128, 43.66525414675645322 ) ) ;
#13502 = CARTESIAN_POINT ( 'NONE',  ( 0.9762797500689124330, -41.77809974471938403, -3.303810967047359881 ) ) ;
#13503 = ORIENTED_EDGE ( 'NONE', *, *, #16715, .F. ) ;
#13504 = CARTESIAN_POINT ( 'NONE',  ( 0.1149546198390367924, 4.509486755524008572, -43.89317821968435851 ) ) ;
#13505 = CARTESIAN_POINT ( 'NONE',  ( -6.016489644550737204, 18.68142234211824260, 2.463898142942827274 ) ) ;
#13506 = CIRCLE ( 'NONE', #58501, 5.000000000000000000 ) ;
#13507 = CARTESIAN_POINT ( 'NONE',  ( 0.5998501479064699549, 24.50586714782546593, 41.39809967730496254 ) ) ;
#13508 = VERTEX_POINT ( 'NONE', #16960 ) ;
#13509 = CARTESIAN_POINT ( 'NONE',  ( -6.001507490154110336, 14.94036486426028887, -11.48377994779686162 ) ) ;
#13510 = CIRCLE ( 'NONE', #37581, 5.100000000000000533 ) ;
#13511 = ORIENTED_EDGE ( 'NONE', *, *, #11624, .F. ) ;
#13512 = EDGE_LOOP ( 'NONE', ( #52297, #40279, #11223, #59376 ) ) ;
#13513 = CARTESIAN_POINT ( 'NONE',  ( -6.063463321072276813, -8.893131869789778321, 17.08018319649995220 ) ) ;
#13514 = DIRECTION ( 'NONE',  ( -1.000000000000000000, -0.000000000000000000, -0.000000000000000000 ) ) ;
#13515 = ORIENTED_EDGE ( 'NONE', *, *, #45769, .F. ) ;
#13516 = CIRCLE ( 'NONE', #48515, 47.09074272231896430 ) ;
#13517 = B_SPLINE_CURVE_WITH_KNOTS ( 'NONE', 3,
 ( #11001, #53878, #52961, #5632, #29779, #5941, #30083, #48279, #20698, #34809, #49195, #39520, #15393, #24151, #6244, #19471, #9745, #643, #48890 ),
 .UNSPECIFIED., .F., .F.,
 ( 4, 3, 3, 3, 3, 3, 4 ),
 ( 9.813227601316442057E-18, 0.0002612768053151707875, 0.0003919133833142900581, 0.0005225499612322555493, 0.0006531865391693305375, 0.0008112755173415146532, 0.0009693688056799714889 ),
 .UNSPECIFIED. ) ;
#13518 = VERTEX_POINT ( 'NONE', #49209 ) ;
#13519 = CARTESIAN_POINT ( 'NONE',  ( 0.5839879882012672940, 3.018602137292904642E-05, 47.89596766821092189 ) ) ;
#13520 = CARTESIAN_POINT ( 'NONE',  ( 0.7246131072078544344, 48.09507913767660625, 0.8205838906004792044 ) ) ;
#13521 = CARTESIAN_POINT ( 'NONE',  ( 0.5998501479064708430, 47.62484632993678701, 6.798102206414301740 ) ) ;
#13522 = B_SPLINE_CURVE_WITH_KNOTS ( 'NONE', 3,
 ( #27955, #61134, #8518, #42083, #28253, #56748, #13554, #56440, #37367, #47078, #9763, #9449, #51742, #37684, #27641, #56134, #14483, #3818, #22954 ),
 .UNSPECIFIED., .F., .F.,
 ( 4, 3, 3, 3, 3, 3, 4 ),
 ( 6.939740885162003740E-18, 0.0002732106629380601551, 0.0004098138914053745105, 0.0005464171197651472318, 0.0006830203481512577175, 0.0008196235766963646087, 0.001011968216111144847 ),
 .UNSPECIFIED. ) ;
#13523 = ADVANCED_FACE ( 'NONE', ( #7204 ), #1588, .T. ) ;
#13524 = VERTEX_POINT ( 'NONE', #1894 ) ;
#13525 = CARTESIAN_POINT ( 'NONE',  ( 0.9736507210033056303, -16.00326134587889015, -39.81239086052233489 ) ) ;
#13526 = CARTESIAN_POINT ( 'NONE',  ( 0.5782707292762423457, 21.90237606067615772, -41.47315127409947166 ) ) ;
#13527 = CARTESIAN_POINT ( 'NONE',  ( 0.5835226383429292785, -44.36069261528489704, -15.21089823903163030 ) ) ;
#13528 = CARTESIAN_POINT ( 'NONE',  ( 0.5817216825391130497, 17.27888236047640547, 43.59673355402070882 ) ) ;
#13529 = ORIENTED_EDGE ( 'NONE', *, *, #39220, .F. ) ;
#13530 = EDGE_CURVE ( 'NONE', #38058, #47205, #43312, .T. ) ;
#13531 = FACE_OUTER_BOUND ( 'NONE', #55019, .T. ) ;
#13532 = CARTESIAN_POINT ( 'NONE',  ( 4.967162193818130511, 0.000000000000000000, 0.000000000000000000 ) ) ;
#13533 = ORIENTED_EDGE ( 'NONE', *, *, #29555, .T. ) ;
#13534 = CARTESIAN_POINT ( 'NONE',  ( 4.553261556744875094, -33.30082861731464305, -28.64601855797546648 ) ) ;
#13535 = ORIENTED_EDGE ( 'NONE', *, *, #9500, .F. ) ;
#13536 = CARTESIAN_POINT ( 'NONE',  ( 0.9740398440564304039, 26.44872719679369411, 33.78760696452714996 ) ) ;
#13537 = CARTESIAN_POINT ( 'NONE',  ( 0.5837799406558237258, 10.78283246128463091, -45.63961079686228572 ) ) ;
#13538 = ORIENTED_EDGE ( 'NONE', *, *, #12879, .F. ) ;
#13539 = CARTESIAN_POINT ( 'NONE',  ( 0.8551540677456715978, -7.157691013574694061, 47.37911285756618440 ) ) ;
#13540 = CARTESIAN_POINT ( 'NONE',  ( 0.7048096507298579061, 46.68221792389239511, -11.63498350884287724 ) ) ;
#13541 = CARTESIAN_POINT ( 'NONE',  ( 0.6039202388192953519, 48.23508111734878412, 9.216325865103440762 ) ) ;
#13542 = DIRECTION ( 'NONE',  ( -1.000000000000000000, -1.836909530733573776E-16, 2.465190328815682145E-32 ) ) ;
#13543 = EDGE_LOOP ( 'NONE', ( #39491, #31858, #35306, #156 ) ) ;
#13544 = DIRECTION ( 'NONE',  ( 0.000000000000000000, 0.000000000000000000, -1.000000000000000000 ) ) ;
#13545 = CARTESIAN_POINT ( 'NONE',  ( 0.5804410086790514622, 46.89585601637878653, 0.5463884574786440629 ) ) ;
#13546 = CARTESIAN_POINT ( 'NONE',  ( 4.322998006666179727, 43.48102276965701662, -20.30542865297603683 ) ) ;
#13547 = EDGE_CURVE ( 'NONE', #1398, #40637, #26638, .T. ) ;
#13548 = CARTESIAN_POINT ( 'NONE',  ( 0.5839879327111913154, -44.28486549479612933, -18.24507200299090925 ) ) ;
#13549 = CARTESIAN_POINT ( 'NONE',  ( 0.8744876279028263033, 40.65405044375290800, 27.52450240960382644 ) ) ;
#13550 = LINE ( 'NONE', #11782, #15816 ) ;
#13551 = CYLINDRICAL_SURFACE ( 'NONE', #15260, 2.500000000000002220 ) ;
#13552 = CARTESIAN_POINT ( 'NONE',  ( 0.1365634738349449651, -41.13330695003092785, 15.96601637785038541 ) ) ;
#13553 = AXIS2_PLACEMENT_3D ( 'NONE', #49161, #30986, #36021 ) ;
#13554 = CARTESIAN_POINT ( 'NONE',  ( 0.9789889208857702751, -12.32462320582296478, 40.05544358607027533 ) ) ;
#13555 = CARTESIAN_POINT ( 'NONE',  ( 0.1064266418746774162, -22.04679912212855442, 37.06314021531073877 ) ) ;
#13556 = AXIS2_PLACEMENT_3D ( 'NONE', #28939, #43371, #38673 ) ;
#13557 = CARTESIAN_POINT ( 'NONE',  ( 5.895596859100789899, -18.51832497669328959, 7.848555489391991991 ) ) ;
#13558 = B_SPLINE_CURVE_WITH_KNOTS ( 'NONE', 3,
 ( #34581, #19873, #52429, #5420, #48361, #38679 ),
 .UNSPECIFIED., .F., .F.,
 ( 4, 2, 4 ),
 ( 1.271362391926013986E-16, 0.0002450741128632365163, 0.0004901482257263459642 ),
 .UNSPECIFIED. ) ;
#13559 = CARTESIAN_POINT ( 'NONE',  ( 4.549368137175248350, 0.000000000000000000, 0.000000000000000000 ) ) ;
#13560 = CARTESIAN_POINT ( 'NONE',  ( 0.9752570700956810779, 37.04395688491844396, 21.65368877244764789 ) ) ;
#13561 = CARTESIAN_POINT ( 'NONE',  ( 2.359973842542475886, -21.51797753960544313, 38.40719382143839056 ) ) ;
#13562 = CARTESIAN_POINT ( 'NONE',  ( 5.960221823109900008, -14.50993159119800957, -14.51763960716773383 ) ) ;
#13563 = EDGE_CURVE ( 'NONE', #199, #4129, #47730, .T. ) ;
#13564 = CARTESIAN_POINT ( 'NONE',  ( 5.896782393890504181, -4.656380635072850716, 19.56640504178861306 ) ) ;
#13565 = LINE ( 'NONE', #45546, #49439 ) ;
#13567 = ORIENTED_EDGE ( 'NONE', *, *, #25584, .T. ) ;
#13566 = CARTESIAN_POINT ( 'NONE',  ( 0.5980894510889457338, 24.66136644716763371, 41.31170365136896550 ) ) ;
#13568 = ORIENTED_EDGE ( 'NONE', *, *, #5616, .F. ) ;
#13569 = B_SPLINE_CURVE_WITH_KNOTS ( 'NONE', 3,
 ( #36000, #50983, #35689, #60369 ),
 .UNSPECIFIED., .F., .F.,
 ( 4, 4 ),
 ( 0.000000000000000000, 0.004444103432399265294 ),
 .UNSPECIFIED. ) ;
#13570 = CARTESIAN_POINT ( 'NONE',  ( 0.6021448801613057400, -39.51107342597083516, 29.16189663506967378 ) ) ;
#13571 = DIRECTION ( 'NONE',  ( -0.07836865515943411409, 0.1223011693452993043, -0.9893941468723544963 ) ) ;
#13572 = CARTESIAN_POINT ( 'NONE',  ( 0.5850706913938533704, -46.21698775168636075, -12.57184842332066133 ) ) ;
#13573 = ORIENTED_EDGE ( 'NONE', *, *, #9696, .F. ) ;
#13574 = VERTEX_POINT ( 'NONE', #6892 ) ;
#13575 = CARTESIAN_POINT ( 'NONE',  ( 0.3676999524040366896, -31.10876963919527682, 31.27610965031171020 ) ) ;
#13576 = CARTESIAN_POINT ( 'NONE',  ( 1.000110580585053865, -39.37003715540507187, -14.36724250348427212 ) ) ;
#13577 = B_SPLINE_CURVE_WITH_KNOTS ( 'NONE', 3,
 ( #18574, #42397, #33302, #4431 ),
 .UNSPECIFIED., .F., .F.,
 ( 4, 4 ),
 ( 0.000000000000000000, 0.004445488388166994251 ),
 .UNSPECIFIED. ) ;
#13578 = EDGE_CURVE ( 'NONE', #31835, #4479, #9617, .T. ) ;
#13579 = ORIENTED_EDGE ( 'NONE', *, *, #44242, .F. ) ;
#13580 = ORIENTED_EDGE ( 'NONE', *, *, #7461, .F. ) ;
#13581 =( BOUNDED_SURFACE ( )  B_SPLINE_SURFACE ( 3, 1, ( 
 ( #9086, #4663 ),
 ( #37944, #56686 ),
 ( #41709, #36698 ),
 ( #60771, #23812 ) ),
 .UNSPECIFIED., .F., .F., .F. ) 
 B_SPLINE_SURFACE_WITH_KNOTS ( ( 4, 4 ),
 ( 2, 2 ),
 ( 0.000000000000000000, 1.000000000000000000 ),
 ( 0.000000000000000000, 1.000000000000000000 ),
 .UNSPECIFIED. ) 
 GEOMETRIC_REPRESENTATION_ITEM ( )  RATIONAL_B_SPLINE_SURFACE ( (
 ( 1.000000000000000000, 1.000000000000000000),
 ( 0.9732289882329797637, 0.9999525324661233672),
 ( 0.9732289882329797637, 0.9999525324661233672),
 ( 1.000000000000000000, 1.000000000000000000) ) ) 
 REPRESENTATION_ITEM ( '' )  SURFACE ( )  );
#13582 = CARTESIAN_POINT ( 'NONE',  ( 0.6030672727741701600, -38.11303703924448172, -29.35514790473137481 ) ) ;
#13583 = EDGE_CURVE ( 'NONE', #19448, #56393, #6581, .T. ) ;
#13584 = DIRECTION ( 'NONE',  ( 1.000000000000000000, 0.000000000000000000, 0.000000000000000000 ) ) ;
#13585 = FACE_OUTER_BOUND ( 'NONE', #56180, .T. ) ;
#13586 = ORIENTED_EDGE ( 'NONE', *, *, #29836, .T. ) ;
#13587 = ORIENTED_EDGE ( 'NONE', *, *, #42616, .F. ) ;
#13588 = CARTESIAN_POINT ( 'NONE',  ( -6.079354080745853928, -17.34954932540448524, 8.353807123313236715 ) ) ;
#13589 = ORIENTED_EDGE ( 'NONE', *, *, #29204, .T. ) ;
#13590 = CARTESIAN_POINT ( 'NONE',  ( 0.8753041380234465318, 33.66554281472474486, -35.74590263041227445 ) ) ;
#13591 = DIRECTION ( 'NONE',  ( 0.1011922191286468015, -0.9172554449906691332, 0.3852305587862797642 ) ) ;
#13592 = CARTESIAN_POINT ( 'NONE',  ( 0.1103744047535531458, -30.46616790811201625, -30.52096488484616899 ) ) ;
#13593 = ORIENTED_EDGE ( 'NONE', *, *, #59184, .T. ) ;
#13594 = B_SPLINE_CURVE_WITH_KNOTS ( 'NONE', 3,
 ( #57374, #33927, #9479, #15428, #25123, #24503 ),
 .UNSPECIFIED., .F., .F.,
 ( 4, 2, 4 ),
 ( 9.929776742050823831E-18, 0.0002448709889506589456, 0.0004897419779013080249 ),
 .UNSPECIFIED. ) ;
#13595 = FACE_OUTER_BOUND ( 'NONE', #23572, .T. ) ;
#13596 = ORIENTED_EDGE ( 'NONE', *, *, #33958, .F. ) ;
#13597 = EDGE_CURVE ( 'NONE', #30061, #34292, #14129, .T. ) ;
#13598 = EDGE_LOOP ( 'NONE', ( #33540, #9864, #50110, #6562 ) ) ;
#13599 = CARTESIAN_POINT ( 'NONE',  ( 0.5807400328401574052, -44.04145271122577299, 18.83234461715166930 ) ) ;
#13600 = AXIS2_PLACEMENT_3D ( 'NONE', #1686, #20824, #39962 ) ;
#13601 = ORIENTED_EDGE ( 'NONE', *, *, #32477, .F. ) ;
#13602 = CARTESIAN_POINT ( 'NONE',  ( 0.5797568599927133137, -8.419849506244490911, 46.13384270753087435 ) ) ;
#13603 = CARTESIAN_POINT ( 'NONE',  ( 4.956653778116973719, 31.29546495791849736, 36.51451553856430365 ) ) ;
#13604 = CARTESIAN_POINT ( 'NONE',  ( 0.8751705887134553219, -24.81530984069179269, -41.19904111682499348 ) ) ;
#13605 = CARTESIAN_POINT ( 'NONE',  ( 0.5837800304671219020, -38.68876759456514236, 26.50314310026687181 ) ) ;
#13606 = EDGE_CURVE ( 'NONE', #47052, #41414, #10618, .T. ) ;
#13607 = VECTOR ( 'NONE', #34577, 999.9999999999998863 ) ;
#13608 = ORIENTED_EDGE ( 'NONE', *, *, #53091, .T. ) ;
#13609 = DIRECTION ( 'NONE',  ( -1.000000000000000000, -0.000000000000000000, -0.000000000000000000 ) ) ;
#13610 = EDGE_CURVE ( 'NONE', #44371, #55732, #28304, .T. ) ;
#13611 = CARTESIAN_POINT ( 'NONE',  ( 0.9749527285493295725, -21.20640438431165364, -37.30179927241198357 ) ) ;
#13612 = ORIENTED_EDGE ( 'NONE', *, *, #46563, .T. ) ;
#13613 = CARTESIAN_POINT ( 'NONE',  ( 2.301430502907645170, -48.01619648598872203, -1.287492012859226875 ) ) ;
#13614 = CARTESIAN_POINT ( 'NONE',  ( 0.9722240741986377666, -26.58024228478319628, 33.68410525900274166 ) ) ;
#13615 = CARTESIAN_POINT ( 'NONE',  ( 3.270143674763207553, -13.53222904135355620, 2.058141141425546827 ) ) ;
#13616 = CARTESIAN_POINT ( 'NONE',  ( -6.077587904424778920, 13.83688374988418879, 13.39166417911236984 ) ) ;
#13617 = AXIS2_PLACEMENT_3D ( 'NONE', #19119, #39156, #54947 ) ;
#13618 = EDGE_LOOP ( 'NONE', ( #17157, #55219, #41197, #16753 ) ) ;
#13619 = EDGE_LOOP ( 'NONE', ( #47269, #10872, #46471, #53095 ) ) ;
#13620 = CARTESIAN_POINT ( 'NONE',  ( 4.956653778117001252, 47.94889704119056972, -3.690426056929486887 ) ) ;
#13621 = LINE ( 'NONE', #13016, #23689 ) ;
#13622 = CARTESIAN_POINT ( 'NONE',  ( 5.895596859100789899, -9.669028665050088733, -17.63627137143583568 ) ) ;
#13623 = EDGE_CURVE ( 'NONE', #53003, #51245, #49271, .T. ) ;
#13624 = CARTESIAN_POINT ( 'NONE',  ( 4.834790513006555379, -36.27562111512906284, -30.27653635467542870 ) ) ;
#13625 = CARTESIAN_POINT ( 'NONE',  ( 0.5837157313716013762, -30.20780093847265846, -35.87096076276234413 ) ) ;
#13626 = CARTESIAN_POINT ( 'NONE',  ( 0.1154773475650540671, -18.02505553582892972, -40.27457017742589329 ) ) ;
#13627 = CARTESIAN_POINT ( 'NONE',  ( 4.960156602257182357, 8.553784487772873035, 45.62767441207052599 ) ) ;
#13628 = CARTESIAN_POINT ( 'NONE',  ( 0.9757892942422816684, 42.90845395884348079, -0.05132855327749175772 ) ) ;
#13629 = DIRECTION ( 'NONE',  ( 0.000000000000000000, 0.000000000000000000, 1.000000000000000000 ) ) ;
#13630 = CARTESIAN_POINT ( 'NONE',  ( 4.956653778116975495, -9.917440902361487787, 47.05699031914946318 ) ) ;
#13631 = CARTESIAN_POINT ( 'NONE',  ( 0.8760168074887090262, -5.394043284319860021, 47.80016357497240165 ) ) ;
#13632 = CARTESIAN_POINT ( 'NONE',  ( 5.896278296736517710, -4.667894692253747202, -19.56368418157513034 ) ) ;
#13633 = ORIENTED_EDGE ( 'NONE', *, *, #13250, .F. ) ;
#13634 = B_SPLINE_CURVE_WITH_KNOTS ( 'NONE', 3,
 ( #27412, #52140, #23647, #42775, #61829, #56223, #56528, #43084, #38087, #8293, #13336, #9537, #3587, #51826, #56834, #17719 ),
 .UNSPECIFIED., .F., .F.,
 ( 4, 3, 3, 3, 3, 4 ),
 ( 1.214354834101861570E-17, 0.0002724568934985521318, 0.0004086836638483778159, 0.0005449104342063536104, 0.0008173270854453650470, 0.001089761613562688792 ),
 .UNSPECIFIED. ) ;
#13635 = CARTESIAN_POINT ( 'NONE',  ( 0.6846871229502899947, 23.20185915381614805, -41.91507847151773802 ) ) ;
#13636 = CARTESIAN_POINT ( 'NONE',  ( -6.001507490154111224, -18.68062548815624169, -2.475062734132633224 ) ) ;
#13637 = CARTESIAN_POINT ( 'NONE',  ( 0.1129192098497447394, -35.64954734424924965, -26.00118385641864194 ) ) ;
#13638 = CARTESIAN_POINT ( 'NONE',  ( 0.5837799406558230597, -34.84162086156078431, -31.38956841558125532 ) ) ;
#13639 = CARTESIAN_POINT ( 'NONE',  ( 0.08486401232817714080, 12.80000000000000071, 3.000000000000000000 ) ) ;
#13641 = B_SPLINE_CURVE_WITH_KNOTS ( 'NONE', 3,
 ( #51899, #27479, #41300, #46007, #23402, #55663 ),
 .UNSPECIFIED., .F., .F.,
 ( 4, 2, 4 ),
 ( 1.184703104989684002E-16, 0.0002448718616795916327, 0.0004897437233590648704 ),
 .UNSPECIFIED. ) ;
#13640 = FACE_OUTER_BOUND ( 'NONE', #5516, .T. ) ;
#13642 = CONTEXT_DEPENDENT_SHAPE_REPRESENTATION ( #37677, #10878 ) ;
#13643 = DIRECTION ( 'NONE',  ( 0.9990097760809872884, 5.448601141172755645E-18, 0.04449120468829285274 ) ) ;
#13644 = FACE_OUTER_BOUND ( 'NONE', #54767, .T. ) ;
#13645 = CARTESIAN_POINT ( 'NONE',  ( 2.528100132419515589, -41.94888324960150072, -1.595297070572732956 ) ) ;
#13646 = B_SPLINE_CURVE_WITH_KNOTS ( 'NONE', 3,
 ( #32101, #51182, #27385, #42143, #60890, #12382 ),
 .UNSPECIFIED., .F., .F.,
 ( 4, 2, 4 ),
 ( 2.197222038435329413E-17, 0.0002293755540694313185, 0.0004587511081388406277 ),
 .UNSPECIFIED. ) ;
#13648 = VERTEX_POINT ( 'NONE', #27879 ) ;
#13647 = CARTESIAN_POINT ( 'NONE',  ( 0.6017667736363749853, -46.37677940471289162, -12.78803812527872097 ) ) ;
#13649 = EDGE_LOOP ( 'NONE', ( #19310, #6375, #49697, #52186 ) ) ;
#13650 = CIRCLE ( 'NONE', #596, 48.09070567114147110 ) ;
#13651 = CARTESIAN_POINT ( 'NONE',  ( 0.1152809850208375148, -7.260492202596367406, 43.52275882186000189 ) ) ;
#13652 = CARTESIAN_POINT ( 'NONE',  ( 4.956653778116970166, 43.37017594958054900, 20.77844580450576117 ) ) ;
#13653 = VECTOR ( 'NONE', #57247, 1000.000000000000000 ) ;
#13654 = DIRECTION ( 'NONE',  ( 0.000000000000000000, 0.000000000000000000, -1.000000000000000000 ) ) ;
#13655 = EDGE_CURVE ( 'NONE', #2006, #41630, #7835, .T. ) ;
#13656 = VERTEX_POINT ( 'NONE', #56061 ) ;
#13657 = DIRECTION ( 'NONE',  ( 0.000000000000000000, 0.000000000000000000, 1.000000000000000000 ) ) ;
#13658 = CARTESIAN_POINT ( 'NONE',  ( 0.5980271706414734822, -8.528665270201470250, -48.36642545765111123 ) ) ;
#13659 = CARTESIAN_POINT ( 'NONE',  ( 0.6031356219577718170, -44.47888959008686527, -18.32926896140815387 ) ) ;
#13660 = EDGE_CURVE ( 'NONE', #19096, #29761, #43629, .T. ) ;
#13661 =( BOUNDED_SURFACE ( )  B_SPLINE_SURFACE ( 3, 1, ( 
 ( #26881, #46313 ),
 ( #55672, #27189 ),
 ( #46019, #13108 ),
 ( #45697, #59769 ) ),
 .UNSPECIFIED., .F., .F., .F. ) 
 B_SPLINE_SURFACE_WITH_KNOTS ( ( 4, 4 ),
 ( 2, 2 ),
 ( 0.000000000000000000, 1.000000000000000000 ),
 ( 0.000000000000000000, 1.000000000000000000 ),
 .UNSPECIFIED. ) 
 GEOMETRIC_REPRESENTATION_ITEM ( )  RATIONAL_B_SPLINE_SURFACE ( (
 ( 1.000000000000000000, 1.000000000000000000),
 ( 0.9754377213608244057, 0.9999580625633939235),
 ( 0.9754377213608244057, 0.9999580625633939235),
 ( 1.000000000000000000, 1.000000000000000000) ) ) 
 REPRESENTATION_ITEM ( '' )  SURFACE ( )  );
#13662 = EDGE_LOOP ( 'NONE', ( #43997, #4639, #43630, #51651 ) ) ;
#13663 = EDGE_LOOP ( 'NONE', ( #48253, #13133 ) ) ;
#13664 = CARTESIAN_POINT ( 'NONE',  ( 0.9740398440564311811, 41.55177796653848077, 10.70454588197301149 ) ) ;
#13665 = EDGE_CURVE ( 'NONE', #4970, #40810, #18482, .T. ) ;
#13666 = AXIS2_PLACEMENT_3D ( 'NONE', #33218, #9082, #9384 ) ;
#13667 = CARTESIAN_POINT ( 'NONE',  ( 1.657374760986086271, -40.35518271633839049, 17.67341719032251390 ) ) ;
#13668 = CYLINDRICAL_SURFACE ( 'NONE', #53195, 2.649999999999992806 ) ;
#13669 = CARTESIAN_POINT ( 'NONE',  ( 0.6030672727741701600, 41.61859040196950588, 24.12926094634001117 ) ) ;
#13670 = CARTESIAN_POINT ( 'NONE',  ( 1.199999999999992628, 0.000000000000000000, -6.887500000000022382 ) ) ;
#13671 = CARTESIAN_POINT ( 'NONE',  ( 0.6028777368367060907, 49.00087957688494811, 3.233207386279532969 ) ) ;
#13672 = ORIENTED_EDGE ( 'NONE', *, *, #57741, .F. ) ;
#13673 = ADVANCED_FACE ( 'NONE', ( #51982 ), #46407, .F. ) ;
#13674 = CARTESIAN_POINT ( 'NONE',  ( 2.301529144917015213, 22.89307126379987167, -42.22700141647020189 ) ) ;
#13675 = PRESENTATION_STYLE_ASSIGNMENT (( #7709 ) ) ;
#13676 = ORIENTED_EDGE ( 'NONE', *, *, #1401, .F. ) ;
#13677 = CARTESIAN_POINT ( 'NONE',  ( 0.9790724872846782167, -37.38600932109895325, -18.93730490392327681 ) ) ;
#13678 = ADVANCED_FACE ( 'NONE', ( #51358 ), #53149, .F. ) ;
#13679 = CARTESIAN_POINT ( 'NONE',  ( 4.956445790444004906, -37.28933980949924631, -28.75835855384189443 ) ) ;
#13680 = CARTESIAN_POINT ( 'NONE',  ( 3.559346040607745287, 38.68187159388032370, -20.90796717848347441 ) ) ;
#13681 = CARTESIAN_POINT ( 'NONE',  ( 4.975801465491695552, 47.10002938642130488, 8.787181743660319455 ) ) ;
#13682 = VERTEX_POINT ( 'NONE', #9073 ) ;
#13683 = ORIENTED_EDGE ( 'NONE', *, *, #26361, .T. ) ;
#13684 = CARTESIAN_POINT ( 'NONE',  ( 0.9762797500689124330, 33.20096159360354449, -25.57383300261748360 ) ) ;
#13685 = CARTESIAN_POINT ( 'NONE',  ( -6.078075953587585900, -14.65899360350508296, 12.48635578459675699 ) ) ;
#13686 = EDGE_CURVE ( 'NONE', #4961, #37380, #1437, .T. ) ;
#13687 = LINE ( 'NONE', #51871, #27184 ) ;
#13688 = VERTEX_POINT ( 'NONE', #36999 ) ;
#13689 = CARTESIAN_POINT ( 'NONE',  ( 0.5809828226811553087, 47.41188724015889022, -6.791453954329836229 ) ) ;
#13690 = CIRCLE ( 'NONE', #49659, 10.00000000000000711 ) ;
#13691 = ORIENTED_EDGE ( 'NONE', *, *, #55583, .T. ) ;
#13692 = CARTESIAN_POINT ( 'NONE',  ( -6.016761891674565099, -0.003433883959915969616, 18.84319130225482297 ) ) ;
#13693 = CARTESIAN_POINT ( 'NONE',  ( 0.5835226383429280572, 27.96423497704858363, 37.64630176649998816 ) ) ;
#13694 = PRESENTATION_LAYER_ASSIGNMENT (  '', '', ( #49663 ) ) ;
#13695 = CARTESIAN_POINT ( 'NONE',  ( 4.956445790443988031, 46.25174887658550915, 8.849507104743643993 ) ) ;
#13696 = VERTEX_POINT ( 'NONE', #23181 ) ;
#13697 = CARTESIAN_POINT ( 'NONE',  ( 4.956445790443991584, 38.51510088324707226, 27.09474218539341450 ) ) ;
#13698 = AXIS2_PLACEMENT_3D ( 'NONE', #43491, #29060, #38179 ) ;
#13699 = CARTESIAN_POINT ( 'NONE',  ( 4.553261556744873317, 31.39705178283683296, -30.72075365562339755 ) ) ;
#13700 = CARTESIAN_POINT ( 'NONE',  ( 0.5830082357119558134, -41.97803085087377895, 20.90638564700811841 ) ) ;
#13701 = EDGE_CURVE ( 'NONE', #44114, #19627, #20112, .T. ) ;
#13702 = ORIENTED_EDGE ( 'NONE', *, *, #6262, .T. ) ;
#13703 = DIRECTION ( 'NONE',  ( -0.1024043820194934229, -0.3927886084231700936, 0.9139094329506590730 ) ) ;
#13704 = CARTESIAN_POINT ( 'NONE',  ( 0.1147471544378677183, 33.39615026987465995, -28.83833101317058123 ) ) ;
#13705 = CARTESIAN_POINT ( 'NONE',  ( 4.962356264823602814, -36.43094049105359744, -21.07183363638911189 ) ) ;
#13706 = CARTESIAN_POINT ( 'NONE',  ( 0.1101816497532063233, 26.14462713083295498, -34.29544870207487151 ) ) ;
#13707 = CARTESIAN_POINT ( 'NONE',  ( 2.643462169533613793, 7.637863311826968093, 47.42536612906431515 ) ) ;
#13708 = VERTEX_POINT ( 'NONE', #42611 ) ;
#13709 = VECTOR ( 'NONE', #36395, 1000.000000000000114 ) ;
#13710 = FACE_OUTER_BOUND ( 'NONE', #11258, .T. ) ;
#13711 = CARTESIAN_POINT ( 'NONE',  ( 4.956653778116987930, -47.05699031914942054, -9.917440902361647659 ) ) ;
#13712 = ORIENTED_EDGE ( 'NONE', *, *, #55036, .F. ) ;
#13713 = CARTESIAN_POINT ( 'NONE',  ( 4.956445790444001354, -28.36659270909979114, 37.58822246682706947 ) ) ;
#13714 = CARTESIAN_POINT ( 'NONE',  ( 0.9784957157296376717, -26.87920163080859837, 32.15340692185988303 ) ) ;
#13715 = CARTESIAN_POINT ( 'NONE',  ( 0.1119898979215351309, -35.02332270898327948, 26.83893020733585644 ) ) ;
#13716 = CARTESIAN_POINT ( 'NONE',  ( 0.2224561200757616264, -11.89200283918819423, 41.44719785461210648 ) ) ;
#13717 = CARTESIAN_POINT ( 'NONE',  ( 1.157643937452368599, -6.156433921344971694, 41.46203801029162861 ) ) ;
#13718 = CARTESIAN_POINT ( 'NONE',  ( -31.75000000000000000, 0.000000000000000000, 0.000000000000000000 ) ) ;
#13719 = CARTESIAN_POINT ( 'NONE',  ( 4.000000000000003553, 2.309401076758480720, -5.599999999999999645 ) ) ;
#13720 = DIRECTION ( 'NONE',  ( 2.736790032596824432E-18, 0.9852296403989260209, -0.1712383008541119855 ) ) ;
#13721 = CARTESIAN_POINT ( 'NONE',  ( 0.6023142530420679819, 47.72938419887611161, 6.019593586345465930 ) ) ;
#13722 = B_SPLINE_CURVE_WITH_KNOTS ( 'NONE', 3,
 ( #18479, #15027, #57275, #18799 ),
 .UNSPECIFIED., .F., .F.,
 ( 4, 4 ),
 ( 4.670885906470169154E-18, 0.004566006591234648103 ),
 .UNSPECIFIED. ) ;
#13723 = CARTESIAN_POINT ( 'NONE',  ( -6.078075953587585900, 12.01009662667731170, -15.05166945109445820 ) ) ;
#13724 = CARTESIAN_POINT ( 'NONE',  ( -6.079354080745853928, 13.83333621897982368, 13.39521423124031330 ) ) ;
#13725 = CARTESIAN_POINT ( 'NONE',  ( 0.5837157313716039297, 32.53625919676243683, 33.77319796914579797 ) ) ;
#13726 = CARTESIAN_POINT ( 'NONE',  ( 0.1064266418746777354, 22.04679912212828796, -37.06314021531088088 ) ) ;
#13727 = ORIENTED_EDGE ( 'NONE', *, *, #6143, .F. ) ;
#13728 = DIRECTION ( 'NONE',  ( 0.1011922191286468153, -0.3909116750758017123, 0.9148487290679540029 ) ) ;
#13729 = CARTESIAN_POINT ( 'NONE',  ( 5.959828726073459926, -20.52560994243598813, -0.004526594003305732528 ) ) ;
#13730 = ADVANCED_FACE ( 'NONE', ( #51669 ), #1547, .F. ) ;
#13731 = CARTESIAN_POINT ( 'NONE',  ( 42.00000000000002132, -72.00000000000001421, 8.817456953860944867E-15 ) ) ;
#13732 = DIRECTION ( 'NONE',  ( -1.000000000000000000, -0.000000000000000000, -0.000000000000000000 ) ) ;
#13733 = DIRECTION ( 'NONE',  ( 0.000000000000000000, 0.000000000000000000, -1.000000000000000000 ) ) ;
#13734 = EDGE_CURVE ( 'NONE', #28932, #56419, #24602, .T. ) ;
#13735 = EDGE_LOOP ( 'NONE', ( #47330, #57531, #30351, #37655 ) ) ;
#13736 = VECTOR ( 'NONE', #45730, 1000.000000000000114 ) ;
#13737 = CARTESIAN_POINT ( 'NONE',  ( 0.9730545539215883499, 11.59290486963565137, -41.31259007387218674 ) ) ;
#13738 = EDGE_CURVE ( 'NONE', #34780, #16119, #8764, .T. ) ;
#13739 =( BOUNDED_SURFACE ( )  B_SPLINE_SURFACE ( 3, 1, ( 
 ( #45712, #44488 ),
 ( #11573, #11254 ),
 ( #1517, #27819 ),
 ( #12818, #13423 ) ),
 .UNSPECIFIED., .F., .F., .F. ) 
 B_SPLINE_SURFACE_WITH_KNOTS ( ( 4, 4 ),
 ( 2, 2 ),
 ( 0.000000000000000000, 1.000000000000000000 ),
 ( 0.000000000000000000, 1.000000000000000000 ),
 .UNSPECIFIED. ) 
 GEOMETRIC_REPRESENTATION_ITEM ( )  RATIONAL_B_SPLINE_SURFACE ( (
 ( 1.000000000000000000, 1.000000000000000000),
 ( 0.7211978278499970862, 0.9934217856018976445),
 ( 0.7211978278499970862, 0.9934217856018976445),
 ( 1.000000000000000000, 1.000000000000000000) ) ) 
 REPRESENTATION_ITEM ( '' )  SURFACE ( )  );
#13740 = ADVANCED_FACE ( 'NONE', ( #48227 ), #31952, .F. ) ;
#13741 = CARTESIAN_POINT ( 'NONE',  ( 4.956653778116966613, 0.000000000000000000, 0.000000000000000000 ) ) ;
#13742 = CARTESIAN_POINT ( 'NONE',  ( -20.00591024382368488, -7.982430833260542258, -0.5467354857925370570 ) ) ;
#13743 = B_SPLINE_CURVE_WITH_KNOTS ( 'NONE', 3,
 ( #61103, #36414, #22607, #51089 ),
 .UNSPECIFIED., .F., .F.,
 ( 4, 4 ),
 ( 4.336808689942017736E-19, 0.004041751736740985604 ),
 .UNSPECIFIED. ) ;
#13744 = VECTOR ( 'NONE', #14448, 1000.000000000000000 ) ;
#13745 = EDGE_CURVE ( 'NONE', #10258, #54854, #26875, .T. ) ;
#13746 = VERTEX_POINT ( 'NONE', #53213 ) ;
#13747 = CARTESIAN_POINT ( 'NONE',  ( 0.6254087463353924514, -46.28445368454761422, 13.11428234126282888 ) ) ;
#13748 = DIRECTION ( 'NONE',  ( 0.000000000000000000, 1.224646799147353947E-16, 1.000000000000000000 ) ) ;
#13749 = ORIENTED_EDGE ( 'NONE', *, *, #53854, .F. ) ;
#13750 = ADVANCED_FACE ( 'NONE', ( #38533 ), #42635, .T. ) ;
#13751 = B_SPLINE_CURVE_WITH_KNOTS ( 'NONE', 3,
 ( #11817, #11189, #44421, #40032, #59083, #20585, #60014, #2377, #2689, #17126, #54685, #55306, #50611, #12425, #35311, #36239, #30898, #31518, #54372 ),
 .UNSPECIFIED., .F., .F.,
 ( 4, 3, 3, 3, 3, 3, 4 ),
 ( 1.121058697680834634E-16, 0.0002618519381806306873, 0.0003927759815485986315, 0.0005237000248299465742, 0.0006546240681325006441, 0.0007855481115631358533, 0.0009699050456655141945 ),
 .UNSPECIFIED. ) ;
#13752 = CARTESIAN_POINT ( 'NONE',  ( 2.706805983486680667, -26.12526257152286391, 35.41534651657021016 ) ) ;
#13753 = ORIENTED_EDGE ( 'NONE', *, *, #15780, .T. ) ;
#13754 = CIRCLE ( 'NONE', #10743, 41.88877248453276536 ) ;
#13755 =( BOUNDED_SURFACE ( )  B_SPLINE_SURFACE ( 3, 1, ( 
 ( #12442, #45352 ),
 ( #3016, #40972 ),
 ( #50326, #60036 ),
 ( #6771, #40658 ) ),
 .UNSPECIFIED., .F., .F., .F. ) 
 B_SPLINE_SURFACE_WITH_KNOTS ( ( 4, 4 ),
 ( 2, 2 ),
 ( 0.000000000000000000, 1.000000000000000000 ),
 ( 0.000000000000000000, 1.000000000000000000 ),
 .UNSPECIFIED. ) 
 GEOMETRIC_REPRESENTATION_ITEM ( )  RATIONAL_B_SPLINE_SURFACE ( (
 ( 1.000000000000000000, 1.000000000000000000),
 ( 0.7223157951917476005, 0.9931996967497186413),
 ( 0.7223157951917476005, 0.9931996967497186413),
 ( 1.000000000000000000, 1.000000000000000000) ) ) 
 REPRESENTATION_ITEM ( '' )  SURFACE ( )  );
#13756 = CARTESIAN_POINT ( 'NONE',  ( 0.6067099128993245216, -29.71710940500705433, -37.56352526808334602 ) ) ;
#13757 = CARTESIAN_POINT ( 'NONE',  ( 2.281448460670572054, -44.80776276180760220, -17.13756432392885287 ) ) ;
#13758 = B_SPLINE_CURVE_WITH_KNOTS ( 'NONE', 3,
 ( #51814, #8915, #14559, #28027, #42757, #23027 ),
 .UNSPECIFIED., .F., .F.,
 ( 4, 2, 4 ),
 ( 1.823789517034659149E-17, 0.0002293319059085091138, 0.0004586638118169999588 ),
 .UNSPECIFIED. ) ;
#13759 = ORIENTED_EDGE ( 'NONE', *, *, #27870, .T. ) ;
#13760 = DIRECTION ( 'NONE',  ( -1.000000000000000000, -5.380183451256491399E-17, -1.298891185607892835E-16 ) ) ;
#13761 = CARTESIAN_POINT ( 'NONE',  ( 0.5837374860065633886, -29.01294733976387263, 38.10878877974134582 ) ) ;
#13762 = CARTESIAN_POINT ( 'NONE',  ( 0.5834584762367742705, -7.620554889515525510, -46.27270396453046430 ) ) ;
#13763 = CARTESIAN_POINT ( 'NONE',  ( 0.5819845901640493535, -38.27312528999452468, 28.79568196372255429 ) ) ;
#13764 =( BOUNDED_SURFACE ( )  B_SPLINE_SURFACE ( 3, 1, ( 
 ( #4925, #61932 ),
 ( #19994, #19364 ),
 ( #20291, #38483 ),
 ( #29982, #59092 ) ),
 .UNSPECIFIED., .F., .F., .F. ) 
 B_SPLINE_SURFACE_WITH_KNOTS ( ( 4, 4 ),
 ( 2, 2 ),
 ( 0.000000000000000000, 1.000000000000000000 ),
 ( 0.000000000000000000, 1.000000000000000000 ),
 .UNSPECIFIED. ) 
 GEOMETRIC_REPRESENTATION_ITEM ( )  RATIONAL_B_SPLINE_SURFACE ( (
 ( 1.000000000000000000, 1.000000000000000000),
 ( 0.9953485035131437453, 0.8621029689291515030),
 ( 0.9953485035131437453, 0.8621029689291515030),
 ( 1.000000000000000000, 1.000000000000000000) ) ) 
 REPRESENTATION_ITEM ( '' )  SURFACE ( )  );
#13765 = VERTEX_POINT ( 'NONE', #57902 ) ;
#13766 = CARTESIAN_POINT ( 'NONE',  ( 5.838029081930955932, -37.08173278831655750, 29.25765116288059176 ) ) ;
#13767 = VERTEX_POINT ( 'NONE', #24103 ) ;
#13768 = CARTESIAN_POINT ( 'NONE',  ( 0.9730545539215883499, -39.44597740938048958, -16.88610103448599986 ) ) ;
#13769 = ORIENTED_EDGE ( 'NONE', *, *, #27670, .F. ) ;
#13770 = AXIS2_PLACEMENT_3D ( 'NONE', #33066, #28340, #47456 ) ;
#13771 = ORIENTED_EDGE ( 'NONE', *, *, #52900, .F. ) ;
#13772 = CARTESIAN_POINT ( 'NONE',  ( 0.6001305935487422083, -33.64689939321919354, -34.38748867424700961 ) ) ;
#13773 = DIRECTION ( 'NONE',  ( 0.1011922191286468292, -0.7895409829358921439, 0.6052975888374620972 ) ) ;
#13774 = CARTESIAN_POINT ( 'NONE',  ( 0.7762783648524366198, 46.49451980369979509, 11.53708172997836456 ) ) ;
#13775 = CARTESIAN_POINT ( 'NONE',  ( 5.959547316686252039, 2.682663672454640658, 20.34955788964377632 ) ) ;
#13776 = VERTEX_POINT ( 'NONE', #28481 ) ;
#13777 = CARTESIAN_POINT ( 'NONE',  ( -6.001507490154111224, 11.45906331631431030, 14.95933060264877845 ) ) ;
#13778 = CARTESIAN_POINT ( 'NONE',  ( -99.49999999999975842, -5.000000000000009770, 6.123233995736898417E-16 ) ) ;
#13779 = CARTESIAN_POINT ( 'NONE',  ( 4.390527457369401532, 1.087462747309237310, 43.92041394843443669 ) ) ;
#13781 = EDGE_LOOP ( 'NONE', ( #16840, #4266, #60012, #43779 ) ) ;
#13780 = EDGE_CURVE ( 'NONE', #2209, #61591, #17899, .T. ) ;
#13782 = ORIENTED_EDGE ( 'NONE', *, *, #26289, .T. ) ;
#13783 =( NAMED_UNIT ( * ) SI_UNIT ( $, .STERADIAN. ) SOLID_ANGLE_UNIT ( ) );
#13784 = EDGE_CURVE ( 'NONE', #51079, #55702, #60465, .T. ) ;
#13785 = CARTESIAN_POINT ( 'NONE',  ( 0.9754292580325131246, 40.26172079307664831, 11.63276861647064742 ) ) ;
#13786 = CARTESIAN_POINT ( 'NONE',  ( 0.1092565886968784178, -34.02318727879980997, 26.49813811968527588 ) ) ;
#13787 = CARTESIAN_POINT ( 'NONE',  ( 0.9762797500689124330, 10.20671408565980975, 40.64662068068264489 ) ) ;
#13788 = CIRCLE ( 'NONE', #48771, 2.649999999999985700 ) ;
#13789 = ORIENTED_EDGE ( 'NONE', *, *, #18197, .T. ) ;
#13790 = CIRCLE ( 'NONE', #4694, 43.08621763946400307 ) ;
#13791 = AXIS2_PLACEMENT_3D ( 'NONE', #44077, #48734, #6398 ) ;
#13792 = CARTESIAN_POINT ( 'NONE',  ( 4.549368137175248350, 0.000000000000000000, 0.000000000000000000 ) ) ;
#13793 = CARTESIAN_POINT ( 'NONE',  ( 49.17116576101606995, 15.32881676279135874, 2.299327193150783266 ) ) ;
#13794 = CARTESIAN_POINT ( 'NONE',  ( 0.5549461598389363592, -38.85229981621156270, -20.87382318738021425 ) ) ;
#13795 = CARTESIAN_POINT ( 'NONE',  ( 5.959547316686252039, -2.682663672455063431, 20.34955788964371948 ) ) ;
#13796 = LINE ( 'NONE', #37924, #39890 ) ;
#13797 = B_SPLINE_CURVE_WITH_KNOTS ( 'NONE', 3,
 ( #55864, #60554, #17989, #51161 ),
 .UNSPECIFIED., .F., .F.,
 ( 4, 4 ),
 ( 0.000000000000000000, 0.004444103432399267896 ),
 .UNSPECIFIED. ) ;
#13798 = VERTEX_POINT ( 'NONE', #33519 ) ;
#13799 = FACE_OUTER_BOUND ( 'NONE', #51577, .T. ) ;
#13800 = CARTESIAN_POINT ( 'NONE',  ( 0.7764139734771248191, 28.53559780214793662, -37.22579923898098286 ) ) ;
#13801 = CARTESIAN_POINT ( 'NONE',  ( 5.896782393890504181, 3.351618377817360273, -19.83160964539916549 ) ) ;
#13802 = CARTESIAN_POINT ( 'NONE',  ( 0.5807400328401574052, -41.75144119563902478, 23.47602859900699812 ) ) ;
#13803 = CARTESIAN_POINT ( 'NONE',  ( 0.9775691876210981235, 28.86184834324568627, 30.38630315127980808 ) ) ;
#13804 = CARTESIAN_POINT ( 'NONE',  ( 2.301529144917013436, -34.86298839095307756, -33.04216096093391997 ) ) ;
#13805 = CARTESIAN_POINT ( 'NONE',  ( 0.8760168074886960365, 17.58183840866336212, 44.77533136581888584 ) ) ;
#13806 = AXIS2_PLACEMENT_3D ( 'NONE', #4802, #18634, #18020 ) ;
#13807 = CARTESIAN_POINT ( 'NONE',  ( 0.5817216825391133828, 22.13701364508538916, -41.34232188792448426 ) ) ;
#13808 = ADVANCED_FACE ( 'NONE', ( #42927 ), #52283, .T. ) ;
#13809 = B_SPLINE_CURVE_WITH_KNOTS ( 'NONE', 3,
 ( #27781, #46915, #50648, #7733 ),
 .UNSPECIFIED., .F., .F.,
 ( 4, 4 ),
 ( 0.000000000000000000, 0.004444103432399267029 ),
 .UNSPECIFIED. ) ;
#13810 = EDGE_CURVE ( 'NONE', #7010, #37701, #58915, .T. ) ;
#13811 = AXIS2_PLACEMENT_3D ( 'NONE', #13974, #23353, #42477 ) ;
#13812 = CARTESIAN_POINT ( 'NONE',  ( 4.975801465491694664, -46.87746200127448049, -9.906103548668065528 ) ) ;
#13813 = VERTEX_POINT ( 'NONE', #48520 ) ;
#13814 = EDGE_CURVE ( 'NONE', #53679, #49781, #23107, .T. ) ;
#13815 = CARTESIAN_POINT ( 'NONE',  ( 0.9787464366903561030, 19.98509552998146788, 36.83653009646780419 ) ) ;
#13816 = CARTESIAN_POINT ( 'NONE',  ( 1.227938101723756947, 6.439911493064564674, 42.43379953535188065 ) ) ;
#13817 = CARTESIAN_POINT ( 'NONE',  ( 0.8751705887134423323, 47.55935879196461968, 7.160166390004468973 ) ) ;
#13818 = ADVANCED_FACE ( 'NONE', ( #48833 ), #38009, .F. ) ;
#13819 = ORIENTED_EDGE ( 'NONE', *, *, #16358, .T. ) ;
#13820 = CARTESIAN_POINT ( 'NONE',  ( 0.6067099128993237445, -46.07641759122972047, 13.08009036336186526 ) ) ;
#13821 = DIRECTION ( 'NONE',  ( 0.000000000000000000, 0.000000000000000000, 1.000000000000000000 ) ) ;
#13822 = DIRECTION ( 'NONE',  ( 1.000000000000000000, 0.000000000000000000, 0.000000000000000000 ) ) ;
#13823 = VERTEX_POINT ( 'NONE', #19721 ) ;
#13824 = CARTESIAN_POINT ( 'NONE',  ( 0.1140933569871964287, 4.614317128159971304, -43.88232021583037579 ) ) ;
#13825 = CARTESIAN_POINT ( 'NONE',  ( 0.5817216825391129387, -46.04481145225960859, -8.894396580618670001 ) ) ;
#13826 = CARTESIAN_POINT ( 'NONE',  ( 0.8753041380234530822, -45.84117188851829638, -17.59901382919792212 ) ) ;
#13827 = EDGE_LOOP ( 'NONE', ( #34460, #5214, #57167, #32767 ) ) ;
#13828 = CARTESIAN_POINT ( 'NONE',  ( 0.8560838555295223751, 31.94705745926225404, -34.34761059777416392 ) ) ;
#13829 = CIRCLE ( 'NONE', #11816, 48.91267123290010943 ) ;
#13830 = ORIENTED_EDGE ( 'NONE', *, *, #5349, .F. ) ;
#13831 = ORIENTED_EDGE ( 'NONE', *, *, #5123, .F. ) ;
#13832 = CARTESIAN_POINT ( 'NONE',  ( 0.8744876279028306332, -45.16590161815026505, 19.24555484778404590 ) ) ;
#13833 = ORIENTED_EDGE ( 'NONE', *, *, #58541, .T. ) ;
#13834 = CARTESIAN_POINT ( 'NONE',  ( 0.5850706913938533704, -0.1816364388703713695, 47.89601588673689037 ) ) ;
#13835 = EDGE_LOOP ( 'NONE', ( #58299, #23501, #14318, #60604 ) ) ;
#13836 = CARTESIAN_POINT ( 'NONE',  ( 0.7056313189692701160, 11.69102722649127202, 45.42101414925695479 ) ) ;
#13837 = B_SPLINE_CURVE_WITH_KNOTS ( 'NONE', 3,
 ( #7891, #17931, #27010, #18235 ),
 .UNSPECIFIED., .F., .F.,
 ( 4, 4 ),
 ( 0.000000000000000000, 0.004041751736740996012 ),
 .UNSPECIFIED. ) ;
#13838 =( BOUNDED_SURFACE ( )  B_SPLINE_SURFACE ( 3, 1, ( 
 ( #30555, #35903 ),
 ( #39377, #54971 ),
 ( #12104, #31179 ),
 ( #25553, #44691 ) ),
 .UNSPECIFIED., .F., .F., .F. ) 
 B_SPLINE_SURFACE_WITH_KNOTS ( ( 4, 4 ),
 ( 2, 2 ),
 ( 0.000000000000000000, 1.000000000000000000 ),
 ( 0.000000000000000000, 1.000000000000000000 ),
 .UNSPECIFIED. ) 
 GEOMETRIC_REPRESENTATION_ITEM ( )  RATIONAL_B_SPLINE_SURFACE ( (
 ( 1.000000000000000000, 1.000000000000000000),
 ( 0.7223157951917476005, 0.9931996967497186413),
 ( 0.7223157951917476005, 0.9931996967497186413),
 ( 1.000000000000000000, 1.000000000000000000) ) ) 
 REPRESENTATION_ITEM ( '' )  SURFACE ( )  );
#13839 = CARTESIAN_POINT ( 'NONE',  ( 3.783198216974390071, 14.86152287314682852, 40.39102707215861443 ) ) ;
#13840 = CARTESIAN_POINT ( 'NONE',  ( 0.6009452777970410997, -0.4363873594209082829, -48.10564074251961131 ) ) ;
#13841 = ORIENTED_EDGE ( 'NONE', *, *, #3602, .F. ) ;
#13842 =( BOUNDED_SURFACE ( )  B_SPLINE_SURFACE ( 3, 1, ( 
 ( #41962, #55398 ),
 ( #17516, #41344 ),
 ( #56638, #60395 ),
 ( #18136, #22524 ) ),
 .UNSPECIFIED., .F., .F., .F. ) 
 B_SPLINE_SURFACE_WITH_KNOTS ( ( 4, 4 ),
 ( 2, 2 ),
 ( 0.000000000000000000, 1.000000000000000000 ),
 ( 0.000000000000000000, 1.000000000000000000 ),
 .UNSPECIFIED. ) 
 GEOMETRIC_REPRESENTATION_ITEM ( )  RATIONAL_B_SPLINE_SURFACE ( (
 ( 1.000000000000000000, 1.000000000000000000),
 ( 0.9751682680413298332, 0.9999560080971552356),
 ( 0.9751682680413298332, 0.9999560080971552356),
 ( 1.000000000000000000, 1.000000000000000000) ) ) 
 REPRESENTATION_ITEM ( '' )  SURFACE ( )  );
#13843 = CARTESIAN_POINT ( 'NONE',  ( 4.967162193818130511, 0.000000000000000000, 0.000000000000000000 ) ) ;
#13844 = VECTOR ( 'NONE', #20852, 1000.000000000000114 ) ;
#13845 = CARTESIAN_POINT ( 'NONE',  ( -6.078726893082806448, -14.66462719274100479, -12.47969352855434444 ) ) ;
#13846 = CARTESIAN_POINT ( 'NONE',  ( 5.894904586330512508, 17.95171060118311246, -9.070032996247173074 ) ) ;
#13847 = CARTESIAN_POINT ( 'NONE',  ( 0.1129192098497447394, -23.28677643606880565, -37.47903188453118162 ) ) ;
#13848 = VERTEX_POINT ( 'NONE', #38848 ) ;
#13849 = CARTESIAN_POINT ( 'NONE',  ( 0.5827359174754811466, -33.60976280407625438, -34.12345922495646278 ) ) ;
#13850 = CARTESIAN_POINT ( 'NONE',  ( 0.1157991065609915993, -31.63987847695578992, -30.75484442329644352 ) ) ;
#13851 = VERTEX_POINT ( 'NONE', #15029 ) ;
#13852 = CARTESIAN_POINT ( 'NONE',  ( 0.5835226383429308328, 43.10343935657192560, -18.47528051695807960 ) ) ;
#13853 = EDGE_LOOP ( 'NONE', ( #35225, #59638, #10060, #58161, #3932, #57013 ) ) ;
#13854 = DIRECTION ( 'NONE',  ( -1.000000000000000000, -0.000000000000000000, -0.000000000000000000 ) ) ;
#13855 = EDGE_CURVE ( 'NONE', #26491, #8159, #2124, .T. ) ;
#13856 = CARTESIAN_POINT ( 'NONE',  ( 0.6029443449137436017, 46.61938292040374421, -15.43284400569447001 ) ) ;
#13857 = EDGE_LOOP ( 'NONE', ( #46722, #41790, #37267, #41170 ) ) ;
#13858 = CARTESIAN_POINT ( 'NONE',  ( 0.5835871038041867687, 4.558181011431630125, 46.67394818063417716 ) ) ;
#13859 = CARTESIAN_POINT ( 'NONE',  ( 0.1129192098497447394, 24.84520063729181416, -36.46461014569973713 ) ) ;
#13860 = CARTESIAN_POINT ( 'NONE',  ( 0.3676999524040366896, -0.5887207181726206162, 44.10900124961835900 ) ) ;
#13861 = DIRECTION ( 'NONE',  ( 0.000000000000000000, 0.000000000000000000, 1.000000000000000000 ) ) ;
#13862 = VECTOR ( 'NONE', #27952, 1000.000000000000114 ) ;
#13863 = EDGE_LOOP ( 'NONE', ( #24391, #48821, #20693, #51800 ) ) ;
#13864 = CARTESIAN_POINT ( 'NONE',  ( 4.962356264823608143, 0.000000000000000000, 0.000000000000000000 ) ) ;
#13865 = CARTESIAN_POINT ( 'NONE',  ( 0.9788927965476027504, -41.80537879722813699, 2.940563934357716125 ) ) ;
#13866 = CARTESIAN_POINT ( 'NONE',  ( -6.016104459813371719, -18.84322058118302579, 0.005335450885000186244 ) ) ;
#13867 = CARTESIAN_POINT ( 'NONE',  ( 4.963659409799330291, 29.14784479683158480, -33.96111158240212546 ) ) ;
#13868 = CARTESIAN_POINT ( 'NONE',  ( 0.5800708057587368183, 46.42229836006555388, -11.78915002112674415 ) ) ;
#13869 = CARTESIAN_POINT ( 'NONE',  ( 0.5837374860065636106, -46.21667939904224198, 12.57177159055146554 ) ) ;
#13870 = AXIS2_PLACEMENT_3D ( 'NONE', #57159, #463, #4850 ) ;
#13871 = LINE ( 'NONE', #33901, #11888 ) ;
#13872 = CIRCLE ( 'NONE', #19861, 2.649999999999997691 ) ;
#13873 = CARTESIAN_POINT ( 'NONE',  ( 0.5835871038041865466, 40.41881746160861866, -23.78137186763330746 ) ) ;
#13874 = FACE_OUTER_BOUND ( 'NONE', #23852, .T. ) ;
#13875 = CARTESIAN_POINT ( 'NONE',  ( 0.9736507210033054083, 30.65767007549955636, -30.02062799605167953 ) ) ;
#13876 = CARTESIAN_POINT ( 'NONE',  ( 0.1073791018717483448, -21.14095454447585709, 37.58707531572169813 ) ) ;
#13877 = CARTESIAN_POINT ( 'NONE',  ( 1.154321713695929619, -34.54400171733321656, 25.46626713715447110 ) ) ;
#13878 = CARTESIAN_POINT ( 'NONE',  ( 4.960386119450149955, -42.32154583640194545, 11.10509895001706226 ) ) ;
#13879 = CARTESIAN_POINT ( 'NONE',  ( -3.282060897439242453, -10.26526840094480164, 3.000000000000015987 ) ) ;
#13880 = ADVANCED_FACE ( 'NONE', ( #20950 ), #61553, .F. ) ;
#13881 = CARTESIAN_POINT ( 'NONE',  ( 0.9756354156337477823, -37.09450626018194441, -21.56699035436975365 ) ) ;
#13882 = EDGE_CURVE ( 'NONE', #40357, #18777, #46306, .T. ) ;
#13883 = CARTESIAN_POINT ( 'NONE',  ( 0.5824935313925952984, 45.13218173562562896, -12.74065731570774318 ) ) ;
#13884 = CARTESIAN_POINT ( 'NONE',  ( 1.227938101723756947, 34.55893248994507161, 25.45152231597068848 ) ) ;
#13886 = ORIENTED_EDGE ( 'NONE', *, *, #10119, .T. ) ;
#13885 = CARTESIAN_POINT ( 'NONE',  ( 0.9757787079277444597, 39.62711913632698923, 16.45683390770799193 ) ) ;
#13887 = B_SPLINE_CURVE_WITH_KNOTS ( 'NONE', 3,
 ( #19929, #39340, #6076, #16138 ),
 .UNSPECIFIED., .F., .F.,
 ( 4, 4 ),
 ( 1.734723475976807094E-18, 0.004050076154993002484 ),
 .UNSPECIFIED. ) ;
#13888 = CIRCLE ( 'NONE', #22860, 47.09074272231896430 ) ;
#13889 = CARTESIAN_POINT ( 'NONE',  ( 4.967162193818132288, 19.45289607368876617, -38.44485641567052880 ) ) ;
#13890 = CARTESIAN_POINT ( 'NONE',  ( 0.5839880159502351953, 23.90868446765477273, 41.50181427378110754 ) ) ;
#13891 = CARTESIAN_POINT ( 'NONE',  ( 5.959547316686252039, 19.82715097195154996, 5.308980600728524735 ) ) ;
#13892 = EDGE_CURVE ( 'NONE', #4050, #47638, #8110, .T. ) ;
#13893 = ORIENTED_EDGE ( 'NONE', *, *, #12516, .T. ) ;
#13894 = CARTESIAN_POINT ( 'NONE',  ( 3.050102900204245682, -30.31663646424969372, 31.87988084470495664 ) ) ;
#13895 = CARTESIAN_POINT ( 'NONE',  ( 0.5987334308729319599, 5.317554817413186363, 48.81891556900394846 ) ) ;
#13896 = B_SPLINE_CURVE_WITH_KNOTS ( 'NONE', 3,
 ( #5121, #53359, #43388, #38382 ),
 .UNSPECIFIED., .F., .F.,
 ( 4, 4 ),
 ( 1.998817200139820460E-17, 0.004444306975806115029 ),
 .UNSPECIFIED. ) ;
#13897 = ORIENTED_EDGE ( 'NONE', *, *, #54468, .F. ) ;
#13898 = EDGE_LOOP ( 'NONE', ( #61945, #41165, #7059, #40662 ) ) ;
#13899 = CARTESIAN_POINT ( 'NONE',  ( 0.5998501479064708430, 41.39809967730453621, 24.50586714782619424 ) ) ;
#13900 = VERTEX_POINT ( 'NONE', #2748 ) ;
#13901 = EDGE_CURVE ( 'NONE', #61276, #59093, #3660, .T. ) ;
#13902 = CARTESIAN_POINT ( 'NONE',  ( 2.500000000000000000, 1.768423874527823791, 1.020999999999998353 ) ) ;
#13903 = CARTESIAN_POINT ( 'NONE',  ( 0.8560838555295158248, 28.55542365806940452, -37.21505896528851309 ) ) ;
#13904 = AXIS2_PLACEMENT_3D ( 'NONE', #30027, #44475, #20637 ) ;
#13905 = VERTEX_POINT ( 'NONE', #1507 ) ;
#13906 = ORIENTED_EDGE ( 'NONE', *, *, #51619, .F. ) ;
#13907 = LINE ( 'NONE', #4756, #43764 ) ;
#13909 = ORIENTED_EDGE ( 'NONE', *, *, #54547, .T. ) ;
#13908 = ADVANCED_FACE ( 'NONE', ( #25335 ), #25528, .F. ) ;
#13910 = CARTESIAN_POINT ( 'NONE',  ( 0.9968887458511651589, 11.73947777183279051, -41.27232779986108113 ) ) ;
#13911 = CARTESIAN_POINT ( 'NONE',  ( 4.975801465491695552, 47.84403947906839960, 2.564218696447662982 ) ) ;
#13912 = B_SPLINE_CURVE_WITH_KNOTS ( 'NONE', 3,
 ( #59712, #16829, #55007, #2695 ),
 .UNSPECIFIED., .F., .F.,
 ( 4, 4 ),
 ( 6.505213034913026604E-19, 0.004048833967417086489 ),
 .UNSPECIFIED. ) ;
#13913 = B_SPLINE_CURVE_WITH_KNOTS ( 'NONE', 3,
 ( #23997, #26453, #11442, #15840 ),
 .UNSPECIFIED., .F., .F.,
 ( 4, 4 ),
 ( 4.336808689942017736E-19, 0.004446298630425052009 ),
 .UNSPECIFIED. ) ;
#13914 = DIRECTION ( 'NONE',  ( -0.1736481776669312471, 0.9848077530122077983, -5.551115123125779621E-17 ) ) ;
#13915 = ORIENTED_EDGE ( 'NONE', *, *, #52235, .F. ) ;
#13916 = CARTESIAN_POINT ( 'NONE',  ( 0.2940135542859016460, -7.834165714058259233, -43.41504803931575651 ) ) ;
#13917 = CARTESIAN_POINT ( 'NONE',  ( 0.9752570700956796346, -33.90066715551953536, -26.30364510018343438 ) ) ;
#13918 = ORIENTED_EDGE ( 'NONE', *, *, #15588, .F. ) ;
#13919 = ORIENTED_EDGE ( 'NONE', *, *, #38543, .F. ) ;
#13920 = CARTESIAN_POINT ( 'NONE',  ( -6.016761891674564211, 11.46828378093580980, -14.95139917749692415 ) ) ;
#13921 = AXIS2_PLACEMENT_3D ( 'NONE', #2011, #22376, #45901 ) ;
#13922 = ORIENTED_EDGE ( 'NONE', *, *, #29760, .T. ) ;
#13923 = CARTESIAN_POINT ( 'NONE',  ( 2.879087469061462734, 34.60096728254691101, 27.18225045678699203 ) ) ;
#13924 = CARTESIAN_POINT ( 'NONE',  ( -2.739355103387248747, 4.908046929417360538, -14.09817868696712040 ) ) ;
#13925 = CARTESIAN_POINT ( 'NONE',  ( 0.9741495583595179975, -0.3955098476634577032, 42.90659993968954922 ) ) ;
#13926 = CARTESIAN_POINT ( 'NONE',  ( 0.1103878639767399694, 5.676988162228092882, 42.74915604780181866 ) ) ;
#13927 = FACE_OUTER_BOUND ( 'NONE', #38554, .T. ) ;
#13928 = ORIENTED_EDGE ( 'NONE', *, *, #17619, .T. ) ;
#13929 = CARTESIAN_POINT ( 'NONE',  ( 5.901764892641288895, -32.89013534638917235, 36.27989063290957006 ) ) ;
#13930 = CARTESIAN_POINT ( 'NONE',  ( 0.1073791018717578927, -10.69234304550026593, -41.77800844988510676 ) ) ;
#13931 = CARTESIAN_POINT ( 'NONE',  ( 5.901463166500145796, 18.99503018386004527, 6.611104193316173827 ) ) ;
#13932 = ADVANCED_FACE ( 'NONE', ( #30031 ), #46782, .F. ) ;
#13933 = ORIENTED_EDGE ( 'NONE', *, *, #18689, .F. ) ;
#13934 = CARTESIAN_POINT ( 'NONE',  ( 4.958415959904823644, 19.57736038521000665, 40.98696029434541543 ) ) ;
#13935 = CARTESIAN_POINT ( 'NONE',  ( 0.9730545539215892381, 29.98130006528861813, 30.69604515769660935 ) ) ;
#13936 = CARTESIAN_POINT ( 'NONE',  ( 4.553261556744875094, -4.442710778082547662, 43.70128015019636791 ) ) ;
#13937 = CONICAL_SURFACE ( 'NONE', #28882, 43.92652462719577500, 1.486293639869522343 ) ;
#13938 = ORIENTED_EDGE ( 'NONE', *, *, #27382, .T. ) ;
#13939 = VERTEX_POINT ( 'NONE', #11561 ) ;
#13940 = CARTESIAN_POINT ( 'NONE',  ( 0.2279481005628787582, 19.73059023567995141, 39.46146596395783490 ) ) ;
#13941 = CARTESIAN_POINT ( 'NONE',  ( 0.1081432562775999084, -42.80885385101085916, 5.208748643065970185 ) ) ;
#13942 = CARTESIAN_POINT ( 'NONE',  ( 4.975801465491695552, -8.787181743660504196, 47.10002938642126935 ) ) ;
#13943 = CARTESIAN_POINT ( 'NONE',  ( 4.975801465491695552, 0.000000000000000000, 0.000000000000000000 ) ) ;
#13944 = CARTESIAN_POINT ( 'NONE',  ( 0.6041374136657476912, 29.14743607025083350, -38.27243465845312187 ) ) ;
#13945 = CARTESIAN_POINT ( 'NONE',  ( -2.569797478183783568, 5.182550149005303197, -13.68441171582010973 ) ) ;
#13946 = CARTESIAN_POINT ( 'NONE',  ( 4.291220156522059348, 35.59851124210522499, 30.85668476442996777 ) ) ;
#13947 = CARTESIAN_POINT ( 'NONE',  ( 0.2224561200757667057, 40.12166550582812619, -15.79689521915824280 ) ) ;
#13948 = CARTESIAN_POINT ( 'NONE',  ( 5.901764892641288895, 39.21882766674634979, -29.32362569474874903 ) ) ;
#13949 = CARTESIAN_POINT ( 'NONE',  ( 0.9730545539215883499, 21.01499094264548972, 37.40983423658480689 ) ) ;
#13950 = CARTESIAN_POINT ( 'NONE',  ( 5.896782393890504181, -17.30835043929363692, 10.24436879210309925 ) ) ;
#13951 = CARTESIAN_POINT ( 'NONE',  ( 0.9780106845699465534, -1.086875070857868941, -41.89450977199504678 ) ) ;
#13952 = FACE_OUTER_BOUND ( 'NONE', #10298, .T. ) ;
#13953 = ORIENTED_EDGE ( 'NONE', *, *, #58107, .F. ) ;
#13954 = CARTESIAN_POINT ( 'NONE',  ( 3.678834586032787790, -38.11572800053880883, -30.75392086575784489 ) ) ;
#13955 = LINE ( 'NONE', #57127, #1389 ) ;
#13956 = CARTESIAN_POINT ( 'NONE',  ( -6.015611763856276717, -11.46610900684733281, 14.95313250337425970 ) ) ;
#13957 = CARTESIAN_POINT ( 'NONE',  ( 0.5997462898726536595, -39.04071682475767346, -29.78882441375276358 ) ) ;
#13958 = DIRECTION ( 'NONE',  ( 0.1011922191286468292, -0.7056551247449976971, 0.7012923639317212299 ) ) ;
#13959 = CARTESIAN_POINT ( 'NONE',  ( 4.956653778116975495, -35.79382859084138602, 32.11725092155030836 ) ) ;
#13960 = CARTESIAN_POINT ( 'NONE',  ( 4.322998006666165516, -47.94177812210863010, -2.120302895116112030 ) ) ;
#13961 = VECTOR ( 'NONE', #17506, 1000.000000000000114 ) ;
#13962 = APPLICATION_CONTEXT ( 'automotive_design' ) ;
#13963 =( BOUNDED_SURFACE ( )  B_SPLINE_SURFACE ( 3, 1, ( 
 ( #43079, #14265 ),
 ( #22719, #61524 ),
 ( #27728, #18031 ),
 ( #33064, #18344 ) ),
 .UNSPECIFIED., .F., .F., .F. ) 
 B_SPLINE_SURFACE_WITH_KNOTS ( ( 4, 4 ),
 ( 2, 2 ),
 ( 0.000000000000000000, 1.000000000000000000 ),
 ( 0.000000000000000000, 1.000000000000000000 ),
 .UNSPECIFIED. ) 
 GEOMETRIC_REPRESENTATION_ITEM ( )  RATIONAL_B_SPLINE_SURFACE ( (
 ( 1.000000000000000000, 1.000000000000000000),
 ( 0.9953390228620291325, 0.8624445117761032620),
 ( 0.9953390228620291325, 0.8624445117761032620),
 ( 1.000000000000000000, 1.000000000000000000) ) ) 
 REPRESENTATION_ITEM ( '' )  SURFACE ( )  );
#13964 = DIRECTION ( 'NONE',  ( -1.000000000000000000, -0.000000000000000000, -0.000000000000000000 ) ) ;
#13965 = B_SPLINE_CURVE_WITH_KNOTS ( 'NONE', 3,
 ( #55822, #42377, #17945, #12944, #27328, #18550 ),
 .UNSPECIFIED., .F., .F.,
 ( 4, 2, 4 ),
 ( 1.540307523853160897E-16, 0.0002445252820015214666, 0.0004890505640028889765 ),
 .UNSPECIFIED. ) ;
#13966 = ADVANCED_FACE ( 'NONE', ( #16882 ), #21142, .F. ) ;
#13967 = CARTESIAN_POINT ( 'NONE',  ( 5.860006189529234355, 3.137522369586185800, -48.13093674595581462 ) ) ;
#13969 = VERTEX_POINT ( 'NONE', #7437 ) ;
#13968 = CARTESIAN_POINT ( 'NONE',  ( 0.1129192098497447394, -35.64954734424924965, -26.00118385641864194 ) ) ;
#13970 = ORIENTED_EDGE ( 'NONE', *, *, #20055, .T. ) ;
#13971 = AXIS2_PLACEMENT_3D ( 'NONE', #32036, #41758, #37671 ) ;
#13972 = CARTESIAN_POINT ( 'NONE',  ( 0.1157991065609915576, -7.122568489526775792, 43.54550933965177251 ) ) ;
#13973 = CARTESIAN_POINT ( 'NONE',  ( 5.910764540655178756, 5.943959005785093730, -19.21381247453792440 ) ) ;
#13974 = CARTESIAN_POINT ( 'NONE',  ( 4.549368137175248350, 0.000000000000000000, 0.000000000000000000 ) ) ;
#13975 = EDGE_CURVE ( 'NONE', #46997, #61046, #22637, .T. ) ;
#13976 = EDGE_LOOP ( 'NONE', ( #44625, #21183, #10908, #46865 ) ) ;
#13977 = CARTESIAN_POINT ( 'NONE',  ( 0.000000000000000000, -2.357898499370432166, 3.035766082959412415E-15 ) ) ;
#13978 = LINE ( 'NONE', #33081, #10147 ) ;
#13979 = CARTESIAN_POINT ( 'NONE',  ( 0.6025881611877910160, -44.36157157392742079, -18.61132239451771042 ) ) ;
#13980 = EDGE_CURVE ( 'NONE', #35775, #57870, #46664, .T. ) ;
#13981 = VERTEX_POINT ( 'NONE', #31582 ) ;
#13982 = ORIENTED_EDGE ( 'NONE', *, *, #59954, .F. ) ;
#13983 = DIRECTION ( 'NONE',  ( 0.1024043820194936311, 0.2701391291102721026, 0.9573600124648768972 ) ) ;
#13984 = CARTESIAN_POINT ( 'NONE',  ( 2.299652685299202304, 23.81424953469105077, -42.86214231647340966 ) ) ;
#13985 = CARTESIAN_POINT ( 'NONE',  ( 0.2940135542859017015, -44.10887657611353774, 0.8047085712246067057 ) ) ;
#13986 = EDGE_CURVE ( 'NONE', #36980, #26618, #22324, .T. ) ;
#13987 = CARTESIAN_POINT ( 'NONE',  ( 0.5998501479064699549, -17.92509395669137362, 44.64337787626217846 ) ) ;
#13988 = CARTESIAN_POINT ( 'NONE',  ( 58.00000000000000000, 0.000000000000000000, 12.50000000000000000 ) ) ;
#13989 = CARTESIAN_POINT ( 'NONE',  ( 4.553261556744875094, 40.63093864075490558, 16.69330377710913993 ) ) ;
#13990 = ORIENTED_EDGE ( 'NONE', *, *, #37704, .F. ) ;
#13991 = LINE ( 'NONE', #3925, #32879 ) ;
#13992 = CARTESIAN_POINT ( 'NONE',  ( 2.282816707992310512, -44.78789143672629791, -14.16127632171569317 ) ) ;
#13993 = VERTEX_POINT ( 'NONE', #41312 ) ;
#13994 = CARTESIAN_POINT ( 'NONE',  ( 2.301430502907646058, -47.43735983879647478, -7.543848632415047106 ) ) ;
#13995 = CARTESIAN_POINT ( 'NONE',  ( -6.077587904424778920, 17.84644683124306397, 7.231898567703008318 ) ) ;
#13996 = CARTESIAN_POINT ( 'NONE',  ( 0.9775691876210976794, 4.570554008562618620, -41.65865750411074231 ) ) ;
#13997 = CARTESIAN_POINT ( 'NONE',  ( 1.227938101723756947, 26.79402671879326547, 33.52879263017872091 ) ) ;
#13998 = ORIENTED_EDGE ( 'NONE', *, *, #9820, .F. ) ;
#13999 = ORIENTED_EDGE ( 'NONE', *, *, #39888, .T. ) ;
#14000 = CARTESIAN_POINT ( 'NONE',  ( 0.1152339509894530906, -44.12360796003454055, 0.2234077984745104495 ) ) ;
#14001 = CARTESIAN_POINT ( 'NONE',  ( -6.078075953587585900, 18.62761703674207325, 4.879247665328402483 ) ) ;
#14002 = CARTESIAN_POINT ( 'NONE',  ( -6.016761891674564211, -2.462934516563682230, -18.68153697670644320 ) ) ;
#14003 = ORIENTED_EDGE ( 'NONE', *, *, #50876, .T. ) ;
#14004 = CARTESIAN_POINT ( 'NONE',  ( -17.97369999999976642, 0.000000000000000000, -1.381000053334577907E-15 ) ) ;
#14005 = ORIENTED_EDGE ( 'NONE', *, *, #13583, .T. ) ;
#14006 = CARTESIAN_POINT ( 'NONE',  ( -6.017396004339687465, -0.001173774849114137117, 18.84316306185412415 ) ) ;
#14007 = CARTESIAN_POINT ( 'NONE',  ( 0.6026777506516367566, -25.30784732013451688, 42.08395483623157673 ) ) ;
#14008 = AXIS2_PLACEMENT_3D ( 'NONE', #33470, #9964, #58162 ) ;
#14009 = ORIENTED_EDGE ( 'NONE', *, *, #14088, .F. ) ;
#14010 = DIRECTION ( 'NONE',  ( 0.000000000000000000, 0.000000000000000000, 1.000000000000000000 ) ) ;
#14011 = EDGE_CURVE ( 'NONE', #59309, #30886, #28957, .T. ) ;
#14012 = CARTESIAN_POINT ( 'NONE',  ( -6.078457390727109555, 19.25602481922002340, 0.004381676659707368741 ) ) ;
#14013 = CARTESIAN_POINT ( 'NONE',  ( 4.553261556744875094, 0.000000000000000000, 0.000000000000000000 ) ) ;
#14015 = EDGE_LOOP ( 'NONE', ( #2717, #61959, #13464, #48922 ) ) ;
#14014 = EDGE_CURVE ( 'NONE', #55761, #41166, #16607, .T. ) ;
#14016 =( BOUNDED_SURFACE ( )  B_SPLINE_SURFACE ( 3, 1, ( 
 ( #39192, #20373 ),
 ( #35101, #39500 ),
 ( #30067, #25680 ),
 ( #1859, #35410 ) ),
 .UNSPECIFIED., .F., .F., .F. ) 
 B_SPLINE_SURFACE_WITH_KNOTS ( ( 4, 4 ),
 ( 2, 2 ),
 ( 0.000000000000000000, 1.000000000000000000 ),
 ( 0.000000000000000000, 1.000000000000000000 ),
 .UNSPECIFIED. ) 
 GEOMETRIC_REPRESENTATION_ITEM ( )  RATIONAL_B_SPLINE_SURFACE ( (
 ( 1.000000000000000000, 1.000000000000000000),
 ( 0.9952954269826590483, 0.8620686068821339365),
 ( 0.9952954269826590483, 0.8620686068821339365),
 ( 1.000000000000000000, 1.000000000000000000) ) ) 
 REPRESENTATION_ITEM ( '' )  SURFACE ( )  );
#14017 = CARTESIAN_POINT ( 'NONE',  ( 0.5998501479064708430, 47.76154736470757456, -5.759754759340284913 ) ) ;
#14018 = CARTESIAN_POINT ( 'NONE',  ( 0.9762797500689124330, -22.12212327108586152, -35.59405072711710716 ) ) ;
#14019 = CARTESIAN_POINT ( 'NONE',  ( 4.956653778116980824, -40.28700667097698584, 26.26162724282358951 ) ) ;
#14020 = CARTESIAN_POINT ( 'NONE',  ( 1.231276596079887931, -41.24008908601417289, -7.518764738684258653 ) ) ;
#14021 = CARTESIAN_POINT ( 'NONE',  ( 4.322998006666179727, 8.359821156455842228, 47.25487450103538833 ) ) ;
#14022 = ORIENTED_EDGE ( 'NONE', *, *, #942, .T. ) ;
#14023 = ADVANCED_FACE ( 'NONE', ( #3974 ), #17132, .F. ) ;
#14024 = CARTESIAN_POINT ( 'NONE',  ( 0.6000166863083106206, -14.47337940799720002, 46.92914627628140067 ) ) ;
#14025 = CARTESIAN_POINT ( 'NONE',  ( 5.895596859100789899, -15.78235929336536536, 12.46777118604649814 ) ) ;
#14026 = AXIS2_PLACEMENT_3D ( 'NONE', #37146, #32432, #56216 ) ;
#14027 = EDGE_LOOP ( 'NONE', ( #1515, #32100, #6145, #10022 ) ) ;
#14028 = CARTESIAN_POINT ( 'NONE',  ( 4.967162193818131399, -38.83676580803778933, 18.65818244221244981 ) ) ;
#14029 = CARTESIAN_POINT ( 'NONE',  ( 1.000433927950262980, 32.47840743411710918, -26.48719932715300018 ) ) ;
#14030 = CARTESIAN_POINT ( 'NONE',  ( 5.860006189529246790, -15.48781697582016115, -45.67886430272047704 ) ) ;
#14031 = B_SPLINE_CURVE_WITH_KNOTS ( 'NONE', 3,
 ( #11220, #25616, #35347, #29388 ),
 .UNSPECIFIED., .F., .F.,
 ( 4, 4 ),
 ( 0.000000000000000000, 0.005004741218457411933 ),
 .UNSPECIFIED. ) ;
#14032 = CARTESIAN_POINT ( 'NONE',  ( -5.995132425357893702, 9.414704407577803025, 16.32377331145323751 ) ) ;
#14033 = CARTESIAN_POINT ( 'NONE',  ( -1.399999999999998579, 0.000000000000000000, -5.000000000000000000 ) ) ;
#14034 = CARTESIAN_POINT ( 'NONE',  ( 0.8760168074887076939, -11.58706983520358236, 46.68716261866156003 ) ) ;
#14035 = CARTESIAN_POINT ( 'NONE',  ( 14.99999999999999289, 80.00000000000001421, -7.562144716216071966E-13 ) ) ;
#14036 = CARTESIAN_POINT ( 'NONE',  ( 0.5837157313716024865, 10.78286503748334546, 45.63953204367286531 ) ) ;
#14037 =( BOUNDED_SURFACE ( )  B_SPLINE_SURFACE ( 3, 1, ( 
 ( #6505, #25647 ),
 ( #44790, #47689 ),
 ( #1831, #4732 ),
 ( #43009, #48 ) ),
 .UNSPECIFIED., .F., .F., .F. ) 
 B_SPLINE_SURFACE_WITH_KNOTS ( ( 4, 4 ),
 ( 2, 2 ),
 ( 0.000000000000000000, 1.000000000000000000 ),
 ( 0.000000000000000000, 1.000000000000000000 ),
 .UNSPECIFIED. ) 
 GEOMETRIC_REPRESENTATION_ITEM ( )  RATIONAL_B_SPLINE_SURFACE ( (
 ( 1.000000000000000000, 1.000000000000000000),
 ( 0.9732289882329797637, 0.9999525324661233672),
 ( 0.9732289882329797637, 0.9999525324661233672),
 ( 1.000000000000000000, 1.000000000000000000) ) ) 
 REPRESENTATION_ITEM ( '' )  SURFACE ( )  );
#14038 = DIRECTION ( 'NONE',  ( 0.000000000000000000, 0.000000000000000000, 1.000000000000000000 ) ) ;
#14039 = EDGE_CURVE ( 'NONE', #30513, #32528, #51591, .T. ) ;
#14040 = DIRECTION ( 'NONE',  ( 0.000000000000000000, 0.000000000000000000, 1.000000000000000000 ) ) ;
#14041 = CARTESIAN_POINT ( 'NONE',  ( 4.553261556744875094, 40.80044851610500700, -16.27461110774390818 ) ) ;
#14042 = VERTEX_POINT ( 'NONE', #50981 ) ;
#14043 = CARTESIAN_POINT ( 'NONE',  ( 0.9754292580325131246, -1.982398290965677656, 41.86164788825186633 ) ) ;
#14044 = CARTESIAN_POINT ( 'NONE',  ( 0.5782707292762442330, 46.57382484760238839, -5.533099743586197050 ) ) ;
#14045 = EDGE_CURVE ( 'NONE', #44739, #50327, #50670, .T. ) ;
#14046 = CARTESIAN_POINT ( 'NONE',  ( -6.077587904424778920, 3.079371755031687474, -19.00824797261030241 ) ) ;
#14047 = CARTESIAN_POINT ( 'NONE',  ( 0.7056555295713301534, -47.89404551051140402, 0.8411712675126342686 ) ) ;
#14048 = CARTESIAN_POINT ( 'NONE',  ( 0.7413678028165014977, 32.96453683174787130, -29.28865656254279060 ) ) ;
#14049 = EDGE_CURVE ( 'NONE', #11576, #37959, #19653, .T. ) ;
#14050 = EDGE_LOOP ( 'NONE', ( #6686, #45911, #37661, #9015 ) ) ;
#14051 = CARTESIAN_POINT ( 'NONE',  ( 1.827326673878744812, -12.32830836993849566, 41.24690799101787064 ) ) ;
#14052 = CARTESIAN_POINT ( 'NONE',  ( 0.6027444965799114707, -45.46931311909032303, -18.54939568734145894 ) ) ;
#14053 = CARTESIAN_POINT ( 'NONE',  ( 2.000000000000010658, -3.464101615137748169, -5.600000000000000533 ) ) ;
#14054 = EDGE_LOOP ( 'NONE', ( #21273, #47960, #29457, #4567 ) ) ;
#14055 = CARTESIAN_POINT ( 'NONE',  ( 4.967162193818130511, 23.56777426397178132, 36.06913038482807821 ) ) ;
#14056 = ADVANCED_FACE ( 'NONE', ( #37536 ), #47634, .F. ) ;
#14057 = CARTESIAN_POINT ( 'NONE',  ( 0.5837800005270550319, 43.17481384069556327, 18.30766802361970136 ) ) ;
#14058 = EDGE_LOOP ( 'NONE', ( #41407, #56849, #15286, #55870 ) ) ;
#14059 = AXIS2_PLACEMENT_3D ( 'NONE', #59948, #17057, #7625 ) ;
#14060 = CARTESIAN_POINT ( 'NONE',  ( 3.727782113643637096, -25.70678629131670689, 35.66425261348605602 ) ) ;
#14061 = VERTEX_POINT ( 'NONE', #22189 ) ;
#14062 = CARTESIAN_POINT ( 'NONE',  ( 53.14999999999999858, 15.50000000000000711, 1.598617295522242905E-15 ) ) ;
#14063 = AXIS2_PLACEMENT_3D ( 'NONE', #52437, #61824, #33668 ) ;
#14064 = CARTESIAN_POINT ( 'NONE',  ( 0.6009452777970410997, 34.32439724342992093, 33.70725232128904736 ) ) ;
#14065 = VERTEX_POINT ( 'NONE', #3356 ) ;
#14066 = CARTESIAN_POINT ( 'NONE',  ( 4.549368137175248350, 0.000000000000000000, 0.000000000000000000 ) ) ;
#14067 = CARTESIAN_POINT ( 'NONE',  ( 0.8751705887134423323, 34.63284514348585930, -33.37254303619518225 ) ) ;
#14068 = LINE ( 'NONE', #31928, #57679 ) ;
#14069 = CARTESIAN_POINT ( 'NONE',  ( 4.960156602257180580, 41.40608197274633540, 20.99019478193063648 ) ) ;
#14070 = B_SPLINE_CURVE_WITH_KNOTS ( 'NONE', 3,
 ( #14557, #53047, #61511, #10459, #10149, #29243 ),
 .UNSPECIFIED., .F., .F.,
 ( 4, 2, 4 ),
 ( 1.516708938535782939E-16, 0.0002445252820015207619, 0.0004890505640028898439 ),
 .UNSPECIFIED. ) ;
#14071 = ORIENTED_EDGE ( 'NONE', *, *, #32980, .T. ) ;
#14072 = LINE ( 'NONE', #14374, #40770 ) ;
#14073 = ORIENTED_EDGE ( 'NONE', *, *, #60382, .F. ) ;
#14074 = CARTESIAN_POINT ( 'NONE',  ( 0.5786265663353153954, -28.58414684753512702, 38.43785771743193891 ) ) ;
#14075 = ORIENTED_EDGE ( 'NONE', *, *, #18760, .T. ) ;
#14076 = ORIENTED_EDGE ( 'NONE', *, *, #6532, .T. ) ;
#14077 = CARTESIAN_POINT ( 'NONE',  ( 1.231276596079887264, 28.52807286890788419, -30.71523773966838888 ) ) ;
#14079 = CARTESIAN_POINT ( 'NONE',  ( 0.9787464366903551038, -37.48376074964096460, 18.74304332156709663 ) ) ;
#14078 = B_SPLINE_CURVE_WITH_KNOTS ( 'NONE', 3,
 ( #52765, #38095, #24265, #52451 ),
 .UNSPECIFIED., .F., .F.,
 ( 4, 4 ),
 ( 9.757819552369539906E-19, 0.004446298630425057213 ),
 .UNSPECIFIED. ) ;
#14080 = CARTESIAN_POINT ( 'NONE',  ( 0.1081432562775998807, -16.89351827868247824, 39.67792926340371906 ) ) ;
#14081 = CYLINDRICAL_SURFACE ( 'NONE', #650, 2.649999999999992806 ) ;
#14082 = VERTEX_POINT ( 'NONE', #46314 ) ;
#14083 = CARTESIAN_POINT ( 'NONE',  ( -6.078457390727109555, -1.853383199521769331, 19.16662416163155314 ) ) ;
#14084 = EDGE_CURVE ( 'NONE', #37022, #4220, #57610, .T. ) ;
#14085 = CARTESIAN_POINT ( 'NONE',  ( 4.549368137175248350, 0.000000000000000000, 0.000000000000000000 ) ) ;
#14086 = CARTESIAN_POINT ( 'NONE',  ( 0.1157991065609916270, -38.48609893810574789, 21.58153270887022046 ) ) ;
#14087 = EDGE_LOOP ( 'NONE', ( #16335, #60573, #28777, #33435 ) ) ;
#14088 = EDGE_CURVE ( 'NONE', #48392, #14741, #19334, .T. ) ;
#14089 = EDGE_LOOP ( 'NONE', ( #9204, #40679, #27923, #27243 ) ) ;
#14090 = CARTESIAN_POINT ( 'NONE',  ( 1.227938101723748288, -42.43379953535180960, -6.439911493065006987 ) ) ;
#14091 = DIRECTION ( 'NONE',  ( -1.000000000000000000, -1.836909530733573776E-16, 1.925929944387235853E-32 ) ) ;
#14092 = CARTESIAN_POINT ( 'NONE',  ( 0.1100053167205930910, -34.10339839758302816, 26.39466280306210777 ) ) ;
#14093 = LINE ( 'NONE', #24395, #10804 ) ;
#14094 = ORIENTED_EDGE ( 'NONE', *, *, #3532, .F. ) ;
#14095 = EDGE_CURVE ( 'NONE', #45275, #28349, #55921, .T. ) ;
#14096 = VECTOR ( 'NONE', #46176, 1000.000000000000227 ) ;
#14097 = EDGE_CURVE ( 'NONE', #46978, #42733, #37314, .T. ) ;
#14098 = ORIENTED_EDGE ( 'NONE', *, *, #8274, .F. ) ;
#14099 = EDGE_CURVE ( 'NONE', #9817, #52417, #5089, .T. ) ;
#14100 = DIRECTION ( 'NONE',  ( 1.000000000000000000, -0.000000000000000000, -0.000000000000000000 ) ) ;
#14101 = CARTESIAN_POINT ( 'NONE',  ( 2.185380717157383135, 42.92198960651596451, -9.824592168906281842 ) ) ;
#14102 = B_SPLINE_CURVE_WITH_KNOTS ( 'NONE', 3,
 ( #44752, #53788, #43839, #38823, #10294, #54407 ),
 .UNSPECIFIED., .F., .F.,
 ( 4, 2, 4 ),
 ( 1.355252715606880735E-18, 0.0002293801035737095346, 0.0004587602071474177140 ),
 .UNSPECIFIED. ) ;
#14103 = CARTESIAN_POINT ( 'NONE',  ( 3.376099380956838925, -12.80728341440187457, 3.960034744197806766 ) ) ;
#14104 = CARTESIAN_POINT ( 'NONE',  ( 4.975801465491694664, 27.09127437476381317, -39.51822597168466444 ) ) ;
#14105 = SURFACE_STYLE_USAGE ( .BOTH. , #52279 ) ;
#14106 = CARTESIAN_POINT ( 'NONE',  ( 4.962356264823602814, 22.27740539909316198, -35.70648129607287302 ) ) ;
#14107 = AXIS2_PLACEMENT_3D ( 'NONE', #51460, #72, #38331 ) ;
#14108 = EDGE_CURVE ( 'NONE', #17781, #35390, #30504, .T. ) ;
#14109 = ORIENTED_EDGE ( 'NONE', *, *, #40281, .F. ) ;
#14110 = CARTESIAN_POINT ( 'NONE',  ( 0.1129192098497447394, 19.97823103613683315, -39.34236993944178806 ) ) ;
#14111 = CARTESIAN_POINT ( 'NONE',  ( 0.8744876279028306332, -45.83369275826206746, -17.59609782084448071 ) ) ;
#14112 = ADVANCED_FACE ( 'NONE', ( #15795 ), #27551, .F. ) ;
#14113 =( BOUNDED_SURFACE ( )  B_SPLINE_SURFACE ( 3, 1, ( 
 ( #34362, #29954 ),
 ( #53434, #48751 ),
 ( #57823, #19337 ),
 ( #39382, #5201 ) ),
 .UNSPECIFIED., .F., .F., .F. ) 
 B_SPLINE_SURFACE_WITH_KNOTS ( ( 4, 4 ),
 ( 2, 2 ),
 ( 0.000000000000000000, 1.000000000000000000 ),
 ( 0.000000000000000000, 1.000000000000000000 ),
 .UNSPECIFIED. ) 
 GEOMETRIC_REPRESENTATION_ITEM ( )  RATIONAL_B_SPLINE_SURFACE ( (
 ( 1.000000000000000000, 1.000000000000000000),
 ( 0.9952954269826590483, 0.8620686068821339365),
 ( 0.9952954269826590483, 0.8620686068821339365),
 ( 1.000000000000000000, 1.000000000000000000) ) ) 
 REPRESENTATION_ITEM ( '' )  SURFACE ( )  );
#14114 = CARTESIAN_POINT ( 'NONE',  ( 0.6000166863083106206, 22.25084548767560122, -43.78039923061506755 ) ) ;
#14115 = FACE_OUTER_BOUND ( 'NONE', #5331, .T. ) ;
#14116 = CARTESIAN_POINT ( 'NONE',  ( 5.880360259849739535, 15.46489389606690779, 45.41096578730653022 ) ) ;
#14117 = CARTESIAN_POINT ( 'NONE',  ( 0.5797568665920715958, 37.19047599010775684, 28.56735556944480336 ) ) ;
#14118 = LINE ( 'NONE', #42016, #22268 ) ;
#14119 = ORIENTED_EDGE ( 'NONE', *, *, #24978, .F. ) ;
#14120 =( BOUNDED_SURFACE ( )  B_SPLINE_SURFACE ( 3, 1, ( 
 ( #49114, #48806 ),
 ( #29690, #30609 ),
 ( #5556, #6166 ),
 ( #24693, #54403 ) ),
 .UNSPECIFIED., .F., .F., .F. ) 
 B_SPLINE_SURFACE_WITH_KNOTS ( ( 4, 4 ),
 ( 2, 2 ),
 ( 0.000000000000000000, 1.000000000000000000 ),
 ( 0.000000000000000000, 1.000000000000000000 ),
 .UNSPECIFIED. ) 
 GEOMETRIC_REPRESENTATION_ITEM ( )  RATIONAL_B_SPLINE_SURFACE ( (
 ( 1.000000000000000000, 1.000000000000000000),
 ( 0.7269869731126821222, 0.9931720237060910339),
 ( 0.7269869731126821222, 0.9931720237060910339),
 ( 1.000000000000000000, 1.000000000000000000) ) ) 
 REPRESENTATION_ITEM ( '' )  SURFACE ( )  );
#14121 = LINE ( 'NONE', #33222, #23868 ) ;
#14122 = CARTESIAN_POINT ( 'NONE',  ( 0.9780303403264780648, 20.42395051976790654, 36.59510703032791668 ) ) ;
#14123 = CARTESIAN_POINT ( 'NONE',  ( 4.694002226626920127, -43.37309735483326278, -14.03777750551312664 ) ) ;
#14124 = CARTESIAN_POINT ( 'NONE',  ( 4.975610109902397937, -10.32228546579698403, -47.81108480154335183 ) ) ;
#14125 = VERTEX_POINT ( 'NONE', #6341 ) ;
#14126 =( BOUNDED_SURFACE ( )  B_SPLINE_SURFACE ( 3, 1, ( 
 ( #32001, #13202 ),
 ( #17906, #61693 ),
 ( #23822, #61089 ),
 ( #42952, #37635 ) ),
 .UNSPECIFIED., .F., .F., .F. ) 
 B_SPLINE_SURFACE_WITH_KNOTS ( ( 4, 4 ),
 ( 2, 2 ),
 ( 0.000000000000000000, 1.000000000000000000 ),
 ( 0.000000000000000000, 1.000000000000000000 ),
 .UNSPECIFIED. ) 
 GEOMETRIC_REPRESENTATION_ITEM ( )  RATIONAL_B_SPLINE_SURFACE ( (
 ( 1.000000000000000000, 1.000000000000000000),
 ( 0.7211978278499970862, 0.9934217856018976445),
 ( 0.7211978278499970862, 0.9934217856018976445),
 ( 1.000000000000000000, 1.000000000000000000) ) ) 
 REPRESENTATION_ITEM ( '' )  SURFACE ( )  );
#14127 = CARTESIAN_POINT ( 'NONE',  ( 4.975801465491694664, -47.10002938642148251, 8.787181743659342459 ) ) ;
#14128 = CARTESIAN_POINT ( 'NONE',  ( 4.975801465491695552, -45.18341283946470099, 15.94009207552969620 ) ) ;
#14130 = ADVANCED_FACE ( 'NONE', ( #44020 ), #51682, .F. ) ;
#14129 = B_SPLINE_CURVE_WITH_KNOTS ( 'NONE', 3,
 ( #40461, #20714, #59526, #16634 ),
 .UNSPECIFIED., .F., .F.,
 ( 4, 4 ),
 ( 0.000000000000000000, 0.005014147105413706458 ),
 .UNSPECIFIED. ) ;
#14131 = B_SPLINE_CURVE_WITH_KNOTS ( 'NONE', 3,
 ( #42086, #51745, #37371, #4418, #18884, #55518 ),
 .UNSPECIFIED., .F., .F.,
 ( 4, 2, 4 ),
 ( 1.189851992356654836E-16, 0.0002448718616795952647, 0.0004897437233590714841 ),
 .UNSPECIFIED. ) ;
#14132 = EDGE_LOOP ( 'NONE', ( #15590, #295, #36062, #37525 ) ) ;
#14133 = CARTESIAN_POINT ( 'NONE',  ( 0.1145239942831223490, 4.561901227362215039, -43.88774929176096151 ) ) ;
#14134 = EDGE_CURVE ( 'NONE', #6976, #20061, #20190, .T. ) ;
#14135 = CARTESIAN_POINT ( 'NONE',  ( 0.5835226383429293895, -45.99229812474374768, -9.162477162354004889 ) ) ;
#14136 = ORIENTED_EDGE ( 'NONE', *, *, #54361, .F. ) ;
#14137 = CARTESIAN_POINT ( 'NONE',  ( -6.016761891674564211, 14.95139917749704495, 11.46828378093564460 ) ) ;
#14138 = EDGE_LOOP ( 'NONE', ( #49789, #36959, #47888, #25601 ) ) ;
#14139 = FACE_BOUND ( 'NONE', #43742, .T. ) ;
#14140 = VERTEX_POINT ( 'NONE', #16099 ) ;
#14141 = FACE_OUTER_BOUND ( 'NONE', #26321, .T. ) ;
#14142 = CARTESIAN_POINT ( 'NONE',  ( 0.8744876279028263033, 48.01195819035220325, 10.25679877483054625 ) ) ;
#14143 = ORIENTED_EDGE ( 'NONE', *, *, #27906, .F. ) ;
#14144 = ORIENTED_EDGE ( 'NONE', *, *, #53130, .F. ) ;
#14146 = B_SPLINE_CURVE_WITH_KNOTS ( 'NONE', 3,
 ( #54617, #39037, #34941, #49321 ),
 .UNSPECIFIED., .F., .F.,
 ( 4, 4 ),
 ( 0.000000000000000000, 0.005014147105413704723 ),
 .UNSPECIFIED. ) ;
#14145 = DIRECTION ( 'NONE',  ( 0.09835009131224564660, 0.3879606369183636883, -0.9164135549743742670 ) ) ;
#14147 = VECTOR ( 'NONE', #46778, 1000.000000000000000 ) ;
#14148 = CARTESIAN_POINT ( 'NONE',  ( 0.5998501479064708430, -38.48283596222049141, 28.86886762351059588 ) ) ;
#14149 = CARTESIAN_POINT ( 'NONE',  ( 0.6023142530420679819, -0.2618396477464183247, -48.10676733004997629 ) ) ;
#14150 = ORIENTED_EDGE ( 'NONE', *, *, #8729, .T. ) ;
#14151 = FACE_OUTER_BOUND ( 'NONE', #54077, .T. ) ;
#14152 = CARTESIAN_POINT ( 'NONE',  ( -6.057079549204054558, 18.62501892953336835, 4.892841809650328777 ) ) ;
#14153 = CARTESIAN_POINT ( 'NONE',  ( 3.238018933889920792, 8.164940828001933326, 10.61796749113878313 ) ) ;
#14154 = CARTESIAN_POINT ( 'NONE',  ( 0.7044674535452954967, -38.84805681606425054, -30.04382140185815331 ) ) ;
#14155 = ORIENTED_EDGE ( 'NONE', *, *, #16280, .F. ) ;
#14156 = CARTESIAN_POINT ( 'NONE',  ( 5.894904586330512508, 0.6708454810754242992, -20.10172575681410123 ) ) ;
#14157 = CARTESIAN_POINT ( 'NONE',  ( -4.908599999999998964, 12.80000000000000071, -3.000000000000000000 ) ) ;
#14158 = ORIENTED_EDGE ( 'NONE', *, *, #44026, .F. ) ;
#14159 = CARTESIAN_POINT ( 'NONE',  ( 0.8551540677456739292, 38.56334384152469852, -28.44084013485079865 ) ) ;
#14160 = ADVANCED_FACE ( 'NONE', ( #35215 ), #57746, .T. ) ;
#14161 = EDGE_LOOP ( 'NONE', ( #49637, #13131, #8138, #57851 ) ) ;
#14162 = DIRECTION ( 'NONE',  ( 0.09835009131224567436, 0.7091251765524070327, -0.6981896185982648939 ) ) ;
#14163 = CARTESIAN_POINT ( 'NONE',  ( 0.1064266379913938465, 11.70292640078096369, 41.50637574965952581 ) ) ;
#14164 = ORIENTED_EDGE ( 'NONE', *, *, #53999, .F. ) ;
#14165 = CARTESIAN_POINT ( 'NONE',  ( 5.896278296736517710, -17.30792457686169428, -10.24513184180911018 ) ) ;
#14166 = CARTESIAN_POINT ( 'NONE',  ( -6.079354080745853928, -19.21634661680160505, 1.234899976151772716 ) ) ;
#14167 = CARTESIAN_POINT ( 'NONE',  ( 4.956653778117001252, 47.05699031914963371, -9.917440902360649346 ) ) ;
#14168 = FACE_OUTER_BOUND ( 'NONE', #55494, .T. ) ;
#14169 = EDGE_CURVE ( 'NONE', #8059, #23991, #29088, .T. ) ;
#14170 = ADVANCED_FACE ( 'NONE', ( #53362 ), #51640, .T. ) ;
#14171 = ORIENTED_EDGE ( 'NONE', *, *, #20124, .T. ) ;
#14172 = CARTESIAN_POINT ( 'NONE',  ( -2.739355103387247858, 1.694972997839761186, -14.83154184458281755 ) ) ;
#14173 = EDGE_CURVE ( 'NONE', #48449, #27747, #61129, .T. ) ;
#14174 = CARTESIAN_POINT ( 'NONE',  ( 0.5786265663353153954, 29.72999788434292512, 37.55861529268563714 ) ) ;
#14175 = CARTESIAN_POINT ( 'NONE',  ( 2.301529144917014325, -19.56451384729014364, -43.86846428170453294 ) ) ;
#14176 = CARTESIAN_POINT ( 'NONE',  ( 0.5806925824938499181, 4.150136846022649095, 46.71186922510005957 ) ) ;
#14177 = CARTESIAN_POINT ( 'NONE',  ( -6.016761891674565099, -16.32039929810263601, 9.418621820384437626 ) ) ;
#14178 = ADVANCED_FACE ( 'NONE', ( #58358 ), #43702, .T. ) ;
#14179 = CARTESIAN_POINT ( 'NONE',  ( 4.956445790443998689, -27.49627641100115838, 38.22947597952995835 ) ) ;
#14180 = CARTESIAN_POINT ( 'NONE',  ( 0.5809828226811544205, 33.48000389720665027, -34.25055090842118233 ) ) ;
#14181 = CARTESIAN_POINT ( 'NONE',  ( 2.624215991343608501, -1.411420423865808571, 47.98682984381860450 ) ) ;
#14182 = CARTESIAN_POINT ( 'NONE',  ( 4.956445790444018229, -5.251077430595369577, -46.79705371022334504 ) ) ;
#14183 = CARTESIAN_POINT ( 'NONE',  ( -5.995132425357893702, -16.31525984181039846, 9.429450169547896721 ) ) ;
#14184 = DIRECTION ( 'NONE',  ( 0.000000000000000000, 0.000000000000000000, 1.000000000000000000 ) ) ;
#14185 = CARTESIAN_POINT ( 'NONE',  ( 4.975610109902397937, 35.53430708602585497, -33.61193875773584949 ) ) ;
#14186 = CIRCLE ( 'NONE', #49176, 0.7500000000000015543 ) ;
#14187 = DIRECTION ( 'NONE',  ( 0.000000000000000000, 0.000000000000000000, 1.000000000000000000 ) ) ;
#14188 = CARTESIAN_POINT ( 'NONE',  ( 0.8753041380234524160, 44.61941359694259290, 20.49990873486889242 ) ) ;
#14189 = AXIS2_PLACEMENT_3D ( 'NONE', #15271, #28739, #34376 ) ;
#14190 = CARTESIAN_POINT ( 'NONE',  ( 0.9741495583595187746, -36.96045061395516740, -21.79582154536840832 ) ) ;
#14191 = CARTESIAN_POINT ( 'NONE',  ( 4.956445790443998689, -5.251077430596073903, 46.79705371022326688 ) ) ;
#14192 = CARTESIAN_POINT ( 'NONE',  ( -31.74999999999995737, 3.061616997868383634E-16, -2.500000000000000444 ) ) ;
#14193 = B_SPLINE_CURVE_WITH_KNOTS ( 'NONE', 3,
 ( #54049, #45314, #2357, #17716, #50902, #21477 ),
 .UNSPECIFIED., .F., .F.,
 ( 4, 2, 4 ),
 ( 3.496446946337351263E-18, 0.0002450742804987356398, 0.0004901485609974678102 ),
 .UNSPECIFIED. ) ;
#14194 = ORIENTED_EDGE ( 'NONE', *, *, #23262, .F. ) ;
#14195 = CARTESIAN_POINT ( 'NONE',  ( 0.5980271706414734822, -34.78940872471004297, 34.66621241824281441 ) ) ;
#14196 = CARTESIAN_POINT ( 'NONE',  ( 5.880360259849752858, -45.44137230084892565, 15.37531919565157246 ) ) ;
#14197 = CARTESIAN_POINT ( 'NONE',  ( 4.975801465491695552, 0.000000000000000000, 0.000000000000000000 ) ) ;
#14198 = ORIENTED_EDGE ( 'NONE', *, *, #61572, .F. ) ;
#14199 = CARTESIAN_POINT ( 'NONE',  ( 0.5836750258453343720, -33.99574025613934225, 33.73891062492391768 ) ) ;
#14200 = CARTESIAN_POINT ( 'NONE',  ( 2.706805983486679335, 26.51819630001240569, 35.12209245352223519 ) ) ;
#14201 =( BOUNDED_SURFACE ( )  B_SPLINE_SURFACE ( 3, 1, ( 
 ( #42761, #9221 ),
 ( #28330, #4497 ),
 ( #18955, #38075 ),
 ( #109, #52431 ) ),
 .UNSPECIFIED., .F., .F., .F. ) 
 B_SPLINE_SURFACE_WITH_KNOTS ( ( 4, 4 ),
 ( 2, 2 ),
 ( 0.000000000000000000, 1.000000000000000000 ),
 ( 0.000000000000000000, 1.000000000000000000 ),
 .UNSPECIFIED. ) 
 GEOMETRIC_REPRESENTATION_ITEM ( )  RATIONAL_B_SPLINE_SURFACE ( (
 ( 1.000000000000000000, 1.000000000000000000),
 ( 0.9732289882329797637, 0.9999525324661233672),
 ( 0.9732289882329797637, 0.9999525324661233672),
 ( 1.000000000000000000, 1.000000000000000000) ) ) 
 REPRESENTATION_ITEM ( '' )  SURFACE ( )  );
#14202 = UNCERTAINTY_MEASURE_WITH_UNIT (LENGTH_MEASURE( 1.000000000000000082E-05 ), #17870, 'distance_accuracy_value', 'NONE');
#14203 = VERTEX_POINT ( 'NONE', #58990 ) ;
#14204 = VERTEX_POINT ( 'NONE', #1349 ) ;
#14205 = EDGE_CURVE ( 'NONE', #45637, #51265, #15181, .T. ) ;
#14206 = CARTESIAN_POINT ( 'NONE',  ( 0.6023143664670691511, -38.00627775314942625, -29.49326149840218747 ) ) ;
#14207 = VERTEX_POINT ( 'NONE', #34909 ) ;
#14208 = CARTESIAN_POINT ( 'NONE',  ( 0.5850706913938533704, -18.16120156791848217, -44.31965802246125463 ) ) ;
#14209 = CARTESIAN_POINT ( 'NONE',  ( -2.739355103387248747, -10.53896796905794986, 10.57249833758263513 ) ) ;
#14210 = EDGE_LOOP ( 'NONE', ( #30565, #16759, #7815, #8107 ) ) ;
#14211 = ORIENTED_EDGE ( 'NONE', *, *, #3840, .T. ) ;
#14212 = CARTESIAN_POINT ( 'NONE',  ( 4.967162193818130511, 0.000000000000000000, 0.000000000000000000 ) ) ;
#14213 = ORIENTED_EDGE ( 'NONE', *, *, #11620, .F. ) ;
#14214 = CARTESIAN_POINT ( 'NONE',  ( 0.7044674535452954967, 33.63530026269786788, -35.78364569253756144 ) ) ;
#14215 = CARTESIAN_POINT ( 'NONE',  ( 4.960386119450151732, 38.83699438620071476, 20.15252668323636698 ) ) ;
#14216 = FACE_OUTER_BOUND ( 'NONE', #380, .T. ) ;
#14217 = EDGE_LOOP ( 'NONE', ( #47564, #47976, #5902, #8030 ) ) ;
#14218 = CARTESIAN_POINT ( 'NONE',  ( 0.2500000000000002220, 0.000000000000000000, 0.000000000000000000 ) ) ;
#14219 = CARTESIAN_POINT ( 'NONE',  ( 0.9762797500689124330, -39.75277516423524560, 13.26806888463673673 ) ) ;
#14220 = ORIENTED_EDGE ( 'NONE', *, *, #31851, .F. ) ;
#14221 = EDGE_LOOP ( 'NONE', ( #7969, #58699, #1296, #54657 ) ) ;
#14222 = CARTESIAN_POINT ( 'NONE',  ( 5.959547316686252039, 18.96456592444100053, -7.851524054666214170 ) ) ;
#14223 = ORIENTED_EDGE ( 'NONE', *, *, #8706, .F. ) ;
#14224 = CARTESIAN_POINT ( 'NONE',  ( 0.6016118706126977189, 46.49486210791674523, 15.80439345086480429 ) ) ;
#14225 = CARTESIAN_POINT ( 'NONE',  ( -6.077587904424778920, -14.66646125808240164, -12.47761738310237334 ) ) ;
#14226 = CARTESIAN_POINT ( 'NONE',  ( -2.708315649062916552, -3.532515819624444831, 14.20182604343554189 ) ) ;
#14227 = DIRECTION ( 'NONE',  ( 0.000000000000000000, 0.000000000000000000, -1.000000000000000000 ) ) ;
#14228 = B_SPLINE_CURVE_WITH_KNOTS ( 'NONE', 3,
 ( #34135, #53811, #6188, #5273 ),
 .UNSPECIFIED., .F., .F.,
 ( 4, 4 ),
 ( 4.336808689942017736E-18, 0.004566006591234648970 ),
 .UNSPECIFIED. ) ;
#14229 = ORIENTED_EDGE ( 'NONE', *, *, #29356, .F. ) ;
#14230 = AXIS2_PLACEMENT_3D ( 'NONE', #30337, #2444, #21570 ) ;
#14231 = CARTESIAN_POINT ( 'NONE',  ( -6.010958268070873523, 0.01451635840163226568, 18.84344976839986785 ) ) ;
#14232 = EDGE_CURVE ( 'NONE', #3395, #48545, #51363, .T. ) ;
#14233 = AXIS2_PLACEMENT_3D ( 'NONE', #28059, #51850, #41252 ) ;
#14234 = FACE_OUTER_BOUND ( 'NONE', #34167, .T. ) ;
#14235 = ORIENTED_EDGE ( 'NONE', *, *, #29933, .F. ) ;
#14236 = LINE ( 'NONE', #18937, #28561 ) ;
#14237 = EDGE_CURVE ( 'NONE', #35972, #6137, #11095, .T. ) ;
#14238 = CARTESIAN_POINT ( 'NONE',  ( 5.283180000000047727, -15.43999999999999240, 1.890854657883513307E-15 ) ) ;
#14239 = CARTESIAN_POINT ( 'NONE',  ( 0.7245667037590747261, 38.65590879674347491, 28.62745028382829560 ) ) ;
#14240 = EDGE_CURVE ( 'NONE', #52565, #36974, #17669, .T. ) ;
#14241 = VERTEX_POINT ( 'NONE', #25795 ) ;
#14242 = ORIENTED_EDGE ( 'NONE', *, *, #33422, .F. ) ;
#14243 = CARTESIAN_POINT ( 'NONE',  ( 5.917102823773431552, -15.77849770028359444, 12.47111576298958546 ) ) ;
#14244 = EDGE_CURVE ( 'NONE', #25918, #14380, #40212, .T. ) ;
#14245 = CARTESIAN_POINT ( 'NONE',  ( 4.691466044806102076, 8.371234562541253865, 43.79545162262311919 ) ) ;
#14246 = CARTESIAN_POINT ( 'NONE',  ( 4.956653778116966613, 0.000000000000000000, 0.000000000000000000 ) ) ;
#14247 = CARTESIAN_POINT ( 'NONE',  ( 4.967162193818130511, 23.56777426397178132, 36.06913038482807821 ) ) ;
#14248 = CARTESIAN_POINT ( 'NONE',  ( 0.5797568665920715958, -20.30903389470142173, -42.27018394643840082 ) ) ;
#14249 = CARTESIAN_POINT ( 'NONE',  ( 0.9747592971366239034, -42.49794971112896036, 5.921534893733981342 ) ) ;
#14250 = CARTESIAN_POINT ( 'NONE',  ( 0.1310142868023724816, 40.08041389954882305, -15.91230901232182759 ) ) ;
#14251 = CARTESIAN_POINT ( 'NONE',  ( 4.975801465491694664, -35.64402118370934147, -32.01766832630300286 ) ) ;
#14252 = CARTESIAN_POINT ( 'NONE',  ( 3.660176727303384503, 45.87883389004768020, 14.24118031989607225 ) ) ;
#14253 = CARTESIAN_POINT ( 'NONE',  ( 4.967162193818130511, -2.375726030842872927, 43.02067033766017801 ) ) ;
#14254 = CARTESIAN_POINT ( 'NONE',  ( 0.9762797500689124330, 41.90547441298052433, -0.5059638413352701702 ) ) ;
#14255 = CARTESIAN_POINT ( 'NONE',  ( 1.227938101723756947, -0.8460948827222184443, -42.91134962331487657 ) ) ;
#14257 = ORIENTED_EDGE ( 'NONE', *, *, #35105, .T. ) ;
#14256 = ADVANCED_FACE ( 'NONE', ( #1972 ), #33599, .F. ) ;
#14258 = CARTESIAN_POINT ( 'NONE',  ( 0.8551540677456715978, 23.16399837394604688, -41.94570365541178347 ) ) ;
#14259 = LINE ( 'NONE', #53054, #46422 ) ;
#14261 = EDGE_CURVE ( 'NONE', #42525, #50188, #6517, .T. ) ;
#14260 = CARTESIAN_POINT ( 'NONE',  ( 0.7948884756798507700, -13.13616255639797181, -47.30898305704783979 ) ) ;
#14262 = LINE ( 'NONE', #19882, #41041 ) ;
#14263 = CARTESIAN_POINT ( 'NONE',  ( -6.078726893082806448, 7.797636468844896918, -17.60655862934208216 ) ) ;
#14264 = B_SPLINE_CURVE_WITH_KNOTS ( 'NONE', 3,
 ( #37329, #17917, #56403, #13519, #50180, #33869, #47333, #23517, #623, #9727 ),
 .UNSPECIFIED., .F., .F.,
 ( 4, 3, 3, 4 ),
 ( 0.0005448802484326158158, 0.0005449104342063607661, 0.0008173270854453680827, 0.001089761613562689226 ),
 .UNSPECIFIED. ) ;
#14265 = CARTESIAN_POINT ( 'NONE',  ( 0.5807400328401637335, 0.5448834511096761757, -47.89582301953902999 ) ) ;
#14266 = CARTESIAN_POINT ( 'NONE',  ( 5.880360259849739535, -47.87242051977163726, -3.090325311464695801 ) ) ;
#14267 = CARTESIAN_POINT ( 'NONE',  ( 0.6021447746440204973, 48.15123689037863386, -9.643626134143064021 ) ) ;
#14268 = CARTESIAN_POINT ( 'NONE',  ( 5.896782393890504181, 16.57826022845085134, 11.38803647148080778 ) ) ;
#14269 = LINE ( 'NONE', #42776, #9411 ) ;
#14271 = ORIENTED_EDGE ( 'NONE', *, *, #6040, .T. ) ;
#14270 = CARTESIAN_POINT ( 'NONE',  ( 0.6025881611877910160, -46.41131722377301116, -12.66175293297386162 ) ) ;
#14272 = EDGE_LOOP ( 'NONE', ( #15730, #43195, #29006, #53925 ) ) ;
#14273 = CARTESIAN_POINT ( 'NONE',  ( 4.694002226626921015, -25.79840873770003284, -37.58625916540110978 ) ) ;
#14274 = CARTESIAN_POINT ( 'NONE',  ( 0.1101816497532063510, 39.89358705406962002, 16.37745527993603289 ) ) ;
#14275 = CARTESIAN_POINT ( 'NONE',  ( 5.981074661064941900, -14.51919955600725842, -14.50705827991440877 ) ) ;
#14276 = VERTEX_POINT ( 'NONE', #2902 ) ;
#14277 = CARTESIAN_POINT ( 'NONE',  ( 0.5830081025819919827, 22.77654563688193079, 40.99342634171097188 ) ) ;
#14278 = CARTESIAN_POINT ( 'NONE',  ( 0.3622758884714600280, -29.89648521331609743, -31.06363466427717412 ) ) ;
#14279 = FACE_OUTER_BOUND ( 'NONE', #57246, .T. ) ;
#14280 = AXIS2_PLACEMENT_3D ( 'NONE', #33220, #60767, #56379 ) ;
#14281 = VECTOR ( 'NONE', #25378, 1000.000000000000114 ) ;
#14282 = ORIENTED_EDGE ( 'NONE', *, *, #57749, .F. ) ;
#14283 = VERTEX_POINT ( 'NONE', #40856 ) ;
#14284 = EDGE_CURVE ( 'NONE', #53979, #31908, #35765, .T. ) ;
#14285 = CARTESIAN_POINT ( 'NONE',  ( 4.322998006666165516, -30.86725474310387085, 36.74401119231355750 ) ) ;
#14286 = CARTESIAN_POINT ( 'NONE',  ( 0.8744876279028306332, -20.68330519280286239, -44.52584571550401193 ) ) ;
#14287 = CARTESIAN_POINT ( 'NONE',  ( 0.5835871038041848813, 16.98216052327276770, -43.71316365653826352 ) ) ;
#14288 = B_SPLINE_CURVE_WITH_KNOTS ( 'NONE', 3,
 ( #4426, #36769, #51139, #3828 ),
 .UNSPECIFIED., .F., .F.,
 ( 4, 4 ),
 ( 0.000000000000000000, 0.004445488388166995986 ),
 .UNSPECIFIED. ) ;
#14289 = CARTESIAN_POINT ( 'NONE',  ( 5.896782393890504181, -2.006887468070122527, -20.01245835894519587 ) ) ;
#14290 = DIRECTION ( 'NONE',  ( -1.000000000000000000, -1.836909530733573776E-16, 1.925929944387235853E-32 ) ) ;
#14291 = CARTESIAN_POINT ( 'NONE',  ( 5.960721111146673579, 2.672857320903031741, 20.35079619394246819 ) ) ;
#14292 = ORIENTED_EDGE ( 'NONE', *, *, #13447, .T. ) ;
#14293 = CARTESIAN_POINT ( 'NONE',  ( 4.956445790444002242, -36.61936279692601204, 29.60676136436992678 ) ) ;
#14294 = CARTESIAN_POINT ( 'NONE',  ( 5.901764892641288895, 19.78248028302103734, -44.79559064563790827 ) ) ;
#14295 = ORIENTED_EDGE ( 'NONE', *, *, #47110, .T. ) ;
#14296 = CARTESIAN_POINT ( 'NONE',  ( 0.9775691876210991227, -37.23235882800789653, -19.23759769546218834 ) ) ;
#14297 = CARTESIAN_POINT ( 'NONE',  ( -5.272380000000000067, 1.538011871406776419E-15, -12.55882000000000076 ) ) ;
#14298 = DIRECTION ( 'NONE',  ( 0.000000000000000000, 0.000000000000000000, 1.000000000000000000 ) ) ;
#14299 = CARTESIAN_POINT ( 'NONE',  ( 0.5998501479064708430, -6.798102206414489146, 47.62484632993676570 ) ) ;
#14300 = ORIENTED_EDGE ( 'NONE', *, *, #56980, .F. ) ;
#14301 = B_SPLINE_CURVE_WITH_KNOTS ( 'NONE', 3,
 ( #44957, #1995, #58384, #34309, #21121, #43729 ),
 .UNSPECIFIED., .F., .F.,
 ( 4, 2, 4 ),
 ( 5.637851296924623827E-18, 0.0002291472222819946974, 0.0004582944445639837569 ),
 .UNSPECIFIED. ) ;
#14302 = ORIENTED_EDGE ( 'NONE', *, *, #47729, .F. ) ;
#14303 = CARTESIAN_POINT ( 'NONE',  ( 5.959828726073459926, 7.858992891710142814, -18.96145866559664483 ) ) ;
#14304 = CARTESIAN_POINT ( 'NONE',  ( 0.9740398440564310700, -42.59352035928883140, -5.189371650077303499 ) ) ;
#14305 = CARTESIAN_POINT ( 'NONE',  ( 0.2224561200757640689, 25.64288022150836355, 34.66601556960360142 ) ) ;
#14306 = VERTEX_POINT ( 'NONE', #16399 ) ;
#14307 = CARTESIAN_POINT ( 'NONE',  ( 0.7056555295713317077, 41.89804573586738456, 23.21854706865595830 ) ) ;
#14308 = EDGE_CURVE ( 'NONE', #31693, #40643, #52928, .T. ) ;
#14309 = EDGE_LOOP ( 'NONE', ( #7424, #50025, #6792, #52169 ) ) ;
#14310 = FACE_OUTER_BOUND ( 'NONE', #26512, .T. ) ;
#14311 = CARTESIAN_POINT ( 'NONE',  ( 0.5837800304671210139, 27.78112706352523631, 37.78156046618196484 ) ) ;
#14312 = VERTEX_POINT ( 'NONE', #17331 ) ;
#14313 = CARTESIAN_POINT ( 'NONE',  ( 0.5839879882104920261, 5.827794150371782279E-15, 47.89596766822081264 ) ) ;
#14314 = ADVANCED_FACE ( 'NONE', ( #36452 ), #50218, .T. ) ;
#14315 = CARTESIAN_POINT ( 'NONE',  ( 0.1152339509894530906, -27.33595233401855396, 34.63651830723620151 ) ) ;
#14316 = PLANE ( 'NONE',  #4901 ) ;
#14317 = PRESENTATION_LAYER_ASSIGNMENT (  '', '', ( #25292 ) ) ;
#14318 = ORIENTED_EDGE ( 'NONE', *, *, #48453, .T. ) ;
#14319 = CARTESIAN_POINT ( 'NONE',  ( 0.5809828226811617480, -17.82437196699647686, -44.45562576850621639 ) ) ;
#14320 = DIRECTION ( 'NONE',  ( 0.000000000000000000, 0.000000000000000000, 1.000000000000000000 ) ) ;
#14321 = CARTESIAN_POINT ( 'NONE',  ( 5.917102823773431552, -19.39960706793701917, -5.305182717059805597 ) ) ;
#14322 = CARTESIAN_POINT ( 'NONE',  ( 0.6027935024548037868, 29.42425667880436180, -38.05972402498746732 ) ) ;
#14323 =( BOUNDED_SURFACE ( )  B_SPLINE_SURFACE ( 3, 1, ( 
 ( #9838, #14860 ),
 ( #6025, #25160 ),
 ( #53046, #53347 ),
 ( #15165, #15779 ) ),
 .UNSPECIFIED., .F., .F., .F. ) 
 B_SPLINE_SURFACE_WITH_KNOTS ( ( 4, 4 ),
 ( 2, 2 ),
 ( 0.000000000000000000, 1.000000000000000000 ),
 ( 0.000000000000000000, 1.000000000000000000 ),
 .UNSPECIFIED. ) 
 GEOMETRIC_REPRESENTATION_ITEM ( )  RATIONAL_B_SPLINE_SURFACE ( (
 ( 1.000000000000000000, 1.000000000000000000),
 ( 0.7223157951917476005, 0.9931996967497186413),
 ( 0.7223157951917476005, 0.9931996967497186413),
 ( 1.000000000000000000, 1.000000000000000000) ) ) 
 REPRESENTATION_ITEM ( '' )  SURFACE ( )  );
#14324 = CARTESIAN_POINT ( 'NONE',  ( 0.1102144999581333162, 16.61938362665549818, -39.79340763430492700 ) ) ;
#14325 = ORIENTED_EDGE ( 'NONE', *, *, #43960, .F. ) ;
#14326 = LINE ( 'NONE', #42838, #6653 ) ;
#14327 = CARTESIAN_POINT ( 'NONE',  ( 2.533389852662419894, -16.35873982657418679, 40.86370226766137392 ) ) ;
#14328 = EDGE_LOOP ( 'NONE', ( #55290, #20438, #55194, #17592 ) ) ;
#14329 = CARTESIAN_POINT ( 'NONE',  ( 0.5997462898726536595, -49.10477184366966696, 0.5225058138009974762 ) ) ;
#14330 = CARTESIAN_POINT ( 'NONE',  ( 5.901463166500145796, -19.93124146756672133, -2.695085138207230280 ) ) ;
#14332 = EDGE_CURVE ( 'NONE', #42831, #58372, #52665, .T. ) ;
#14331 = CARTESIAN_POINT ( 'NONE',  ( 2.624215991343608501, 4.864192649745388231, 47.76052319582218075 ) ) ;
#14333 = CARTESIAN_POINT ( 'NONE',  ( 3.783278058412225864, 35.16831859152132722, 24.80906179324452054 ) ) ;
#14334 = VECTOR ( 'NONE', #12965, 999.9999999999998863 ) ;
#14335 = B_SPLINE_CURVE_WITH_KNOTS ( 'NONE', 3,
 ( #52678, #9775, #61753, #27963 ),
 .UNSPECIFIED., .F., .F.,
 ( 4, 4 ),
 ( 0.000000000000000000, 0.004447772540403791171 ),
 .UNSPECIFIED. ) ;
#14336 = CARTESIAN_POINT ( 'NONE',  ( 0.8560838555295158248, -6.899551485031924614, -46.39794201672231111 ) ) ;
#14337 = CARTESIAN_POINT ( 'NONE',  ( 0.3676999524040366896, -40.57213187173863389, 17.31625533148228513 ) ) ;
#14338 = CARTESIAN_POINT ( 'NONE',  ( 51.35430322215398746, 15.29482815186059774, 2.514508868274447639 ) ) ;
#14339 = CARTESIAN_POINT ( 'NONE',  ( 1.154321713695927620, -41.66001467525148172, 10.30834583266716287 ) ) ;
#14340 = CARTESIAN_POINT ( 'NONE',  ( 4.975801465491694664, -9.906103548668557579, 46.87746200127438101 ) ) ;
#14341 = CARTESIAN_POINT ( 'NONE',  ( 0.5807400328401574052, -46.12278621143506996, 12.92266817605998419 ) ) ;
#14343 = ORIENTED_EDGE ( 'NONE', *, *, #45623, .T. ) ;
#14342 = CARTESIAN_POINT ( 'NONE',  ( 1.827119703190777988, 20.44859290426037646, -37.88337895042275250 ) ) ;
#14344 = EDGE_LOOP ( 'NONE', ( #23068, #20968, #37167, #30496 ) ) ;
#14345 = CARTESIAN_POINT ( 'NONE',  ( 5.981074661064941900, -10.26976685693835556, 17.77058762078859999 ) ) ;
#14346 = CARTESIAN_POINT ( 'NONE',  ( 4.956445790444004018, -43.14021684453488348, -18.88014143872194950 ) ) ;
#14347 = CARTESIAN_POINT ( 'NONE',  ( 0.7954196712028469562, -48.09103417491925114, -0.8690072546823950361 ) ) ;
#14348 = CARTESIAN_POINT ( 'NONE',  ( 0.1313383488274136590, 17.09007684155447748, 39.59253935480806064 ) ) ;
#14349 = CARTESIAN_POINT ( 'NONE',  ( 0.5998501479064699549, -41.92175333043603302, -23.59887241503339439 ) ) ;
#14350 = ORIENTED_EDGE ( 'NONE', *, *, #47556, .T. ) ;
#14351 = EDGE_CURVE ( 'NONE', #57783, #17208, #30793, .T. ) ;
#14352 = CARTESIAN_POINT ( 'NONE',  ( 2.624215991343620935, -44.87417713512076745, -17.05978231157451219 ) ) ;
#14353 = DIRECTION ( 'NONE',  ( -0.07906939808003035641, 0.9635513351855523601, 0.2555716235214721688 ) ) ;
#14354 = FACE_OUTER_BOUND ( 'NONE', #39470, .T. ) ;
#14355 = VERTEX_POINT ( 'NONE', #2276 ) ;
#14356 = B_SPLINE_CURVE_WITH_KNOTS ( 'NONE', 3,
 ( #49925, #54596, #12048, #30804 ),
 .UNSPECIFIED., .F., .F.,
 ( 4, 4 ),
 ( 0.000000000000000000, 0.005014147105413707325 ),
 .UNSPECIFIED. ) ;
#14357 = MECHANICAL_DESIGN_GEOMETRIC_PRESENTATION_REPRESENTATION (  '', ( #40395 ), #35380 ) ;
#14358 = EDGE_CURVE ( 'NONE', #35248, #15688, #18548, .T. ) ;
#14359 = CARTESIAN_POINT ( 'NONE',  ( 2.624215991343620935, 30.33228621715034734, 37.21129343241614151 ) ) ;
#14360 = CARTESIAN_POINT ( 'NONE',  ( 3.782542959838393504, -19.24495247062706227, 37.37471950128691134 ) ) ;
#14361 = ORIENTED_EDGE ( 'NONE', *, *, #8954, .T. ) ;
#14362 = EDGE_CURVE ( 'NONE', #40053, #25757, #27685, .T. ) ;
#14363 = PLANE ( 'NONE',  #14008 ) ;
#14364 = ORIENTED_EDGE ( 'NONE', *, *, #10075, .F. ) ;
#14365 = CARTESIAN_POINT ( 'NONE',  ( -6.015611763856276717, -13.32857883366824048, -13.31979030221813254 ) ) ;
#14366 = DIRECTION ( 'NONE',  ( 1.000000000000000000, 0.000000000000000000, 0.000000000000000000 ) ) ;
#14367 = EDGE_LOOP ( 'NONE', ( #45121, #21987, #57890, #858 ) ) ;
#14368 = CARTESIAN_POINT ( 'NONE',  ( 4.960386119450151732, 28.60674280242284695, -33.10726099979230241 ) ) ;
#14369 = CARTESIAN_POINT ( 'NONE',  ( 5.895596859100789899, -4.666058297670689470, 19.56415301451167466 ) ) ;
#14370 = DIRECTION ( 'NONE',  ( 0.1024043820194936311, -0.9878630899050863112, -0.1167898032637303823 ) ) ;
#14371 = CARTESIAN_POINT ( 'NONE',  ( 4.963659409799330291, 39.92545197189549100, 20.22157859941743752 ) ) ;
#14372 = VERTEX_POINT ( 'NONE', #26718 ) ;
#14373 = B_SPLINE_CURVE_WITH_KNOTS ( 'NONE', 3,
 ( #51412, #55498, #12625, #50807, #7897, #36744, #46141, #8502, #55812, #60500, #42068, #32646, #61122, #8826, #7574, #17617 ),
 .UNSPECIFIED., .F., .F.,
 ( 4, 3, 3, 3, 3, 4 ),
 ( 2.221635811791082109E-17, 0.0002612764279487765238, 0.0003919131003184790824, 0.0005225497727000667737, 0.0007837925190632461132, 0.001045051706266717818 ),
 .UNSPECIFIED. ) ;
#14374 = CARTESIAN_POINT ( 'NONE',  ( 0.5326698147273788431, 5.129895114339477383E-15, 41.88877248453276536 ) ) ;
#14376 = ORIENTED_EDGE ( 'NONE', *, *, #16934, .F. ) ;
#14375 =( BOUNDED_SURFACE ( )  B_SPLINE_SURFACE ( 3, 1, ( 
 ( #56644, #13766 ),
 ( #51946, #44138 ),
 ( #48480, #24684 ),
 ( #29376, #30296 ) ),
 .UNSPECIFIED., .F., .F., .F. ) 
 B_SPLINE_SURFACE_WITH_KNOTS ( ( 4, 4 ),
 ( 2, 2 ),
 ( 0.000000000000000000, 1.000000000000000000 ),
 ( 0.000000000000000000, 1.000000000000000000 ),
 .UNSPECIFIED. ) 
 GEOMETRIC_REPRESENTATION_ITEM ( )  RATIONAL_B_SPLINE_SURFACE ( (
 ( 1.000000000000000000, 1.000000000000000000),
 ( 0.7282232189291693025, 0.9929344683865674037),
 ( 0.7282232189291693025, 0.9929344683865674037),
 ( 1.000000000000000000, 1.000000000000000000) ) ) 
 REPRESENTATION_ITEM ( '' )  SURFACE ( )  );
#14377 = CARTESIAN_POINT ( 'NONE',  ( 0.7056313189692680066, -39.13839767847387208, -25.84442824129003569 ) ) ;
#14378 = ORIENTED_EDGE ( 'NONE', *, *, #53926, .F. ) ;
#14379 = ADVANCED_FACE ( 'NONE', ( #46161 ), #48767, .F. ) ;
#14380 = VERTEX_POINT ( 'NONE', #51131 ) ;
#14381 = CARTESIAN_POINT ( 'NONE',  ( 4.962356264823603702, -4.645793755590432283, -41.82884409403234116 ) ) ;
#14382 = CARTESIAN_POINT ( 'NONE',  ( 0.9790320750461896093, -37.44297633391666835, 18.82446960208836728 ) ) ;
#14383 = CARTESIAN_POINT ( 'NONE',  ( 0.2224561200757590174, 20.89867881469716338, 37.71651051365635254 ) ) ;
#14384 = CARTESIAN_POINT ( 'NONE',  ( 0.7413678028165009426, -28.21704311592099756, -33.88634783455570698 ) ) ;
#14385 = ORIENTED_EDGE ( 'NONE', *, *, #26487, .F. ) ;
#14386 = CARTESIAN_POINT ( 'NONE',  ( 0.9730545539215883499, 0.5054011016618756846, -42.90536227157002003 ) ) ;
#14387 = EDGE_CURVE ( 'NONE', #61878, #39018, #28258, .T. ) ;
#14388 = DIRECTION ( 'NONE',  ( 0.000000000000000000, 0.000000000000000000, -1.000000000000000000 ) ) ;
#14389 = CARTESIAN_POINT ( 'NONE',  ( 0.5807400328401637335, -38.33001520688930697, -28.72484455891680710 ) ) ;
#14390 = VERTEX_POINT ( 'NONE', #22646 ) ;
#14391 = EDGE_CURVE ( 'NONE', #2006, #16817, #27528, .T. ) ;
#14392 = VERTEX_POINT ( 'NONE', #22960 ) ;
#14393 =( BOUNDED_SURFACE ( )  B_SPLINE_SURFACE ( 3, 1, ( 
 ( #39169, #6207 ),
 ( #29734, #44188 ),
 ( #43249, #20658 ),
 ( #1218, #20353 ) ),
 .UNSPECIFIED., .F., .F., .F. ) 
 B_SPLINE_SURFACE_WITH_KNOTS ( ( 4, 4 ),
 ( 2, 2 ),
 ( 0.000000000000000000, 1.000000000000000000 ),
 ( 0.000000000000000000, 1.000000000000000000 ),
 .UNSPECIFIED. ) 
 GEOMETRIC_REPRESENTATION_ITEM ( )  RATIONAL_B_SPLINE_SURFACE ( (
 ( 1.000000000000000000, 1.000000000000000000),
 ( 0.7282232189291693025, 0.9929344683865674037),
 ( 0.7282232189291693025, 0.9929344683865674037),
 ( 1.000000000000000000, 1.000000000000000000) ) ) 
 REPRESENTATION_ITEM ( '' )  SURFACE ( )  );
#14394 = CARTESIAN_POINT ( 'NONE',  ( 1.154321713695929619, 17.18284946700681104, -39.32643513900308108 ) ) ;
#14395 = CARTESIAN_POINT ( 'NONE',  ( -6.072942160501519915, -6.664073831083357824, -18.06638542329068642 ) ) ;
#14396 = CARTESIAN_POINT ( 'NONE',  ( 0.1102847568649952675, 30.55869130182067295, 30.42833243501160823 ) ) ;
#14397 = CARTESIAN_POINT ( 'NONE',  ( -6.072942160501519915, -17.35560219702253093, -8.341896347217875984 ) ) ;
#14398 = DIRECTION ( 'NONE',  ( 0.09722883295013594329, -0.5094590954038252795, 0.8549842011133718112 ) ) ;
#14399 = ORIENTED_EDGE ( 'NONE', *, *, #28496, .F. ) ;
#14400 = VERTEX_POINT ( 'NONE', #18563 ) ;
#14401 = CARTESIAN_POINT ( 'NONE',  ( 1.399999999999998579, 0.000000000000000000, 0.000000000000000000 ) ) ;
#14403 = EDGE_CURVE ( 'NONE', #27021, #60419, #48385, .T. ) ;
#14402 = CARTESIAN_POINT ( 'NONE',  ( 0.9789889208857702751, -41.04960742935966067, 8.441837947854031299 ) ) ;
#14404 = DIRECTION ( 'NONE',  ( 0.09722883295013594329, -0.02434548463873833016, 0.9949642463027802419 ) ) ;
#14405 = AXIS2_PLACEMENT_3D ( 'NONE', #57657, #42685, #43003 ) ;
#14406 = CARTESIAN_POINT ( 'NONE',  ( 1.231276596079887264, 41.65019306089983786, 4.747440258480190245 ) ) ;
#14407 = CARTESIAN_POINT ( 'NONE',  ( 0.8557997880470599172, 11.51622788066458369, 46.50333260518563350 ) ) ;
#14408 = PRESENTATION_STYLE_ASSIGNMENT (( #58209 ) ) ;
#14409 = CARTESIAN_POINT ( 'NONE',  ( 0.6009452777970413218, 0.4363873594205723294, 48.10564074251961841 ) ) ;
#14410 = VERTEX_POINT ( 'NONE', #60838 ) ;
#14411 = CARTESIAN_POINT ( 'NONE',  ( 0.2885697896453118805, 34.69058521462536504, -25.60460893337440780 ) ) ;
#14412 = CARTESIAN_POINT ( 'NONE',  ( 0.9762797500689124330, -39.75277516423524560, 13.26806888463673673 ) ) ;
#14413 = CARTESIAN_POINT ( 'NONE',  ( 0.8554163680231720024, -6.900908941297191568, 46.40671211038057464 ) ) ;
#14414 = CARTESIAN_POINT ( 'NONE',  ( 5.896278296736517710, 20.06830682785022191, 1.337924017888904471 ) ) ;
#14415 = CARTESIAN_POINT ( 'NONE',  ( 0.9754292580325137907, -41.77202903244706533, -3.380097249548380756 ) ) ;
#14416 = CARTESIAN_POINT ( 'NONE',  ( 0.9790724872846782167, -34.57410215488273764, 23.68473496083889529 ) ) ;
#14417 = AXIS2_PLACEMENT_3D ( 'NONE', #36880, #27765, #18066 ) ;
#14418 = CARTESIAN_POINT ( 'NONE',  ( 5.958863334805807099, 20.34989385289154029, 2.680345151634683454 ) ) ;
#14419 = B_SPLINE_CURVE_WITH_KNOTS ( 'NONE', 3,
 ( #821, #52510, #61892, #29630, #19955, #9294, #23713, #14636, #15248, #19032, #38147, #57192, #14327, #34354, #9598, #28716, #47840, #5802, #24952, #38446, #44088, #4885, #24018, #43147, #18711 ),
 .UNSPECIFIED., .F., .F.,
 ( 4, 3, 3, 3, 3, 3, 3, 3, 4 ),
 ( 3.878959614448864246E-18, 0.0005656085177311386642, 0.001131215744874498972, 0.001696821861372764615, 0.002262427090022496416, 0.002828031679238744624, 0.003393635864401603561, 0.003977030878808131623, 0.004561030005651159000 ),
 .UNSPECIFIED. ) ;
#14420 = CARTESIAN_POINT ( 'NONE',  ( 5.901764892641288895, 30.56558498815964242, 38.25880920482585879 ) ) ;
#14421 = VERTEX_POINT ( 'NONE', #18886 ) ;
#14422 = ADVANCED_FACE ( 'NONE', ( #46465 ), #26654, .T. ) ;
#14423 = CARTESIAN_POINT ( 'NONE',  ( 1.227938101723748288, -10.28900963485351205, -41.66816631169202623 ) ) ;
#14424 = CARTESIAN_POINT ( 'NONE',  ( 0.8557997880470606944, 47.37054680076706603, 7.156447707085862753 ) ) ;
#14425 = CARTESIAN_POINT ( 'NONE',  ( 0.5980894510889457338, 13.12879507229223819, 46.28687279963696710 ) ) ;
#14426 = CARTESIAN_POINT ( 'NONE',  ( 0.5998501479064699549, -23.59887241503383493, 41.92175333043579144 ) ) ;
#14427 = ORIENTED_EDGE ( 'NONE', *, *, #58145, .F. ) ;
#14428 = EDGE_CURVE ( 'NONE', #61565, #44407, #31979, .T. ) ;
#14429 = CARTESIAN_POINT ( 'NONE',  ( -2.708315649062910779, 14.20182604343559873, -3.532515819624206799 ) ) ;
#14430 = CARTESIAN_POINT ( 'NONE',  ( 0.5848930533535030563, 11.04862722691790999, 45.57631971526624426 ) ) ;
#14431 = ADVANCED_FACE ( 'NONE', ( #3510 ), #29551, .F. ) ;
#14432 = CARTESIAN_POINT ( 'NONE',  ( -6.072942160501519027, -6.636811946999439549, -18.07641804863966684 ) ) ;
#14433 = VERTEX_POINT ( 'NONE', #37373 ) ;
#14434 = CARTESIAN_POINT ( 'NONE',  ( 4.975610109902397937, -33.30777373088848492, -35.81957029655308133 ) ) ;
#14435 = EDGE_CURVE ( 'NONE', #42430, #16350, #40994, .T. ) ;
#14436 = CARTESIAN_POINT ( 'NONE',  ( 1.091591847532195070, 25.48625600094100818, -33.27476139674539013 ) ) ;
#14437 = ORIENTED_EDGE ( 'NONE', *, *, #42818, .F. ) ;
#14438 = CARTESIAN_POINT ( 'NONE',  ( 4.956445790444002242, -37.28933980949966553, 28.75835855384135087 ) ) ;
#14439 = ORIENTED_EDGE ( 'NONE', *, *, #39008, .T. ) ;
#14440 = CARTESIAN_POINT ( 'NONE',  ( 4.694002226626921015, 42.38457918174899675, 16.78785927485048646 ) ) ;
#14441 = VERTEX_POINT ( 'NONE', #4122 ) ;
#14442 = CARTESIAN_POINT ( 'NONE',  ( 0.8744876279028306332, 16.11801507201633399, -46.37412684372340266 ) ) ;
#14443 = CARTESIAN_POINT ( 'NONE',  ( 0.000000000000000000, 0.000000000000000000, -5.574599999999999334 ) ) ;
#14444 = VERTEX_POINT ( 'NONE', #56753 ) ;
#14445 = CARTESIAN_POINT ( 'NONE',  ( -14.84250595937557549, -4.999999999999997335, -10.00000000000000711 ) ) ;
#14446 = AXIS2_PLACEMENT_3D ( 'NONE', #17335, #51138, #37378 ) ;
#14447 = EDGE_LOOP ( 'NONE', ( #34858, #46504, #3858, #5587 ) ) ;
#14448 = DIRECTION ( 'NONE',  ( 0.09722883295013594329, 0.9936727386027179865, -0.05622315004452352327 ) ) ;
#14449 = B_SPLINE_CURVE_WITH_KNOTS ( 'NONE', 3,
 ( #61485, #23302, #42427, #57705, #9814, #57098, #33636, #18608, #56795, #28604, #13925, #33028, #48037 ),
 .UNSPECIFIED., .F., .F.,
 ( 4, 3, 3, 3, 4 ),
 ( 0.0005054209210073039738, 0.0005449106435901839799, 0.0006811373090491489642, 0.0008459866663933692660, 0.001010840725717212932 ),
 .UNSPECIFIED. ) ;
#14450 = CARTESIAN_POINT ( 'NONE',  ( 0.6041374136657475802, 46.42299778158138679, 12.61972904329615197 ) ) ;
#14451 = EDGE_CURVE ( 'NONE', #58203, #44946, #59575, .T. ) ;
#14452 = ORIENTED_EDGE ( 'NONE', *, *, #38922, .F. ) ;
#14453 = CARTESIAN_POINT ( 'NONE',  ( 0.8554163680231708922, 46.36773742900841455, 7.158100224665131073 ) ) ;
#14454 = CARTESIAN_POINT ( 'NONE',  ( 5.959547316686252039, -7.851524054666280783, -18.96456592444097922 ) ) ;
#14455 = CARTESIAN_POINT ( 'NONE',  ( 0.1155031312995260795, -22.72937730850169302, -37.81953251561390061 ) ) ;
#14456 = ORIENTED_EDGE ( 'NONE', *, *, #37789, .F. ) ;
#14457 = EDGE_CURVE ( 'NONE', #34231, #10639, #34202, .T. ) ;
#14458 = CARTESIAN_POINT ( 'NONE',  ( 0.6041374136657476912, -24.20487816031493367, -41.57494627055135794 ) ) ;
#14459 = LINE ( 'NONE', #47967, #41933 ) ;
#14460 = AXIS2_PLACEMENT_3D ( 'NONE', #3190, #13542, #32647 ) ;
#14461 = ORIENTED_EDGE ( 'NONE', *, *, #9784, .F. ) ;
#14462 = CARTESIAN_POINT ( 'NONE',  ( 5.860006189529234355, 40.09484204000635543, -26.81109398084667106 ) ) ;
#14463 = EDGE_CURVE ( 'NONE', #58483, #9846, #14795, .T. ) ;
#14464 = VERTEX_POINT ( 'NONE', #44248 ) ;
#14465 = CARTESIAN_POINT ( 'NONE',  ( 0.8760168074886965917, -46.22580377597776646, -13.30888447662064777 ) ) ;
#14466 = DIRECTION ( 'NONE',  ( 0.000000000000000000, 0.000000000000000000, 1.000000000000000000 ) ) ;
#14467 = ORIENTED_EDGE ( 'NONE', *, *, #9540, .T. ) ;
#14468 = CARTESIAN_POINT ( 'NONE',  ( 5.895881250540457863, -17.30746725809826358, -10.24593864505140317 ) ) ;
#14469 = CARTESIAN_POINT ( 'NONE',  ( 0.6000166863083090663, 33.40185771989251862, 36.00193581696004230 ) ) ;
#14470 = DIRECTION ( 'NONE',  ( -1.000000000000000000, -0.000000000000000000, -0.000000000000000000 ) ) ;
#14471 = CARTESIAN_POINT ( 'NONE',  ( 0.9783242366443549720, -22.32385813646210693, -35.46801161764835086 ) ) ;
#14472 = ORIENTED_EDGE ( 'NONE', *, *, #5959, .F. ) ;
#14473 = CARTESIAN_POINT ( 'NONE',  ( -6.016761891674564211, -18.68243340030201338, -2.456125503350905959 ) ) ;
#14474 = CARTESIAN_POINT ( 'NONE',  ( 0.6253024248130498730, -26.04123622408341276, 41.63289856999066529 ) ) ;
#14476 = EDGE_CURVE ( 'NONE', #43532, #18131, #31182, .T. ) ;
#14475 = CARTESIAN_POINT ( 'NONE',  ( 5.974727161628367256, -10.24903993265021285, 17.78288073588484863 ) ) ;
#14477 = CARTESIAN_POINT ( 'NONE',  ( 4.975801465491694664, -21.70134120755230711, 42.71626295676225027 ) ) ;
#14478 = CARTESIAN_POINT ( 'NONE',  ( 0.5807400328401574052, 38.33001520688988961, -28.72484455891602906 ) ) ;
#14479 = EDGE_CURVE ( 'NONE', #4083, #25777, #57344, .T. ) ;
#14480 = CONICAL_SURFACE ( 'NONE', #12469, 42.08604991992415023, 1.569615340895231137 ) ;
#14481 = CARTESIAN_POINT ( 'NONE',  ( 3.050102900204245682, -8.802340948619855610, -43.10387503464520620 ) ) ;
#14482 = CARTESIAN_POINT ( 'NONE',  ( 0.5997462898726536595, 46.76781179977606229, 14.97743000668126001 ) ) ;
#14483 = CARTESIAN_POINT ( 'NONE',  ( 0.9775691876210985676, -12.77678863225218286, 39.91349873459780895 ) ) ;
#14484 = CARTESIAN_POINT ( 'NONE',  ( 0.3622758884714600280, -22.26738722580193652, 36.91764744403282350 ) ) ;
#14485 =( BOUNDED_SURFACE ( )  B_SPLINE_SURFACE ( 3, 1, ( 
 ( #61402, #19153 ),
 ( #42347, #12 ),
 ( #9413, #5316 ),
 ( #10047, #33250 ) ),
 .UNSPECIFIED., .F., .F., .F. ) 
 B_SPLINE_SURFACE_WITH_KNOTS ( ( 4, 4 ),
 ( 2, 2 ),
 ( 0.000000000000000000, 1.000000000000000000 ),
 ( 0.000000000000000000, 1.000000000000000000 ),
 .UNSPECIFIED. ) 
 GEOMETRIC_REPRESENTATION_ITEM ( )  RATIONAL_B_SPLINE_SURFACE ( (
 ( 1.000000000000000000, 1.000000000000000000),
 ( 0.7269869731126821222, 0.9931720237060910339),
 ( 0.7269869731126821222, 0.9931720237060910339),
 ( 1.000000000000000000, 1.000000000000000000) ) ) 
 REPRESENTATION_ITEM ( '' )  SURFACE ( )  );
#14486 = CARTESIAN_POINT ( 'NONE',  ( 0.6031357023905875581, 48.10744334619843698, 0.04361601114929824358 ) ) ;
#14487 = CARTESIAN_POINT ( 'NONE',  ( 2.500000000000000000, -2.357898499370432166, 3.035766082959412415E-15 ) ) ;
#14488 = CARTESIAN_POINT ( 'NONE',  ( 0.1152809850208375841, 39.65805943382677867, 19.34382600296067878 ) ) ;
#14489 = CARTESIAN_POINT ( 'NONE',  ( 4.958415959904820092, 2.023024899603357074, -45.37743188059707222 ) ) ;
#14490 = CARTESIAN_POINT ( 'NONE',  ( 0.5836750258453353712, -23.79054009282519289, -41.56963612796212004 ) ) ;
#14491 = CARTESIAN_POINT ( 'NONE',  ( 1.500000000000001332, 0.000000000000000000, 0.000000000000000000 ) ) ;
#14492 = CIRCLE ( 'NONE', #46468, 47.09074272231896430 ) ;
#14493 = CARTESIAN_POINT ( 'NONE',  ( 0.5782707292762442330, 11.57561326132714363, -45.45042938556033363 ) ) ;
#14494 = CARTESIAN_POINT ( 'NONE',  ( 0.9722240750034564227, 34.39263040572789265, 25.65687433776909643 ) ) ;
#14495 = ORIENTED_EDGE ( 'NONE', *, *, #13610, .T. ) ;
#14496 = CARTESIAN_POINT ( 'NONE',  ( 3.678834586032787790, -43.55038525248056658, 22.40482791696642195 ) ) ;
#14497 = VECTOR ( 'NONE', #37231, 1000.000000000000114 ) ;
#14498 = CARTESIAN_POINT ( 'NONE',  ( 0.7948884756798513251, 5.577371174960814137, -48.78105754672471761 ) ) ;
#14499 = CARTESIAN_POINT ( 'NONE',  ( 4.956445790444011124, -11.44166143951963122, -45.67960632101645757 ) ) ;
#14500 = EDGE_LOOP ( 'NONE', ( #6849, #59080, #32087, #39544 ) ) ;
#14501 = EDGE_CURVE ( 'NONE', #1609, #59890, #34518, .T. ) ;
#14502 = CARTESIAN_POINT ( 'NONE',  ( 0.9756950546413931669, 5.696573146291977530, 42.52863374229711013 ) ) ;
#14503 = CIRCLE ( 'NONE', #22498, 42.92674063221959813 ) ;
#14504 = CARTESIAN_POINT ( 'NONE',  ( 0.7044674535452954967, -39.85538961151654291, 28.69408722585759719 ) ) ;
#14505 = ADVANCED_FACE ( 'NONE', ( #44554 ), #23518, .F. ) ;
#14506 = VERTEX_POINT ( 'NONE', #30105 ) ;
#14507 = ORIENTED_EDGE ( 'NONE', *, *, #27677, .T. ) ;
#14508 = PLANE ( 'NONE',  #43569 ) ;
#14509 = ADVANCED_FACE ( 'NONE', ( #53588 ), #38369, .F. ) ;
#14510 = EDGE_LOOP ( 'NONE', ( #35956, #30927, #48126, #41007 ) ) ;
#14511 = EDGE_CURVE ( 'NONE', #5679, #26211, #32661, .T. ) ;
#14512 = CARTESIAN_POINT ( 'NONE',  ( 2.299746137290199055, 47.86635935193019264, -10.63451832844456746 ) ) ;
#14513 = EDGE_CURVE ( 'NONE', #53665, #1366, #21539, .T. ) ;
#14514 = ORIENTED_EDGE ( 'NONE', *, *, #26883, .T. ) ;
#14515 = EDGE_LOOP ( 'NONE', ( #37509, #29201, #8730, #49541 ) ) ;
#14516 = CARTESIAN_POINT ( 'NONE',  ( 0.6000166863083106206, 44.01764848084281567, -21.77774331572052802 ) ) ;
#14517 = ORIENTED_EDGE ( 'NONE', *, *, #8397, .T. ) ;
#14518 = CARTESIAN_POINT ( 'NONE',  ( 4.975801465491694664, -20.67815041659109809, -43.22084481528213473 ) ) ;
#14519 = CARTESIAN_POINT ( 'NONE',  ( -6.010958268070873523, 11.48268200989196863, 14.94067681728554042 ) ) ;
#14520 = CARTESIAN_POINT ( 'NONE',  ( 0.1084644655670282398, -30.77359411724706106, -30.21121552070987448 ) ) ;
#14521 = ORIENTED_EDGE ( 'NONE', *, *, #7461, .T. ) ;
#14522 = CARTESIAN_POINT ( 'NONE',  ( 5.960721111146673579, -10.25731071096570268, -17.77882586010663246 ) ) ;
#14523 = CIRCLE ( 'NONE', #36529, 47.67072199303260049 ) ;
#14524 = EDGE_CURVE ( 'NONE', #24124, #43366, #34672, .T. ) ;
#14525 = B_SPLINE_CURVE_WITH_KNOTS ( 'NONE', 3,
 ( #12821, #18430, #56006, #55686 ),
 .UNSPECIFIED., .F., .F.,
 ( 4, 4 ),
 ( 2.301370753934467307E-17, 0.004559932413162187670 ),
 .UNSPECIFIED. ) ;
#14526 = CARTESIAN_POINT ( 'NONE',  ( 0.9756950546413944991, -34.10037081504538037, -26.04419981250922689 ) ) ;
#14527 = VERTEX_POINT ( 'NONE', #12573 ) ;
#14528 = EDGE_LOOP ( 'NONE', ( #31221, #40275, #53163, #47948 ) ) ;
#14529 = LINE ( 'NONE', #28913, #19593 ) ;
#14530 = ORIENTED_EDGE ( 'NONE', *, *, #50030, .F. ) ;
#14531 = CARTESIAN_POINT ( 'NONE',  ( 3.894904216938897434, 34.86916712789552975, 26.76313726533365767 ) ) ;
#14532 = CARTESIAN_POINT ( 'NONE',  ( -6.016104459813374383, -2.464823636987575117, 18.68131780085930771 ) ) ;
#14533 = LINE ( 'NONE', #18927, #6571 ) ;
#14534 = CARTESIAN_POINT ( 'NONE',  ( 0.1087620492084205304, 5.269740196867345183, 42.80136086877935497 ) ) ;
#14535 = VERTEX_POINT ( 'NONE', #21647 ) ;
#14536 = CARTESIAN_POINT ( 'NONE',  ( 1.827326673878744367, 20.44853789448401216, 37.88339879236866636 ) ) ;
#14537 = CARTESIAN_POINT ( 'NONE',  ( 2.299652685299200972, 33.90758011679142925, -35.41973652473327405 ) ) ;
#14538 = B_SPLINE_CURVE_WITH_KNOTS ( 'NONE', 3,
 ( #23022, #36824, #13017, #3568 ),
 .UNSPECIFIED., .F., .F.,
 ( 4, 4 ),
 ( 0.000000000000000000, 0.005014147105413707325 ),
 .UNSPECIFIED. ) ;
#14539 = FACE_OUTER_BOUND ( 'NONE', #29948, .T. ) ;
#14540 = B_SPLINE_CURVE_WITH_KNOTS ( 'NONE', 3,
 ( #53098, #38415, #53695, #9894 ),
 .UNSPECIFIED., .F., .F.,
 ( 4, 4 ),
 ( 0.000000000000000000, 0.004442905043737213969 ),
 .UNSPECIFIED. ) ;
#14541 = CIRCLE ( 'NONE', #21497, 2.041999999999999815 ) ;
#14542 = ORIENTED_EDGE ( 'NONE', *, *, #29380, .F. ) ;
#14543 = CARTESIAN_POINT ( 'NONE',  ( 0.6067099128993197477, -38.42667919752384620, -28.59222530349265412 ) ) ;
#14544 = CARTESIAN_POINT ( 'NONE',  ( 2.648799415243708655, -31.64453936086600194, -37.45851828260430239 ) ) ;
#14545 = CARTESIAN_POINT ( 'NONE',  ( 0.5998501479064708430, -44.24259072156073813, -18.89267974119652749 ) ) ;
#14547 = ORIENTED_EDGE ( 'NONE', *, *, #23645, .T. ) ;
#14546 = CIRCLE ( 'NONE', #49529, 48.91267123290010943 ) ;
#14548 = ORIENTED_EDGE ( 'NONE', *, *, #52104, .T. ) ;
#14549 = CARTESIAN_POINT ( 'NONE',  ( 0.2885697896453121580, 37.73587455644747735, -20.85752796052974389 ) ) ;
#14550 = CARTESIAN_POINT ( 'NONE',  ( 0.5809828226811553087, -46.11980934799348830, 12.92184523170186594 ) ) ;
#14551 = AXIS2_PLACEMENT_3D ( 'NONE', #41190, #55244, #12372 ) ;
#14553 = EDGE_CURVE ( 'NONE', #8991, #7406, #20004, .T. ) ;
#14552 = CARTESIAN_POINT ( 'NONE',  ( 5.895881250540457863, -11.93421320881311232, 16.18957185026495793 ) ) ;
#14554 = CARTESIAN_POINT ( 'NONE',  ( 0.5848930533535030563, -44.36099898510374118, -15.21101086158259541 ) ) ;
#14555 = CARTESIAN_POINT ( 'NONE',  ( 0.1158816050234199313, -17.86592162500884839, -40.34539485237691991 ) ) ;
#14556 = CARTESIAN_POINT ( 'NONE',  ( 0.3622758884714600280, -33.69533458712325569, -26.89560658783373626 ) ) ;
#14557 = CARTESIAN_POINT ( 'NONE',  ( 0.8557997880470599172, 47.60865952217007191, -5.347802024196765203 ) ) ;
#14558 = EDGE_CURVE ( 'NONE', #19604, #41057, #5601, .T. ) ;
#14559 = CARTESIAN_POINT ( 'NONE',  ( 0.1310142868023716767, 42.83311553787493864, -4.996535778098907699 ) ) ;
#14560 = CARTESIAN_POINT ( 'NONE',  ( 4.303969348037246512, -47.36875205922767407, -8.413118729224548176 ) ) ;
#14561 = CARTESIAN_POINT ( 'NONE',  ( 0.5998501479064708430, -17.92509395669076966, -44.64337787626241294 ) ) ;
#14562 = CARTESIAN_POINT ( 'NONE',  ( 2.526552050251863246, -22.53110080776681556, 36.59987178591175194 ) ) ;
#14563 = ORIENTED_EDGE ( 'NONE', *, *, #2332, .T. ) ;
#14564 = CARTESIAN_POINT ( 'NONE',  ( -6.016761891674564211, -9.424569481870138432, -16.31696541414282109 ) ) ;
#14565 = CARTESIAN_POINT ( 'NONE',  ( 0.6028777368367060907, 41.10879128012145856, 26.86274574198404963 ) ) ;
#14566 = CARTESIAN_POINT ( 'NONE',  ( -6.078457390727109555, -8.902764005229952815, 17.07440494145227561 ) ) ;
#14567 = CARTESIAN_POINT ( 'NONE',  ( 4.975610109902397937, -47.89734868211972696, -9.914302615979444511 ) ) ;
#14568 = FACE_OUTER_BOUND ( 'NONE', #38594, .T. ) ;
#14569 = CARTESIAN_POINT ( 'NONE',  ( -6.015611763856276717, -17.41126425312532433, -7.205255340944797027 ) ) ;
#14570 = CARTESIAN_POINT ( 'NONE',  ( 2.600000000000000533, -11.64055411052240352, -1.199999999999999956 ) ) ;
#14571 =( BOUNDED_SURFACE ( )  B_SPLINE_SURFACE ( 3, 1, ( 
 ( #42612, #18805 ),
 ( #22876, #56369 ),
 ( #57279, #33520 ),
 ( #33213, #37929 ) ),
 .UNSPECIFIED., .F., .F., .F. ) 
 B_SPLINE_SURFACE_WITH_KNOTS ( ( 4, 4 ),
 ( 2, 2 ),
 ( 0.000000000000000000, 1.000000000000000000 ),
 ( 0.000000000000000000, 1.000000000000000000 ),
 .UNSPECIFIED. ) 
 GEOMETRIC_REPRESENTATION_ITEM ( )  RATIONAL_B_SPLINE_SURFACE ( (
 ( 1.000000000000000000, 1.000000000000000000),
 ( 0.7223157951917480446, 0.9931996967497186413),
 ( 0.7223157951917480446, 0.9931996967497186413),
 ( 1.000000000000000000, 1.000000000000000000) ) ) 
 REPRESENTATION_ITEM ( '' )  SURFACE ( )  );
#14572 = CARTESIAN_POINT ( 'NONE',  ( 0.6026112563231247332, 22.86833861538397628, -43.45779658330994977 ) ) ;
#14573 = CARTESIAN_POINT ( 'NONE',  ( 0.9741495583595165542, -11.48707840139614866, 41.34222751889824821 ) ) ;
#14574 = CARTESIAN_POINT ( 'NONE',  ( -2.708315649062916552, -0.2635547933242615160, -14.63219292706383001 ) ) ;
#14575 = CARTESIAN_POINT ( 'NONE',  ( 0.8744876279028306332, 27.35388303025845147, -40.76904626731451486 ) ) ;
#14577 = ORIENTED_EDGE ( 'NONE', *, *, #451, .F. ) ;
#14576 = LINE ( 'NONE', #34290, #33339 ) ;
#14578 = ORIENTED_EDGE ( 'NONE', *, *, #13115, .T. ) ;
#14579 = CARTESIAN_POINT ( 'NONE',  ( 4.975610109902397937, -47.89734868211986907, 9.914302615978730415 ) ) ;
#14580 = CARTESIAN_POINT ( 'NONE',  ( 0.1104177457020372732, 39.84367193872654411, 16.49849172082177162 ) ) ;
#14581 = CARTESIAN_POINT ( 'NONE',  ( 5.960721111146673579, -5.318514366755071165, 19.82454228767736382 ) ) ;
#14582 = EDGE_LOOP ( 'NONE', ( #32288, #20119, #47971, #6699 ) ) ;
#14583 = CARTESIAN_POINT ( 'NONE',  ( 5.901764892641288895, 48.56171591663485287, -6.304856435457647734 ) ) ;
#14584 = CARTESIAN_POINT ( 'NONE',  ( 4.962356264823608143, 0.9708976703217077064, 42.07484944210865052 ) ) ;
#14585 = EDGE_CURVE ( 'NONE', #41729, #26419, #38767, .T. ) ;
#14586 = ORIENTED_EDGE ( 'NONE', *, *, #55140, .T. ) ;
#14587 = ORIENTED_EDGE ( 'NONE', *, *, #21660, .F. ) ;
#14588 = CIRCLE ( 'NONE', #57512, 8.000000000000000000 ) ;
#14589 = EDGE_CURVE ( 'NONE', #1466, #61467, #49943, .T. ) ;
#14590 = DIRECTION ( 'NONE',  ( 0.1011922191286468292, 0.6783146913069540984, 0.7277700971769667238 ) ) ;
#14591 = EDGE_CURVE ( 'NONE', #49122, #5485, #17775, .T. ) ;
#14592 = CARTESIAN_POINT ( 'NONE',  ( 4.975610109902397937, 24.86209007719020647, -42.12274782266053563 ) ) ;
#14593 = AXIS2_PLACEMENT_3D ( 'NONE', #5459, #52780, #57154 ) ;
#14594 = CARTESIAN_POINT ( 'NONE',  ( 0.3676999524040323597, 14.45783756353398175, 41.67639039443440652 ) ) ;
#14595 = ADVANCED_FACE ( 'NONE', ( #40788 ), #50658, .T. ) ;
#14597 = CARTESIAN_POINT ( 'NONE',  ( 58.00000000000000000, -15.49999999999999112, -2.995852231480068572E-16 ) ) ;
#14596 = VECTOR ( 'NONE', #32893, 1000.000000000000000 ) ;
#14598 = CARTESIAN_POINT ( 'NONE',  ( 0.3622758884714730732, 10.35929834645922831, -41.85013935980092015 ) ) ;
#14599 = CARTESIAN_POINT ( 'NONE',  ( 0.9747592971366223491, 42.58247319705107259, 5.279515277919533567 ) ) ;
#14600 = EDGE_LOOP ( 'NONE', ( #40062, #38176, #60007, #30485 ) ) ;
#14601 = ORIENTED_EDGE ( 'NONE', *, *, #38831, .T. ) ;
#14602 = CARTESIAN_POINT ( 'NONE',  ( -4.062725214796418349, -12.40828859588279798, -1.199999999999999956 ) ) ;
#14603 = EDGE_CURVE ( 'NONE', #9240, #40503, #44861, .T. ) ;
#14604 = CARTESIAN_POINT ( 'NONE',  ( 2.533389852662419894, 43.99903125671219328, 1.239265994240477342 ) ) ;
#14605 = ORIENTED_EDGE ( 'NONE', *, *, #31122, .T. ) ;
#14606 = CARTESIAN_POINT ( 'NONE',  ( 0.1158403557922069033, 41.88819111113468097, -13.86793973958918080 ) ) ;
#14607 = CARTESIAN_POINT ( 'NONE',  ( 5.901764892641307547, -46.46096922681047658, -15.47158058974737038 ) ) ;
#14608 = CARTESIAN_POINT ( 'NONE',  ( 4.963659409799330291, -37.47512675766677859, -24.46566636552866214 ) ) ;
#14609 = CARTESIAN_POINT ( 'NONE',  ( 0.5782707292762423457, -8.514009628393930385, -46.12209875705174511 ) ) ;
#14610 = EDGE_CURVE ( 'NONE', #35234, #25288, #24527, .T. ) ;
#14611 = ORIENTED_EDGE ( 'NONE', *, *, #55791, .F. ) ;
#14612 = EDGE_LOOP ( 'NONE', ( #25533, #50736, #47325, #17283 ) ) ;
#14613 = CARTESIAN_POINT ( 'NONE',  ( 0.9754402186311929013, 0.1875553420611592303, 42.90805920318130262 ) ) ;
#14614 = DIRECTION ( 'NONE',  ( -1.000000000000000000, -0.000000000000000000, -0.000000000000000000 ) ) ;
#14615 = CARTESIAN_POINT ( 'NONE',  ( 0.1100247026804066219, -37.26174279786198440, -21.70899701554510841 ) ) ;
#14616 = DIRECTION ( 'NONE',  ( 0.000000000000000000, 0.000000000000000000, -1.000000000000000000 ) ) ;
#14617 = B_SPLINE_CURVE_WITH_KNOTS ( 'NONE', 3,
 ( #56512, #13627, #28626, #30091 ),
 .UNSPECIFIED., .F., .F.,
 ( 4, 4 ),
 ( 5.647850449853784215E-17, 0.005004741218457476985 ),
 .UNSPECIFIED. ) ;
#14618 = ORIENTED_EDGE ( 'NONE', *, *, #60955, .T. ) ;
#14619 = CARTESIAN_POINT ( 'NONE',  ( 0.3676999524040323597, -26.85386693986589890, -34.99743438737782242 ) ) ;
#14620 = ORIENTED_EDGE ( 'NONE', *, *, #56317, .T. ) ;
#14621 = CARTESIAN_POINT ( 'NONE',  ( 5.896278296736517710, -9.661066686814107740, 17.64060004895849332 ) ) ;
#14622 = CARTESIAN_POINT ( 'NONE',  ( 0.8744876279028263033, -13.11369837310799547, -47.31153099783008997 ) ) ;
#14623 = ORIENTED_EDGE ( 'NONE', *, *, #39161, .T. ) ;
#14624 = CARTESIAN_POINT ( 'NONE',  ( 2.500000000000000000, -1.178949249685218748, -2.041999999999998039 ) ) ;
#14625 = CARTESIAN_POINT ( 'NONE',  ( 5.880360259849739535, -39.91356965504129306, -26.61251048557234711 ) ) ;
#14626 = CARTESIAN_POINT ( 'NONE',  ( 0.9756354156337460060, 26.22428641656300741, -33.96210048825346917 ) ) ;
#14627 = ORIENTED_EDGE ( 'NONE', *, *, #41368, .F. ) ;
#14628 = CARTESIAN_POINT ( 'NONE',  ( 0.7948884756798504370, -0.7064021483319558037, -49.09378413409362452 ) ) ;
#14629 = CARTESIAN_POINT ( 'NONE',  ( 0.8744876279028306332, -24.68559978112762110, 42.43785119236699188 ) ) ;
#14630 = DIRECTION ( 'NONE',  ( 0.000000000000000000, 0.000000000000000000, 1.000000000000000000 ) ) ;
#14631 = EDGE_CURVE ( 'NONE', #12553, #1788, #37203, .T. ) ;
#14632 = CARTESIAN_POINT ( 'NONE',  ( -5.995132425357893702, -2.451215106828221302, -18.68405145320026506 ) ) ;
#14633 = ORIENTED_EDGE ( 'NONE', *, *, #50876, .F. ) ;
#14634 = CARTESIAN_POINT ( 'NONE',  ( 0.5809828226811617480, -24.41822904836953612, 41.20389530892298779 ) ) ;
#14635 = CARTESIAN_POINT ( 'NONE',  ( 4.322998006666165516, 22.13465289016567894, 42.57894920390135240 ) ) ;
#14636 = CARTESIAN_POINT ( 'NONE',  ( 3.390910168358336918, -15.98239228339566687, 40.97145681365616099 ) ) ;
#14637 = ORIENTED_EDGE ( 'NONE', *, *, #38088, .F. ) ;
#14638 = AXIS2_PLACEMENT_3D ( 'NONE', #61790, #28301, #23917 ) ;
#14639 = CARTESIAN_POINT ( 'NONE',  ( 43.00000000000000000, 15.50000000000000533, 1.598617315530390848E-15 ) ) ;
#14640 = CARTESIAN_POINT ( 'NONE',  ( 2.618530812446115519, 46.75512741918793580, 4.866708252371440224 ) ) ;
#14641 = CARTESIAN_POINT ( 'NONE',  ( 2.301430502907645170, -28.20897229937376594, -38.87758534782497577 ) ) ;
#14642 = CONICAL_SURFACE ( 'NONE', #28606, 43.08621763946400307, 1.568696531533066763 ) ;
#14643 = LINE ( 'NONE', #58433, #6951 ) ;
#14644 = CARTESIAN_POINT ( 'NONE',  ( 4.322998006666179727, -25.80712523194247510, -40.45864630878510582 ) ) ;
#14645 = CARTESIAN_POINT ( 'NONE',  ( 3.783278058412225420, 36.37891728069903508, -22.99727281874588058 ) ) ;
#14646 = CARTESIAN_POINT ( 'NONE',  ( -6.016104459813374383, 4.882138007283004733, -18.19977249352305648 ) ) ;
#14647 = DIRECTION ( 'NONE',  ( -1.000000000000000000, 6.071532164548154356E-18, -5.169878828456422968E-26 ) ) ;
#14648 = CARTESIAN_POINT ( 'NONE',  ( 0.5830081025819929819, 11.13700143456257052, 45.55435471421800742 ) ) ;
#14649 = CARTESIAN_POINT ( 'NONE',  ( 4.694002226626921015, 39.88981857773283934, -22.07005086722039522 ) ) ;
#14650 = AXIS2_PLACEMENT_3D ( 'NONE', #19183, #34205, #15406 ) ;
#14651 = CARTESIAN_POINT ( 'NONE',  ( 5.958863334805807099, 19.82594244347352586, -5.313608583996313861 ) ) ;
#14653 = ORIENTED_EDGE ( 'NONE', *, *, #26651, .F. ) ;
#14652 = DIRECTION ( 'NONE',  ( 0.000000000000000000, 0.000000000000000000, -1.000000000000000000 ) ) ;
#14654 = EDGE_LOOP ( 'NONE', ( #1011, #59641, #27688, #6776 ) ) ;
#14655 = DIRECTION ( 'NONE',  ( 0.000000000000000000, 0.000000000000000000, 1.000000000000000000 ) ) ;
#14656 = DIRECTION ( 'NONE',  ( -0.1011922191286467460, -0.1083236746284043789, 0.9889520293233740045 ) ) ;
#14657 = CARTESIAN_POINT ( 'NONE',  ( 4.335381028904216727, -5.712845112848606632, 48.65306001045512829 ) ) ;
#14658 = CARTESIAN_POINT ( 'NONE',  ( 0.5807400328401574052, 47.41494605191442702, 6.791881299635745606 ) ) ;
#14659 = CARTESIAN_POINT ( 'NONE',  ( 0.9730545539215883499, 30.69604515769692554, -29.98130006528829483 ) ) ;
#14660 = VERTEX_POINT ( 'NONE', #31664 ) ;
#14661 = EDGE_CURVE ( 'NONE', #59261, #58751, #33700, .T. ) ;
#14662 = DIRECTION ( 'NONE',  ( -0.9848077530122079093, -0.1736481776669316079, 5.551115123125783935E-17 ) ) ;
#14663 = B_SPLINE_CURVE_WITH_KNOTS ( 'NONE', 3,
 ( #16458, #45297, #59352, #36509, #17698, #21158 ),
 .UNSPECIFIED., .F., .F.,
 ( 4, 2, 4 ),
 ( 0.000000000000000000, 0.0002447195606305753966, 0.0004894391212611507933 ),
 .UNSPECIFIED. ) ;
#14664 = CARTESIAN_POINT ( 'NONE',  ( -18.90751475399365589, -7.774715922560747394, 1.885931201481398922 ) ) ;
#14665 = DIRECTION ( 'NONE',  ( 0.000000000000000000, 0.000000000000000000, 1.000000000000000000 ) ) ;
#14666 = EDGE_LOOP ( 'NONE', ( #31618, #49110, #51377, #8297 ) ) ;
#14667 = ADVANCED_FACE ( 'NONE', ( #26649 ), #33971, .F. ) ;
#14668 = B_SPLINE_CURVE_WITH_KNOTS ( 'NONE', 3,
 ( #30270, #20577, #40634, #21189, #49687, #6743 ),
 .UNSPECIFIED., .F., .F.,
 ( 4, 2, 4 ),
 ( 1.426045310262811165E-18, 0.0002450742804987334714, 0.0004901485609974655334 ),
 .UNSPECIFIED. ) ;
#14669 = CARTESIAN_POINT ( 'NONE',  ( 5.901463166500145796, -1.998795974254174102, -20.01306285889149450 ) ) ;
#14670 = CARTESIAN_POINT ( 'NONE',  ( 0.5835226383429282793, -25.38729180038570377, -39.43003791005067171 ) ) ;
#14671 = VERTEX_POINT ( 'NONE', #25723 ) ;
#14672 = CARTESIAN_POINT ( 'NONE',  ( 0.8557997880470599172, 28.43566216844970640, 38.55640757422448672 ) ) ;
#14673 = ORIENTED_EDGE ( 'NONE', *, *, #60171, .F. ) ;
#14674 = CARTESIAN_POINT ( 'NONE',  ( 53.15000000000000568, 15.50000000000000711, -0.1732459626436144429 ) ) ;
#14675 = EDGE_CURVE ( 'NONE', #18847, #51998, #5745, .T. ) ;
#14676 = CARTESIAN_POINT ( 'NONE',  ( -6.016104459813371719, 7.206059014950318087, -17.41090761020828737 ) ) ;
#14677 = AXIS2_PLACEMENT_3D ( 'NONE', #3759, #61387, #13822 ) ;
#14678 = ORIENTED_EDGE ( 'NONE', *, *, #48749, .T. ) ;
#14679 = CARTESIAN_POINT ( 'NONE',  ( 4.291220156522059348, -43.75057291092625178, -17.47215977695438127 ) ) ;
#14680 = CARTESIAN_POINT ( 'NONE',  ( 0.5848930533535030563, 11.04862722691854060, -45.57631971526609505 ) ) ;
#14681 = CARTESIAN_POINT ( 'NONE',  ( 0.5806925824938511393, -42.09901922557415332, -20.66143612114853312 ) ) ;
#14682 = CARTESIAN_POINT ( 'NONE',  ( 0.5819845079324652559, -37.72030202710095637, 29.51613512130369799 ) ) ;
#14683 = EDGE_CURVE ( 'NONE', #12273, #60753, #28971, .T. ) ;
#14684 = B_SPLINE_CURVE_WITH_KNOTS ( 'NONE', 3,
 ( #1403, #40295, #36504, #2646, #3256, #31796 ),
 .UNSPECIFIED., .F., .F.,
 ( 4, 2, 4 ),
 ( 6.106282077343213345E-18, 0.0002291472222819920411, 0.0004582944445639780106 ),
 .UNSPECIFIED. ) ;
#14685 = ORIENTED_EDGE ( 'NONE', *, *, #11252, .F. ) ;
#14686 = CARTESIAN_POINT ( 'NONE',  ( 0.5806925824938499181, -46.75147433417400578, -3.677228565731735621 ) ) ;
#14687 = ORIENTED_EDGE ( 'NONE', *, *, #58400, .F. ) ;
#14688 = CARTESIAN_POINT ( 'NONE',  ( 4.553261556744875094, -39.47791437445886942, -19.26223877088359515 ) ) ;
#14689 = EDGE_LOOP ( 'NONE', ( #38186, #16989, #49619, #11117 ) ) ;
#14690 = VERTEX_POINT ( 'NONE', #1904 ) ;
#14691 = FACE_OUTER_BOUND ( 'NONE', #36367, .T. ) ;
#14693 = AXIS2_PLACEMENT_3D ( 'NONE', #60154, #36081, #12268 ) ;
#14692 = CARTESIAN_POINT ( 'NONE',  ( 0.6009452777970410997, -33.70725232128916815, 34.32439724342980014 ) ) ;
#14694 = FACE_OUTER_BOUND ( 'NONE', #34409, .T. ) ;
#14695 = ORIENTED_EDGE ( 'NONE', *, *, #60096, .F. ) ;
#14696 = CARTESIAN_POINT ( 'NONE',  ( 0.8557997880470606944, -34.51495345639572321, 33.22501220301889191 ) ) ;
#14697 = CARTESIAN_POINT ( 'NONE',  ( 0.8554163680231816613, -20.57434774096662622, -42.16517150618031451 ) ) ;
#14698 = CARTESIAN_POINT ( 'NONE',  ( 5.901764892641307547, -48.87142464753282667, 3.094401454271700214 ) ) ;
#14699 = ORIENTED_EDGE ( 'NONE', *, *, #38715, .T. ) ;
#14700 = CIRCLE ( 'NONE', #39755, 47.91270532121795611 ) ;
#14701 = EDGE_LOOP ( 'NONE', ( #15216, #49875, #40953, #40460 ) ) ;
#14702 = CARTESIAN_POINT ( 'NONE',  ( 0.8751705887134553219, 41.19904111682508585, -24.81530984069164703 ) ) ;
#14703 = CARTESIAN_POINT ( 'NONE',  ( 1.231276596079881935, 38.91607545535268997, -15.58254928345689017 ) ) ;
#14704 = EDGE_CURVE ( 'NONE', #18146, #47447, #60451, .T. ) ;
#14705 = CARTESIAN_POINT ( 'NONE',  ( 4.967162193818130511, 0.000000000000000000, 0.000000000000000000 ) ) ;
#14706 = DIRECTION ( 'NONE',  ( -0.1024043820194934368, -0.2447326578667193553, -0.9641676559171111771 ) ) ;
#14707 = VERTEX_POINT ( 'NONE', #4350 ) ;
#14708 = ORIENTED_EDGE ( 'NONE', *, *, #1811, .T. ) ;
#14709 = DIRECTION ( 'NONE',  ( 1.000000000000000000, 0.000000000000000000, 0.000000000000000000 ) ) ;
#14710 = CARTESIAN_POINT ( 'NONE',  ( 2.879087469061462734, 42.82528940656273164, -10.10426959396493274 ) ) ;
#14711 = DIRECTION ( 'NONE',  ( 0.000000000000000000, 0.000000000000000000, 1.000000000000000000 ) ) ;
#14712 = CARTESIAN_POINT ( 'NONE',  ( 4.553261556744875094, 0.000000000000000000, 0.000000000000000000 ) ) ;
#14713 = CARTESIAN_POINT ( 'NONE',  ( 4.956653778116966613, 0.000000000000000000, 0.000000000000000000 ) ) ;
#14714 = CARTESIAN_POINT ( 'NONE',  ( 3.782542959838390395, 21.69833210684487668, -36.00583615440189789 ) ) ;
#14715 = VERTEX_POINT ( 'NONE', #61074 ) ;
#14716 = CARTESIAN_POINT ( 'NONE',  ( 4.975801465491694664, -42.71626295676247764, -21.70134120755185947 ) ) ;
#14717 = CARTESIAN_POINT ( 'NONE',  ( 3.678748215320120085, -46.05789111167558758, -16.65183114989213919 ) ) ;
#14718 = AXIS2_PLACEMENT_3D ( 'NONE', #55264, #40296, #21774 ) ;
#14719 = CARTESIAN_POINT ( 'NONE',  ( 0.8557997880470690211, -46.50333260518550560, -11.51622788066506686 ) ) ;
#14720 = CARTESIAN_POINT ( 'NONE',  ( 1.231276596079881047, 36.49189576017899839, -20.63051901543672884 ) ) ;
#14721 = VECTOR ( 'NONE', #11667, 1000.000000000000114 ) ;
#14722 = CARTESIAN_POINT ( 'NONE',  ( 1.091591847532195070, -41.76074381686517256, -3.577606297232447385 ) ) ;
#14723 = CARTESIAN_POINT ( 'NONE',  ( 0.9787284016396595732, -34.44493023777801000, 23.87221774036584776 ) ) ;
#14724 = VERTEX_POINT ( 'NONE', #18187 ) ;
#14725 = B_SPLINE_CURVE_WITH_KNOTS ( 'NONE', 3,
 ( #15544, #44680, #6402, #49047, #29941, #10849 ),
 .UNSPECIFIED., .F., .F.,
 ( 4, 2, 4 ),
 ( 8.673617379884035472E-19, 0.0002293801035737077186, 0.0004587602071474145699 ),
 .UNSPECIFIED. ) ;
#14726 = EDGE_CURVE ( 'NONE', #27747, #54885, #8449, .T. ) ;
#14727 = SURFACE_STYLE_USAGE ( .BOTH. , #25348 ) ;
#14728 = AXIS2_PLACEMENT_3D ( 'NONE', #17578, #2212, #31055 ) ;
#14729 = CARTESIAN_POINT ( 'NONE',  ( 0.6845945791218034371, -39.15688516782669382, 25.82914757919002469 ) ) ;
#14730 = CARTESIAN_POINT ( 'NONE',  ( 0.6016118706126977189, -47.41192439221646282, -12.79298558627663773 ) ) ;
#14731 = CARTESIAN_POINT ( 'NONE',  ( -4.000000000000000000, 0.7862748000878058141, -0.03447227762756577968 ) ) ;
#14732 = DIRECTION ( 'NONE',  ( 0.000000000000000000, 0.000000000000000000, 1.000000000000000000 ) ) ;
#14733 = VERTEX_POINT ( 'NONE', #4048 ) ;
#14734 = EDGE_CURVE ( 'NONE', #35972, #9945, #22207, .T. ) ;
#14735 = CARTESIAN_POINT ( 'NONE',  ( 0.9752570700956806338, -37.27462300504088688, 21.25416333281084746 ) ) ;
#14736 = CARTESIAN_POINT ( 'NONE',  ( 5.894904586330512508, -4.663773726906127237, -19.56472914931006457 ) ) ;
#14737 = VECTOR ( 'NONE', #51040, 1000.000000000000000 ) ;
#14738 = ADVANCED_FACE ( 'NONE', ( #23486 ), #3557, .F. ) ;
#14739 =( BOUNDED_SURFACE ( )  B_SPLINE_SURFACE ( 3, 1, ( 
 ( #33485, #42277 ),
 ( #41970, #47267 ),
 ( #52561, #37895 ),
 ( #3702, #4616 ) ),
 .UNSPECIFIED., .F., .F., .F. ) 
 B_SPLINE_SURFACE_WITH_KNOTS ( ( 4, 4 ),
 ( 2, 2 ),
 ( 0.000000000000000000, 1.000000000000000000 ),
 ( 0.000000000000000000, 1.000000000000000000 ),
 .UNSPECIFIED. ) 
 GEOMETRIC_REPRESENTATION_ITEM ( )  RATIONAL_B_SPLINE_SURFACE ( (
 ( 1.000000000000000000, 1.000000000000000000),
 ( 0.7211978278499970862, 0.9934217856018976445),
 ( 0.7211978278499970862, 0.9934217856018976445),
 ( 1.000000000000000000, 1.000000000000000000) ) ) 
 REPRESENTATION_ITEM ( '' )  SURFACE ( )  );
#14740 = DIRECTION ( 'NONE',  ( 0.5000000000000066613, 0.8660254037844348218, -0.000000000000000000 ) ) ;
#14741 = VERTEX_POINT ( 'NONE', #37933 ) ;
#14742 = CYLINDRICAL_SURFACE ( 'NONE', #48074, 5.612499999999999822 ) ;
#14743 = CARTESIAN_POINT ( 'NONE',  ( 0.5809828226811617480, 23.47450554821709900, 41.74875432577658074 ) ) ;
#14744 = ORIENTED_EDGE ( 'NONE', *, *, #6197, .T. ) ;
#14745 = CARTESIAN_POINT ( 'NONE',  ( -6.078726893082806448, -6.653559303940370206, 18.06998035022918359 ) ) ;
#14746 = ORIENTED_EDGE ( 'NONE', *, *, #18052, .F. ) ;
#14747 = CARTESIAN_POINT ( 'NONE',  ( 0.8751705887134553219, 33.37254303619554463, -34.63284514348550402 ) ) ;
#14748 = EDGE_LOOP ( 'NONE', ( #3118, #11131, #40274, #41796 ) ) ;
#14749 = CARTESIAN_POINT ( 'NONE',  ( 0.1139756605157201536, 29.36928842959055430, -32.93023104739080509 ) ) ;
#14750 = CARTESIAN_POINT ( 'NONE',  ( 0.2885700199627508344, 40.13549263616302909, 15.75356883787167739 ) ) ;
#14751 = ORIENTED_EDGE ( 'NONE', *, *, #33058, .F. ) ;
#14752 = CARTESIAN_POINT ( 'NONE',  ( 5.895596859100789899, 8.469463536103054579, -18.24270732712412624 ) ) ;
#14753 = EDGE_CURVE ( 'NONE', #25935, #15210, #10221, .T. ) ;
#14754 = B_SPLINE_CURVE_WITH_KNOTS ( 'NONE', 3,
 ( #24547, #44300, #10453, #405, #19247, #5103 ),
 .UNSPECIFIED., .F., .F.,
 ( 4, 2, 4 ),
 ( 3.476216610979977084E-18, 0.0002291966416970801898, 0.0004583932833941569101 ),
 .UNSPECIFIED. ) ;
#14755 = ORIENTED_EDGE ( 'NONE', *, *, #23632, .T. ) ;
#14756 = DIRECTION ( 'NONE',  ( -0.1011922191286467460, -0.6592733245820187049, -0.7450629626295969254 ) ) ;
#14757 =( BOUNDED_SURFACE ( )  B_SPLINE_SURFACE ( 3, 1, ( 
 ( #31281, #35382 ),
 ( #49766, #17191 ),
 ( #35696, #11892 ),
 ( #55377, #55070 ) ),
 .UNSPECIFIED., .F., .F., .F. ) 
 B_SPLINE_SURFACE_WITH_KNOTS ( ( 4, 4 ),
 ( 2, 2 ),
 ( 0.000000000000000000, 1.000000000000000000 ),
 ( 0.000000000000000000, 1.000000000000000000 ),
 .UNSPECIFIED. ) 
 GEOMETRIC_REPRESENTATION_ITEM ( )  RATIONAL_B_SPLINE_SURFACE ( (
 ( 1.000000000000000000, 1.000000000000000000),
 ( 0.9953390228620291325, 0.8624445117761032620),
 ( 0.9953390228620291325, 0.8624445117761032620),
 ( 1.000000000000000000, 1.000000000000000000) ) ) 
 REPRESENTATION_ITEM ( '' )  SURFACE ( )  );
#14758 = CARTESIAN_POINT ( 'NONE',  ( 0.5830081025819935370, 40.48790813666568056, 23.66350204638288091 ) ) ;
#14759 = TOROIDAL_SURFACE ( 'NONE', #22747, 6.866799999999992465, 0.02570000000000859444 ) ;
#14760 = ORIENTED_EDGE ( 'NONE', *, *, #43745, .F. ) ;
#14761 = CARTESIAN_POINT ( 'NONE',  ( 0.9747592971366236814, -16.71904224817876639, -39.51726118357609607 ) ) ;
#14762 = CARTESIAN_POINT ( 'NONE',  ( -6.077587904424778920, 13.83688374988418879, 13.39166417911236984 ) ) ;
#14763 = AXIS2_PLACEMENT_3D ( 'NONE', #50033, #26841, #35646 ) ;
#14764 = CARTESIAN_POINT ( 'NONE',  ( 0.1129192098497455998, -22.45785791439690371, -37.98152716363461678 ) ) ;
#14765 = ORIENTED_EDGE ( 'NONE', *, *, #58733, .F. ) ;
#14766 = CARTESIAN_POINT ( 'NONE',  ( 0.6001305935487422083, -23.60027211631801691, -41.92422178329160687 ) ) ;
#14767 = CARTESIAN_POINT ( 'NONE',  ( 0.1156867017252034696, -17.97492158142190988, 40.29696020070147711 ) ) ;
#14768 = ORIENTED_EDGE ( 'NONE', *, *, #41755, .F. ) ;
#14769 = CARTESIAN_POINT ( 'NONE',  ( 5.960221823109900008, 7.849768660536558862, -18.96526051813972913 ) ) ;
#14770 = ORIENTED_EDGE ( 'NONE', *, *, #49804, .T. ) ;
#14771 = CARTESIAN_POINT ( 'NONE',  ( 4.291220156522060236, -28.73895862173628757, 37.32909394351577959 ) ) ;
#14772 = CARTESIAN_POINT ( 'NONE',  ( 0.8557997880470690211, 41.02602466100812961, -24.73961900479208609 ) ) ;
#14773 = ORIENTED_EDGE ( 'NONE', *, *, #45653, .T. ) ;
#14774 = CARTESIAN_POINT ( 'NONE',  ( 0.5806925824938499181, 4.150136846022649095, 46.71186922510005957 ) ) ;
#14775 = CARTESIAN_POINT ( 'NONE',  ( 0.1158816050234198897, 25.23951143218047122, -36.19266643907288028 ) ) ;
#14776 = CARTESIAN_POINT ( 'NONE',  ( 0.6041374136657476912, 47.71861871402581556, 6.106202762793639494 ) ) ;
#14777 = CARTESIAN_POINT ( 'NONE',  ( 0.9785694773339241870, -22.36238727067532039, -35.44374474108247597 ) ) ;
#14778 = B_SPLINE_CURVE_WITH_KNOTS ( 'NONE', 3,
 ( #53950, #53035, #57406, #48049, #43995, #10137 ),
 .UNSPECIFIED., .F., .F.,
 ( 4, 2, 4 ),
 ( 9.822656275951702151E-18, 0.0002291459268755758727, 0.0004582918537511419333 ),
 .UNSPECIFIED. ) ;
#14779 = ORIENTED_EDGE ( 'NONE', *, *, #19968, .F. ) ;
#14780 = CARTESIAN_POINT ( 'NONE',  ( 0.1149546198390368063, -41.00147165784255776, 16.30416777742285106 ) ) ;
#14781 = EDGE_CURVE ( 'NONE', #42220, #19259, #49827, .T. ) ;
#14782 = CARTESIAN_POINT ( 'NONE',  ( -6.001507490154110336, 7.196845540359404048, -17.41542759839256860 ) ) ;
#14783 = CARTESIAN_POINT ( 'NONE',  ( 4.298462506757085855, 0.6202153076419610889, -48.94031900834726656 ) ) ;
#14784 = CONICAL_SURFACE ( 'NONE', #61778, 42.08604991992415023, 1.569615340895231137 ) ;
#14785 = EDGE_CURVE ( 'NONE', #40747, #56645, #49044, .T. ) ;
#14786 = LINE ( 'NONE', #29791, #23930 ) ;
#14787 = CARTESIAN_POINT ( 'NONE',  ( 0.5980894510889457338, 41.31170365136888023, -24.66136644716778292 ) ) ;
#14788 = CARTESIAN_POINT ( 'NONE',  ( 0.6253024248130490959, -35.74992959045948737, 33.66580998126782021 ) ) ;
#14789 = EDGE_CURVE ( 'NONE', #22756, #10982, #55661, .T. ) ;
#14790 = CARTESIAN_POINT ( 'NONE',  ( -17.69685288772385690, -7.723236801699937537, -2.086240377089799480 ) ) ;
#14791 = DIRECTION ( 'NONE',  ( 1.000000000000000000, 0.000000000000000000, 0.000000000000000000 ) ) ;
#14792 = CARTESIAN_POINT ( 'NONE',  ( 0.8554163680231816613, 11.76336166872287947, 45.41837508500981357 ) ) ;
#14793 = DIRECTION ( 'NONE',  ( -1.000000000000000000, -3.135800716341489291E-16, 1.298891185607901956E-16 ) ) ;
#14794 = CARTESIAN_POINT ( 'NONE',  ( 0.8560838555295223751, 31.94705745926225404, -34.34761059777416392 ) ) ;
#14795 = LINE ( 'NONE', #58283, #37682 ) ;
#14796 = CARTESIAN_POINT ( 'NONE',  ( 0.9790724872846782167, 9.675934389771114752, 40.77635961763012773 ) ) ;
#14797 = B_SPLINE_CURVE_WITH_KNOTS ( 'NONE', 3,
 ( #28589, #22989, #51778, #8876, #19219, #38330 ),
 .UNSPECIFIED., .F., .F.,
 ( 4, 2, 4 ),
 ( 8.609910155989501895E-17, 0.0002293366620881446324, 0.0004586733241762031791 ),
 .UNSPECIFIED. ) ;
#14798 = B_SPLINE_CURVE_WITH_KNOTS ( 'NONE', 3,
 ( #30731, #6908, #45182, #2211, #40476, #11973, #31054, #50162, #13497, #22584, #32601, #8780, #31988, #42021, #18193, #9390 ),
 .UNSPECIFIED., .F., .F.,
 ( 4, 3, 3, 3, 3, 4 ),
 ( 1.040890552917501732E-17, 0.0002724568934985527823, 0.0004086836638483798759, 0.0005449104342063559956, 0.0008173270854453659143, 0.001089761613562691394 ),
 .UNSPECIFIED. ) ;
#14799 = ADVANCED_FACE ( 'NONE', ( #47615 ), #42389, .F. ) ;
#14800 = CARTESIAN_POINT ( 'NONE',  ( 0.5836750258453341500, 33.73891062492405979, 33.99574025613924988 ) ) ;
#14801 = CARTESIAN_POINT ( 'NONE',  ( 0.9730545539215883499, -10.61654491617534291, -41.57420493492396929 ) ) ;
#14802 = ORIENTED_EDGE ( 'NONE', *, *, #20954, .T. ) ;
#14803 = VECTOR ( 'NONE', #56814, 1000.000000000000114 ) ;
#14804 = CARTESIAN_POINT ( 'NONE',  ( 2.282803330402965347, -39.45519406433361098, 25.49087226445491794 ) ) ;
#14805 = CARTESIAN_POINT ( 'NONE',  ( 0.7242003506639952404, -7.027071004854443359, 48.59662485418876088 ) ) ;
#14806 = CARTESIAN_POINT ( 'NONE',  ( 3.270143674763207553, -13.60381564321235359, 1.514386915940542311 ) ) ;
#14807 = ORIENTED_EDGE ( 'NONE', *, *, #11772, .T. ) ;
#14808 = CARTESIAN_POINT ( 'NONE',  ( 0.9730545539215883499, -21.01499094264575618, 37.40983423658466478 ) ) ;
#14809 = FACE_OUTER_BOUND ( 'NONE', #29944, .T. ) ;
#14810 = EDGE_CURVE ( 'NONE', #47700, #5679, #50588, .T. ) ;
#14811 = EDGE_LOOP ( 'NONE', ( #9181, #11047, #42779, #25006 ) ) ;
#14812 = EDGE_LOOP ( 'NONE', ( #58799, #46657, #31843, #36270 ) ) ;
#14813 = CARTESIAN_POINT ( 'NONE',  ( 4.834790513006553603, -44.69577334950020031, -15.32570342967947497 ) ) ;
#14814 = ORIENTED_EDGE ( 'NONE', *, *, #35674, .F. ) ;
#14815 = CARTESIAN_POINT ( 'NONE',  ( 0.5786265663353196143, 28.58414684753485346, 38.43785771743214497 ) ) ;
#14816 = CIRCLE ( 'NONE', #3782, 12.50000000000000000 ) ;
#14817 = ORIENTED_EDGE ( 'NONE', *, *, #10779, .F. ) ;
#14818 = VERTEX_POINT ( 'NONE', #48233 ) ;
#14819 = CARTESIAN_POINT ( 'NONE',  ( -6.079354080745853928, 19.09804277166044173, 2.461243088358096465 ) ) ;
#14820 = ORIENTED_EDGE ( 'NONE', *, *, #27421, .F. ) ;
#14821 = CARTESIAN_POINT ( 'NONE',  ( -6.078457390727109555, -12.94259897003423099, 14.25775728992385183 ) ) ;
#14822 = DIRECTION ( 'NONE',  ( 1.000000000000000000, 1.558861125776144859E-16, -3.851859888774471706E-32 ) ) ;
#14823 = EDGE_CURVE ( 'NONE', #28115, #24133, #31667, .T. ) ;
#14824 = VECTOR ( 'NONE', #46380, 1000.000000000000000 ) ;
#14825 = LINE ( 'NONE', #42419, #60560 ) ;
#14826 = VERTEX_POINT ( 'NONE', #4977 ) ;
#14827 = CARTESIAN_POINT ( 'NONE',  ( 2.624215991343620935, 25.21574086439706619, 40.85210347989540480 ) ) ;
#14828 = CARTESIAN_POINT ( 'NONE',  ( 0.9754402186311944556, -34.15542855230918917, -25.97197377940591068 ) ) ;
#14829 = ORIENTED_EDGE ( 'NONE', *, *, #57991, .T. ) ;
#14830 = COLOUR_RGB ( '', 0.31764706, 0.68627451, 0.89019608) ;
#14831 = ORIENTED_EDGE ( 'NONE', *, *, #21515, .F. ) ;
#14832 = CARTESIAN_POINT ( 'NONE',  ( -6.016104459813371719, 11.46679299034602018, -14.95258000663120157 ) ) ;
#14833 = VERTEX_POINT ( 'NONE', #57285 ) ;
#14834 = CARTESIAN_POINT ( 'NONE',  ( 4.322998006666165516, -45.10383234877044600, 16.38761975793128656 ) ) ;
#14835 = CARTESIAN_POINT ( 'NONE',  ( 0.9722240741986377666, -30.74950262511622512, 29.92651525529365131 ) ) ;
#14836 = CARTESIAN_POINT ( 'NONE',  ( 1.231276596079887264, 28.52807286890788419, -30.71523773966838888 ) ) ;
#14837 = CARTESIAN_POINT ( 'NONE',  ( 0.1073791018717578927, 5.147744207006301309, 42.81622261970996135 ) ) ;
#14838 = ORIENTED_EDGE ( 'NONE', *, *, #29715, .T. ) ;
#14839 = CARTESIAN_POINT ( 'NONE',  ( -6.079354080745853928, 7.793434646514300290, 17.60838810506720975 ) ) ;
#14840 = CARTESIAN_POINT ( 'NONE',  ( 1.231276596079881047, 41.42457922925067493, 6.425029704024775690 ) ) ;
#14841 = CARTESIAN_POINT ( 'NONE',  ( 0.1073791018717483448, 40.02496097243036388, 16.05399293000829175 ) ) ;
#14842 = B_SPLINE_CURVE_WITH_KNOTS ( 'NONE', 3,
 ( #59786, #16571, #59462, #40401, #50086, #31910, #31592, #54761, #31284, #35698, #3071, #46031, #45403, #16896, #36315, #50680, #26579, #45710, #2452 ),
 .UNSPECIFIED., .F., .F.,
 ( 4, 3, 3, 3, 3, 3, 4 ),
 ( 1.161276725443423652E-16, 0.0002618519381806260252, 0.0003927759815485984689, 0.0005237000248299447311, 0.0006546240681325002104, 0.0007855481115631340102, 0.0009699050456655109419 ),
 .UNSPECIFIED. ) ;
#14843 = DIRECTION ( 'NONE',  ( 0.000000000000000000, 0.000000000000000000, 1.000000000000000000 ) ) ;
#14844 = ORIENTED_EDGE ( 'NONE', *, *, #55667, .T. ) ;
#14845 = CARTESIAN_POINT ( 'NONE',  ( 6.999999999999995559, 58.44237546506882808, -54.69470952477875159 ) ) ;
#14846 = CARTESIAN_POINT ( 'NONE',  ( 4.963659409799333844, -24.46566636552799068, -37.47512675766720491 ) ) ;
#14847 = CARTESIAN_POINT ( 'NONE',  ( 0.6001305935487315502, -46.60388846085731984, 11.94532529598297010 ) ) ;
#14848 = CARTESIAN_POINT ( 'NONE',  ( 0.6029442701453591180, -35.33687315128987905, -34.10059561133684980 ) ) ;
#14849 = CIRCLE ( 'NONE', #59853, 2.649999999999997691 ) ;
#14850 = VECTOR ( 'NONE', #29032, 1000.000000000000000 ) ;
#14851 = VERTEX_POINT ( 'NONE', #10953 ) ;
#14852 = ORIENTED_EDGE ( 'NONE', *, *, #50476, .T. ) ;
#14853 = FACE_OUTER_BOUND ( 'NONE', #35099, .T. ) ;
#14854 = FACE_OUTER_BOUND ( 'NONE', #2775, .T. ) ;
#14855 = EDGE_CURVE ( 'NONE', #17365, #28495, #39469, .T. ) ;
#14856 = CARTESIAN_POINT ( 'NONE',  ( 0.1084644655670282953, -39.68806829486960197, 16.86976209534710236 ) ) ;
#14857 = CARTESIAN_POINT ( 'NONE',  ( -6.057079549204054558, 16.77479338118054386, -9.457142175014601193 ) ) ;
#14858 = CARTESIAN_POINT ( 'NONE',  ( 4.975610109902397937, -44.31543648230415755, 20.70245146161774841 ) ) ;
#14859 = EDGE_CURVE ( 'NONE', #20273, #30001, #39163, .T. ) ;
#14860 = CARTESIAN_POINT ( 'NONE',  ( 5.880360259849752858, 3.184717612777935525, -47.86623372148046229 ) ) ;
#14861 = CARTESIAN_POINT ( 'NONE',  ( 0.1313383488274153799, -17.09007684155478302, -39.59253935480791853 ) ) ;
#14862 =( BOUNDED_SURFACE ( )  B_SPLINE_SURFACE ( 3, 1, ( 
 ( #29153, #56721 ),
 ( #52021, #48270 ),
 ( #28526, #14154 ),
 ( #52639, #27926 ) ),
 .UNSPECIFIED., .F., .F., .F. ) 
 B_SPLINE_SURFACE_WITH_KNOTS ( ( 4, 4 ),
 ( 2, 2 ),
 ( 0.000000000000000000, 1.000000000000000000 ),
 ( 0.000000000000000000, 1.000000000000000000 ),
 .UNSPECIFIED. ) 
 GEOMETRIC_REPRESENTATION_ITEM ( )  RATIONAL_B_SPLINE_SURFACE ( (
 ( 1.000000000000000000, 1.000000000000000000),
 ( 0.9953485035131437453, 0.8621029689291523912),
 ( 0.9953485035131437453, 0.8621029689291523912),
 ( 1.000000000000000000, 1.000000000000000000) ) ) 
 REPRESENTATION_ITEM ( '' )  SURFACE ( )  );
#14863 = LINE ( 'NONE', #24556, #42830 ) ;
#14864 = FACE_OUTER_BOUND ( 'NONE', #10818, .T. ) ;
#14865 = ADVANCED_FACE ( 'NONE', ( #24108 ), #22797, .F. ) ;
#14866 = CYLINDRICAL_SURFACE ( 'NONE', #25740, 1.000000000000000888 ) ;
#14867 = EDGE_CURVE ( 'NONE', #37711, #37128, #6626, .T. ) ;
#14868 = DIRECTION ( 'NONE',  ( 0.09722883295013597105, 0.8999532196066800660, -0.4250067723727768421 ) ) ;
#14869 = ORIENTED_EDGE ( 'NONE', *, *, #2396, .F. ) ;
#14870 = VECTOR ( 'NONE', #28482, 1000.000000000000114 ) ;
#14871 = EDGE_CURVE ( 'NONE', #5563, #25568, #910, .T. ) ;
#14872 = DIRECTION ( 'NONE',  ( -1.000000000000000000, -0.000000000000000000, -0.000000000000000000 ) ) ;
#14873 = CARTESIAN_POINT ( 'NONE',  ( 0.3676999524040323597, -35.84016207189440451, 25.71834687500696859 ) ) ;
#14874 = CARTESIAN_POINT ( 'NONE',  ( 5.958863334805807099, -12.49619391867194373, 16.28335246510346224 ) ) ;
#14875 = CARTESIAN_POINT ( 'NONE',  ( -2.739355103387247858, -10.90485690860422707, 10.19468796746048689 ) ) ;
#14876 = CARTESIAN_POINT ( 'NONE',  ( -6.079354080745853928, 7.793434646514551645, -17.60838810506710317 ) ) ;
#14877 = CARTESIAN_POINT ( 'NONE',  ( 0.5809828226811553087, -41.20389530892325070, 24.41822904836909203 ) ) ;
#14878 = DIRECTION ( 'NONE',  ( -1.000000000000000000, -0.000000000000000000, -0.000000000000000000 ) ) ;
#14879 = ITEM_DEFINED_TRANSFORMATION ( 'NONE', 'NONE', #39935,  #14677 ) ;
#14880 = CARTESIAN_POINT ( 'NONE',  ( 4.694002226626921015, -16.06750747807337021, 42.66286411960865621 ) ) ;
#14881 =( GEOMETRIC_REPRESENTATION_CONTEXT ( 3 ) GLOBAL_UNCERTAINTY_ASSIGNED_CONTEXT ( ( #48012 ) ) GLOBAL_UNIT_ASSIGNED_CONTEXT ( ( #11240, #2435, #6189 ) ) REPRESENTATION_CONTEXT ( 'NONE', 'WORKASPACE' ) );
#14882 = DIRECTION ( 'NONE',  ( -1.000000000000000000, 0.000000000000000000, 0.000000000000000000 ) ) ;
#14883 = ADVANCED_FACE ( 'NONE', ( #52917 ), #40028, .F. ) ;
#14884 = CARTESIAN_POINT ( 'NONE',  ( 5.959547316686252039, -16.28624005235090877, -12.49238070347970364 ) ) ;
#14885 = ADVANCED_FACE ( 'NONE', ( #40962 ), #59551, .F. ) ;
#14886 = CARTESIAN_POINT ( 'NONE',  ( 0.6016117650947689910, -1.922104516163298804, -49.06991510562703240 ) ) ;
#14887 = CARTESIAN_POINT ( 'NONE',  ( 4.303969348037246512, 2.158280495710879876, -48.06163817123223936 ) ) ;
#14889 = ORIENTED_EDGE ( 'NONE', *, *, #48583, .T. ) ;
#14888 = DIRECTION ( 'NONE',  ( 0.000000000000000000, 0.000000000000000000, 1.000000000000000000 ) ) ;
#14890 = VERTEX_POINT ( 'NONE', #15342 ) ;
#14891 = CARTESIAN_POINT ( 'NONE',  ( 4.834790513006555379, -46.28862912354751558, 9.484310981144012942 ) ) ;
#14892 = CARTESIAN_POINT ( 'NONE',  ( 4.060580049360325461, 43.64911337592206308, -5.120800313926658909 ) ) ;
#14893 = CARTESIAN_POINT ( 'NONE',  ( 0.1140933569871964148, 41.75531667278490744, 14.26336144249862947 ) ) ;
#14894 = VERTEX_POINT ( 'NONE', #10636 ) ;
#14895 = CARTESIAN_POINT ( 'NONE',  ( 3.782625744892853525, 40.05508866136273127, -12.76040659326237048 ) ) ;
#14896 = CARTESIAN_POINT ( 'NONE',  ( 0.5997462898726536595, -13.47075269803089803, -47.22383351542737984 ) ) ;
#14898 = B_SPLINE_CURVE_WITH_KNOTS ( 'NONE', 3,
 ( #40696, #26249, #7434, #41609 ),
 .UNSPECIFIED., .F., .F.,
 ( 4, 4 ),
 ( 0.000000000000000000, 0.004446090762761359047 ),
 .UNSPECIFIED. ) ;
#14897 = CARTESIAN_POINT ( 'NONE',  ( 5.960221823109900008, 5.307149561567809926, 19.82761049839343670 ) ) ;
#14899 = VERTEX_POINT ( 'NONE', #29727 ) ;
#14900 = ORIENTED_EDGE ( 'NONE', *, *, #32630, .T. ) ;
#14901 = CARTESIAN_POINT ( 'NONE',  ( 4.962356264823603702, 30.91935898304086550, -28.55221248765493414 ) ) ;
#14902 = CARTESIAN_POINT ( 'NONE',  ( 4.956653778116982600, -45.71126949320260735, 14.93973939759871072 ) ) ;
#14903 = AXIS2_PLACEMENT_3D ( 'NONE', #19583, #761, #439 ) ;
#14904 = CIRCLE ( 'NONE', #50864, 75.00000000000001421 ) ;
#14905 = FACE_OUTER_BOUND ( 'NONE', #52082, .T. ) ;
#14906 = CARTESIAN_POINT ( 'NONE',  ( 4.553261556744875094, 27.21079963941838997, 34.48350256002230196 ) ) ;
#14907 = CARTESIAN_POINT ( 'NONE',  ( 5.896278296736517710, -2.007758883826515017, -20.01239325714941941 ) ) ;
#14908 = EDGE_CURVE ( 'NONE', #31680, #53617, #48839, .T. ) ;
#14909 = CARTESIAN_POINT ( 'NONE',  ( 0.8554163680231738898, -44.61245466728234987, 14.52357950615125048 ) ) ;
#14910 = ADVANCED_FACE ( 'NONE', ( #9698 ), #14757, .F. ) ;
#14911 = CARTESIAN_POINT ( 'NONE',  ( 0.5832366564991497970, 37.83193087518350950, -29.37287047358843139 ) ) ;
#14912 = ORIENTED_EDGE ( 'NONE', *, *, #23555, .F. ) ;
#14913 = ORIENTED_EDGE ( 'NONE', *, *, #29687, .F. ) ;
#14914 = FACE_OUTER_BOUND ( 'NONE', #28385, .T. ) ;
#14915 = CARTESIAN_POINT ( 'NONE',  ( 2.706805983486679779, 43.99338256706222694, 1.165505739093682269 ) ) ;
#14916 = CONICAL_SURFACE ( 'NONE', #34943, 43.08621763946400307, 1.568696531533066763 ) ;
#14917 = EDGE_LOOP ( 'NONE', ( #38933, #39816, #55879, #57330 ) ) ;
#14918 = CARTESIAN_POINT ( 'NONE',  ( 0.1156867017252034419, 41.91550876716623719, -13.78524327187579246 ) ) ;
#14919 = DIRECTION ( 'NONE',  ( 0.000000000000000000, -0.7071067811865553443, 0.7071067811865395791 ) ) ;
#14920 = CARTESIAN_POINT ( 'NONE',  ( -6.016489644550736315, 9.425415887801086967, 16.31649074174280045 ) ) ;
#14921 = CARTESIAN_POINT ( 'NONE',  ( 4.553261556744875094, 0.000000000000000000, 0.000000000000000000 ) ) ;
#14922 = VERTEX_POINT ( 'NONE', #30343 ) ;
#14923 = ORIENTED_EDGE ( 'NONE', *, *, #20881, .F. ) ;
#14924 = CARTESIAN_POINT ( 'NONE',  ( 0.5837157313716002660, -13.98107098236325641, 44.76345292499393480 ) ) ;
#14925 = CARTESIAN_POINT ( 'NONE',  ( 1.154321485836933725, 10.30834589251769451, -41.66001465002018023 ) ) ;
#14926 = B_SPLINE_CURVE_WITH_KNOTS ( 'NONE', 3,
 ( #44652, #16135, #11430, #25829, #44966, #2004 ),
 .UNSPECIFIED., .F., .F.,
 ( 4, 2, 4 ),
 ( 1.206508049868409138E-16, 0.0002448718616795903316, 0.0004897437233590599915 ),
 .UNSPECIFIED. ) ;
#14927 = CARTESIAN_POINT ( 'NONE',  ( 0.1081432562775997419, -37.13343246403911024, -21.92800090985256745 ) ) ;
#14928 = AXIS2_PLACEMENT_3D ( 'NONE', #23411, #32831, #56604 ) ;
#14929 = ORIENTED_EDGE ( 'NONE', *, *, #16258, .T. ) ;
#14930 = CARTESIAN_POINT ( 'NONE',  ( -6.017396004339686577, 13.32329839588573606, -13.32495836419610669 ) ) ;
#14931 = ORIENTED_EDGE ( 'NONE', *, *, #40438, .T. ) ;
#14932 = CARTESIAN_POINT ( 'NONE',  ( -6.010958268070873523, 9.434296419346207330, 16.31164801516945317 ) ) ;
#14933 = CARTESIAN_POINT ( 'NONE',  ( 0.1157506346131639274, 9.908971581732375356, 42.99712713653383389 ) ) ;
#14934 = ORIENTED_EDGE ( 'NONE', *, *, #31089, .F. ) ;
#14935 = CARTESIAN_POINT ( 'NONE',  ( 4.549368137175248350, -24.02461520945298545, 35.57418903283073064 ) ) ;
#14936 = CARTESIAN_POINT ( 'NONE',  ( 0.5998501479064708430, -47.76154736470761719, 5.759754759339972274 ) ) ;
#14937 = DIRECTION ( 'NONE',  ( -1.000000000000000000, -0.000000000000000000, -0.000000000000000000 ) ) ;
#14938 = EDGE_CURVE ( 'NONE', #10414, #49122, #46708, .T. ) ;
#14939 = CARTESIAN_POINT ( 'NONE',  ( -6.017396004339687465, -7.212050743684302212, 17.40836349643165093 ) ) ;
#14940 =( BOUNDED_SURFACE ( )  B_SPLINE_SURFACE ( 3, 1, ( 
 ( #1679, #15201 ),
 ( #29898, #44046 ),
 ( #49013, #30202 ),
 ( #53994, #44640 ) ),
 .UNSPECIFIED., .F., .F., .F. ) 
 B_SPLINE_SURFACE_WITH_KNOTS ( ( 4, 4 ),
 ( 2, 2 ),
 ( 0.000000000000000000, 1.000000000000000000 ),
 ( 0.000000000000000000, 1.000000000000000000 ),
 .UNSPECIFIED. ) 
 GEOMETRIC_REPRESENTATION_ITEM ( )  RATIONAL_B_SPLINE_SURFACE ( (
 ( 1.000000000000000000, 1.000000000000000000),
 ( 0.9953390228620291325, 0.8624445117761032620),
 ( 0.9953390228620291325, 0.8624445117761032620),
 ( 1.000000000000000000, 1.000000000000000000) ) ) 
 REPRESENTATION_ITEM ( '' )  SURFACE ( )  );
#14941 = DIRECTION ( 'NONE',  ( -0.07906939808003037029, -0.5431863341251643718, -0.8358807550763009964 ) ) ;
#14942 = CARTESIAN_POINT ( 'NONE',  ( 4.956445790443988031, 46.25174887658550915, 8.849507104743643993 ) ) ;
#14943 = CARTESIAN_POINT ( 'NONE',  ( 0.6031356219577718170, 29.21669799774962684, -38.21934428970583753 ) ) ;
#14944 = CARTESIAN_POINT ( 'NONE',  ( 4.956653778116970166, 36.51451553856417576, 31.29546495791861460 ) ) ;
#14945 = ORIENTED_EDGE ( 'NONE', *, *, #57312, .F. ) ;
#14946 = CARTESIAN_POINT ( 'NONE',  ( 5.917102823773431552, -20.11192790512648543, -0.008601786823262999593 ) ) ;
#14947 = LINE ( 'NONE', #34976, #16673 ) ;
#14948 = EDGE_CURVE ( 'NONE', #54066, #12972, #58006, .T. ) ;
#14949 = CARTESIAN_POINT ( 'NONE',  ( 0.8744876279028306332, 11.79038800009151089, 47.65854384249261244 ) ) ;
#14950 = VERTEX_POINT ( 'NONE', #60087 ) ;
#14951 = CIRCLE ( 'NONE', #51986, 9.500000000000000000 ) ;
#14952 = B_SPLINE_CURVE_WITH_KNOTS ( 'NONE', 3,
 ( #1801, #54414, #13624, #21545 ),
 .UNSPECIFIED., .F., .F.,
 ( 4, 4 ),
 ( 0.000000000000000000, 0.005013413432710151982 ),
 .UNSPECIFIED. ) ;
#14953 = EDGE_CURVE ( 'NONE', #10282, #17462, #20646, .T. ) ;
#14954 = DIRECTION ( 'NONE',  ( -1.000000000000000000, 0.000000000000000000, -0.000000000000000000 ) ) ;
#14955 = CARTESIAN_POINT ( 'NONE',  ( 4.291220156522060236, 46.92833126662970500, 4.137719400244832535 ) ) ;
#14956 = CARTESIAN_POINT ( 'NONE',  ( 0.6026112563231247332, 22.55952149237266013, 43.61890627857813740 ) ) ;
#14957 = CARTESIAN_POINT ( 'NONE',  ( 0.7764146366350266337, -44.59376577618206028, -14.54085718134173000 ) ) ;
#14958 = CARTESIAN_POINT ( 'NONE',  ( 2.299746137290199943, -24.30809607782931536, 42.58400876804762447 ) ) ;
#14959 = DIRECTION ( 'NONE',  ( 0.04915571944256429127, 0.6398721219583684006, -0.7669076755298376291 ) ) ;
#14960 = CARTESIAN_POINT ( 'NONE',  ( 0.1313383488274159905, -41.81465294768286611, -10.54394128763545346 ) ) ;
#14961 = DIRECTION ( 'NONE',  ( -1.000000000000000000, -0.000000000000000000, -0.000000000000000000 ) ) ;
#14962 = CARTESIAN_POINT ( 'NONE',  ( 0.2224561200757608770, -25.64288022150858737, -34.66601556960344510 ) ) ;
#14964 = EDGE_LOOP ( 'NONE', ( #13448, #27617 ) ) ;
#14963 = CARTESIAN_POINT ( 'NONE',  ( 0.1073791018717483448, 11.62916352156094035, 41.52698815987171344 ) ) ;
#14965 = VERTEX_POINT ( 'NONE', #6201 ) ;
#14966 = CONICAL_SURFACE ( 'NONE', #49951, 43.08621763946400307, 1.568696531533066763 ) ;
#14967 = DIRECTION ( 'NONE',  ( 0.000000000000000000, 0.000000000000000000, 1.000000000000000000 ) ) ;
#14968 = DIRECTION ( 'NONE',  ( -2.168404344971009361E-16, 1.000000000000000000, 0.000000000000000000 ) ) ;
#14969 = CARTESIAN_POINT ( 'NONE',  ( 4.999999999999997335, -2.784000523420839360E-13, 80.00000000000001421 ) ) ;
#14970 = CARTESIAN_POINT ( 'NONE',  ( 0.9749527285493299056, 42.57770849153634174, -5.317382389862751246 ) ) ;
#14971 = CARTESIAN_POINT ( 'NONE',  ( -6.015611763856276717, 18.68122482568283260, -2.465697960550860657 ) ) ;
#14972 = CARTESIAN_POINT ( 'NONE',  ( 0.5800708119828325016, 17.74761857127127840, -44.48635609075538611 ) ) ;
#14973 = ORIENTED_EDGE ( 'NONE', *, *, #59241, .T. ) ;
#14974 = CARTESIAN_POINT ( 'NONE',  ( 5.895596859100789899, 5.962379729971948983, 19.20880556328547684 ) ) ;
#14975 = B_SPLINE_CURVE_WITH_KNOTS ( 'NONE', 3,
 ( #46234, #60598, #49988, #45009 ),
 .UNSPECIFIED., .F., .F.,
 ( 4, 4 ),
 ( 0.000000000000000000, 0.004442905043737214836 ),
 .UNSPECIFIED. ) ;
#14976 = CARTESIAN_POINT ( 'NONE',  ( 0.1064266379913941379, -10.61815631313391073, 41.79703901861799409 ) ) ;
#14977 = CARTESIAN_POINT ( 'NONE',  ( -2.601141883200665639, 8.903211435101033189, -11.98032777561927986 ) ) ;
#14978 = ORIENTED_EDGE ( 'NONE', *, *, #1260, .F. ) ;
#14979 = CARTESIAN_POINT ( 'NONE',  ( 4.303969348037258058, 30.97035057417660298, 36.81598326424561662 ) ) ;
#14980 = CARTESIAN_POINT ( 'NONE',  ( 0.5806925824938499181, -24.77160101449041463, -39.81946942793766198 ) ) ;
#14981 = EDGE_LOOP ( 'NONE', ( #22592, #9654, #2986, #56702 ) ) ;
#14982 = VECTOR ( 'NONE', #31068, 1000.000000000000000 ) ;
#14983 = ADVANCED_FACE ( 'NONE', ( #44791 ), #49677, .T. ) ;
#14984 = CARTESIAN_POINT ( 'NONE',  ( 0.5800708057587384836, -44.48635630048008238, 17.74761804745386584 ) ) ;
#14985 = ORIENTED_EDGE ( 'NONE', *, *, #17762, .T. ) ;
#14986 = CARTESIAN_POINT ( 'NONE',  ( 0.5800708119828336118, -29.65250521075920886, -37.61306658477503362 ) ) ;
#14988 = CARTESIAN_POINT ( 'NONE',  ( 0.6031356755773454870, 34.01711753073210787, 34.01708126935054111 ) ) ;
#14987 = AXIS2_PLACEMENT_3D ( 'NONE', #46493, #3543, #42125 ) ;
#14989 = ORIENTED_EDGE ( 'NONE', *, *, #23698, .F. ) ;
#14990 = CARTESIAN_POINT ( 'NONE',  ( 4.553261556744873317, -29.36425772793689859, 32.66925058691941075 ) ) ;
#14991 = CARTESIAN_POINT ( 'NONE',  ( 0.3676999524040323597, 3.413584541508654091, 43.98065510995502336 ) ) ;
#14992 = CARTESIAN_POINT ( 'NONE',  ( 0.9788927965476027504, 40.45682727923838939, 10.93534357620513298 ) ) ;
#14993 = FACE_OUTER_BOUND ( 'NONE', #47263, .T. ) ;
#14994 = VERTEX_POINT ( 'NONE', #45705 ) ;
#14995 = DIRECTION ( 'NONE',  ( 0.000000000000000000, 0.000000000000000000, 1.000000000000000000 ) ) ;
#14996 = ORIENTED_EDGE ( 'NONE', *, *, #49449, .F. ) ;
#14997 = FACE_OUTER_BOUND ( 'NONE', #36041, .T. ) ;
#14998 = VERTEX_POINT ( 'NONE', #40102 ) ;
#14999 = ORIENTED_EDGE ( 'NONE', *, *, #46529, .F. ) ;
#15000 = CARTESIAN_POINT ( 'NONE',  ( 0.5797568665920715958, -46.82898593237341345, -2.504273377137976819 ) ) ;
#15001 = PLANE ( 'NONE',  #59412 ) ;
#15002 = CONICAL_SURFACE ( 'NONE', #40019, 42.08604991992415023, 1.569615340895231137 ) ;
#15003 = DIRECTION ( 'NONE',  ( 0.07906939808003034253, -0.6987975377710964331, 0.7109360248941636318 ) ) ;
#15004 = ORIENTED_EDGE ( 'NONE', *, *, #52603, .T. ) ;
#15005 = CARTESIAN_POINT ( 'NONE',  ( 0.9730545539215883499, -34.34678117142538412, -25.71816799638815354 ) ) ;
#15006 = CARTESIAN_POINT ( 'NONE',  ( 4.322998006666179727, -45.10383234877022574, -16.38761975793193315 ) ) ;
#15007 = CARTESIAN_POINT ( 'NONE',  ( 3.678834586032787346, -26.95182293378241667, 40.89268406664441358 ) ) ;
#15008 = ORIENTED_EDGE ( 'NONE', *, *, #55861, .T. ) ;
#15009 = B_SPLINE_CURVE_WITH_KNOTS ( 'NONE', 3,
 ( #22394, #37139, #50893, #7984 ),
 .UNSPECIFIED., .F., .F.,
 ( 4, 4 ),
 ( 0.000000000000000000, 0.005004948556313786219 ),
 .UNSPECIFIED. ) ;
#15010 = EDGE_CURVE ( 'NONE', #21977, #30486, #43077, .T. ) ;
#15011 = ORIENTED_EDGE ( 'NONE', *, *, #60867, .F. ) ;
#15012 = DIRECTION ( 'NONE',  ( 1.000000000000000000, 0.000000000000000000, 0.000000000000000000 ) ) ;
#15013 = CARTESIAN_POINT ( 'NONE',  ( 0.3676999524040323597, 24.55639947020961600, 36.64606156713607277 ) ) ;
#15014 = CARTESIAN_POINT ( 'NONE',  ( 1.091591847532196624, 38.88578709869444339, -15.64143703982636247 ) ) ;
#15015 = CARTESIAN_POINT ( 'NONE',  ( 2.301529144917014769, -13.67115311794032451, -46.04684498357975997 ) ) ;
#15016 = CARTESIAN_POINT ( 'NONE',  ( 0.9790850452238858415, 38.60296000837998065, 16.31406782058402527 ) ) ;
#15017 = EDGE_LOOP ( 'NONE', ( #23318, #49149 ) ) ;
#15018 = EDGE_CURVE ( 'NONE', #10097, #5228, #2448, .T. ) ;
#15019 =( BOUNDED_SURFACE ( )  B_SPLINE_SURFACE ( 3, 1, ( 
 ( #42716, #23589 ),
 ( #14821, #33932 ),
 ( #23903, #14214 ),
 ( #53007, #13590 ) ),
 .UNSPECIFIED., .F., .F., .F. ) 
 B_SPLINE_SURFACE_WITH_KNOTS ( ( 4, 4 ),
 ( 2, 2 ),
 ( 0.000000000000000000, 1.000000000000000000 ),
 ( 0.000000000000000000, 1.000000000000000000 ),
 .UNSPECIFIED. ) 
 GEOMETRIC_REPRESENTATION_ITEM ( )  RATIONAL_B_SPLINE_SURFACE ( (
 ( 1.000000000000000000, 1.000000000000000000),
 ( 0.9953485035131437453, 0.8621029689291523912),
 ( 0.9953485035131437453, 0.8621029689291523912),
 ( 1.000000000000000000, 1.000000000000000000) ) ) 
 REPRESENTATION_ITEM ( '' )  SURFACE ( )  );
#15020 = CARTESIAN_POINT ( 'NONE',  ( 0.7762783648524371749, 7.133808749409432437, 47.37038525648361542 ) ) ;
#15021 = VERTEX_POINT ( 'NONE', #2130 ) ;
#15022 = EDGE_CURVE ( 'NONE', #40637, #6465, #40099, .T. ) ;
#15023 = CARTESIAN_POINT ( 'NONE',  ( 0.3622758884714600280, -42.62881903538205108, -6.444611261694439541 ) ) ;
#15024 = CARTESIAN_POINT ( 'NONE',  ( 0.9762797500689124330, -37.17323042682959766, -19.35137526946170183 ) ) ;
#15025 = CARTESIAN_POINT ( 'NONE',  ( 0.1154773475650540254, -42.63511898549099044, 11.36618929717198512 ) ) ;
#15026 = CARTESIAN_POINT ( 'NONE',  ( 0.9749527285493325701, -21.70110358462066458, 37.01618455594564949 ) ) ;
#15027 = CARTESIAN_POINT ( 'NONE',  ( 3.238931869106853600, -42.34694073502594591, 7.419701784410414724 ) ) ;
#15028 = CARTESIAN_POINT ( 'NONE',  ( 0.5980894510889448457, -6.974827154144452201, 47.60453381548680341 ) ) ;
#15029 = CARTESIAN_POINT ( 'NONE',  ( 0.8560838555295223751, 28.55542365806889293, 37.21505896528891810 ) ) ;
#15030 = CARTESIAN_POINT ( 'NONE',  ( 4.975610109902397937, -5.269241389990889424, -48.62802178077758697 ) ) ;
#15032 = EDGE_CURVE ( 'NONE', #33451, #56839, #1514, .T. ) ;
#15031 = DIRECTION ( 'NONE',  ( -1.000000000000000000, -0.000000000000000000, -0.000000000000000000 ) ) ;
#15033 = LINE ( 'NONE', #1510, #190 ) ;
#15034 = EDGE_CURVE ( 'NONE', #35339, #16043, #12196, .T. ) ;
#15035 = CARTESIAN_POINT ( 'NONE',  ( 5.901764892641288895, -16.95277890151785627, -45.94120976809306001 ) ) ;
#15036 = CARTESIAN_POINT ( 'NONE',  ( 0.8551540677456715978, -47.90804413217340141, -0.9122407826480831705 ) ) ;
#15037 = B_SPLINE_CURVE_WITH_KNOTS ( 'NONE', 3,
 ( #7074, #45341, #2693, #31217, #45641, #40646 ),
 .UNSPECIFIED., .F., .F.,
 ( 4, 2, 4 ),
 ( 1.267283937151336631E-16, 0.0002450741128632354321, 0.0004901482257263441210 ),
 .UNSPECIFIED. ) ;
#15038 = B_SPLINE_CURVE_WITH_KNOTS ( 'NONE', 3,
 ( #16123, #55232, #21740, #40880, #16425, #11738 ),
 .UNSPECIFIED., .F., .F.,
 ( 4, 2, 4 ),
 ( 7.007167689862070887E-18, 0.0002448709889506568856, 0.0004897419779013068323 ),
 .UNSPECIFIED. ) ;
#15039 = VECTOR ( 'NONE', #23502, 1000.000000000000227 ) ;
#15040 = ORIENTED_EDGE ( 'NONE', *, *, #19673, .F. ) ;
#15041 = LINE ( 'NONE', #30974, #8243 ) ;
#15042 = VECTOR ( 'NONE', #45241, 1000.000000000000227 ) ;
#15043 = CARTESIAN_POINT ( 'NONE',  ( 0.5782707292762442330, -39.07253195953447999, 25.94366203870946563 ) ) ;
#15044 = CARTESIAN_POINT ( 'NONE',  ( 0.5832367798473374609, 18.58036934788136563, -44.14510605973664781 ) ) ;
#15045 = CARTESIAN_POINT ( 'NONE',  ( 0.8554163680231720024, 39.89400665120465561, -24.69157156653778884 ) ) ;
#15046 = VERTEX_POINT ( 'NONE', #11250 ) ;
#15047 = CARTESIAN_POINT ( 'NONE',  ( 0.8744876279028263033, -13.11369837310799547, -47.31153099783008997 ) ) ;
#15048 = CARTESIAN_POINT ( 'NONE',  ( 3.783278058412224976, 18.05212641201972446, 39.06943705276837164 ) ) ;
#15049 = CARTESIAN_POINT ( 'NONE',  ( 4.291220156522060236, -23.50705364442154988, 40.82655295593768585 ) ) ;
#15050 = ORIENTED_EDGE ( 'NONE', *, *, #25341, .T. ) ;
#15051 = CARTESIAN_POINT ( 'NONE',  ( 0.3622758884714730732, -31.06363466427707820, -29.89648521331620756 ) ) ;
#15052 = EDGE_CURVE ( 'NONE', #9163, #39811, #33424, .T. ) ;
#15053 = CARTESIAN_POINT ( 'NONE',  ( 0.9722240741986373225, -41.29187377038493878, -11.66659279944019545 ) ) ;
#15054 = VERTEX_POINT ( 'NONE', #41026 ) ;
#15055 = CARTESIAN_POINT ( 'NONE',  ( 0.5997462898726536595, -31.02483596213004091, -38.06587952047387091 ) ) ;
#15056 = ORIENTED_EDGE ( 'NONE', *, *, #17695, .F. ) ;
#15057 = CARTESIAN_POINT ( 'NONE',  ( 0.6067375320500700830, -17.67235760802231681, -44.51755737952373693 ) ) ;
#15058 = ORIENTED_EDGE ( 'NONE', *, *, #26723, .F. ) ;
#15059 = CARTESIAN_POINT ( 'NONE',  ( -2.739355103387247858, -7.512526911498964566, -12.89998086645948661 ) ) ;
#15060 = CARTESIAN_POINT ( 'NONE',  ( 0.8751705887134553219, 41.19904111682508585, -24.81530984069164703 ) ) ;
#15061 = ORIENTED_EDGE ( 'NONE', *, *, #55972, .F. ) ;
#15062 = CARTESIAN_POINT ( 'NONE',  ( 2.282816707992309180, -46.93788479523038859, -1.825359514628755342 ) ) ;
#15063 = ORIENTED_EDGE ( 'NONE', *, *, #41623, .F. ) ;
#15064 = FACE_OUTER_BOUND ( 'NONE', #28894, .T. ) ;
#15065 = CARTESIAN_POINT ( 'NONE',  ( 0.3622758884714730732, 33.69533458712344753, -26.89560658783350178 ) ) ;
#15066 = CARTESIAN_POINT ( 'NONE',  ( 0.9762797500689124330, -39.75277516423524560, 13.26806888463673673 ) ) ;
#15067 = ORIENTED_EDGE ( 'NONE', *, *, #43459, .F. ) ;
#15068 = DIRECTION ( 'NONE',  ( -1.000000000000000000, -0.000000000000000000, -0.000000000000000000 ) ) ;
#15069 = CARTESIAN_POINT ( 'NONE',  ( 4.834790513006553603, -36.27562111512950338, 30.27653635467491355 ) ) ;
#15070 = B_SPLINE_CURVE_WITH_KNOTS ( 'NONE', 3,
 ( #3209, #13258, #32361, #47085 ),
 .UNSPECIFIED., .F., .F.,
 ( 4, 4 ),
 ( 1.998817200139820460E-17, 0.004444306975806115029 ),
 .UNSPECIFIED. ) ;
#15071 = CARTESIAN_POINT ( 'NONE',  ( 3.782625744892852637, 16.70566327442924504, 38.57666287610150846 ) ) ;
#15072 = CARTESIAN_POINT ( 'NONE',  ( 4.691466044806102076, 36.88741755356034702, 25.04870410140802406 ) ) ;
#15073 = ORIENTED_EDGE ( 'NONE', *, *, #32108, .F. ) ;
#15074 = CARTESIAN_POINT ( 'NONE',  ( 0.5980271706414734822, 46.82647351461020691, 14.80981502339485623 ) ) ;
#15075 = CARTESIAN_POINT ( 'NONE',  ( 0.1158816050234198758, -17.85553307869832551, 40.34999355366331741 ) ) ;
#15076 = VERTEX_POINT ( 'NONE', #40710 ) ;
#15077 = DIRECTION ( 'NONE',  ( 0.000000000000000000, 0.000000000000000000, -1.000000000000000000 ) ) ;
#15078 = B_SPLINE_CURVE_WITH_KNOTS ( 'NONE', 3,
 ( #7145, #49158, #35707, #12206 ),
 .UNSPECIFIED., .F., .F.,
 ( 4, 4 ),
 ( 0.000000000000000000, 0.005014147105413698652 ),
 .UNSPECIFIED. ) ;
#15079 = ORIENTED_EDGE ( 'NONE', *, *, #38507, .T. ) ;
#15080 = CIRCLE ( 'NONE', #43126, 72.00000000000002842 ) ;
#15081 = CARTESIAN_POINT ( 'NONE',  ( 5.959547316686252039, 0.003562808152905788499, -20.52562247508876681 ) ) ;
#15082 = ORIENTED_EDGE ( 'NONE', *, *, #33975, .T. ) ;
#15083 = CARTESIAN_POINT ( 'NONE',  ( 0.9789889208857693870, -12.50833032322637095, -39.99845710233616103 ) ) ;
#15084 = B_SPLINE_CURVE_WITH_KNOTS ( 'NONE', 3,
 ( #5804, #45004, #40308, #10858 ),
 .UNSPECIFIED., .F., .F.,
 ( 4, 4 ),
 ( 0.000000000000000000, 0.004048833967417086489 ),
 .UNSPECIFIED. ) ;
#15085 = CARTESIAN_POINT ( 'NONE',  ( 0.6039202388192952409, 49.01762936092972467, -2.972494690241308302 ) ) ;
#15086 = CARTESIAN_POINT ( 'NONE',  ( 4.960386119450146403, 12.51307094103760065, -41.92683532413223446 ) ) ;
#15087 = CARTESIAN_POINT ( 'NONE',  ( 0.5806925824938502512, -2.112975627976310111, -46.84824112321764744 ) ) ;
#15088 = EDGE_CURVE ( 'NONE', #58860, #47387, #36312, .T. ) ;
#15089 = ORIENTED_EDGE ( 'NONE', *, *, #17540, .T. ) ;
#15090 = CARTESIAN_POINT ( 'NONE',  ( 0.1140933569871964148, -41.04033302048136278, 16.20620299921893093 ) ) ;
#15091 = EDGE_CURVE ( 'NONE', #56469, #58608, #19221, .T. ) ;
#15092 = CARTESIAN_POINT ( 'NONE',  ( 4.553261556744875094, 38.16266689001181334, 21.75202109381179483 ) ) ;
#15093 = CARTESIAN_POINT ( 'NONE',  ( 1.154321713695929841, 33.53917066545422898, 26.77578845938192487 ) ) ;
#15094 = CARTESIAN_POINT ( 'NONE',  ( 0.5980894510889448457, 0.7015180096004866028, -48.10766805928368939 ) ) ;
#15095 = CARTESIAN_POINT ( 'NONE',  ( 0.9730545539215883499, -42.60426903087357431, 5.099196237954729760 ) ) ;
#15096 = CARTESIAN_POINT ( 'NONE',  ( -6.015611763856276717, 14.94556629257425584, 11.47596948473816170 ) ) ;
#15097 = CARTESIAN_POINT ( 'NONE',  ( 0.5797568599927149791, 43.41643190453758194, -17.72678056923071210 ) ) ;
#15098 = CARTESIAN_POINT ( 'NONE',  ( 0.8751705887134553219, -46.67919521768879321, -11.58504748649183647 ) ) ;
#15099 = DIRECTION ( 'NONE',  ( -1.000000000000000000, -0.000000000000000000, -0.000000000000000000 ) ) ;
#15100 = CARTESIAN_POINT ( 'NONE',  ( 0.3676999524040323597, 34.11874447325018167, -27.96179284115914854 ) ) ;
#15101 = ADVANCED_FACE ( 'NONE', ( #39790, #61005 ), #61611, .T. ) ;
#15102 = CARTESIAN_POINT ( 'NONE',  ( 0.1158516988532803521, -43.76817641532991843, -5.593647478108881188 ) ) ;
#15103 = CARTESIAN_POINT ( 'NONE',  ( 0.6001305935487422083, 44.24520387813801392, 18.89378601236078481 ) ) ;
#15104 = CARTESIAN_POINT ( 'NONE',  ( 0.5835871038041858805, -1.703517860905799264, 46.86504539418556448 ) ) ;
#15105 =( BOUNDED_SURFACE ( )  B_SPLINE_SURFACE ( 3, 1, ( 
 ( #24940, #1714 ),
 ( #1105, #29936 ),
 ( #49042, #38434 ),
 ( #57483, #14625 ) ),
 .UNSPECIFIED., .F., .F., .F. ) 
 B_SPLINE_SURFACE_WITH_KNOTS ( ( 4, 4 ),
 ( 2, 2 ),
 ( 0.000000000000000000, 1.000000000000000000 ),
 ( 0.000000000000000000, 1.000000000000000000 ),
 .UNSPECIFIED. ) 
 GEOMETRIC_REPRESENTATION_ITEM ( )  RATIONAL_B_SPLINE_SURFACE ( (
 ( 1.000000000000000000, 1.000000000000000000),
 ( 0.7223157951917480446, 0.9931996967497186413),
 ( 0.7223157951917480446, 0.9931996967497186413),
 ( 1.000000000000000000, 1.000000000000000000) ) ) 
 REPRESENTATION_ITEM ( '' )  SURFACE ( )  );
#15106 = CARTESIAN_POINT ( 'NONE',  ( 0.5819845079324657000, 34.18710788661951483, 33.54497088780092895 ) ) ;
#15107 = CARTESIAN_POINT ( 'NONE',  ( 0.7242003506640003474, -39.83544447980661829, -28.70799605026916268 ) ) ;
#15108 = ORIENTED_EDGE ( 'NONE', *, *, #54004, .F. ) ;
#15109 = CARTESIAN_POINT ( 'NONE',  ( 0.5839880159502345292, 29.19321933421549531, -37.97080096460551601 ) ) ;
#15110 = CARTESIAN_POINT ( 'NONE',  ( 0.5987334308729319599, -7.239498256756843553, 48.57110840366055271 ) ) ;
#15111 = CARTESIAN_POINT ( 'NONE',  ( 0.5998501479064708430, 28.86886762351073088, 38.48283596222038483 ) ) ;
#15112 = EDGE_LOOP ( 'NONE', ( #47046, #8400, #30914, #19464 ) ) ;
#15113 = CARTESIAN_POINT ( 'NONE',  ( -2.569797478183790229, -2.353985772484857630, 14.44232325624822622 ) ) ;
#15114 = CARTESIAN_POINT ( 'NONE',  ( -6.078457390727109555, 15.42941986619915440, -11.52074275513721702 ) ) ;
#15115 =( BOUNDED_SURFACE ( )  B_SPLINE_SURFACE ( 3, 1, ( 
 ( #40164, #39530 ),
 ( #16315, #30715 ),
 ( #59523, #16631 ),
 ( #11955, #6256 ) ),
 .UNSPECIFIED., .F., .F., .F. ) 
 B_SPLINE_SURFACE_WITH_KNOTS ( ( 4, 4 ),
 ( 2, 2 ),
 ( 0.000000000000000000, 1.000000000000000000 ),
 ( 0.000000000000000000, 1.000000000000000000 ),
 .UNSPECIFIED. ) 
 GEOMETRIC_REPRESENTATION_ITEM ( )  RATIONAL_B_SPLINE_SURFACE ( (
 ( 1.000000000000000000, 1.000000000000000000),
 ( 0.9953485035131437453, 0.8621029689291523912),
 ( 0.9953485035131437453, 0.8621029689291523912),
 ( 1.000000000000000000, 1.000000000000000000) ) ) 
 REPRESENTATION_ITEM ( '' )  SURFACE ( )  );
#15117 = ORIENTED_EDGE ( 'NONE', *, *, #9009, .T. ) ;
#15116 = VECTOR ( 'NONE', #38537, 1000.000000000000000 ) ;
#15118 = CARTESIAN_POINT ( 'NONE',  ( 0.3622758884714600280, -40.13994584881793770, 15.73321244754782811 ) ) ;
#15119 = CARTESIAN_POINT ( 'NONE',  ( -6.010958268070873523, 4.863021950010647743, 18.20513189769810225 ) ) ;
#15120 = ORIENTED_EDGE ( 'NONE', *, *, #3223, .T. ) ;
#15121 = CARTESIAN_POINT ( 'NONE',  ( 0.7048096507298579061, 24.78213711671599029, -41.23648859290900504 ) ) ;
#15122 = B_SPLINE_CURVE_WITH_KNOTS ( 'NONE', 3,
 ( #15786, #48982, #10778, #6641, #26096, #44612, #34899, #49906, #34584, #59289, #39924, #1965, #54264, #58347, #1649, #40532 ),
 .UNSPECIFIED., .F., .F.,
 ( 4, 3, 3, 3, 3, 4 ),
 ( 2.081781105835003155E-17, 0.0002618515315864400794, 0.0003927756766341976660, 0.0005236998216950558300, 0.0007855159896329891398, 0.001047349442285927437 ),
 .UNSPECIFIED. ) ;
#15123 = ORIENTED_EDGE ( 'NONE', *, *, #57961, .T. ) ;
#15124 = EDGE_LOOP ( 'NONE', ( #49606, #3097, #21845, #49542 ) ) ;
#15125 = CARTESIAN_POINT ( 'NONE',  ( -6.077587904424778920, 7.788877841491745002, 17.61049128685084142 ) ) ;
#15126 = ORIENTED_EDGE ( 'NONE', *, *, #1116, .T. ) ;
#15127 = CARTESIAN_POINT ( 'NONE',  ( 0.6001305935487422083, 34.38748867424667566, 33.64689939321953460 ) ) ;
#15128 = CARTESIAN_POINT ( 'NONE',  ( 3.661933894777864573, 26.36408373158522878, 38.95595274082788961 ) ) ;
#15129 = B_SPLINE_CURVE_WITH_KNOTS ( 'NONE', 3,
 ( #14346, #39706, #53743, #10558 ),
 .UNSPECIFIED., .F., .F.,
 ( 4, 4 ),
 ( 4.654751537338637096E-17, 0.005004948556313857343 ),
 .UNSPECIFIED. ) ;
#15130 = EDGE_CURVE ( 'NONE', #37162, #34651, #47613, .T. ) ;
#15131 = CARTESIAN_POINT ( 'NONE',  ( -4.923482091946717709, -0.9563062221994661494, -2.999999999999945377 ) ) ;
#15132 = ORIENTED_EDGE ( 'NONE', *, *, #23090, .F. ) ;
#15133 = FACE_OUTER_BOUND ( 'NONE', #34451, .T. ) ;
#15134 = CARTESIAN_POINT ( 'NONE',  ( 4.975610109902397937, 48.43414999183897862, -6.825138951392602849 ) ) ;
#15135 = EDGE_LOOP ( 'NONE', ( #28785, #14605, #13371, #53596 ) ) ;
#15136 = EDGE_CURVE ( 'NONE', #10287, #48653, #661, .T. ) ;
#15137 = ORIENTED_EDGE ( 'NONE', *, *, #17712, .T. ) ;
#15138 = DIRECTION ( 'NONE',  ( 0.000000000000000000, 0.000000000000000000, -1.000000000000000000 ) ) ;
#15139 = CARTESIAN_POINT ( 'NONE',  ( 4.322998006666179727, 45.10383234877009784, 16.38761975793224934 ) ) ;
#15140 = CARTESIAN_POINT ( 'NONE',  ( 0.9730545539215883499, -41.31259007387239279, 11.59290486963492128 ) ) ;
#15141 = FACE_OUTER_BOUND ( 'NONE', #37722, .T. ) ;
#15142 = CARTESIAN_POINT ( 'NONE',  ( 0.8560838555295158248, -0.6537497281619772949, -46.90357604036880446 ) ) ;
#15143 = ORIENTED_EDGE ( 'NONE', *, *, #39922, .T. ) ;
#15144 = CARTESIAN_POINT ( 'NONE',  ( 0.1157991065609915854, -1.332877529279917983, -44.10403386346468579 ) ) ;
#15145 = CARTESIAN_POINT ( 'NONE',  ( 1.231276596079887264, -26.41281459480383376, 32.55211200826430229 ) ) ;
#15146 = B_SPLINE_CURVE_WITH_KNOTS ( 'NONE', 3,
 ( #57106, #49567, #31094, #2256, #1634, #44295 ),
 .UNSPECIFIED., .F., .F.,
 ( 4, 2, 4 ),
 ( 6.314488766312913488E-18, 0.0002291472222819943992, 0.0004582944445639824558 ),
 .UNSPECIFIED. ) ;
#15147 = CARTESIAN_POINT ( 'NONE',  ( 0.5806925824938494740, 36.46274162637944016, -29.49052111156159128 ) ) ;
#15148 = B_SPLINE_CURVE_WITH_KNOTS ( 'NONE', 3,
 ( #35830, #54899, #31108, #26402, #26712, #2588 ),
 .UNSPECIFIED., .F., .F.,
 ( 4, 2, 4 ),
 ( 1.519728548185745998E-16, 0.0002445252820015200571, 0.0004890505640028882176 ),
 .UNSPECIFIED. ) ;
#15149 = CARTESIAN_POINT ( 'NONE',  ( 2.528190830796658961, -41.36197007608242870, 7.172277712015144857 ) ) ;
#15150 = ORIENTED_EDGE ( 'NONE', *, *, #46686, .T. ) ;
#15151 = CARTESIAN_POINT ( 'NONE',  ( 0.8551540677456715978, -34.52115452272906282, -33.23105123575935949 ) ) ;
#15152 = CARTESIAN_POINT ( 'NONE',  ( 0.1135584504625007374, 37.21391936710485737, -23.70814749139775302 ) ) ;
#15153 = CARTESIAN_POINT ( 'NONE',  ( 1.227938101723748288, 0.8460948827231143943, -42.91134962331486236 ) ) ;
#15154 = CARTESIAN_POINT ( 'NONE',  ( 0.7056759521544979652, -35.34448603454957549, 30.83044171059700389 ) ) ;
#15155 = EDGE_CURVE ( 'NONE', #25145, #60457, #39421, .T. ) ;
#15156 = ORIENTED_EDGE ( 'NONE', *, *, #20619, .F. ) ;
#15157 = ORIENTED_EDGE ( 'NONE', *, *, #17284, .T. ) ;
#15158 = CARTESIAN_POINT ( 'NONE',  ( 4.975610109902397937, 7.237810502494805398, -48.37420290059309025 ) ) ;
#15159 = CARTESIAN_POINT ( 'NONE',  ( 3.270143674763207553, 3.277085381513114015, 13.28976595685394635 ) ) ;
#15160 = EDGE_CURVE ( 'NONE', #51214, #21652, #46855, .T. ) ;
#15161 = CARTESIAN_POINT ( 'NONE',  ( 3.238741278300273141, -38.11287256318076544, 19.89284324544627935 ) ) ;
#15162 = CARTESIAN_POINT ( 'NONE',  ( 4.553261556744873317, 43.53643125131393532, -5.841123155973635406 ) ) ;
#15163 = CARTESIAN_POINT ( 'NONE',  ( 2.526464513654346433, 6.809833384819025781, 42.43615126908559176 ) ) ;
#15164 = EDGE_CURVE ( 'NONE', #33009, #27817, #37876, .T. ) ;
#15165 = CARTESIAN_POINT ( 'NONE',  ( -6.015611763856276717, -2.465697960551179513, 18.68122482568278997 ) ) ;
#15166 = AXIS2_PLACEMENT_3D ( 'NONE', #42617, #61677, #47614 ) ;
#15167 = CARTESIAN_POINT ( 'NONE',  ( -11.40403086437694569, 0.6959691356230539583, -1.199999999999999956 ) ) ;
#15168 = LINE ( 'NONE', #5717, #6772 ) ;
#15169 = CARTESIAN_POINT ( 'NONE',  ( 5.895596859100789899, 12.98817590332804883, 15.35693556399505155 ) ) ;
#15170 = CARTESIAN_POINT ( 'NONE',  ( 0.1095718737110178143, 30.67477146794372800, -30.31138510522961838 ) ) ;
#15171 = DIRECTION ( 'NONE',  ( -0.000000000000000000, 0.000000000000000000, -1.000000000000000000 ) ) ;
#15172 = VERTEX_POINT ( 'NONE', #51295 ) ;
#15173 = B_SPLINE_CURVE_WITH_KNOTS ( 'NONE', 3,
 ( #48028, #77, #18919, #52709, #14828, #5390, #14526, #24514, #19841, #28596, #5078, #28294, #56787, #13917, #58011, #10431, #47411, #38959, #23908 ),
 .UNSPECIFIED., .F., .F.,
 ( 4, 3, 3, 3, 3, 3, 4 ),
 ( 0.000000000000000000, 0.0002724573126191766771, 0.0004086839781548628429, 0.0005449106435901976409, 0.0006811373090491553610, 0.0008459866663933662302, 0.001010840725717216402 ),
 .UNSPECIFIED. ) ;
#15174 = CARTESIAN_POINT ( 'NONE',  ( 0.1147471544378675795, -7.348573952980992807, -43.50805269522889773 ) ) ;
#15175 = CARTESIAN_POINT ( 'NONE',  ( 0.6845945791218023269, 33.22744374803170331, 33.11107824709630165 ) ) ;
#15176 = FACE_OUTER_BOUND ( 'NONE', #31017, .T. ) ;
#15177 = CARTESIAN_POINT ( 'NONE',  ( 0.8744876279028306332, -47.70753782033967383, -11.59055156152427557 ) ) ;
#15178 = EDGE_CURVE ( 'NONE', #10350, #30761, #52812, .T. ) ;
#15179 = LINE ( 'NONE', #39000, #50126 ) ;
#15180 = CARTESIAN_POINT ( 'NONE',  ( 0.5997462898726536595, 33.39998138387895921, -35.99990102348682797 ) ) ;
#15181 = LINE ( 'NONE', #34285, #30667 ) ;
#15182 = CARTESIAN_POINT ( 'NONE',  ( 3.238741278300275805, 9.350673766180220170, 41.96285461600083977 ) ) ;
#15183 = CARTESIAN_POINT ( 'NONE',  ( 0.7242486021783856032, 48.34643330280884044, -8.581016797036948418 ) ) ;
#15184 = CARTESIAN_POINT ( 'NONE',  ( 0.6026777506516367566, -30.48164694038906930, 38.50215046511933537 ) ) ;
#15185 = CARTESIAN_POINT ( 'NONE',  ( 0.7048096507298579061, -13.26491767067547478, 46.24547838151344337 ) ) ;
#15186 = CARTESIAN_POINT ( 'NONE',  ( 7.000000000000005329, 2.649999999999714806, 80.00000000000002842 ) ) ;
#15188 = ORIENTED_EDGE ( 'NONE', *, *, #45876, .T. ) ;
#15187 = CARTESIAN_POINT ( 'NONE',  ( 0.8751705887134553219, -7.160166390003972481, -47.55935879196468363 ) ) ;
#15189 = ORIENTED_EDGE ( 'NONE', *, *, #37727, .T. ) ;
#15190 = CARTESIAN_POINT ( 'NONE',  ( 0.5806925824938502512, -24.77160101449099727, 39.81946942793729249 ) ) ;
#15191 = DIRECTION ( 'NONE',  ( -0.000000000000000000, 1.287488025362403787E-15, 1.000000000000000000 ) ) ;
#15192 = CARTESIAN_POINT ( 'NONE',  ( 3.238741278300274029, 14.74792908357247256, 40.38334873621888477 ) ) ;
#15193 = ORIENTED_EDGE ( 'NONE', *, *, #52467, .T. ) ;
#15194 = CARTESIAN_POINT ( 'NONE',  ( 0.5837800304671222351, -45.96535232605464216, 9.296435753618650821 ) ) ;
#15195 = CARTESIAN_POINT ( 'NONE',  ( -6.016489644550737204, 17.40716454747929731, 7.215050741358106201 ) ) ;
#15196 = ORIENTED_EDGE ( 'NONE', *, *, #3513, .F. ) ;
#15197 = VERTEX_POINT ( 'NONE', #32219 ) ;
#15198 = B_SPLINE_CURVE_WITH_KNOTS ( 'NONE', 3,
 ( #5087, #58019, #709, #48338 ),
 .UNSPECIFIED., .F., .F.,
 ( 4, 4 ),
 ( 0.000000000000000000, 0.005014147105413699519 ),
 .UNSPECIFIED. ) ;
#15199 = CARTESIAN_POINT ( 'NONE',  ( 4.549368137175248350, 42.06008734272396765, -8.582197505783977221 ) ) ;
#15200 = EDGE_CURVE ( 'NONE', #18005, #35841, #7125, .T. ) ;
#15201 = CARTESIAN_POINT ( 'NONE',  ( 0.5807400328401637335, 29.58941477093070915, -37.66660715020834260 ) ) ;
#15202 = CARTESIAN_POINT ( 'NONE',  ( 4.963659409799329403, -19.36487359954728049, 40.34793212403964446 ) ) ;
#15203 = CARTESIAN_POINT ( 'NONE',  ( 0.1368894036331278763, -44.11864566353360573, 0.6375192066904099564 ) ) ;
#15204 = ADVANCED_FACE ( 'NONE', ( #18424 ), #2121, .T. ) ;
#15205 = CARTESIAN_POINT ( 'NONE',  ( 0.9791128995231617171, -41.06991714040155728, -8.342621909610549835 ) ) ;
#15206 = VECTOR ( 'NONE', #20009, 1000.000000000000227 ) ;
#15207 = EDGE_CURVE ( 'NONE', #18160, #28471, #61777, .T. ) ;
#15208 = CARTESIAN_POINT ( 'NONE',  ( -6.015611763856276717, -7.205255340944484388, -17.41126425312545223 ) ) ;
#15209 = CARTESIAN_POINT ( 'NONE',  ( 4.553261556744875094, 0.000000000000000000, 0.000000000000000000 ) ) ;
#15210 = VERTEX_POINT ( 'NONE', #26892 ) ;
#15211 = EDGE_CURVE ( 'NONE', #30629, #31192, #30397, .T. ) ;
#15212 = ADVANCED_FACE ( 'NONE', ( #29049 ), #51179, .T. ) ;
#15213 = ORIENTED_EDGE ( 'NONE', *, *, #54194, .T. ) ;
#15214 = CARTESIAN_POINT ( 'NONE',  ( 0.5997462898726536595, -2.096122762664449635, -49.06279547180479739 ) ) ;
#15215 = CARTESIAN_POINT ( 'NONE',  ( 3.782542959838399721, -42.02453062021629648, 1.084748610081117670 ) ) ;
#15216 = ORIENTED_EDGE ( 'NONE', *, *, #14045, .T. ) ;
#15217 = FACE_OUTER_BOUND ( 'NONE', #50120, .T. ) ;
#15218 = CARTESIAN_POINT ( 'NONE',  ( 0.7764139734771249302, 5.581186588129950721, -46.57135200072405468 ) ) ;
#15219 = DIRECTION ( 'NONE',  ( 0.1024043820194936449, -0.7971196296869297315, -0.5950744814819213246 ) ) ;
#15220 = CARTESIAN_POINT ( 'NONE',  ( 4.549368137175248350, 32.41327393324100825, 28.14399996863509301 ) ) ;
#15221 = ORIENTED_EDGE ( 'NONE', *, *, #58457, .T. ) ;
#15222 = CARTESIAN_POINT ( 'NONE',  ( 0.5824936645240097466, 46.52475202343088512, -5.889450585459719889 ) ) ;
#15223 = DIRECTION ( 'NONE',  ( 0.000000000000000000, 0.000000000000000000, 1.000000000000000000 ) ) ;
#15224 = CARTESIAN_POINT ( 'NONE',  ( 0.9730545539215883499, -42.90536227157002003, -0.5054011016617259155 ) ) ;
#15225 =( BOUNDED_SURFACE ( )  B_SPLINE_SURFACE ( 3, 1, ( 
 ( #4238, #55945 ),
 ( #12440, #8032 ),
 ( #41887, #27763 ),
 ( #8962, #46272 ) ),
 .UNSPECIFIED., .F., .F., .F. ) 
 B_SPLINE_SURFACE_WITH_KNOTS ( ( 4, 4 ),
 ( 2, 2 ),
 ( 0.000000000000000000, 1.000000000000000000 ),
 ( 0.000000000000000000, 1.000000000000000000 ),
 .UNSPECIFIED. ) 
 GEOMETRIC_REPRESENTATION_ITEM ( )  RATIONAL_B_SPLINE_SURFACE ( (
 ( 1.000000000000000000, 1.000000000000000000),
 ( 0.7269869731126821222, 0.9931720237060910339),
 ( 0.7269869731126821222, 0.9931720237060910339),
 ( 1.000000000000000000, 1.000000000000000000) ) ) 
 REPRESENTATION_ITEM ( '' )  SURFACE ( )  );
#15226 = CARTESIAN_POINT ( 'NONE',  ( 3.270143674763207553, -13.60381564321233228, -1.514386915940737710 ) ) ;
#15227 = ORIENTED_EDGE ( 'NONE', *, *, #9696, .T. ) ;
#15228 = CARTESIAN_POINT ( 'NONE',  ( 0.6029443449137436017, 4.758762304982984581, -48.87631041013637656 ) ) ;
#15229 = VERTEX_POINT ( 'NONE', #57842 ) ;
#15230 = CARTESIAN_POINT ( 'NONE',  ( 0.8760168074886960365, -23.27577685234568960, -42.09738177923946267 ) ) ;
#15231 = CARTESIAN_POINT ( 'NONE',  ( 0.5819845079324652559, 23.55367910461055558, -41.70428776698872753 ) ) ;
#15232 = EDGE_CURVE ( 'NONE', #52654, #18536, #12443, .T. ) ;
#15233 = ORIENTED_EDGE ( 'NONE', *, *, #20841, .F. ) ;
#15234 = CARTESIAN_POINT ( 'NONE',  ( 2.526552050251862358, -40.15571433620797137, 15.32056541070828537 ) ) ;
#15235 = EDGE_CURVE ( 'NONE', #56168, #2858, #4197, .T. ) ;
#15236 = CARTESIAN_POINT ( 'NONE',  ( -6.016761891674564211, 16.31696541414285306, -9.424569481870079812 ) ) ;
#15237 = FACE_OUTER_BOUND ( 'NONE', #39793, .T. ) ;
#15238 = EDGE_CURVE ( 'NONE', #52918, #60249, #42862, .T. ) ;
#15239 = CARTESIAN_POINT ( 'NONE',  ( -6.016761891674565099, -7.214149619366484245, 17.40752468084780702 ) ) ;
#15240 = CARTESIAN_POINT ( 'NONE',  ( 4.956445790444004906, -37.28933980949924631, -28.75835855384189443 ) ) ;
#15241 = CARTESIAN_POINT ( 'NONE',  ( 0.5800708119828327236, 5.628966929618427706, -47.56394195701280836 ) ) ;
#15242 = CARTESIAN_POINT ( 'NONE',  ( 0.6029303876144825880, 29.38970229176903359, -38.08638053211507923 ) ) ;
#15243 = B_SPLINE_CURVE_WITH_KNOTS ( 'NONE', 3,
 ( #22240, #46067, #3715, #41665 ),
 .UNSPECIFIED., .F., .F.,
 ( 4, 4 ),
 ( 8.359247967715799972E-17, 0.005004741218457506476 ),
 .UNSPECIFIED. ) ;
#15244 = CARTESIAN_POINT ( 'NONE',  ( 0.5809828226811617480, 47.89273459658653564, 0.5448590168534191980 ) ) ;
#15245 = ORIENTED_EDGE ( 'NONE', *, *, #47041, .F. ) ;
#15246 = CARTESIAN_POINT ( 'NONE',  ( 4.962356264823603702, 26.83784316460332420, -32.41860225448503030 ) ) ;
#15247 = CARTESIAN_POINT ( 'NONE',  ( 0.5997462898726536595, -20.35457962188166192, -44.69052157405179315 ) ) ;
#15248 = CARTESIAN_POINT ( 'NONE',  ( 3.221118495291108719, -16.06124188590834478, 40.94872316378246779 ) ) ;
#15249 = ORIENTED_EDGE ( 'NONE', *, *, #33975, .F. ) ;
#15250 = CARTESIAN_POINT ( 'NONE',  ( -15.87364823402127811, -12.50000869668378556, -0.1364485216735404627 ) ) ;
#15251 = DIRECTION ( 'NONE',  ( -0.8831157194574164038, 0.000000000000000000, 0.4691552259617384202 ) ) ;
#15252 = CARTESIAN_POINT ( 'NONE',  ( 0.6008122571543327295, 23.09929608320648953, 43.33563280864464673 ) ) ;
#15253 = CARTESIAN_POINT ( 'NONE',  ( 0.5797568665920712627, -44.50349591956066320, -14.78729723578712729 ) ) ;
#15254 = EDGE_CURVE ( 'NONE', #58067, #50843, #13198, .T. ) ;
#15255 =( REPRESENTATION_RELATIONSHIP ('NONE','NONE', #44881, #10831 ) REPRESENTATION_RELATIONSHIP_WITH_TRANSFORMATION ( #19267 )SHAPE_REPRESENTATION_RELATIONSHIP( ) );
#15256 = CARTESIAN_POINT ( 'NONE',  ( 0.7056555295713337062, -28.48870155114937219, 38.50897360867676156 ) ) ;
#15257 = AXIS2_PLACEMENT_3D ( 'NONE', #41389, #55135, #44857 ) ;
#15258 = CARTESIAN_POINT ( 'NONE',  ( 0.6030672727741701600, 38.21927534816984462, -29.21669544497209969 ) ) ;
#15259 = DIRECTION ( 'NONE',  ( 0.07836865515943411409, -0.1379401902675706781, 0.9873352307081156853 ) ) ;
#15260 = AXIS2_PLACEMENT_3D ( 'NONE', #47364, #60828, #57050 ) ;
#15261 = ADVANCED_FACE ( 'NONE', ( #57214 ), #3923, .F. ) ;
#15262 = DIRECTION ( 'NONE',  ( 0.000000000000000000, 0.000000000000000000, 1.000000000000000000 ) ) ;
#15263 = CARTESIAN_POINT ( 'NONE',  ( 3.270143674763207553, 10.69018354892887324, 8.548517033725294922 ) ) ;
#15265 = ORIENTED_EDGE ( 'NONE', *, *, #48813, .T. ) ;
#15264 = LINE ( 'NONE', #54356, #38346 ) ;
#15266 = EDGE_LOOP ( 'NONE', ( #15909, #50400, #60306, #35945 ) ) ;
#15267 = CARTESIAN_POINT ( 'NONE',  ( 0.5836750258453370366, -12.57171936981193916, 46.21662382526648116 ) ) ;
#15268 = FACE_OUTER_BOUND ( 'NONE', #23044, .T. ) ;
#15269 = CARTESIAN_POINT ( 'NONE',  ( 0.1100053167205930355, 16.66867746965590413, 39.77279469894219943 ) ) ;
#15270 = CARTESIAN_POINT ( 'NONE',  ( 0.1140933569871964842, -23.19718125549982801, 37.53452719674769611 ) ) ;
#15271 = CARTESIAN_POINT ( 'NONE',  ( 4.967162193818130511, 0.000000000000000000, 0.000000000000000000 ) ) ;
#15272 = CARTESIAN_POINT ( 'NONE',  ( 4.553261556744875094, -24.94552653848424129, -36.15605442441715667 ) ) ;
#15273 = B_SPLINE_CURVE_WITH_KNOTS ( 'NONE', 3,
 ( #30930, #44747, #36267, #50041, #21531, #46284 ),
 .UNSPECIFIED., .F., .F.,
 ( 4, 2, 4 ),
 ( 1.035625919765556564E-17, 0.0002291978881530155638, 0.0004583957763060207734 ),
 .UNSPECIFIED. ) ;
#15274 = B_SPLINE_CURVE_WITH_KNOTS ( 'NONE', 3,
 ( #39365, #5795, #43450, #492 ),
 .UNSPECIFIED., .F., .F.,
 ( 4, 4 ),
 ( 6.505213034913026604E-19, 0.004446298630425053744 ),
 .UNSPECIFIED. ) ;
#15275 = VERTEX_POINT ( 'NONE', #29657 ) ;
#15276 = CARTESIAN_POINT ( 'NONE',  ( 4.960156602257184133, 34.56254177294310637, -30.99165383632728421 ) ) ;
#15277 = DIRECTION ( 'NONE',  ( -0.9848077530122079093, -0.1736481776669316357, -2.245658157333249735E-31 ) ) ;
#15278 = CARTESIAN_POINT ( 'NONE',  ( 4.967162193818130511, 7.970725651239789045, 42.34252806656596846 ) ) ;
#15279 = EDGE_LOOP ( 'NONE', ( #49882, #42980, #30344, #45058 ) ) ;
#15280 = EDGE_CURVE ( 'NONE', #17545, #34842, #11012, .T. ) ;
#15281 = EDGE_CURVE ( 'NONE', #19329, #30492, #52024, .T. ) ;
#15282 = CARTESIAN_POINT ( 'NONE',  ( 0.9730545539215883499, 21.01499094264601908, -37.40983423658450846 ) ) ;
#15283 = CARTESIAN_POINT ( 'NONE',  ( 0.5835871038041856584, -25.11868534319529900, -39.60159213378984333 ) ) ;
#15284 = ORIENTED_EDGE ( 'NONE', *, *, #60880, .T. ) ;
#15285 = FACE_OUTER_BOUND ( 'NONE', #39314, .T. ) ;
#15286 = ORIENTED_EDGE ( 'NONE', *, *, #27598, .F. ) ;
#15287 = EDGE_CURVE ( 'NONE', #11600, #23542, #58783, .T. ) ;
#15288 = EDGE_CURVE ( 'NONE', #13993, #31436, #41632, .T. ) ;
#15289 = CARTESIAN_POINT ( 'NONE',  ( 0.9968887458511656030, -33.63815526548964385, -26.64009929991538783 ) ) ;
#15290 = CARTESIAN_POINT ( 'NONE',  ( 0.5980894510889448457, -19.05812566676535269, 44.17723055703920210 ) ) ;
#15291 = ORIENTED_EDGE ( 'NONE', *, *, #23680, .T. ) ;
#15292 = CARTESIAN_POINT ( 'NONE',  ( 5.910764540655178756, 19.00446553125916793, 6.582668785556910152 ) ) ;
#15293 = EDGE_CURVE ( 'NONE', #9430, #18146, #22866, .T. ) ;
#15294 = CARTESIAN_POINT ( 'NONE',  ( 0.8751705887134553219, -28.56654290188682666, 38.69254731947783199 ) ) ;
#15295 = CARTESIAN_POINT ( 'NONE',  ( 0.8744876279028263033, -48.57046782678510510, -7.159588358748426806 ) ) ;
#15296 = CARTESIAN_POINT ( 'NONE',  ( 4.967162193818130511, 32.68434214048205888, -28.07411493385260925 ) ) ;
#15297 = AXIS2_PLACEMENT_3D ( 'NONE', #49525, #44864, #10091 ) ;
#15298 = VERTEX_POINT ( 'NONE', #15886 ) ;
#15299 = CARTESIAN_POINT ( 'NONE',  ( 4.549368137175248350, 8.166781970325731166, -42.14271863032826104 ) ) ;
#15300 = CARTESIAN_POINT ( 'NONE',  ( 4.303969348037246512, -36.81598326424528977, -30.97035057417698312 ) ) ;
#15301 = ORIENTED_EDGE ( 'NONE', *, *, #4640, .T. ) ;
#15302 = DIRECTION ( 'NONE',  ( 0.07439287786467665975, -0.01320009283087630186, 0.9971416435352941088 ) ) ;
#15303 =( BOUNDED_SURFACE ( )  B_SPLINE_SURFACE ( 3, 1, ( 
 ( #29033, #24645 ),
 ( #34664, #10543 ),
 ( #24024, #44093 ),
 ( #826, #29638 ) ),
 .UNSPECIFIED., .F., .F., .F. ) 
 B_SPLINE_SURFACE_WITH_KNOTS ( ( 4, 4 ),
 ( 2, 2 ),
 ( 0.000000000000000000, 1.000000000000000000 ),
 ( 0.000000000000000000, 1.000000000000000000 ),
 .UNSPECIFIED. ) 
 GEOMETRIC_REPRESENTATION_ITEM ( )  RATIONAL_B_SPLINE_SURFACE ( (
 ( 1.000000000000000000, 1.000000000000000000),
 ( 0.7269869731126821222, 0.9931720237060910339),
 ( 0.7269869731126821222, 0.9931720237060910339),
 ( 1.000000000000000000, 1.000000000000000000) ) ) 
 REPRESENTATION_ITEM ( '' )  SURFACE ( )  );
#15304 = VECTOR ( 'NONE', #47661, 1000.000000000000114 ) ;
#15305 = EDGE_CURVE ( 'NONE', #21442, #25607, #14668, .T. ) ;
#15306 = B_SPLINE_CURVE_WITH_KNOTS ( 'NONE', 3,
 ( #8616, #27743, #55924, #61238, #46873, #8304, #22422, #46553, #15194, #52456, #58075, #23970, #4520, #766, #28661, #19907 ),
 .UNSPECIFIED., .F., .F.,
 ( 4, 3, 3, 3, 3, 4 ),
 ( 1.214354834101861724E-17, 0.0002732102107931876143, 0.0004098135523333793113, 0.0005464168938824958896, 0.0008195847345945451784, 0.001092771384553108301 ),
 .UNSPECIFIED. ) ;
#15307 = ORIENTED_EDGE ( 'NONE', *, *, #47885, .T. ) ;
#15308 = CARTESIAN_POINT ( 'NONE',  ( 0.8753041380234471980, 28.81806460335509001, -39.75748332565621723 ) ) ;
#15309 = ORIENTED_EDGE ( 'NONE', *, *, #35046, .F. ) ;
#15310 = CARTESIAN_POINT ( 'NONE',  ( 0.2940135542859014239, 36.52812816767694670, -24.73734830690602138 ) ) ;
#15311 = CARTESIAN_POINT ( 'NONE',  ( 0.9789889208857698311, 36.00916266840548730, -21.44003502708611464 ) ) ;
#15312 = CARTESIAN_POINT ( 'NONE',  ( 0.3676999524040323597, 10.61898383218351860, -42.81574203134477585 ) ) ;
#15313 = ORIENTED_EDGE ( 'NONE', *, *, #26763, .T. ) ;
#15314 = FACE_OUTER_BOUND ( 'NONE', #40307, .T. ) ;
#15315 = CARTESIAN_POINT ( 'NONE',  ( 0.5836750258453360374, -6.431686642655086494, 47.46217286060750951 ) ) ;
#15316 = CARTESIAN_POINT ( 'NONE',  ( 3.680882792899936362, -36.90742604464144705, 30.65151321162936782 ) ) ;
#15317 = EDGE_LOOP ( 'NONE', ( #27371, #51181, #44891, #44715 ) ) ;
#15318 = VERTEX_POINT ( 'NONE', #39708 ) ;
#15319 = CARTESIAN_POINT ( 'NONE',  ( 1.227938101723756947, 22.18841447410719780, 36.73927144310519566 ) ) ;
#15320 = CARTESIAN_POINT ( 'NONE',  ( 4.956445790443991584, 41.78282513192503700, 21.71942849465911252 ) ) ;
#15321 = CARTESIAN_POINT ( 'NONE',  ( 0.1104177457020372732, 30.49705356371264031, 30.49013195371466267 ) ) ;
#15322 = CIRCLE ( 'NONE', #35308, 47.91270532121795611 ) ;
#15323 = CARTESIAN_POINT ( 'NONE',  ( 2.618530812446115519, 15.57291328060520819, -44.35325423408014700 ) ) ;
#15324 = CARTESIAN_POINT ( 'NONE',  ( 0.6041374136657475802, -38.27243465845360504, 29.14743607025020466 ) ) ;
#15325 = ORIENTED_EDGE ( 'NONE', *, *, #10573, .F. ) ;
#15326 = CARTESIAN_POINT ( 'NONE',  ( 0.8560838555295223751, 40.81790744942443183, 23.11430867518979326 ) ) ;
#15327 = ORIENTED_EDGE ( 'NONE', *, *, #36554, .F. ) ;
#15328 = LINE ( 'NONE', #52586, #58356 ) ;
#15329 = CARTESIAN_POINT ( 'NONE',  ( 4.962356264823593932, 31.50371261889118557, 27.90612278853270922 ) ) ;
#15330 = CARTESIAN_POINT ( 'NONE',  ( 0.5997462898726536595, -25.90236585764231947, -41.72072714036939090 ) ) ;
#15331 = CARTESIAN_POINT ( 'NONE',  ( -6.078726893082806448, 18.62537590944121391, -4.887679766589349661 ) ) ;
#15332 = CARTESIAN_POINT ( 'NONE',  ( 0.7044674535452954967, -48.59206901384826693, -7.114320189892598734 ) ) ;
#15333 = FILL_AREA_STYLE_COLOUR ( '', #44897 ) ;
#15334 = CARTESIAN_POINT ( 'NONE',  ( 0.8551540677456739292, 46.51172240253136891, -11.51835730326431850 ) ) ;
#15335 = ADVANCED_FACE ( 'NONE', ( #54679 ), #16763, .F. ) ;
#15336 = CARTESIAN_POINT ( 'NONE',  ( 0.1158816050234199174, 20.40407993419151822, -39.12308223215911340 ) ) ;
#15337 = CARTESIAN_POINT ( 'NONE',  ( 4.335381028904201628, 26.25686719067146058, 41.35618179904649594 ) ) ;
#15338 = CARTESIAN_POINT ( 'NONE',  ( 0.8551540677456715978, 47.90804413217340851, 0.9122407826477486603 ) ) ;
#15339 = CARTESIAN_POINT ( 'NONE',  ( 0.9762797500689124330, 4.697980241568662230, 41.64437257103935508 ) ) ;
#15340 = CARTESIAN_POINT ( 'NONE',  ( 0.9762797500689124330, -41.77809974471938403, -3.303810967047359881 ) ) ;
#15341 = CARTESIAN_POINT ( 'NONE',  ( 0.9780303403264757334, -34.36697018299320661, 23.98439021189286535 ) ) ;
#15342 = CARTESIAN_POINT ( 'NONE',  ( 4.975801465491694664, 42.71626295676232843, 21.70134120755216145 ) ) ;
#15343 = B_SPLINE_CURVE_WITH_KNOTS ( 'NONE', 3,
 ( #310, #37651, #14761, #15, #52948, #33257, #38269, #4693, #23521, #47338, #52327, #10053, #29150, #48268, #32629, #61105, #56409, #13525, #9419 ),
 .UNSPECIFIED., .F., .F.,
 ( 4, 3, 3, 3, 3, 3, 4 ),
 ( 0.000000000000000000, 0.0002724573126191739665, 0.0004086839781548579098, 0.0005449106435901954724, 0.0006811373090491585052, 0.0008459866663933821680, 0.001010840725717218353 ),
 .UNSPECIFIED. ) ;
#15344 = B_SPLINE_CURVE_WITH_KNOTS ( 'NONE', 3,
 ( #42798, #53088, #43733, #47796 ),
 .UNSPECIFIED., .F., .F.,
 ( 4, 4 ),
 ( 0.000000000000000000, 0.005004741218457414535 ),
 .UNSPECIFIED. ) ;
#15345 = ORIENTED_EDGE ( 'NONE', *, *, #55929, .F. ) ;
#15346 = CARTESIAN_POINT ( 'NONE',  ( 0.9762797500689124330, -6.471194619075235188, -41.40589843715211771 ) ) ;
#15347 = DIRECTION ( 'NONE',  ( 0.000000000000000000, 0.000000000000000000, 1.000000000000000000 ) ) ;
#15348 = CARTESIAN_POINT ( 'NONE',  ( 1.657374760986086049, 24.17973270432427313, -36.82704133649178146 ) ) ;
#15349 = CARTESIAN_POINT ( 'NONE',  ( 2.281448460670573386, 11.14236343022437659, -46.66132715497951011 ) ) ;
#15350 = CARTESIAN_POINT ( 'NONE',  ( 5.896782393890504181, -19.93252920631901404, -2.687073932226577533 ) ) ;
#15351 = ORIENTED_EDGE ( 'NONE', *, *, #52354, .T. ) ;
#15352 = ADVANCED_FACE ( 'NONE', ( #25576 ), #59181, .F. ) ;
#15353 = CARTESIAN_POINT ( 'NONE',  ( 0.9757892942422835558, -37.13414688883477766, 21.49867881049932095 ) ) ;
#15354 = CARTESIAN_POINT ( 'NONE',  ( 0.9754402186311943446, 16.24692483025473067, -39.71365199966000148 ) ) ;
#15355 = VECTOR ( 'NONE', #9863, 1000.000000000000227 ) ;
#15356 = EDGE_CURVE ( 'NONE', #25455, #8551, #26189, .T. ) ;
#15357 = DIRECTION ( 'NONE',  ( 0.000000000000000000, 0.000000000000000000, 1.000000000000000000 ) ) ;
#15358 = ORIENTED_EDGE ( 'NONE', *, *, #51649, .F. ) ;
#15359 = DIRECTION ( 'NONE',  ( 1.000000000000000000, 0.000000000000000000, 0.000000000000000000 ) ) ;
#15360 = ADVANCED_FACE ( 'NONE', ( #31199 ), #23166, .F. ) ;
#15361 = CARTESIAN_POINT ( 'NONE',  ( 4.956653778116990594, -3.690426056929668075, -47.94889704119055551 ) ) ;
#15362 = EDGE_LOOP ( 'NONE', ( #13472, #14929, #17004, #58034 ) ) ;
#15363 = ADVANCED_FACE ( 'NONE', ( #6132 ), #5927, .F. ) ;
#15364 = CARTESIAN_POINT ( 'NONE',  ( -6.078075953587585900, -6.655346486686461560, 18.06935354098995461 ) ) ;
#15365 = VERTEX_POINT ( 'NONE', #8012 ) ;
#15366 = CARTESIAN_POINT ( 'NONE',  ( -5.995132425357893702, 17.41298668506980718, -7.203480333238889699 ) ) ;
#15367 = ADVANCED_FACE ( 'NONE', ( #55299 ), #7687, .F. ) ;
#15368 = VERTEX_POINT ( 'NONE', #41866 ) ;
#15369 = CARTESIAN_POINT ( 'NONE',  ( 0.1368894036331270714, -13.16414094522229838, -42.11373551583444907 ) ) ;
#15370 = CARTESIAN_POINT ( 'NONE',  ( 0.6254311100348657337, -28.73641524052546004, -38.58047947916320197 ) ) ;
#15371 = ORIENTED_EDGE ( 'NONE', *, *, #22794, .T. ) ;
#15372 = CARTESIAN_POINT ( 'NONE',  ( 0.5987334308729318488, 4.112662331024658613, -48.93515009807060778 ) ) ;
#15373 = VERTEX_POINT ( 'NONE', #22734 ) ;
#15374 = DIRECTION ( 'NONE',  ( -0.07836865515943412797, -0.4916162952473555614, 0.8672783706145142935 ) ) ;
#15375 = CARTESIAN_POINT ( 'NONE',  ( 0.9730545539215883499, -5.099196237954599198, -42.60426903087358852 ) ) ;
#15376 = CARTESIAN_POINT ( 'NONE',  ( 0.5835226383429296115, 40.44198222182293989, 23.74212603192314575 ) ) ;
#15377 =( BOUNDED_SURFACE ( )  B_SPLINE_SURFACE ( 3, 1, ( 
 ( #13920, #38340 ),
 ( #5394, #23298 ),
 ( #14832, #33023 ),
 ( #18603, #43660 ) ),
 .UNSPECIFIED., .F., .F., .F. ) 
 B_SPLINE_SURFACE_WITH_KNOTS ( ( 4, 4 ),
 ( 2, 2 ),
 ( 0.000000000000000000, 1.000000000000000000 ),
 ( 0.000000000000000000, 1.000000000000000000 ),
 .UNSPECIFIED. ) 
 GEOMETRIC_REPRESENTATION_ITEM ( )  RATIONAL_B_SPLINE_SURFACE ( (
 ( 1.000000000000000000, 1.000000000000000000),
 ( 0.9953040768229013402, 0.8617119497784988535),
 ( 0.9953040768229013402, 0.8617119497784988535),
 ( 1.000000000000000000, 1.000000000000000000) ) ) 
 REPRESENTATION_ITEM ( '' )  SURFACE ( )  );
#15378 = EDGE_LOOP ( 'NONE', ( #13229, #18664, #55240, #57871 ) ) ;
#15379 = CARTESIAN_POINT ( 'NONE',  ( 0.5848930533535030563, -38.55997537638081951, -26.69084826978085800 ) ) ;
#15380 = CARTESIAN_POINT ( 'NONE',  ( 4.553261556744875094, 0.000000000000000000, 0.000000000000000000 ) ) ;
#15381 = ADVANCED_FACE ( 'NONE', ( #26815, #27424, #60304 ), #36232, .T. ) ;
#15382 = CARTESIAN_POINT ( 'NONE',  ( 0.5834584762367737154, 32.73240943502174360, -33.58311125538091346 ) ) ;
#15383 = CARTESIAN_POINT ( 'NONE',  ( 0.6000166863083090663, -45.32251430608278753, 18.91277818522110010 ) ) ;
#15384 = ORIENTED_EDGE ( 'NONE', *, *, #42801, .F. ) ;
#15385 = CARTESIAN_POINT ( 'NONE',  ( 0.3676999524040323597, 3.413584541508654091, 43.98065510995502336 ) ) ;
#15386 = EDGE_CURVE ( 'NONE', #6658, #39805, #35202, .T. ) ;
#15387 = CARTESIAN_POINT ( 'NONE',  ( 0.1129192098497455998, -18.30288010335110016, 40.14917642626692640 ) ) ;
#15388 = ORIENTED_EDGE ( 'NONE', *, *, #1330, .T. ) ;
#15389 = CIRCLE ( 'NONE', #2339, 5.633200000000004870 ) ;
#15390 = CARTESIAN_POINT ( 'NONE',  ( 4.975801465491695552, 0.000000000000000000, 0.000000000000000000 ) ) ;
#15391 = ORIENTED_EDGE ( 'NONE', *, *, #40438, .F. ) ;
#15392 = CARTESIAN_POINT ( 'NONE',  ( -6.010958268070873523, 13.33459572764757617, 13.31406649671967379 ) ) ;
#15393 = CARTESIAN_POINT ( 'NONE',  ( 0.1155031312995260795, 25.10578313294615427, 36.28555202574827376 ) ) ;
#15394 = ORIENTED_EDGE ( 'NONE', *, *, #13443, .F. ) ;
#15395 = DIRECTION ( 'NONE',  ( 0.09722883295013592941, 0.9469132758617033740, 0.3064340092744473054 ) ) ;
#15396 = CARTESIAN_POINT ( 'NONE',  ( 4.962356264823602814, -25.31392337492848554, -33.62202970123303203 ) ) ;
#15397 = CARTESIAN_POINT ( 'NONE',  ( 51.18991377541220800, 12.23415317001104086, 2.564509504438283294 ) ) ;
#15398 = DIRECTION ( 'NONE',  ( -0.000000000000000000, -0.000000000000000000, 1.000000000000000000 ) ) ;
#15399 = VERTEX_POINT ( 'NONE', #4213 ) ;
#15400 = CARTESIAN_POINT ( 'NONE',  ( 0.6025881611877910160, 18.61132239451786319, -44.36157157392734973 ) ) ;
#15401 = FACE_OUTER_BOUND ( 'NONE', #12908, .T. ) ;
#15402 = CIRCLE ( 'NONE', #16367, 48.91267123290010943 ) ;
#15403 = CARTESIAN_POINT ( 'NONE',  ( 0.8760168074886965917, 0.8912768426706281222, -48.09529047980637273 ) ) ;
#15404 = CARTESIAN_POINT ( 'NONE',  ( 1.092182651088191792, 20.82421885325586430, 36.37462155946074915 ) ) ;
#15405 = ADVANCED_FACE ( 'NONE', ( #60009 ), #42755, .F. ) ;
#15406 = DIRECTION ( 'NONE',  ( 0.000000000000000000, 0.000000000000000000, 1.000000000000000000 ) ) ;
#15407 = CARTESIAN_POINT ( 'NONE',  ( 0.7056555295713251574, 33.27140645154245391, -34.46100226633700458 ) ) ;
#15408 = CARTESIAN_POINT ( 'NONE',  ( -15.98202953935055959, -7.972086415228249123, 0.6796618530310959416 ) ) ;
#15409 = CARTESIAN_POINT ( 'NONE',  ( 0.8557997880470690211, 23.15977007032381607, -41.93815086860232810 ) ) ;
#15410 = DIRECTION ( 'NONE',  ( -1.000000000000000000, 0.000000000000000000, 0.000000000000000000 ) ) ;
#15411 = CARTESIAN_POINT ( 'NONE',  ( 0.5837800005270571413, -1.566997147869758411, 46.86981735168539132 ) ) ;
#15412 = CARTESIAN_POINT ( 'NONE',  ( 0.3676999524040323597, -38.02468164711575582, -22.36233818182566324 ) ) ;
#15413 = ORIENTED_EDGE ( 'NONE', *, *, #43659, .T. ) ;
#15414 = CARTESIAN_POINT ( 'NONE',  ( 0.5836750258453368145, 29.30109045202441820, -37.88760409476664393 ) ) ;
#15415 = CARTESIAN_POINT ( 'NONE',  ( 2.706805983486679779, 18.87354163078242664, -39.75632703898686060 ) ) ;
#15416 = CARTESIAN_POINT ( 'NONE',  ( 4.962356264823608143, 6.570263404306589727, 41.57002810511892221 ) ) ;
#15417 = ORIENTED_EDGE ( 'NONE', *, *, #45373, .F. ) ;
#15418 = CARTESIAN_POINT ( 'NONE',  ( 4.999999999999986677, 56.56854249492450037, -56.56854249492312192 ) ) ;
#15419 = DIRECTION ( 'NONE',  ( 0.07439287786467665975, 0.7991213610169868309, -0.5965490341031238763 ) ) ;
#15420 = VECTOR ( 'NONE', #25720, 1000.000000000000227 ) ;
#15421 = PRODUCT_DEFINITION_CONTEXT ( 'detailed design', #18800, 'design' ) ;
#15422 = EDGE_LOOP ( 'NONE', ( #42505, #59941, #57835, #30617 ) ) ;
#15423 = ORIENTED_EDGE ( 'NONE', *, *, #45629, .T. ) ;
#15424 = B_SPLINE_CURVE_WITH_KNOTS ( 'NONE', 3,
 ( #51985, #9077, #43544, #43237 ),
 .UNSPECIFIED., .F., .F.,
 ( 4, 4 ),
 ( 7.757919228897728493E-17, 0.005004741218457496067 ),
 .UNSPECIFIED. ) ;
#15425 = CARTESIAN_POINT ( 'NONE',  ( 0.5786265663353196143, -38.43785771743223023, 28.58414684753472201 ) ) ;
#15426 = EDGE_CURVE ( 'NONE', #25300, #38104, #42192, .T. ) ;
#15427 = ORIENTED_EDGE ( 'NONE', *, *, #6830, .F. ) ;
#15428 = CARTESIAN_POINT ( 'NONE',  ( 0.7056313189692703380, 28.49521968211951872, 37.25279988437523571 ) ) ;
#15429 = ORIENTED_EDGE ( 'NONE', *, *, #32636, .T. ) ;
#15430 = EDGE_CURVE ( 'NONE', #10841, #8991, #58151, .T. ) ;
#15431 = ORIENTED_EDGE ( 'NONE', *, *, #48538, .T. ) ;
#15432 = CARTESIAN_POINT ( 'NONE',  ( 0.6000166863083106206, -48.63754814943177252, -6.797969676319517873 ) ) ;
#15433 = VERTEX_POINT ( 'NONE', #56541 ) ;
#15434 = CARTESIAN_POINT ( 'NONE',  ( 0.3622758884714600280, 43.10531414739104150, 0.8252992914329575491 ) ) ;
#15435 = CARTESIAN_POINT ( 'NONE',  ( 0.9730545539215892381, 39.44597740938061037, 16.88610103448572630 ) ) ;
#15436 = AXIS2_PLACEMENT_3D ( 'NONE', #27318, #23242, #7898 ) ;
#15437 = CARTESIAN_POINT ( 'NONE',  ( 1.231276596079887931, -37.78837162824473950, -18.14705873423390869 ) ) ;
#15438 = ORIENTED_EDGE ( 'NONE', *, *, #41923, .F. ) ;
#15439 = CARTESIAN_POINT ( 'NONE',  ( 0.1103936448916675722, 0.03072591687002976246, 43.12443171339901937 ) ) ;
#15440 = CARTESIAN_POINT ( 'NONE',  ( -1.318516776095821186, -3.857556137907092175, -1.739862437281285109E-14 ) ) ;
#15441 = ORIENTED_EDGE ( 'NONE', *, *, #23685, .T. ) ;
#15442 = VERTEX_POINT ( 'NONE', #45951 ) ;
#15443 = CARTESIAN_POINT ( 'NONE',  ( 0.1157506346131639274, 43.29263408050130835, -8.525754756891059216 ) ) ;
#15444 = CARTESIAN_POINT ( 'NONE',  ( 47.85015878647476484, 12.49996633727064932, 0.3510238927397298925 ) ) ;
#15445 = CARTESIAN_POINT ( 'NONE',  ( 0.8557997880470599172, 24.73961900479308440, -41.02602466100753276 ) ) ;
#15446 = CARTESIAN_POINT ( 'NONE',  ( 0.9762797500689124330, 36.31338395866797697, 20.92039508843128814 ) ) ;
#15447 = EDGE_CURVE ( 'NONE', #17462, #50427, #46247, .T. ) ;
#15448 = ORIENTED_EDGE ( 'NONE', *, *, #6139, .T. ) ;
#15449 = CARTESIAN_POINT ( 'NONE',  ( 0.1135584504625008623, -0.9824315139179617962, -44.11334129779462643 ) ) ;
#15450 = CARTESIAN_POINT ( 'NONE',  ( 4.549368137175248350, -3.018832571116875751, 42.82045902618767030 ) ) ;
#15451 = FACE_OUTER_BOUND ( 'NONE', #51970, .T. ) ;
#15452 = CARTESIAN_POINT ( 'NONE',  ( 0.3622758884714730732, -31.06363466427707820, -29.89648521331620756 ) ) ;
#15453 = ORIENTED_EDGE ( 'NONE', *, *, #54161, .T. ) ;
#15454 = CARTESIAN_POINT ( 'NONE',  ( 4.390527457369401532, -43.06122069908267491, -8.713013745743406702 ) ) ;
#15455 = CARTESIAN_POINT ( 'NONE',  ( 0.1073791018717578927, 42.68962945260945929, 6.109314776652849943 ) ) ;
#15456 = CARTESIAN_POINT ( 'NONE',  ( 1.227938101723747621, -20.72293514920724533, -37.58536632582800507 ) ) ;
#15457 = CARTESIAN_POINT ( 'NONE',  ( 0.6028777368367060907, -35.21566487464662742, -34.22567423364589700 ) ) ;
#15458 = ORIENTED_EDGE ( 'NONE', *, *, #30827, .T. ) ;
#15459 = VERTEX_POINT ( 'NONE', #47171 ) ;
#15460 = DIRECTION ( 'NONE',  ( 1.000000000000000000, 1.836970198721027715E-16, -2.218671295934095703E-31 ) ) ;
#15461 = CARTESIAN_POINT ( 'NONE',  ( 3.678748215320120529, -3.416822541561816529, -48.85630090396691827 ) ) ;
#15462 = CARTESIAN_POINT ( 'NONE',  ( 8.000000000000007105, -54.69470952477895764, -58.44237546506863623 ) ) ;
#15463 = B_SPLINE_CURVE_WITH_KNOTS ( 'NONE', 3,
 ( #53187, #53485, #31548, #30934, #45989, #55031 ),
 .UNSPECIFIED., .F., .F.,
 ( 4, 2, 4 ),
 ( 1.870559545977334001E-17, 0.0002293319059085097372, 0.0004586638118170007720 ),
 .UNSPECIFIED. ) ;
#15464 = CARTESIAN_POINT ( 'NONE',  ( -6.078726893082806448, -12.94836301907731801, -14.25250631976393656 ) ) ;
#15465 = CARTESIAN_POINT ( 'NONE',  ( 0.1100053167205930771, 34.10339839758286473, -26.39466280306232449 ) ) ;
#15466 = CARTESIAN_POINT ( 'NONE',  ( 4.694002226626921015, 12.64038892846058282, 43.80074587473810510 ) ) ;
#15467 =( BOUNDED_SURFACE ( )  B_SPLINE_SURFACE ( 3, 1, ( 
 ( #54970, #17709 ),
 ( #13027, #2350 ),
 ( #59678, #32122 ),
 ( #26476, #16792 ) ),
 .UNSPECIFIED., .F., .F., .F. ) 
 B_SPLINE_SURFACE_WITH_KNOTS ( ( 4, 4 ),
 ( 2, 2 ),
 ( 0.000000000000000000, 1.000000000000000000 ),
 ( 0.000000000000000000, 1.000000000000000000 ),
 .UNSPECIFIED. ) 
 GEOMETRIC_REPRESENTATION_ITEM ( )  RATIONAL_B_SPLINE_SURFACE ( (
 ( 1.000000000000000000, 1.000000000000000000),
 ( 0.9953390228620291325, 0.8624445117760984880),
 ( 0.9953390228620291325, 0.8624445117760984880),
 ( 1.000000000000000000, 1.000000000000000000) ) ) 
 REPRESENTATION_ITEM ( '' )  SURFACE ( )  );
#15468 = CARTESIAN_POINT ( 'NONE',  ( 0.9791128995231628274, 9.710313423905196473, -40.76821368978151128 ) ) ;
#15469 = CARTESIAN_POINT ( 'NONE',  ( 4.962356264823608143, 7.429277797797782412, -41.42513040734446861 ) ) ;
#15470 = EDGE_CURVE ( 'NONE', #51356, #29746, #53439, .T. ) ;
#15471 = CARTESIAN_POINT ( 'NONE',  ( 4.549368137175248350, -40.71620287708334018, -13.59764261105737404 ) ) ;
#15472 = CIRCLE ( 'NONE', #39502, 13.00000000000000178 ) ;
#15473 = CARTESIAN_POINT ( 'NONE',  ( 0.9775691876210961251, -1.022782437399945232, -41.89615286724711751 ) ) ;
#15474 = FACE_OUTER_BOUND ( 'NONE', #51098, .T. ) ;
#15475 = ORIENTED_EDGE ( 'NONE', *, *, #41972, .F. ) ;
#15476 = B_SPLINE_CURVE_WITH_KNOTS ( 'NONE', 3,
 ( #5806, #24643, #53728, #24956, #39078, #58131 ),
 .UNSPECIFIED., .F., .F.,
 ( 4, 2, 4 ),
 ( 0.000000000000000000, 0.0002447195606305743666, 0.0004894391212611487333 ),
 .UNSPECIFIED. ) ;
#15477 = CARTESIAN_POINT ( 'NONE',  ( 4.967162193818130511, 0.000000000000000000, 0.000000000000000000 ) ) ;
#15478 = CARTESIAN_POINT ( 'NONE',  ( 2.618530812446111078, 39.70953715621322999, 25.15709538157219072 ) ) ;
#15479 = CARTESIAN_POINT ( 'NONE',  ( 0.1154773475650540393, -35.25385042465135399, 26.53506473107669450 ) ) ;
#15480 = CARTESIAN_POINT ( 'NONE',  ( 0.5782707292762423457, 37.25243273660916543, 28.49548400908516399 ) ) ;
#15481 = CIRCLE ( 'NONE', #29461, 43.08621763946400307 ) ;
#15482 = CARTESIAN_POINT ( 'NONE',  ( -6.001507490154111224, 7.225628667346816414, -17.40350523682687722 ) ) ;
#15483 = CARTESIAN_POINT ( 'NONE',  ( 0.6021447746440204973, 32.82110281078899305, -36.52829518841669199 ) ) ;
#15484 = EDGE_CURVE ( 'NONE', #36659, #42702, #15306, .T. ) ;
#15485 = CARTESIAN_POINT ( 'NONE',  ( 3.782625744892852193, 11.41484085274463567, 40.45910913998868352 ) ) ;
#15486 = CARTESIAN_POINT ( 'NONE',  ( 2.281351352603294913, 19.56575819747284584, -43.80196780981699334 ) ) ;
#15487 =( BOUNDED_SURFACE ( )  B_SPLINE_SURFACE ( 3, 1, ( 
 ( #127, #4209 ),
 ( #18658, #48084 ),
 ( #4517, #42782 ),
 ( #24266, #23966 ) ),
 .UNSPECIFIED., .F., .F., .F. ) 
 B_SPLINE_SURFACE_WITH_KNOTS ( ( 4, 4 ),
 ( 2, 2 ),
 ( 0.000000000000000000, 1.000000000000000000 ),
 ( 0.000000000000000000, 1.000000000000000000 ),
 .UNSPECIFIED. ) 
 GEOMETRIC_REPRESENTATION_ITEM ( )  RATIONAL_B_SPLINE_SURFACE ( (
 ( 1.000000000000000000, 1.000000000000000000),
 ( 0.7223157951917476005, 0.9931996967497186413),
 ( 0.7223157951917476005, 0.9931996967497186413),
 ( 1.000000000000000000, 1.000000000000000000) ) ) 
 REPRESENTATION_ITEM ( '' )  SURFACE ( )  );
#15488 = CARTESIAN_POINT ( 'NONE',  ( 0.9756008150404597012, -10.96816689273726908, 41.48296819691550752 ) ) ;
#15489 = CARTESIAN_POINT ( 'NONE',  ( -6.015611763856276717, 4.870987357968431297, -18.20278301740931681 ) ) ;
#15490 = CARTESIAN_POINT ( 'NONE',  ( 0.6016118706126977189, 49.02773421256183894, -2.798630516221145115 ) ) ;
#15492 = ORIENTED_EDGE ( 'NONE', *, *, #15160, .F. ) ;
#15491 = CARTESIAN_POINT ( 'NONE',  ( 4.975610109902397937, -17.43163075979644816, -45.70106843599929647 ) ) ;
#15493 = ORIENTED_EDGE ( 'NONE', *, *, #17200, .T. ) ;
#15494 = CARTESIAN_POINT ( 'NONE',  ( 0.1073791018717578927, -43.12183934961191056, -0.4849339620931655825 ) ) ;
#15495 = CARTESIAN_POINT ( 'NONE',  ( 2.185380717157383135, 43.82594162643527369, -4.255190198274171998 ) ) ;
#15496 = CARTESIAN_POINT ( 'NONE',  ( 0.9754292589017200532, -34.21816598153960598, 24.19596213741219515 ) ) ;
#15497 = ORIENTED_EDGE ( 'NONE', *, *, #4496, .F. ) ;
#15498 = ORIENTED_EDGE ( 'NONE', *, *, #56245, .T. ) ;
#15499 = CARTESIAN_POINT ( 'NONE',  ( 0.1092355843206037486, -11.45151637801156497, 41.57624119012368880 ) ) ;
#15500 = CARTESIAN_POINT ( 'NONE',  ( 5.901764892641307547, 7.858096707079341492, -48.33468509861078388 ) ) ;
#15501 = CARTESIAN_POINT ( 'NONE',  ( 4.549368137175248350, 0.000000000000000000, 0.000000000000000000 ) ) ;
#15502 = ORIENTED_EDGE ( 'NONE', *, *, #33601, .T. ) ;
#15503 = AXIS2_PLACEMENT_3D ( 'NONE', #49595, #40246, #55523 ) ;
#15504 = VERTEX_POINT ( 'NONE', #43096 ) ;
#15505 = CARTESIAN_POINT ( 'NONE',  ( -6.016761891674564211, -18.20023637398602290, 4.880293656734900232 ) ) ;
#15506 = EDGE_CURVE ( 'NONE', #59587, #10433, #55658, .T. ) ;
#15507 = CARTESIAN_POINT ( 'NONE',  ( 4.967162193818130511, 0.000000000000000000, 0.000000000000000000 ) ) ;
#15508 = CARTESIAN_POINT ( 'NONE',  ( 4.956653778116975495, 26.26162724282373517, 40.28700667097690769 ) ) ;
#15509 = LINE ( 'NONE', #49015, #31922 ) ;
#15510 = EDGE_CURVE ( 'NONE', #41881, #46997, #22186, .T. ) ;
#15511 = CARTESIAN_POINT ( 'NONE',  ( 0.9789233960466707796, -41.04249736261641601, -8.476446016578329079 ) ) ;
#15512 = CARTESIAN_POINT ( 'NONE',  ( 4.975610109902397937, 42.89797504594920241, 23.49921581872238718 ) ) ;
#15513 = EDGE_CURVE ( 'NONE', #28003, #39250, #38498, .T. ) ;
#15514 = CARTESIAN_POINT ( 'NONE',  ( 0.1149546198390367924, 15.49570923134082534, -41.31379382773940279 ) ) ;
#15515 = ORIENTED_EDGE ( 'NONE', *, *, #20625, .T. ) ;
#15516 = VERTEX_POINT ( 'NONE', #18661 ) ;
#15517 = CARTESIAN_POINT ( 'NONE',  ( 2.528100132419516477, 33.68154901921120370, 25.05607779159677406 ) ) ;
#15518 = CARTESIAN_POINT ( 'NONE',  ( 0.3676999524040323597, -40.57213187173838520, -17.31625533148287843 ) ) ;
#15519 = ORIENTED_EDGE ( 'NONE', *, *, #12113, .F. ) ;
#15520 = CARTESIAN_POINT ( 'NONE',  ( 2.643462169533613793, 46.02269433264232390, -13.76277278785512692 ) ) ;
#15521 = CARTESIAN_POINT ( 'NONE',  ( 4.303969348037258058, -32.45857549159325828, 35.51084504003185316 ) ) ;
#15522 = CARTESIAN_POINT ( 'NONE',  ( -2.569797478183783568, -11.87678401312189003, -8.547745408040752224 ) ) ;
#15523 = CARTESIAN_POINT ( 'NONE',  ( 0.1157991065609916270, -40.86881191294364868, -16.63377823472870531 ) ) ;
#15524 = EDGE_CURVE ( 'NONE', #10739, #25025, #51893, .T. ) ;
#15525 = CIRCLE ( 'NONE', #50519, 47.91270532121795611 ) ;
#15526 = B_SPLINE_CURVE_WITH_KNOTS ( 'NONE', 3,
 ( #15775, #34889, #15461, #34574 ),
 .UNSPECIFIED., .F., .F.,
 ( 4, 4 ),
 ( 0.000000000000000000, 0.004442905043737216571 ),
 .UNSPECIFIED. ) ;
#15527 = ORIENTED_EDGE ( 'NONE', *, *, #11620, .T. ) ;
#15528 = DIRECTION ( 'NONE',  ( 0.000000000000000000, 0.000000000000000000, 1.000000000000000000 ) ) ;
#15529 = CARTESIAN_POINT ( 'NONE',  ( 4.962356264823603702, 17.31942680647464528, -38.35717733303005161 ) ) ;
#15530 = CARTESIAN_POINT ( 'NONE',  ( 5.272380000000000067, 1.530808498934191324E-15, -12.49999999999999822 ) ) ;
#15531 = CARTESIAN_POINT ( 'NONE',  ( 5.895596859100789899, 17.94951300836806141, 9.074313526372865368 ) ) ;
#15532 = EDGE_LOOP ( 'NONE', ( #21426, #35862, #10154, #26934 ) ) ;
#15533 = CARTESIAN_POINT ( 'NONE',  ( 5.959547316686252039, 20.52562247508876681, -0.003562808152693846490 ) ) ;
#15534 = CARTESIAN_POINT ( 'NONE',  ( 4.553261556744875094, -29.36425772793644029, -32.66925058691983708 ) ) ;
#15535 = ORIENTED_EDGE ( 'NONE', *, *, #22063, .F. ) ;
#15536 = CARTESIAN_POINT ( 'NONE',  ( 2.282803330402963127, -2.882084055115845977, 46.88486428428933550 ) ) ;
#15537 = CARTESIAN_POINT ( 'NONE',  ( 0.5809828226811617480, 24.41822904836982389, -41.20389530892281726 ) ) ;
#15538 = ORIENTED_EDGE ( 'NONE', *, *, #16051, .F. ) ;
#15539 = CARTESIAN_POINT ( 'NONE',  ( 0.5848930533535030563, -1.749067435711075591, -46.86377967570363978 ) ) ;
#15540 = CARTESIAN_POINT ( 'NONE',  ( 3.238018933889920792, -4.230209958194933506, -12.70876925895034759 ) ) ;
#15541 = DIRECTION ( 'NONE',  ( 0.07500201931887537365, -0.9127009170568822771, -0.4016861126571554808 ) ) ;
#15542 = CARTESIAN_POINT ( 'NONE',  ( -6.016761891674564211, -7.207804629151436160, 17.41015286184800459 ) ) ;
#15543 = CARTESIAN_POINT ( 'NONE',  ( 0.9762797500689124330, 38.38274741215490593, -16.82526333465304091 ) ) ;
#15544 = CARTESIAN_POINT ( 'NONE',  ( 0.3676999524040366896, -31.10876963919527682, 31.27610965031171020 ) ) ;
#15545 = CARTESIAN_POINT ( 'NONE',  ( 0.8760168074887090262, -46.68716261866168082, -11.58706983520309741 ) ) ;
#15546 = DIRECTION ( 'NONE',  ( -1.000000000000000000, -3.135800716341471541E-16, -1.298891185607920445E-16 ) ) ;
#15547 = ORIENTED_EDGE ( 'NONE', *, *, #38718, .T. ) ;
#15548 = CARTESIAN_POINT ( 'NONE',  ( 5.896782393890504181, -20.11283288166117345, -0.006352352428112362746 ) ) ;
#15549 = CARTESIAN_POINT ( 'NONE',  ( 0.9769922540276034795, 41.47347701830330635, 6.023475665958448744 ) ) ;
#15550 = CARTESIAN_POINT ( 'NONE',  ( 0.5837157313716023754, 27.89101090674457240, -37.70051159045296885 ) ) ;
#15551 = B_SPLINE_CURVE_WITH_KNOTS ( 'NONE', 3,
 ( #16378, #35501, #30773, #49892 ),
 .UNSPECIFIED., .F., .F.,
 ( 4, 4 ),
 ( 1.192622389734054877E-18, 0.004444878191957666105 ),
 .UNSPECIFIED. ) ;
#15552 = EDGE_LOOP ( 'NONE', ( #54777, #56630 ) ) ;
#15553 = EDGE_CURVE ( 'NONE', #12288, #44917, #24585, .T. ) ;
#15554 = CARTESIAN_POINT ( 'NONE',  ( 0.5807400328401637335, -5.711437504336293713, 47.55718917606841956 ) ) ;
#15555 = CARTESIAN_POINT ( 'NONE',  ( 3.661933894777891219, 24.23903144487420747, -40.31253551398190638 ) ) ;
#15556 = CARTESIAN_POINT ( 'NONE',  ( 50.00005079999999680, 12.80000000000000071, 3.000000000000000000 ) ) ;
#15557 = CARTESIAN_POINT ( 'NONE',  ( 4.549368137175248350, 0.000000000000000000, 0.000000000000000000 ) ) ;
#15558 = CARTESIAN_POINT ( 'NONE',  ( 0.5980894510889457338, 44.71414919659881093, 17.76188940524963300 ) ) ;
#15559 = CARTESIAN_POINT ( 'NONE',  ( 0.6017666602106489515, 37.95277954208636118, -29.56224131406230171 ) ) ;
#15560 = EDGE_CURVE ( 'NONE', #46829, #12599, #7846, .T. ) ;
#15561 = CARTESIAN_POINT ( 'NONE',  ( 14.99999999999999289, 56.56854249492425879, 56.56854249492337061 ) ) ;
#15562 = CARTESIAN_POINT ( 'NONE',  ( 5.910764540655177868, -9.651974367317830428, -17.64484710281737634 ) ) ;
#15563 = CARTESIAN_POINT ( 'NONE',  ( 0.6025881611877910160, -0.2181813582441801125, 48.10699274197334319 ) ) ;
#15564 = STYLED_ITEM ( 'NONE', ( #13675 ), #7748 ) ;
#15565 = EDGE_CURVE ( 'NONE', #28832, #60778, #26486, .T. ) ;
#15566 = CARTESIAN_POINT ( 'NONE',  ( 0.9787284016396621267, 28.99970135845135033, -30.25480656109806432 ) ) ;
#15568 = VERTEX_POINT ( 'NONE', #14896 ) ;
#15567 = DIRECTION ( 'NONE',  ( 1.836970198721031906E-16, -1.000000000000000000, 1.110223024625156540E-16 ) ) ;
#15569 = ORIENTED_EDGE ( 'NONE', *, *, #48733, .T. ) ;
#15570 = CARTESIAN_POINT ( 'NONE',  ( 0.6846871229502899947, -37.47592888575268688, 29.84551600520619274 ) ) ;
#15571 = AXIS2_PLACEMENT_3D ( 'NONE', #51698, #8789, #18508 ) ;
#15572 = CARTESIAN_POINT ( 'NONE',  ( 4.303969348037258058, -47.93217632892346103, -4.133486515473800083 ) ) ;
#15573 = CARTESIAN_POINT ( 'NONE',  ( 0.5804410086790514622, 22.05813747677497716, -41.38790189066235570 ) ) ;
#15574 = VECTOR ( 'NONE', #5106, 1000.000000000000114 ) ;
#15575 = DIRECTION ( 'NONE',  ( 0.1024043820194936449, -0.7126273545981441915, -0.6940285268068283608 ) ) ;
#15576 = CARTESIAN_POINT ( 'NONE',  ( 0.8554163680231738898, -6.900908941296520993, -46.40671211038068833 ) ) ;
#15577 = CARTESIAN_POINT ( 'NONE',  ( 0.5998501479064699549, 11.94461217097469685, -46.60114184914306179 ) ) ;
#15578 = B_SPLINE_CURVE_WITH_KNOTS ( 'NONE', 3,
 ( #15577, #10563, #44113, #43801, #34377, #53451 ),
 .UNSPECIFIED., .F., .F.,
 ( 4, 2, 4 ),
 ( 1.764953265579307567E-18, 0.0002450742804987340135, 0.0004901485609974661839 ),
 .UNSPECIFIED. ) ;
#15579 = ORIENTED_EDGE ( 'NONE', *, *, #10378, .F. ) ;
#15580 = EDGE_LOOP ( 'NONE', ( #7630, #10757, #42908, #46118 ) ) ;
#15581 = CARTESIAN_POINT ( 'NONE',  ( 0.2224561200757615154, -4.874377913226201287, -42.84309024201774463 ) ) ;
#15582 = ADVANCED_FACE ( 'NONE', ( #53075 ), #28162, .T. ) ;
#15583 = CARTESIAN_POINT ( 'NONE',  ( 2.643462169533613793, -28.13401304854749085, 38.93558293168490536 ) ) ;
#15584 = CARTESIAN_POINT ( 'NONE',  ( 0.5809828226811617480, 41.74875432577682233, -23.47450554821666202 ) ) ;
#15585 = EDGE_CURVE ( 'NONE', #22596, #50555, #39020, .T. ) ;
#15586 = ORIENTED_EDGE ( 'NONE', *, *, #16298, .T. ) ;
#15587 = CARTESIAN_POINT ( 'NONE',  ( 0.1313383488274115496, 37.02311703718855540, -22.11173226734854325 ) ) ;
#15588 = EDGE_CURVE ( 'NONE', #32480, #20677, #48088, .T. ) ;
#15589 = CARTESIAN_POINT ( 'NONE',  ( 40.00000000000000000, 0.000000000000000000, 0.000000000000000000 ) ) ;
#15590 = ORIENTED_EDGE ( 'NONE', *, *, #19840, .T. ) ;
#15591 = APPLICATION_CONTEXT ( 'automotive_design' ) ;
#15592 =( BOUNDED_SURFACE ( )  B_SPLINE_SURFACE ( 3, 1, ( 
 ( #49018, #6069 ),
 ( #44347, #1376 ),
 ( #20515, #27061 ),
 ( #17362, #3539 ) ),
 .UNSPECIFIED., .F., .F., .F. ) 
 B_SPLINE_SURFACE_WITH_KNOTS ( ( 4, 4 ),
 ( 2, 2 ),
 ( 0.000000000000000000, 1.000000000000000000 ),
 ( 0.000000000000000000, 1.000000000000000000 ),
 .UNSPECIFIED. ) 
 GEOMETRIC_REPRESENTATION_ITEM ( )  RATIONAL_B_SPLINE_SURFACE ( (
 ( 1.000000000000000000, 1.000000000000000000),
 ( 0.9953485035131437453, 0.8621029689291523912),
 ( 0.9953485035131437453, 0.8621029689291523912),
 ( 1.000000000000000000, 1.000000000000000000) ) ) 
 REPRESENTATION_ITEM ( '' )  SURFACE ( )  );
#15593 = DIRECTION ( 'NONE',  ( 1.000000000000000000, 0.000000000000000000, 0.000000000000000000 ) ) ;
#15594 = ORIENTED_EDGE ( 'NONE', *, *, #39480, .T. ) ;
#15595 = CARTESIAN_POINT ( 'NONE',  ( 0.5817216825391120505, -34.47346183105885586, 31.79332290890629764 ) ) ;
#15596 = FACE_OUTER_BOUND ( 'NONE', #3711, .T. ) ;
#15597 = B_SPLINE_CURVE_WITH_KNOTS ( 'NONE', 3,
 ( #42374, #18547, #28863, #37676, #38597, #5341, #23546, #10076, #24475, #37360, #13548, #32654, #42676, #61738, #51737, #20102 ),
 .UNSPECIFIED., .F., .F.,
 ( 4, 3, 3, 3, 3, 4 ),
 ( 1.250973872328959318E-17, 0.0002724568934985534328, 0.0004086836638483776533, 0.0005449104342063536104, 0.0008173270854453626617, 0.001089761613562690310 ),
 .UNSPECIFIED. ) ;
#15598 = ORIENTED_EDGE ( 'NONE', *, *, #40702, .F. ) ;
#15599 = CARTESIAN_POINT ( 'NONE',  ( 4.335381028904216727, 26.25686719067205033, -41.35618179904614067 ) ) ;
#15600 = CARTESIAN_POINT ( 'NONE',  ( 5.838029081930957709, 47.13000430274633601, 3.134924652369162956 ) ) ;
#15601 = DIRECTION ( 'NONE',  ( 0.000000000000000000, 0.000000000000000000, 1.000000000000000000 ) ) ;
#15602 = CARTESIAN_POINT ( 'NONE',  ( 0.6039202388192953519, 4.888815891286212967, 48.86372061182098747 ) ) ;
#15603 = B_SPLINE_CURVE_WITH_KNOTS ( 'NONE', 3,
 ( #60411, #60724, #56032, #46356, #46663, #27233 ),
 .UNSPECIFIED., .F., .F.,
 ( 4, 2, 4 ),
 ( 0.000000000000000000, 0.0002291459268755698824, 0.0004582918537511397649 ),
 .UNSPECIFIED. ) ;
#15604 = ADVANCED_FACE ( 'NONE', ( #43721 ), #33192, .T. ) ;
#15605 = EDGE_LOOP ( 'NONE', ( #28972, #43608, #56693, #38857, #24437, #7820 ) ) ;
#15606 = LINE ( 'NONE', #34405, #24725 ) ;
#15607 = CARTESIAN_POINT ( 'NONE',  ( 0.6031356755825967308, -1.709377936827843777E-05, -48.10744332413644031 ) ) ;
#15608 = ORIENTED_EDGE ( 'NONE', *, *, #30401, .F. ) ;
#15609 = CARTESIAN_POINT ( 'NONE',  ( 4.967162193818130511, 0.000000000000000000, 0.000000000000000000 ) ) ;
#15610 = ORIENTED_EDGE ( 'NONE', *, *, #5112, .F. ) ;
#15611 = CARTESIAN_POINT ( 'NONE',  ( 1.231276596079887931, -39.86997064245532840, -12.94844438486017779 ) ) ;
#15612 = VERTEX_POINT ( 'NONE', #37792 ) ;
#15613 = CARTESIAN_POINT ( 'NONE',  ( 1.157643937452369043, -31.63536294457205145, -27.49920155131693988 ) ) ;
#15614 = CARTESIAN_POINT ( 'NONE',  ( 0.6021448801613057400, -48.67017654873032484, -6.538734842641000355 ) ) ;
#15615 = TOROIDAL_SURFACE ( 'NONE', #18604, 5.633200000000004870, 0.02570000000000859444 ) ;
#15616 = CARTESIAN_POINT ( 'NONE',  ( -6.078457390727109555, 16.78028475769473005, 9.445451523785720838 ) ) ;
#15617 = ORIENTED_EDGE ( 'NONE', *, *, #13901, .F. ) ;
#15618 = CARTESIAN_POINT ( 'NONE',  ( 0.1129192098497447394, -35.64954734424924965, -26.00118385641864194 ) ) ;
#15619 = CARTESIAN_POINT ( 'NONE',  ( 0.5839254288179557273, -6.341681103464875235, 47.47429404163006694 ) ) ;
#15620 = CARTESIAN_POINT ( 'NONE',  ( 4.549368137175248350, 0.000000000000000000, 0.000000000000000000 ) ) ;
#15621 = AXIS2_PLACEMENT_3D ( 'NONE', #43314, #57981, #5357 ) ;
#15622 = VERTEX_POINT ( 'NONE', #56846 ) ;
#15623 = B_SPLINE_CURVE_WITH_KNOTS ( 'NONE', 3,
 ( #58813, #2421, #1802, #51892, #8986, #13706, #51572, #60351, #28096, #55657, #26863, #36907, #3956, #41296, #50965, #23398, #27787, #56278, #8664 ),
 .UNSPECIFIED., .F., .F.,
 ( 4, 3, 3, 3, 3, 3, 4 ),
 ( 1.165802754517233128E-16, 0.0002618519381806228810, 0.0003927759815485970052, 0.0005237000248299436469, 0.0006546240681324961988, 0.0007855481115631307576, 0.0009699050456655114840 ),
 .UNSPECIFIED. ) ;
#15624 = ORIENTED_EDGE ( 'NONE', *, *, #15989, .F. ) ;
#15625 = CARTESIAN_POINT ( 'NONE',  ( 0.9780303403264766215, -31.29797956580119944, -27.87070304986538360 ) ) ;
#15626 = CARTESIAN_POINT ( 'NONE',  ( 3.894904216938897878, 31.16049771651687195, 31.00238240095667663 ) ) ;
#15627 = CARTESIAN_POINT ( 'NONE',  ( 0.8560838555295158248, -38.14845555156047396, -27.29593693413630362 ) ) ;
#15628 = CARTESIAN_POINT ( 'NONE',  ( -2.569797478183790229, 5.182550149005106022, 13.68441171582018079 ) ) ;
#15629 = CARTESIAN_POINT ( 'NONE',  ( 0.9783242366443545279, -26.85209652948670467, -32.17606878065826947 ) ) ;
#15630 = CARTESIAN_POINT ( 'NONE',  ( -6.015611763856276717, -2.465697960550925938, -18.68122482568282550 ) ) ;
#15631 = ORIENTED_EDGE ( 'NONE', *, *, #8440, .T. ) ;
#15632 = VECTOR ( 'NONE', #8371, 1000.000000000000114 ) ;
#15633 = CARTESIAN_POINT ( 'NONE',  ( 0.8751705887134423323, 46.67919521768887847, -11.58504748649151317 ) ) ;
#15634 = ORIENTED_EDGE ( 'NONE', *, *, #18197, .F. ) ;
#15635 = EDGE_CURVE ( 'NONE', #2290, #35035, #13978, .T. ) ;
#15636 = CARTESIAN_POINT ( 'NONE',  ( 10.00000000000000533, 1.836909530733574959E-15, -1.925929944387237167E-31 ) ) ;
#15637 = CARTESIAN_POINT ( 'NONE',  ( 0.6016118706126977189, -19.55889245893339279, -45.04443118259803214 ) ) ;
#15638 = CARTESIAN_POINT ( 'NONE',  ( 4.549368137175248350, -13.59764261105721950, -40.71620287708339703 ) ) ;
#15639 = CARTESIAN_POINT ( 'NONE',  ( 0.8751705887134423323, -5.393078191592370452, -47.79200036674278351 ) ) ;
#15640 = CARTESIAN_POINT ( 'NONE',  ( 0.8751705887134423323, -37.60752970653809513, -29.98056538504947710 ) ) ;
#15641 = ADVANCED_FACE ( 'NONE', ( #47472 ), #23660, .F. ) ;
#15642 =( NAMED_UNIT ( * ) PLANE_ANGLE_UNIT ( ) SI_UNIT ( $, .RADIAN. ) );
#15643 = CARTESIAN_POINT ( 'NONE',  ( 0.5804410086790514622, 32.20888702807360460, 34.08969709851039909 ) ) ;
#15644 = CARTESIAN_POINT ( 'NONE',  ( -2.739355103387247858, -9.100462108390344085, -11.83339158334450580 ) ) ;
#15645 = CARTESIAN_POINT ( 'NONE',  ( -6.016761891674564211, -17.40752468084787452, 7.214149619366299504 ) ) ;
#15646 = EDGE_CURVE ( 'NONE', #34181, #38682, #5153, .T. ) ;
#15647 = CARTESIAN_POINT ( 'NONE',  ( -6.072942160501519915, 3.087637228657821975, 19.00712126107544719 ) ) ;
#15648 = EDGE_CURVE ( 'NONE', #30211, #5781, #37724, .T. ) ;
#15649 = LINE ( 'NONE', #11563, #24856 ) ;
#15650 = EDGE_CURVE ( 'NONE', #48653, #9174, #58637, .T. ) ;
#15651 = CARTESIAN_POINT ( 'NONE',  ( 4.549368137175248350, 0.000000000000000000, 0.000000000000000000 ) ) ;
#15652 = DIRECTION ( 'NONE',  ( 0.1024043820194936311, 0.9573600124648758980, -0.2701391291102754333 ) ) ;
#15653 = CARTESIAN_POINT ( 'NONE',  ( 3.660176727303410260, -45.87883389004760915, -14.24118031989642574 ) ) ;
#15654 = CARTESIAN_POINT ( 'NONE',  ( 5.896278296736517710, -7.223603833371336158, 18.77089575041337000 ) ) ;
#15655 = ADVANCED_FACE ( 'NONE', ( #26120 ), #35996, .F. ) ;
#15656 = VERTEX_POINT ( 'NONE', #49004 ) ;
#15657 = CIRCLE ( 'NONE', #4602, 15.50000000000000000 ) ;
#15658 = EDGE_CURVE ( 'NONE', #26755, #22273, #28055, .T. ) ;
#15659 = CARTESIAN_POINT ( 'NONE',  ( -2.708315649062910779, -14.20182604343562360, 3.532515819624108655 ) ) ;
#15660 = AXIS2_PLACEMENT_3D ( 'NONE', #35642, #35328, #16210 ) ;
#15661 = CARTESIAN_POINT ( 'NONE',  ( 0.5839879327111922036, 18.24507200299104426, -44.28486549479607959 ) ) ;
#15662 = CARTESIAN_POINT ( 'NONE',  ( 2.359973842542475886, 40.29593983161778681, 17.73057042847576170 ) ) ;
#15663 = CARTESIAN_POINT ( 'NONE',  ( 4.975801465491695552, 0.000000000000000000, 0.000000000000000000 ) ) ;
#15664 = EDGE_LOOP ( 'NONE', ( #30806, #31931 ) ) ;
#15665 = CARTESIAN_POINT ( 'NONE',  ( 4.960386119450151732, -30.75418163181185705, 31.12260877288193583 ) ) ;
#15666 = CARTESIAN_POINT ( 'NONE',  ( 0.6028777368367059797, 28.16654571100842830, -40.22667687021567673 ) ) ;
#15667 = B_SPLINE_CURVE_WITH_KNOTS ( 'NONE', 3,
 ( #14337, #8678, #33441, #9608, #28725, #32201 ),
 .UNSPECIFIED., .F., .F.,
 ( 4, 2, 4 ),
 ( 9.215718466126787689E-19, 0.0002293801035737121367, 0.0004587602071474233519 ),
 .UNSPECIFIED. ) ;
#15668 = CARTESIAN_POINT ( 'NONE',  ( 4.833616638992205949, 41.67905425467705527, -20.04871863793763964 ) ) ;
#15669 =( BOUNDED_SURFACE ( )  B_SPLINE_SURFACE ( 3, 1, ( 
 ( #899, #18797 ),
 ( #20037, #24097 ),
 ( #39151, #23475 ),
 ( #13795, #42920 ) ),
 .UNSPECIFIED., .F., .F., .F. ) 
 B_SPLINE_SURFACE_WITH_KNOTS ( ( 4, 4 ),
 ( 2, 2 ),
 ( 0.000000000000000000, 1.000000000000000000 ),
 ( 0.000000000000000000, 1.000000000000000000 ),
 .UNSPECIFIED. ) 
 GEOMETRIC_REPRESENTATION_ITEM ( )  RATIONAL_B_SPLINE_SURFACE ( (
 ( 1.000000000000000000, 1.000000000000000000),
 ( 0.9953390228620291325, 0.8624445117760984880),
 ( 0.9953390228620291325, 0.8624445117760984880),
 ( 1.000000000000000000, 1.000000000000000000) ) ) 
 REPRESENTATION_ITEM ( '' )  SURFACE ( )  );
#15670 = ORIENTED_EDGE ( 'NONE', *, *, #38573, .F. ) ;
#15671 = CARTESIAN_POINT ( 'NONE',  ( 0.7048096507298635682, 47.80151517212779311, 5.442192462019629140 ) ) ;
#15672 = CARTESIAN_POINT ( 'NONE',  ( 0.6067375320500723035, 23.33187539052128301, 41.82999795871614879 ) ) ;
#15673 = ORIENTED_EDGE ( 'NONE', *, *, #7431, .F. ) ;
#15674 = VECTOR ( 'NONE', #47372, 1000.000000000000114 ) ;
#15675 = CARTESIAN_POINT ( 'NONE',  ( 3.270143674763207553, 0.2742231296311491984, -13.68510027222512981 ) ) ;
#15676 = VERTEX_POINT ( 'NONE', #39626 ) ;
#15677 = CARTESIAN_POINT ( 'NONE',  ( 5.960721111146673579, -12.50019045452726907, -16.28018152803688778 ) ) ;
#15678 = ORIENTED_EDGE ( 'NONE', *, *, #639, .F. ) ;
#15679 = CARTESIAN_POINT ( 'NONE',  ( 2.299652685299202304, 48.83329552428664755, 4.426169121920126237 ) ) ;
#15680 = CARTESIAN_POINT ( 'NONE',  ( 4.549368137175248350, 28.14399996863453168, 32.41327393324149853 ) ) ;
#15681 = VERTEX_POINT ( 'NONE', #6985 ) ;
#15682 = CARTESIAN_POINT ( 'NONE',  ( 7.000000000000006217, 1.285836671513502038E-15, -1.348150961071066192E-31 ) ) ;
#15683 = ADVANCED_FACE ( 'NONE', ( #44335 ), #10802, .T. ) ;
#15684 = ORIENTED_EDGE ( 'NONE', *, *, #31973, .F. ) ;
#15685 = CARTESIAN_POINT ( 'NONE',  ( 4.553261556744875094, 0.000000000000000000, 0.000000000000000000 ) ) ;
#15686 = CARTESIAN_POINT ( 'NONE',  ( 0.1154773475650540393, -1.234467219940398319, 44.10691239169902644 ) ) ;
#15687 = ADVANCED_FACE ( 'NONE', ( #40257 ), #12379, .F. ) ;
#15688 = VERTEX_POINT ( 'NONE', #44949 ) ;
#15689 = CARTESIAN_POINT ( 'NONE',  ( -6.078726893082806448, -17.35055002122458490, 8.351793533709011896 ) ) ;
#15690 = CARTESIAN_POINT ( 'NONE',  ( 1.657374760986086715, -36.03312162084205283, -25.34767432152008482 ) ) ;
#15691 = CARTESIAN_POINT ( 'NONE',  ( 0.1368894036331280983, -32.13611142736034054, -30.23461043657771441 ) ) ;
#15692 = CARTESIAN_POINT ( 'NONE',  ( 0.6017667736363750963, 44.31084570541175083, 18.73201910948677096 ) ) ;
#15693 = ORIENTED_EDGE ( 'NONE', *, *, #45962, .F. ) ;
#15694 = DIRECTION ( 'NONE',  ( 0.000000000000000000, 0.000000000000000000, 1.000000000000000000 ) ) ;
#15695 = CARTESIAN_POINT ( 'NONE',  ( 0.5839254288179548391, -44.28478521851634753, 18.24509008251461850 ) ) ;
#15696 = ORIENTED_EDGE ( 'NONE', *, *, #8063, .T. ) ;
#15697 = CARTESIAN_POINT ( 'NONE',  ( 0.5800708119828333897, 47.40012378203040555, -6.873289505980164193 ) ) ;
#15698 = ORIENTED_EDGE ( 'NONE', *, *, #38930, .F. ) ;
#15699 = CARTESIAN_POINT ( 'NONE',  ( 1.231276596079887264, -2.246340108599748309, -41.85965512441022440 ) ) ;
#15700 = CARTESIAN_POINT ( 'NONE',  ( 0.000000000000000000, 0.000000000000000000, -1.199999999999999956 ) ) ;
#15701 = ORIENTED_EDGE ( 'NONE', *, *, #27446, .T. ) ;
#15702 = CARTESIAN_POINT ( 'NONE',  ( 4.975610109902397937, 45.11887670192734134, 18.88746601040093154 ) ) ;
#15703 = CARTESIAN_POINT ( 'NONE',  ( 0.5997462898726536595, 48.09935696025624452, 9.899671214447447909 ) ) ;
#15704 = CARTESIAN_POINT ( 'NONE',  ( 50.50000000000000000, 12.21587082446438011, 2.649999999999992806 ) ) ;
#15705 = CARTESIAN_POINT ( 'NONE',  ( 0.6064782688330851990, -39.06168768307265537, 25.95224463835178952 ) ) ;
#15706 = VECTOR ( 'NONE', #39989, 999.9999999999998863 ) ;
#15707 =( GEOMETRIC_REPRESENTATION_CONTEXT ( 3 ) GLOBAL_UNCERTAINTY_ASSIGNED_CONTEXT ( ( #28578 ) ) GLOBAL_UNIT_ASSIGNED_CONTEXT ( ( #40801, #36092, #26980 ) ) REPRESENTATION_CONTEXT ( 'NONE', 'WORKASPACE' ) );
#15708 = VERTEX_POINT ( 'NONE', #21114 ) ;
#15709 = CARTESIAN_POINT ( 'NONE',  ( 0.5997462898726536595, -30.20781297212564454, -38.71743361310750231 ) ) ;
#15710 = VECTOR ( 'NONE', #23907, 1000.000000000000000 ) ;
#15711 = CARTESIAN_POINT ( 'NONE',  ( -4.000000000000000000, 0.000000000000000000, -5.599999999999999645 ) ) ;
#15712 = B_SPLINE_CURVE_WITH_KNOTS ( 'NONE', 3,
 ( #39707, #45025, #39091, #40025, #58756, #35301, #54364, #58447, #34681, #25270, #11486, #19661, #30573, #29348, #25575, #58146, #15270, #53745, #24972 ),
 .UNSPECIFIED., .F., .F.,
 ( 4, 3, 3, 3, 3, 3, 4 ),
 ( 3.469552829456483146E-18, 0.0002612768053151673722, 0.0003919133833142922265, 0.0005225499612322564167, 0.0006531865391693380185, 0.0008112755173415141111, 0.0009693688056799736573 ),
 .UNSPECIFIED. ) ;
#15713 = ADVANCED_FACE ( 'NONE', ( #55765 ), #48166, .T. ) ;
#15714 =( LENGTH_UNIT ( ) NAMED_UNIT ( * ) SI_UNIT ( .MILLI., .METRE. ) );
#15715 = DIRECTION ( 'NONE',  ( 0.000000000000000000, 0.000000000000000000, 1.000000000000000000 ) ) ;
#15716 = CARTESIAN_POINT ( 'NONE',  ( 5.880360259849752858, -39.86101557989652378, -26.69116321728556329 ) ) ;
#15717 = ADVANCED_FACE ( 'NONE', ( #22276 ), #44416, .F. ) ;
#15718 = AXIS2_PLACEMENT_3D ( 'NONE', #22657, #43016, #61452 ) ;
#15719 = CARTESIAN_POINT ( 'NONE',  ( 0.5997462898726536595, -7.321308210775074876, -48.55872811583048332 ) ) ;
#15720 = EDGE_CURVE ( 'NONE', #44327, #3716, #16074, .T. ) ;
#15721 = EDGE_CURVE ( 'NONE', #43021, #54546, #51372, .T. ) ;
#15722 = CARTESIAN_POINT ( 'NONE',  ( -15.94137352497273419, -7.982459924543421792, 0.5466233485435718631 ) ) ;
#15723 = CARTESIAN_POINT ( 'NONE',  ( 4.553261556744875094, 38.16266689001181334, 21.75202109381179483 ) ) ;
#15724 = CARTESIAN_POINT ( 'NONE',  ( 0.6254087463353920073, 47.60024110474252979, -6.960754339421318271 ) ) ;
#15725 = CARTESIAN_POINT ( 'NONE',  ( 5.960721111146673579, -19.82454228767742066, -5.318514366754864220 ) ) ;
#15726 = CARTESIAN_POINT ( 'NONE',  ( 4.834790513006555379, -10.06429236341644362, 46.16599787882916672 ) ) ;
#15727 = CARTESIAN_POINT ( 'NONE',  ( 4.956445790443988031, 0.000000000000000000, 0.000000000000000000 ) ) ;
#15728 = CARTESIAN_POINT ( 'NONE',  ( 0.5809828226811617480, 33.48000389720616710, 34.25055090842165839 ) ) ;
#15729 = CARTESIAN_POINT ( 'NONE',  ( 0.1140933569871964287, 36.77173631030485268, 24.38830372964288529 ) ) ;
#15730 = ORIENTED_EDGE ( 'NONE', *, *, #35236, .F. ) ;
#15731 = CARTESIAN_POINT ( 'NONE',  ( -2.708315649062916552, -7.087851317224052039, 12.80362818457433427 ) ) ;
#15732 = CARTESIAN_POINT ( 'NONE',  ( 0.8744876279028306332, -6.955970791788286256, 48.60004650947653460 ) ) ;
#15733 = CARTESIAN_POINT ( 'NONE',  ( 0.9762797500689124330, 38.38274741215490593, -16.82526333465304091 ) ) ;
#15734 = ORIENTED_EDGE ( 'NONE', *, *, #2128, .T. ) ;
#15735 = CARTESIAN_POINT ( 'NONE',  ( 1.227938101723748288, 10.28900963485380693, 41.66816631169195517 ) ) ;
#15736 = CARTESIAN_POINT ( 'NONE',  ( 0.1158403557922069033, 4.199242128790555917, 43.92387360795505202 ) ) ;
#15737 = VERTEX_POINT ( 'NONE', #42325 ) ;
#15738 = VERTEX_POINT ( 'NONE', #51687 ) ;
#15739 = LINE ( 'NONE', #1921, #1535 ) ;
#15741 = ORIENTED_EDGE ( 'NONE', *, *, #47307, .F. ) ;
#15740 =( BOUNDED_SURFACE ( )  B_SPLINE_SURFACE ( 3, 1, ( 
 ( #38185, #28757 ),
 ( #33163, #15290 ),
 ( #14676, #34396 ),
 ( #24063, #42884 ) ),
 .UNSPECIFIED., .F., .F., .F. ) 
 B_SPLINE_SURFACE_WITH_KNOTS ( ( 4, 4 ),
 ( 2, 2 ),
 ( 0.000000000000000000, 1.000000000000000000 ),
 ( 0.000000000000000000, 1.000000000000000000 ),
 .UNSPECIFIED. ) 
 GEOMETRIC_REPRESENTATION_ITEM ( )  RATIONAL_B_SPLINE_SURFACE ( (
 ( 1.000000000000000000, 1.000000000000000000),
 ( 0.9953040768229013402, 0.8617119497784988535),
 ( 0.9953040768229013402, 0.8617119497784988535),
 ( 1.000000000000000000, 1.000000000000000000) ) ) 
 REPRESENTATION_ITEM ( '' )  SURFACE ( )  );
#15742 = CARTESIAN_POINT ( 'NONE',  ( 0.6029442701453592290, 11.01234799411597010, 47.85680115526702139 ) ) ;
#15743 = CIRCLE ( 'NONE', #48773, 2.500000000000002220 ) ;
#15744 = AXIS2_PLACEMENT_3D ( 'NONE', #34633, #9899, #48114 ) ;
#15745 = ORIENTED_EDGE ( 'NONE', *, *, #37223, .F. ) ;
#15746 = ORIENTED_EDGE ( 'NONE', *, *, #56995, .T. ) ;
#15747 = CARTESIAN_POINT ( 'NONE',  ( 1.154321713695931839, 25.46626713715458834, 34.54400171733310998 ) ) ;
#15748 = VERTEX_POINT ( 'NONE', #8455 ) ;
#15749 = CARTESIAN_POINT ( 'NONE',  ( 0.8557997880470599172, -37.44587306708076824, -29.88293891557508530 ) ) ;
#15750 = CARTESIAN_POINT ( 'NONE',  ( 0.9789889208857698311, -17.72799716457255670, -37.97437312945766053 ) ) ;
#15751 = ORIENTED_EDGE ( 'NONE', *, *, #55689, .T. ) ;
#15752 = DIRECTION ( 'NONE',  ( -0.1024043820194934368, -0.1167898032637205152, -0.9878630899050874214 ) ) ;
#15753 = EDGE_CURVE ( 'NONE', #10639, #25145, #11184, .T. ) ;
#15754 = CARTESIAN_POINT ( 'NONE',  ( 3.238018933889920792, -0.7223087070292297796, -13.37481822304148871 ) ) ;
#15755 = ORIENTED_EDGE ( 'NONE', *, *, #26378, .T. ) ;
#15756 =( BOUNDED_SURFACE ( )  B_SPLINE_SURFACE ( 3, 1, ( 
 ( #5270, #53505 ),
 ( #24401, #10940 ),
 ( #6186, #39451 ),
 ( #48826, #19713 ) ),
 .UNSPECIFIED., .F., .F., .F. ) 
 B_SPLINE_SURFACE_WITH_KNOTS ( ( 4, 4 ),
 ( 2, 2 ),
 ( 0.000000000000000000, 1.000000000000000000 ),
 ( 0.000000000000000000, 1.000000000000000000 ),
 .UNSPECIFIED. ) 
 GEOMETRIC_REPRESENTATION_ITEM ( )  RATIONAL_B_SPLINE_SURFACE ( (
 ( 1.000000000000000000, 1.000000000000000000),
 ( 0.9952954269826590483, 0.8620686068821339365),
 ( 0.9952954269826590483, 0.8620686068821339365),
 ( 1.000000000000000000, 1.000000000000000000) ) ) 
 REPRESENTATION_ITEM ( '' )  SURFACE ( )  );
#15757 = CARTESIAN_POINT ( 'NONE',  ( 48.20159250628719150, 12.42985392437715220, 1.330251472907249433 ) ) ;
#15758 = CARTESIAN_POINT ( 'NONE',  ( 5.838029081930957709, 13.97520979541510044, -45.11938130479024522 ) ) ;
#15759 = CARTESIAN_POINT ( 'NONE',  ( 0.9784957157296372277, 36.17631838904543429, 21.15672575817877288 ) ) ;
#15760 =( BOUNDED_SURFACE ( )  B_SPLINE_SURFACE ( 3, 1, ( 
 ( #43285, #29463 ),
 ( #52956, #38583 ),
 ( #14769, #19780 ),
 ( #19167, #638 ) ),
 .UNSPECIFIED., .F., .F., .F. ) 
 B_SPLINE_SURFACE_WITH_KNOTS ( ( 4, 4 ),
 ( 2, 2 ),
 ( 0.000000000000000000, 1.000000000000000000 ),
 ( 0.000000000000000000, 1.000000000000000000 ),
 .UNSPECIFIED. ) 
 GEOMETRIC_REPRESENTATION_ITEM ( )  RATIONAL_B_SPLINE_SURFACE ( (
 ( 1.000000000000000000, 1.000000000000000000),
 ( 0.9953390228620291325, 0.8624445117761032620),
 ( 0.9953390228620291325, 0.8624445117761032620),
 ( 1.000000000000000000, 1.000000000000000000) ) ) 
 REPRESENTATION_ITEM ( '' )  SURFACE ( )  );
#15761 = B_SPLINE_CURVE_WITH_KNOTS ( 'NONE', 3,
 ( #18769, #38195, #32245, #28449 ),
 .UNSPECIFIED., .F., .F.,
 ( 4, 4 ),
 ( 0.000000000000000000, 0.004447772540403797242 ),
 .UNSPECIFIED. ) ;
#15762 = ORIENTED_EDGE ( 'NONE', *, *, #51680, .T. ) ;
#15763 = CARTESIAN_POINT ( 'NONE',  ( 1.227938101723756947, 41.66816631169191965, 10.28900963485394904 ) ) ;
#15764 = CARTESIAN_POINT ( 'NONE',  ( 0.1104177457020373426, 41.65628910360723580, 11.15670205480019028 ) ) ;
#15765 = DIRECTION ( 'NONE',  ( 0.000000000000000000, 0.000000000000000000, -1.000000000000000000 ) ) ;
#15766 = CARTESIAN_POINT ( 'NONE',  ( 0.8744876279028306332, 28.81338721758086052, 39.75095932715638014 ) ) ;
#15767 = ORIENTED_EDGE ( 'NONE', *, *, #44729, .T. ) ;
#15768 = CARTESIAN_POINT ( 'NONE',  ( 3.221118495291108719, -42.98720608046416913, -9.319953490090810533 ) ) ;
#15769 = DIRECTION ( 'NONE',  ( 1.000000000000000000, 1.836909530733573776E-16, 0.000000000000000000 ) ) ;
#15770 = CARTESIAN_POINT ( 'NONE',  ( 2.618530812446111078, -46.97577780651596413, 1.732942200721546699 ) ) ;
#15771 = DIRECTION ( 'NONE',  ( -0.9848077530122079093, -0.1736481776669315802, 1.387778780781445367E-17 ) ) ;
#15772 = VERTEX_POINT ( 'NONE', #56383 ) ;
#15773 = ORIENTED_EDGE ( 'NONE', *, *, #17196, .F. ) ;
#15774 = CARTESIAN_POINT ( 'NONE',  ( 4.553261556744873317, 6.787618719204111528, -43.39893775135914922 ) ) ;
#15775 = CARTESIAN_POINT ( 'NONE',  ( 0.8744876279028306332, -2.462621419132613454, -49.03351451941336592 ) ) ;
#15776 = CARTESIAN_POINT ( 'NONE',  ( 0.6001305935487315502, -18.89378601236034427, -44.24520387813821287 ) ) ;
#15777 = CARTESIAN_POINT ( 'NONE',  ( -6.077587904424778920, -19.21610359950805247, 1.239912838430311970 ) ) ;
#15778 = DIRECTION ( 'NONE',  ( 0.1011922191286468153, 0.3556331495180372615, 0.9291314211411113577 ) ) ;
#15779 = CARTESIAN_POINT ( 'NONE',  ( 0.8760168074887090262, 5.394043284319505638, -47.80016357497244428 ) ) ;
#15780 = EDGE_CURVE ( 'NONE', #40551, #54789, #49675, .T. ) ;
#15781 = CARTESIAN_POINT ( 'NONE',  ( 0.9790850452238875068, 9.666011576262016902, -40.77873895145319239 ) ) ;
#15782 = CARTESIAN_POINT ( 'NONE',  ( 0.6000166863083090663, 16.46965316277442781, 46.26633772416364110 ) ) ;
#15783 = CARTESIAN_POINT ( 'NONE',  ( 0.8557997880470599172, 7.156447707086380561, -47.37054680076698077 ) ) ;
#15784 = EDGE_CURVE ( 'NONE', #59245, #57068, #42278, .T. ) ;
#15785 = CARTESIAN_POINT ( 'NONE',  ( 1.231276596079881047, -11.60895935156387537, -40.28037777618035875 ) ) ;
#15786 = CARTESIAN_POINT ( 'NONE',  ( 0.5998501479064708430, -6.798102206414489146, 47.62484632993676570 ) ) ;
#15787 = VECTOR ( 'NONE', #2888, 1000.000000000000114 ) ;
#15788 = CIRCLE ( 'NONE', #23648, 48.91267123290010943 ) ;
#15789 = EDGE_CURVE ( 'NONE', #35743, #24966, #23488, .T. ) ;
#15790 = CARTESIAN_POINT ( 'NONE',  ( 1.231276596079881047, 15.85305549123227564, -38.80666698661426040 ) ) ;
#15791 = DIRECTION ( 'NONE',  ( -1.000000000000000000, -3.673819061467147552E-16, 1.925929944387235306E-32 ) ) ;
#15792 = CARTESIAN_POINT ( 'NONE',  ( -6.015611763856276717, -14.95313250337422062, -11.46610900684738432 ) ) ;
#15793 = DIRECTION ( 'NONE',  ( 1.000000000000000000, 0.000000000000000000, 0.000000000000000000 ) ) ;
#15794 = CARTESIAN_POINT ( 'NONE',  ( 4.553261556744875094, 0.000000000000000000, 0.000000000000000000 ) ) ;
#15795 = FACE_OUTER_BOUND ( 'NONE', #37142, .T. ) ;
#15796 = CARTESIAN_POINT ( 'NONE',  ( 0.9722240750034573109, 6.177112354445118747, 42.46141201102046381 ) ) ;
#15797 = FACE_OUTER_BOUND ( 'NONE', #11644, .T. ) ;
#15798 = CARTESIAN_POINT ( 'NONE',  ( 0.6029443449137436017, 49.00930124176078095, -3.102890551997893542 ) ) ;
#15800 = ORIENTED_EDGE ( 'NONE', *, *, #22432, .F. ) ;
#15799 = CARTESIAN_POINT ( 'NONE',  ( 0.6067099128993247437, 41.12102523654892394, -24.55985149487281305 ) ) ;
#15801 = ORIENTED_EDGE ( 'NONE', *, *, #56300, .F. ) ;
#15802 = EDGE_CURVE ( 'NONE', #54760, #50250, #36189, .T. ) ;
#15803 = TOROIDAL_SURFACE ( 'NONE', #22814, 5.100000000000000533, 0.1000000000000005884 ) ;
#15804 = CARTESIAN_POINT ( 'NONE',  ( 3.376099380956842921, 13.21675742563012967, -2.241808819707415079 ) ) ;
#15805 = CARTESIAN_POINT ( 'NONE',  ( 5.895881250540457863, -13.98558879082096240, 14.45444526027768184 ) ) ;
#15806 = CARTESIAN_POINT ( 'NONE',  ( 1.000433927950260093, -34.17502901178241359, 24.25873182375112691 ) ) ;
#15807 = ORIENTED_EDGE ( 'NONE', *, *, #36514, .T. ) ;
#15808 = EDGE_CURVE ( 'NONE', #31069, #13981, #54874, .T. ) ;
#15809 = ORIENTED_EDGE ( 'NONE', *, *, #3643, .T. ) ;
#15810 = CARTESIAN_POINT ( 'NONE',  ( 1.399999999999999467, 0.000000000000000000, -5.100000000000000533 ) ) ;
#15811 = CARTESIAN_POINT ( 'NONE',  ( -6.015611763856276717, 11.47596948473832690, -14.94556629257413327 ) ) ;
#15812 = DIRECTION ( 'NONE',  ( -1.000000000000000000, -0.000000000000000000, -0.000000000000000000 ) ) ;
#15813 = ORIENTED_EDGE ( 'NONE', *, *, #45775, .T. ) ;
#15814 = ORIENTED_EDGE ( 'NONE', *, *, #23451, .F. ) ;
#15815 = DIRECTION ( 'NONE',  ( 0.000000000000000000, 0.000000000000000000, 1.000000000000000000 ) ) ;
#15816 = VECTOR ( 'NONE', #44999, 1000.000000000000114 ) ;
#15817 = CARTESIAN_POINT ( 'NONE',  ( 0.6000166863083090663, 44.01764848084249593, 21.77774331572116040 ) ) ;
#15818 = CARTESIAN_POINT ( 'NONE',  ( 0.8760168074887090262, 13.30888447662015928, 46.22580377597790147 ) ) ;
#15819 = DIRECTION ( 'NONE',  ( -1.000000000000000000, -0.000000000000000000, -0.000000000000000000 ) ) ;
#15820 = CARTESIAN_POINT ( 'NONE',  ( 0.6254087463353933396, 19.04342133627982747, 44.17672642933511895 ) ) ;
#15821 = CARTESIAN_POINT ( 'NONE',  ( -6.078726893082806448, -16.13637198556907748, 10.50768958487361537 ) ) ;
#15822 = ADVANCED_FACE ( 'NONE', ( #56077 ), #44210, .F. ) ;
#15823 = CARTESIAN_POINT ( 'NONE',  ( 0.1158816050234199313, 15.23361400778437336, -41.41109809660929386 ) ) ;
#15824 = ORIENTED_EDGE ( 'NONE', *, *, #52464, .F. ) ;
#15825 = VERTEX_POINT ( 'NONE', #61381 ) ;
#15826 = CARTESIAN_POINT ( 'NONE',  ( 0.2285344041767117251, 34.08191643308648366, 28.01649768517765082 ) ) ;
#15827 = CARTESIAN_POINT ( 'NONE',  ( -6.015611763856276717, -9.416239407363189429, -16.32183393015606754 ) ) ;
#15828 = CIRCLE ( 'NONE', #16871, 47.91270532121795611 ) ;
#15829 = B_SPLINE_CURVE_WITH_KNOTS ( 'NONE', 3,
 ( #5778, #14925, #43123, #19305, #23993, #38124 ),
 .UNSPECIFIED., .F., .F.,
 ( 4, 2, 4 ),
 ( 9.140795285775094282E-18, 0.0002291978881530172714, 0.0004583957763060254355 ),
 .UNSPECIFIED. ) ;
#15830 = ORIENTED_EDGE ( 'NONE', *, *, #44014, .T. ) ;
#15831 = DIRECTION ( 'NONE',  ( 0.000000000000000000, 0.000000000000000000, 1.000000000000000000 ) ) ;
#15832 = CARTESIAN_POINT ( 'NONE',  ( 0.5997462898726536595, -8.352924653000716404, 48.39194436975645175 ) ) ;
#15833 = CARTESIAN_POINT ( 'NONE',  ( 2.282816707992307848, 18.10202035515079544, 43.34528608129922134 ) ) ;
#15834 = CARTESIAN_POINT ( 'NONE',  ( 4.975801465491695552, 36.39623109580423943, 31.15993731089136887 ) ) ;
#15835 = ORIENTED_EDGE ( 'NONE', *, *, #20545, .F. ) ;
#15836 = CARTESIAN_POINT ( 'NONE',  ( 0.5835226383429313879, 46.45302275910173506, -6.431108076244583138 ) ) ;
#15837 = CARTESIAN_POINT ( 'NONE',  ( 0.6029442701453591180, -35.21567780871351516, 34.22573975286961456 ) ) ;
#15838 = CARTESIAN_POINT ( 'NONE',  ( 0.8744876279028263033, 28.81338721758142896, -39.75095932715596092 ) ) ;
#15839 =( BOUNDED_SURFACE ( )  B_SPLINE_SURFACE ( 3, 1, ( 
 ( #59989, #50584 ),
 ( #22096, #36519 ),
 ( #55585, #12715 ),
 ( #9849, #61519 ) ),
 .UNSPECIFIED., .F., .F., .F. ) 
 B_SPLINE_SURFACE_WITH_KNOTS ( ( 4, 4 ),
 ( 2, 2 ),
 ( 0.000000000000000000, 1.000000000000000000 ),
 ( 0.000000000000000000, 1.000000000000000000 ),
 .UNSPECIFIED. ) 
 GEOMETRIC_REPRESENTATION_ITEM ( )  RATIONAL_B_SPLINE_SURFACE ( (
 ( 1.000000000000000000, 1.000000000000000000),
 ( 0.9751682680413298332, 0.9999560080971552356),
 ( 0.9751682680413298332, 0.9999560080971552356),
 ( 1.000000000000000000, 1.000000000000000000) ) ) 
 REPRESENTATION_ITEM ( '' )  SURFACE ( )  );
#15840 = CARTESIAN_POINT ( 'NONE',  ( 4.956445790443996025, 13.43466403631381567, 45.13366650706556982 ) ) ;
#15841 = ORIENTED_EDGE ( 'NONE', *, *, #34296, .F. ) ;
#15842 = CARTESIAN_POINT ( 'NONE',  ( 4.553261556744873317, -25.31600221269608397, -35.89762663172042068 ) ) ;
#15843 = PLANE ( 'NONE',  #57644 ) ;
#15844 = VERTEX_POINT ( 'NONE', #13816 ) ;
#15845 = CARTESIAN_POINT ( 'NONE',  ( 2.281351352603296245, 30.23585463601430590, -37.24546109640787250 ) ) ;
#15846 = CARTESIAN_POINT ( 'NONE',  ( 5.981074661064941900, 18.96560215432005947, 7.846517100474887485 ) ) ;
#15847 = VECTOR ( 'NONE', #3815, 1000.000000000000114 ) ;
#15848 = ORIENTED_EDGE ( 'NONE', *, *, #28516, .T. ) ;
#15849 = FACE_OUTER_BOUND ( 'NONE', #47574, .T. ) ;
#15850 = CARTESIAN_POINT ( 'NONE',  ( -6.016104459813371719, 16.31603998697582725, -9.426230926598471171 ) ) ;
#15851 = CARTESIAN_POINT ( 'NONE',  ( 4.967162193818130511, -43.02067033766017801, -2.375726030843023029 ) ) ;
#15852 = CARTESIAN_POINT ( 'NONE',  ( 5.880360259849752858, -47.87242051977163726, 3.090325311464702462 ) ) ;
#15853 = CARTESIAN_POINT ( 'NONE',  ( 0.1129192098497455998, 33.91039995638899995, -28.23183597612607798 ) ) ;
#15854 = CARTESIAN_POINT ( 'NONE',  ( 0.5797568665920714848, 45.39179673982854268, 11.78176970289104197 ) ) ;
#15855 = CARTESIAN_POINT ( 'NONE',  ( 0.8751705887134553219, 44.76769609654211735, 17.57879340691559378 ) ) ;
#15856 = FACE_OUTER_BOUND ( 'NONE', #24117, .T. ) ;
#15858 = EDGE_CURVE ( 'NONE', #13508, #18777, #37308, .T. ) ;
#15857 = FACE_OUTER_BOUND ( 'NONE', #26156, .T. ) ;
#15859 = STYLED_ITEM ( 'NONE', ( #58210 ), #10859 ) ;
#15860 = DIRECTION ( 'NONE',  ( 0.1011922191286468153, -0.5046905544709855418, 0.8573491581704556497 ) ) ;
#15861 = B_SPLINE_CURVE_WITH_KNOTS ( 'NONE', 3,
 ( #7257, #12311, #3187, #55810 ),
 .UNSPECIFIED., .F., .F.,
 ( 4, 4 ),
 ( 0.000000000000000000, 0.004050076154993000749 ),
 .UNSPECIFIED. ) ;
#15862 = CARTESIAN_POINT ( 'NONE',  ( 0.5806925824938502512, 27.37593026015236219, -38.07598724570169679 ) ) ;
#15863 = ORIENTED_EDGE ( 'NONE', *, *, #60454, .T. ) ;
#15864 = ADVANCED_FACE ( 'NONE', ( #19133 ), #50767, .F. ) ;
#15865 = CARTESIAN_POINT ( 'NONE',  ( -17.69803791752843836, -12.32468874903235267, 2.086332406704181519 ) ) ;
#15866 = CARTESIAN_POINT ( 'NONE',  ( 0.6039202388192953519, 37.27969488251792995, -31.96541978944368267 ) ) ;
#15867 = CARTESIAN_POINT ( 'NONE',  ( 0.6029442701453591180, 22.79128462898585994, 43.49830537065587777 ) ) ;
#15868 = DIRECTION ( 'NONE',  ( 0.000000000000000000, 0.000000000000000000, -1.000000000000000000 ) ) ;
#15869 = CARTESIAN_POINT ( 'NONE',  ( 1.500000000000001332, 6.678152076600409922E-16, -5.453125000000000000 ) ) ;
#15870 = CARTESIAN_POINT ( 'NONE',  ( 0.5998501479064699549, 37.84527566984857572, -29.69975237324574024 ) ) ;
#15871 = EDGE_CURVE ( 'NONE', #13524, #28607, #47478, .T. ) ;
#15872 = DIRECTION ( 'NONE',  ( 6.982962677686266711E-15, 0.000000000000000000, -1.000000000000000000 ) ) ;
#15873 = DIRECTION ( 'NONE',  ( -0.07439287786467653485, 0.6957517427943171739, -0.7144194931002945115 ) ) ;
#15874 = CARTESIAN_POINT ( 'NONE',  ( 0.6023143664670691511, -0.2618215695310947000, 48.10676742339276046 ) ) ;
#15875 = VECTOR ( 'NONE', #46867, 1000.000000000000114 ) ;
#15876 = CARTESIAN_POINT ( 'NONE',  ( 0.6254087463353912302, -29.82831063981306485, -37.74264085326048956 ) ) ;
#15878 = ORIENTED_EDGE ( 'NONE', *, *, #32413, .F. ) ;
#15877 = CARTESIAN_POINT ( 'NONE',  ( 0.7056313189692637877, -29.63221772841613344, 36.35492148875172802 ) ) ;
#15879 = ORIENTED_EDGE ( 'NONE', *, *, #5639, .T. ) ;
#15880 = CARTESIAN_POINT ( 'NONE',  ( 0.5807400328401637335, -37.66660715020886840, 29.58941477093002348 ) ) ;
#15881 = AXIS2_PLACEMENT_3D ( 'NONE', #9502, #56492, #3555 ) ;
#15882 = CARTESIAN_POINT ( 'NONE',  ( 5.860006189529246790, 31.81514841426808005, -36.25227510158430277 ) ) ;
#15883 = CARTESIAN_POINT ( 'NONE',  ( 0.9730545539215883499, 42.90536227157002003, 0.5054011016614263774 ) ) ;
#15884 = EDGE_CURVE ( 'NONE', #19530, #25568, #32498, .T. ) ;
#15885 = CARTESIAN_POINT ( 'NONE',  ( -1.500000000000001332, 9.123618653647808769E-16, 7.400000000000021672 ) ) ;
#15886 = CARTESIAN_POINT ( 'NONE',  ( 0.5997462898726536595, -1.051648045106814422, -49.09628974305016413 ) ) ;
#15887 = CARTESIAN_POINT ( 'NONE',  ( 0.9730545539215883499, 37.40983423658502716, -21.01499094264509893 ) ) ;
#15888 = B_SPLINE_CURVE_WITH_KNOTS ( 'NONE', 3,
 ( #52950, #42354, #37337, #28843, #61408, #632 ),
 .UNSPECIFIED., .F., .F.,
 ( 4, 2, 4 ),
 ( 0.000000000000000000, 0.0002447195606305751798, 0.0004894391212611503596 ),
 .UNSPECIFIED. ) ;
#15889 = EDGE_LOOP ( 'NONE', ( #34404, #8201, #20581, #54995, #25224 ) ) ;
#15890 = VERTEX_POINT ( 'NONE', #24735 ) ;
#15891 = CARTESIAN_POINT ( 'NONE',  ( -1.399999999999998579, 0.000000000000000000, -7.500000000000022204 ) ) ;
#15892 = AXIS2_PLACEMENT_3D ( 'NONE', #38923, #50449, #2823 ) ;
#15893 = CARTESIAN_POINT ( 'NONE',  ( 0.1103310638050661596, -11.08182869403265514, -41.67627416617910541 ) ) ;
#15894 = LINE ( 'NONE', #25582, #26913 ) ;
#15895 = ORIENTED_EDGE ( 'NONE', *, *, #34454, .F. ) ;
#15896 = CARTESIAN_POINT ( 'NONE',  ( 0.1103936448916680718, -0.01291577404971127989, 43.12443171339901937 ) ) ;
#15897 = CARTESIAN_POINT ( 'NONE',  ( 4.967162193818130511, -32.68434214048189546, 28.07411493385282242 ) ) ;
#15898 = EDGE_LOOP ( 'NONE', ( #7086, #42866, #31719, #20632 ) ) ;
#15899 = DIRECTION ( 'NONE',  ( 0.07836865515943412797, 0.6131273243286281538, -0.7860872967108163412 ) ) ;
#15900 = VERTEX_POINT ( 'NONE', #5900 ) ;
#15901 = CARTESIAN_POINT ( 'NONE',  ( -48.95476116535499500, 0.000000000000000000, 0.000000000000000000 ) ) ;
#15902 = CARTESIAN_POINT ( 'NONE',  ( 2.624215991343620935, -45.98641578154040843, 13.78323291683767415 ) ) ;
#15903 = ORIENTED_EDGE ( 'NONE', *, *, #22502, .F. ) ;
#15904 = FACE_BOUND ( 'NONE', #24389, .T. ) ;
#15905 = CARTESIAN_POINT ( 'NONE',  ( 0.5824936645240085253, -20.06997566773453912, 42.38436333999664640 ) ) ;
#15906 = CARTESIAN_POINT ( 'NONE',  ( -3.673643420401911275, -2.497823135841290565, -5.351519936624989704 ) ) ;
#15907 = CARTESIAN_POINT ( 'NONE',  ( 0.5809828226811553087, -37.66417181417572380, 29.58751527316164953 ) ) ;
#15908 = EDGE_CURVE ( 'NONE', #7974, #28331, #34069, .T. ) ;
#15909 = ORIENTED_EDGE ( 'NONE', *, *, #2337, .F. ) ;
#15910 = EDGE_CURVE ( 'NONE', #55102, #9584, #8621, .T. ) ;
#15911 = CARTESIAN_POINT ( 'NONE',  ( -6.017396004339687465, -17.40926186480783855, 7.209881890566491869 ) ) ;
#15912 = CARTESIAN_POINT ( 'NONE',  ( 2.500000000000000000, 0.000000000000000000, 0.000000000000000000 ) ) ;
#15913 = ORIENTED_EDGE ( 'NONE', *, *, #13296, .T. ) ;
#15914 = CARTESIAN_POINT ( 'NONE',  ( 4.956445790443996913, 8.365049606151725214, 46.34181691762049127 ) ) ;
#15915 = EDGE_LOOP ( 'NONE', ( #19346, #56273, #35497, #14869 ) ) ;
#15916 = CARTESIAN_POINT ( 'NONE',  ( 0.9780303403264789530, 4.516970423409048863, 41.66457237977044770 ) ) ;
#15917 = EDGE_CURVE ( 'NONE', #45566, #51246, #18297, .T. ) ;
#15918 = ORIENTED_EDGE ( 'NONE', *, *, #49210, .F. ) ;
#15919 = CARTESIAN_POINT ( 'NONE',  ( 3.407937589446174087, 12.47329436636629119, 5.663729899985116667 ) ) ;
#15920 = CARTESIAN_POINT ( 'NONE',  ( 0.9791128995231609400, 36.05569391225776599, -21.36175017997689451 ) ) ;
#15921 = CIRCLE ( 'NONE', #61894, 42.08604991992415023 ) ;
#15922 = CARTESIAN_POINT ( 'NONE',  ( 2.618530812446111078, -45.76452502972750125, -10.73941516106192573 ) ) ;
#15923 = VERTEX_POINT ( 'NONE', #1519 ) ;
#15924 = CARTESIAN_POINT ( 'NONE',  ( 0.8744876279028263033, -49.08725279547490317, -0.8897546699139439186 ) ) ;
#15925 = DIRECTION ( 'NONE',  ( 1.000000000000000000, 0.000000000000000000, 0.000000000000000000 ) ) ;
#15926 = DIRECTION ( 'NONE',  ( -1.000000000000000000, -0.000000000000000000, -0.000000000000000000 ) ) ;
#15927 = VERTEX_POINT ( 'NONE', #10644 ) ;
#15928 = B_SPLINE_CURVE_WITH_KNOTS ( 'NONE', 3,
 ( #47005, #4038, #33209, #9374, #37605, #52280 ),
 .UNSPECIFIED., .F., .F.,
 ( 4, 2, 4 ),
 ( 9.965227682168975268E-18, 0.0002445244328975359929, 0.0004890488657950620112 ),
 .UNSPECIFIED. ) ;
#15929 = VERTEX_POINT ( 'NONE', #20053 ) ;
#15930 = CARTESIAN_POINT ( 'NONE',  ( 0.9791128995231611620, -31.08508259969504195, -28.10791835081888834 ) ) ;
#15931 = CARTESIAN_POINT ( 'NONE',  ( 4.060580049360325461, 31.21837995092301554, 30.93348424602403668 ) ) ;
#15932 = CARTESIAN_POINT ( 'NONE',  ( 4.967162193818130511, 28.74031574030056646, -32.10009971360042158 ) ) ;
#15933 = CARTESIAN_POINT ( 'NONE',  ( 0.9730545539215883499, -0.5054011016609686324, -42.90536227157002713 ) ) ;
#15934 = CARTESIAN_POINT ( 'NONE',  ( 0.9790320750461896093, -26.99170229640500906, -32.05908825410412533 ) ) ;
#15935 = AXIS2_PLACEMENT_3D ( 'NONE', #51886, #4558, #61881 ) ;
#15936 = CARTESIAN_POINT ( 'NONE',  ( 0.8753041380234530822, 40.66072100792177935, -27.52896828776785654 ) ) ;
#15937 = ORIENTED_EDGE ( 'NONE', *, *, #31804, .T. ) ;
#15938 = EDGE_CURVE ( 'NONE', #54002, #44253, #18203, .T. ) ;
#15939 = DIRECTION ( 'NONE',  ( -1.000000000000000000, 0.000000000000000000, 0.000000000000000000 ) ) ;
#15940 = AXIS2_PLACEMENT_3D ( 'NONE', #52829, #61593, #46929 ) ;
#15941 = ORIENTED_EDGE ( 'NONE', *, *, #47662, .T. ) ;
#15942 = EDGE_CURVE ( 'NONE', #39564, #10841, #24276, .T. ) ;
#15943 = CARTESIAN_POINT ( 'NONE',  ( 0.1119898979215349227, -38.71871422322526257, -21.16181648989621422 ) ) ;
#15944 = CARTESIAN_POINT ( 'NONE',  ( -4.000000000000000000, -0.7779732554280797130, -5.566455648918322119 ) ) ;
#15945 = CARTESIAN_POINT ( 'NONE',  ( 0.5980271706414734822, 41.53842981737961537, 26.20320764998614038 ) ) ;
#15946 = DIRECTION ( 'NONE',  ( -0.07439287786467650709, 0.6174937095821703137, 0.7830499462674533895 ) ) ;
#15947 = CARTESIAN_POINT ( 'NONE',  ( 0.6041374136657475802, -41.74951251761589788, 23.90252055111250584 ) ) ;
#15948 = ADVANCED_FACE ( 'NONE', ( #57916 ), #14393, .F. ) ;
#15949 = FACE_OUTER_BOUND ( 'NONE', #17411, .T. ) ;
#15950 = CARTESIAN_POINT ( 'NONE',  ( 1.231276596079887931, -35.03243822710496858, -23.02183839058345072 ) ) ;
#15951 = CARTESIAN_POINT ( 'NONE',  ( 3.783198216974390959, -9.462293521184577116, -41.98529422752524454 ) ) ;
#15952 = CARTESIAN_POINT ( 'NONE',  ( 1.231276596079887264, -30.51591784428387655, 28.74118176309011830 ) ) ;
#15953 = CARTESIAN_POINT ( 'NONE',  ( -5.999999999999999112, -15.14599999999999014, 1.854850041988580438E-15 ) ) ;
#15954 = B_SPLINE_CURVE_WITH_KNOTS ( 'NONE', 3,
 ( #54233, #58311, #15440, #1614 ),
 .UNSPECIFIED., .F., .F.,
 ( 4, 4 ),
 ( 2.380737582495642427E-07, 0.002336974151641604130 ),
 .UNSPECIFIED. ) ;
#15955 = CARTESIAN_POINT ( 'NONE',  ( 0.1313383488274134925, 0.6377633466094576598, 43.11882601516400371 ) ) ;
#15956 = LINE ( 'NONE', #49763, #21749 ) ;
#15957 = EDGE_CURVE ( 'NONE', #5641, #61479, #10192, .T. ) ;
#15958 = CARTESIAN_POINT ( 'NONE',  ( 3.559346040607745287, -19.65740999566269664, -39.33213080681503726 ) ) ;
#15959 = LINE ( 'NONE', #44484, #60453 ) ;
#15960 = CARTESIAN_POINT ( 'NONE',  ( 3.238741278300274029, -18.12697907494920102, 38.98370040185395879 ) ) ;
#15961 = AXIS2_PLACEMENT_3D ( 'NONE', #40181, #34844, #16040 ) ;
#15962 =( BOUNDED_SURFACE ( )  B_SPLINE_SURFACE ( 3, 1, ( 
 ( #12969, #44943 ),
 ( #31433, #12655 ),
 ( #49924, #27045 ),
 ( #46171, #8229 ) ),
 .UNSPECIFIED., .F., .F., .F. ) 
 B_SPLINE_SURFACE_WITH_KNOTS ( ( 4, 4 ),
 ( 2, 2 ),
 ( 0.000000000000000000, 1.000000000000000000 ),
 ( 0.000000000000000000, 1.000000000000000000 ),
 .UNSPECIFIED. ) 
 GEOMETRIC_REPRESENTATION_ITEM ( )  RATIONAL_B_SPLINE_SURFACE ( (
 ( 1.000000000000000000, 1.000000000000000000),
 ( 0.9952954269826590483, 0.8620686068821339365),
 ( 0.9952954269826590483, 0.8620686068821339365),
 ( 1.000000000000000000, 1.000000000000000000) ) ) 
 REPRESENTATION_ITEM ( '' )  SURFACE ( )  );
#15963 = ORIENTED_EDGE ( 'NONE', *, *, #24386, .T. ) ;
#15964 = CARTESIAN_POINT ( 'NONE',  ( 1.000110580585052089, 24.32719571472549447, 34.12630995916995147 ) ) ;
#15965 = VECTOR ( 'NONE', #6683, 1000.000000000000000 ) ;
#15966 = CARTESIAN_POINT ( 'NONE',  ( 0.5830082357119570347, -19.49201582728397852, -42.65317519162255167 ) ) ;
#15967 = CARTESIAN_POINT ( 'NONE',  ( 5.960721111146673579, 20.35079619394246109, -2.672857320903093914 ) ) ;
#15968 = CARTESIAN_POINT ( 'NONE',  ( 0.2230388203127608715, -29.94794547692467646, 31.02270543585776608 ) ) ;
#15969 = CARTESIAN_POINT ( 'NONE',  ( 0.9756008150404587020, 39.58764833544701389, -16.55159915785236890 ) ) ;
#15970 = VERTEX_POINT ( 'NONE', #19428 ) ;
#15971 = CARTESIAN_POINT ( 'NONE',  ( 3.407937589446174087, -9.356405769958984209, -10.00592723328970912 ) ) ;
#15972 = FACE_OUTER_BOUND ( 'NONE', #9983, .T. ) ;
#15973 = CARTESIAN_POINT ( 'NONE',  ( 0.6021447746440204973, -13.72175854280559193, 47.15139957182002206 ) ) ;
#15974 = ORIENTED_EDGE ( 'NONE', *, *, #59318, .F. ) ;
#15975 = CARTESIAN_POINT ( 'NONE',  ( 3.727782113643637096, -43.91135458311394046, 2.137922959793808975 ) ) ;
#15976 = CARTESIAN_POINT ( 'NONE',  ( 1.231276596079881047, 25.54232633153377208, -33.23952972879584422 ) ) ;
#15977 = ORIENTED_EDGE ( 'NONE', *, *, #1966, .F. ) ;
#15978 = EDGE_CURVE ( 'NONE', #16995, #32229, #46706, .T. ) ;
#15979 = CARTESIAN_POINT ( 'NONE',  ( 5.981074661064941900, -0.008585178657759484633, 20.52466374824937034 ) ) ;
#15980 = VECTOR ( 'NONE', #46485, 1000.000000000000000 ) ;
#15981 = ORIENTED_EDGE ( 'NONE', *, *, #27078, .F. ) ;
#15982 = CARTESIAN_POINT ( 'NONE',  ( 5.981074661064941900, -12.50143471347269930, -16.27808421740022027 ) ) ;
#15983 = ORIENTED_EDGE ( 'NONE', *, *, #57065, .T. ) ;
#15984 = CARTESIAN_POINT ( 'NONE',  ( 0.5998501479064708430, -0.5236536531318284338, 48.10473956285918717 ) ) ;
#15985 = CARTESIAN_POINT ( 'NONE',  ( 0.1073791018717483448, 37.10214135362888754, -21.98088480513627729 ) ) ;
#15986 = EDGE_CURVE ( 'NONE', #29832, #23990, #16575, .T. ) ;
#15987 = ORIENTED_EDGE ( 'NONE', *, *, #8369, .F. ) ;
#15988 = ORIENTED_EDGE ( 'NONE', *, *, #47277, .T. ) ;
#15989 = EDGE_CURVE ( 'NONE', #21198, #52461, #21283, .T. ) ;
#15990 = CARTESIAN_POINT ( 'NONE',  ( 0.3676999524040366896, 16.00695768809390884, 41.10629986868691077 ) ) ;
#15991 = CARTESIAN_POINT ( 'NONE',  ( 0.2885700199627521112, 33.71073713194521559, -26.88157179738468017 ) ) ;
#15992 = ORIENTED_EDGE ( 'NONE', *, *, #46218, .T. ) ;
#15993 = ADVANCED_FACE ( 'NONE', ( #50090 ), #12749, .F. ) ;
#15994 = ORIENTED_EDGE ( 'NONE', *, *, #20163, .F. ) ;
#15995 = DIRECTION ( 'NONE',  ( -1.000000000000000000, -1.836909530733573529E-16, 1.361838123766461297E-32 ) ) ;
#15996 = CARTESIAN_POINT ( 'NONE',  ( 1.227938101723748288, -22.18841447410744649, 36.73927144310504644 ) ) ;
#15997 = CARTESIAN_POINT ( 'NONE',  ( 0.6009452777970412107, 24.43074291040848323, 41.44251326863938090 ) ) ;
#15998 = CARTESIAN_POINT ( 'NONE',  ( -6.078075953587585900, 17.85074021576670233, -7.221235905047362458 ) ) ;
#15999 = VERTEX_POINT ( 'NONE', #16899 ) ;
#16000 = CARTESIAN_POINT ( 'NONE',  ( 4.975610109902397937, 0.000000000000000000, 0.000000000000000000 ) ) ;
#16001 = LINE ( 'NONE', #35114, #39925 ) ;
#16002 = B_SPLINE_CURVE_WITH_KNOTS ( 'NONE', 3,
 ( #37319, #32613, #51699, #47029 ),
 .UNSPECIFIED., .F., .F.,
 ( 4, 4 ),
 ( 0.000000000000000000, 0.004041751736740999482 ),
 .UNSPECIFIED. ) ;
#16003 = ORIENTED_EDGE ( 'NONE', *, *, #35961, .T. ) ;
#16004 = CARTESIAN_POINT ( 'NONE',  ( 0.5837800005270565862, -46.79128237205272001, -3.132275948988451741 ) ) ;
#16005 = VERTEX_POINT ( 'NONE', #54138 ) ;
#16006 = CARTESIAN_POINT ( 'NONE',  ( 1.227938101723748288, -36.73927144310496828, -22.18841447410757795 ) ) ;
#16007 = EDGE_CURVE ( 'NONE', #55289, #57068, #35703, .T. ) ;
#16008 = CARTESIAN_POINT ( 'NONE',  ( 0.9787464366903542157, 40.46600164325194982, -10.90122488066344886 ) ) ;
#16009 = ORIENTED_EDGE ( 'NONE', *, *, #54642, .F. ) ;
#16010 = CARTESIAN_POINT ( 'NONE',  ( 0.9785694773339246311, -12.20375881750114999, -40.09243914304710898 ) ) ;
#16011 = CARTESIAN_POINT ( 'NONE',  ( 0.7044674535453004927, 36.84332507061654383, -32.47109669462652448 ) ) ;
#16012 = CARTESIAN_POINT ( 'NONE',  ( 53.01364348093722612, 12.47163566169240845, -0.8566609489383912868 ) ) ;
#16013 = CARTESIAN_POINT ( 'NONE',  ( 0.9762797500689124330, -22.12212327108586152, -35.59405072711710716 ) ) ;
#16014 = EDGE_CURVE ( 'NONE', #32792, #30530, #43725, .T. ) ;
#16015 = VECTOR ( 'NONE', #11844, 999.9999999999998863 ) ;
#16016 = ORIENTED_EDGE ( 'NONE', *, *, #5764, .F. ) ;
#16017 = CARTESIAN_POINT ( 'NONE',  ( 0.9762797500689124330, -41.84568905980458453, 2.294143041716202092 ) ) ;
#16018 = LINE ( 'NONE', #59518, #8330 ) ;
#16019 = CARTESIAN_POINT ( 'NONE',  ( 0.9968887458511670463, 33.63815526548984991, 26.64009929991515691 ) ) ;
#16020 =( BOUNDED_SURFACE ( )  B_SPLINE_SURFACE ( 3, 1, ( 
 ( #3934, #28687 ),
 ( #52177, #8968 ),
 ( #14303, #28378 ),
 ( #18070, #47813 ) ),
 .UNSPECIFIED., .F., .F., .F. ) 
 B_SPLINE_SURFACE_WITH_KNOTS ( ( 4, 4 ),
 ( 2, 2 ),
 ( 0.000000000000000000, 1.000000000000000000 ),
 ( 0.000000000000000000, 1.000000000000000000 ),
 .UNSPECIFIED. ) 
 GEOMETRIC_REPRESENTATION_ITEM ( )  RATIONAL_B_SPLINE_SURFACE ( (
 ( 1.000000000000000000, 1.000000000000000000),
 ( 0.9953390228620291325, 0.8624445117760984880),
 ( 0.9953390228620291325, 0.8624445117760984880),
 ( 1.000000000000000000, 1.000000000000000000) ) ) 
 REPRESENTATION_ITEM ( '' )  SURFACE ( )  );
#16021 = CARTESIAN_POINT ( 'NONE',  ( 0.9754292589017248272, 20.64935455141624487, 36.46822758930269259 ) ) ;
#16022 = CARTESIAN_POINT ( 'NONE',  ( 1.112077966505211846, -8.069605668463317727, -43.33487959466437900 ) ) ;
#16023 = CARTESIAN_POINT ( 'NONE',  ( 0.5806925824938499181, 43.38503874128572591, -17.80339225430652306 ) ) ;
#16024 = AXIS2_PLACEMENT_3D ( 'NONE', #25240, #59665, #34972 ) ;
#16025 = CARTESIAN_POINT ( 'NONE',  ( -17.42622638222554698, -7.737665651455587046, -2.032071817730983554 ) ) ;
#16026 = CARTESIAN_POINT ( 'NONE',  ( 0.7246131072078513258, -42.06185227555128137, 23.33689307364176457 ) ) ;
#16027 = CARTESIAN_POINT ( 'NONE',  ( 0.1368894036331274600, -27.00909305656406190, 34.89083286746241441 ) ) ;
#16028 = EDGE_CURVE ( 'NONE', #6381, #55761, #34714, .T. ) ;
#16029 = CARTESIAN_POINT ( 'NONE',  ( -6.057079549204054558, -1.840653143754341636, -19.16880870331085163 ) ) ;
#16030 = CARTESIAN_POINT ( 'NONE',  ( 0.8557997880470599172, -43.90420959842167292, -19.17299735372055736 ) ) ;
#16031 =( BOUNDED_SURFACE ( )  B_SPLINE_SURFACE ( 3, 1, ( 
 ( #41017, #36299 ),
 ( #51912, #37855 ),
 ( #56913, #37226 ),
 ( #46937, #46621 ) ),
 .UNSPECIFIED., .F., .F., .F. ) 
 B_SPLINE_SURFACE_WITH_KNOTS ( ( 4, 4 ),
 ( 2, 2 ),
 ( 0.000000000000000000, 1.000000000000000000 ),
 ( 0.000000000000000000, 1.000000000000000000 ),
 .UNSPECIFIED. ) 
 GEOMETRIC_REPRESENTATION_ITEM ( )  RATIONAL_B_SPLINE_SURFACE ( (
 ( 1.000000000000000000, 1.000000000000000000),
 ( 0.7211978278499968642, 0.9934217856018975334),
 ( 0.7211978278499968642, 0.9934217856018975334),
 ( 1.000000000000000000, 1.000000000000000000) ) ) 
 REPRESENTATION_ITEM ( '' )  SURFACE ( )  );
#16032 = EDGE_CURVE ( 'NONE', #4962, #11037, #29186, .T. ) ;
#16033 = LINE ( 'NONE', #1283, #43212 ) ;
#16034 = VERTEX_POINT ( 'NONE', #12204 ) ;
#16035 = DIRECTION ( 'NONE',  ( 0.07906939808003034253, -0.9592846432126428402, -0.2711475679102691161 ) ) ;
#16036 = CARTESIAN_POINT ( 'NONE',  ( 4.956445790444005794, -36.61936279692559992, -29.60676136437043127 ) ) ;
#16037 = CARTESIAN_POINT ( 'NONE',  ( 0.6254311100348688424, 28.73641524052521490, 38.58047947916339382 ) ) ;
#16038 = ORIENTED_EDGE ( 'NONE', *, *, #9547, .F. ) ;
#16039 = CARTESIAN_POINT ( 'NONE',  ( 5.960721111146673579, 5.318514366754659939, 19.82454228767747750 ) ) ;
#16040 = DIRECTION ( 'NONE',  ( 0.000000000000000000, 0.000000000000000000, 1.000000000000000000 ) ) ;
#16041 = CARTESIAN_POINT ( 'NONE',  ( 4.549368137175248350, -42.82045902618774136, 3.018832571115817487 ) ) ;
#16042 = PRODUCT_DEFINITION_CONTEXT ( 'detailed design', #34463, 'design' ) ;
#16043 = VERTEX_POINT ( 'NONE', #31288 ) ;
#16044 = EDGE_LOOP ( 'NONE', ( #52310, #32371, #2246, #11128 ) ) ;
#16045 = B_SPLINE_CURVE_WITH_KNOTS ( 'NONE', 3,
 ( #18339, #61216, #27724, #26477, #12402, #36212 ),
 .UNSPECIFIED., .F., .F.,
 ( 4, 2, 4 ),
 ( 0.000000000000000000, 0.0002447195606305733366, 0.0004894391212611466733 ),
 .UNSPECIFIED. ) ;
#16046 = ORIENTED_EDGE ( 'NONE', *, *, #4289, .F. ) ;
#16047 = FACE_OUTER_BOUND ( 'NONE', #30446, .T. ) ;
#16048 = VERTEX_POINT ( 'NONE', #17199 ) ;
#16049 = ORIENTED_EDGE ( 'NONE', *, *, #34883, .T. ) ;
#16050 = DIRECTION ( 'NONE',  ( 1.000000000000000000, -0.000000000000000000, -0.000000000000000000 ) ) ;
#16051 = EDGE_CURVE ( 'NONE', #33083, #22554, #44386, .T. ) ;
#16052 = VERTEX_POINT ( 'NONE', #50386 ) ;
#16053 = CARTESIAN_POINT ( 'NONE',  ( 0.000000000000000000, 0.6959691356230525150, -1.199999999999999956 ) ) ;
#16054 = CARTESIAN_POINT ( 'NONE',  ( 0.9784957157296365615, -17.85167291169407022, -37.91636627165451046 ) ) ;
#16055 = VERTEX_POINT ( 'NONE', #21897 ) ;
#16056 = ADVANCED_FACE ( 'NONE', ( #41032 ), #18784, .F. ) ;
#16057 = CARTESIAN_POINT ( 'NONE',  ( 4.553261556744875094, -29.36425772793644029, -32.66925058691983708 ) ) ;
#16058 = CLOSED_SHELL ( 'NONE', ( #40991, #40127, #22764, #42448, #27007, #43945, #13288, #43538, #50797, #42562, #34538, #53402, #1505, #45288, #25320, #46623, #19460, #32230, #32534, #30968, #46795, #35161, #38036, #61514, #53877, #11702, #60588, #47824, #34250, #60049, #28858, #7794, #4786, #43308, #7700, #39258, #52688, #11331, #47394, #23497, #53474, #3559, #41955, #38159, #6474, #42712, #21694, #20109, #40348, #3465, #59549, #42186, #17867, #40470, #1892, #42048, #24975, #32394, #2388, #6751, #17981, #18142, #53384, #4145, #37549, #22125, #24983, #11567, #34269, #9036, #28245, #57827, #21023, #10993, #26515, #25406, #17985, #8060, #26166, #33090, #49207, #7586, #50913, #24469, #2868, #28648, #30976, #37807, #2038, #5734, #19470, #61921, #19128, #47544, #35634, #45116, #59081, #61870, #35149, #926, #19079, #45310, #47457, #60969, #41251, #13740, #19983, #44310, #23135, #58898, #25106, #31048, #47965, #18053, #58383, #10208, #16849, #48901, #54521, #46041, #60283, #27928, #55648, #45072, #8207, #24109, #44591, #56915, #22535, #55768, #19113, #60663, #11564, #51173, #10496, #49546, #60519, #36119, #18875, #40909, #9185, #58526, #40622, #21961, #4574, #47697, #27816, #19830, #19853, #44678, #53004, #41843, #47981, #44788, #18048, #4223, #10273, #31601, #25816, #21429, #16260, #47681, #34847, #12979, #5389, #13673, #52611, #48165, #32830, #2991, #9555, #58072, #41178, #51523, #32769, #2437, #51762, #53548, #59836, #18470, #34804, #47045, #46266, #23762, #32942, #18201, #54433, #42748, #7251, #27700, #5283, #23264, #15993, #32848, #16158, #54506, #34825, #36026, #53800, #14056, #49150, #38433, #49348, #58817, #1155, #8568, #45505, #7836, #9112, #5925, #15405, #31555, #20574, #39575, #36638, #6435, #15717, #50549, #28705, #46619, #6900, #42846, #53552, #19374, #30039, #13471, #33262, #21498, #47305, #15822, #61336, #28368, #53861, #15363, #20045, #41195, #59949, #19630, #44364, #18188, #10270, #9624, #47722, #3026, #42752, #38273, #38289, #46699, #16771, #13818, #25539, #31956, #53458, #37087, #55186, #6204, #35479, #39333, #40487, #1756, #52332, #17189, #14023, #5248, #33483, #8325, #61368, #28897, #10335, #4653, #29327, #6920, #17498, #50979, #41548, #29065, #49104, #29066, #30762, #43478, #60100, #44792, #60716, #26845, #46340, #61737, #2200, #28010, #54502, #46183, #1857, #7858, #38253, #29642, #28903, #14595, #7939, #8287, #25947, #36614, #245, #3917, #1131, #31996, #13808, #43948 ) ) ;
#16059 = CARTESIAN_POINT ( 'NONE',  ( 0.8560838555295158248, -45.77741231505087427, -10.23725333375899105 ) ) ;
#16060 = EDGE_CURVE ( 'NONE', #9752, #52483, #36164, .T. ) ;
#16061 = ORIENTED_EDGE ( 'NONE', *, *, #2954, .T. ) ;
#16062 = EDGE_CURVE ( 'NONE', #28594, #54914, #14525, .T. ) ;
#16063 = CARTESIAN_POINT ( 'NONE',  ( 0.6017666602106489515, -18.08695057064621992, 44.57804174182690815 ) ) ;
#16064 = CIRCLE ( 'NONE', #17054, 2.649999999999997691 ) ;
#16065 = CARTESIAN_POINT ( 'NONE',  ( 0.5782707292762442330, 16.17912178775479504, 44.02240761117701595 ) ) ;
#16066 = LINE ( 'NONE', #11358, #17265 ) ;
#16067 = CARTESIAN_POINT ( 'NONE',  ( 0.8551540677456739292, 37.45266983663496063, 29.88829867897826631 ) ) ;
#16069 = ADVANCED_FACE ( 'NONE', ( #61014 ), #25161, .F. ) ;
#16068 = ORIENTED_EDGE ( 'NONE', *, *, #41173, .F. ) ;
#16070 = ORIENTED_EDGE ( 'NONE', *, *, #26132, .T. ) ;
#16071 = CARTESIAN_POINT ( 'NONE',  ( 0.5809828226811553087, 37.66417181417592275, -29.58751527316140795 ) ) ;
#16072 = CARTESIAN_POINT ( 'NONE',  ( 0.5804410086790514622, -14.41595396256412620, -44.62846763227064173 ) ) ;
#16073 = ADVANCED_FACE ( 'NONE', ( #32225 ), #52226, .T. ) ;
#16074 = B_SPLINE_CURVE_WITH_KNOTS ( 'NONE', 3,
 ( #53675, #29891, #47621, #37624, #23891, #32291 ),
 .UNSPECIFIED., .F., .F.,
 ( 4, 2, 4 ),
 ( 1.084202172485504434E-19, 0.0002445244328975357219, 0.0004890488657950713353 ),
 .UNSPECIFIED. ) ;
#16075 = FACE_OUTER_BOUND ( 'NONE', #53702, .T. ) ;
#16076 = ORIENTED_EDGE ( 'NONE', *, *, #46382, .F. ) ;
#16077 = CARTESIAN_POINT ( 'NONE',  ( 0.5786265663353153954, -34.37803667029788812, -33.35675271369575512 ) ) ;
#16078 = CARTESIAN_POINT ( 'NONE',  ( -2.739355103387248747, 11.53562761125299474, 9.475065306662248332 ) ) ;
#16079 = CARTESIAN_POINT ( 'NONE',  ( 0.5804410086790514622, 46.89585601637878653, -0.5463884574786393999 ) ) ;
#16080 = CARTESIAN_POINT ( 'NONE',  ( 0.7762777257811928067, 29.86325207275931959, -37.45705273430974103 ) ) ;
#16081 = ORIENTED_EDGE ( 'NONE', *, *, #4331, .F. ) ;
#16082 = ORIENTED_EDGE ( 'NONE', *, *, #15200, .F. ) ;
#16083 = CARTESIAN_POINT ( 'NONE',  ( 4.694002226626920127, 6.935496447963913624, -45.05755941533467279 ) ) ;
#16084 = CARTESIAN_POINT ( 'NONE',  ( 0.1100053167205930632, 34.32189548568247517, 26.10991185395899450 ) ) ;
#16085 = CARTESIAN_POINT ( 'NONE',  ( 2.282816707992319394, 3.392768508892113566, -46.85067863172353952 ) ) ;
#16086 = CARTESIAN_POINT ( 'NONE',  ( 1.227938101723756947, -33.52879263017882039, 26.79402671879314823 ) ) ;
#16087 = CARTESIAN_POINT ( 'NONE',  ( 0.2885700199627512785, -43.10898996868492361, 0.8047882683537324056 ) ) ;
#16088 = DIRECTION ( 'NONE',  ( 0.000000000000000000, 0.000000000000000000, 1.000000000000000000 ) ) ;
#16089 = CARTESIAN_POINT ( 'NONE',  ( 0.9268187852002115479, -13.49168632951830737, -41.97295239668654432 ) ) ;
#16090 = CARTESIAN_POINT ( 'NONE',  ( -6.016761891674565099, 11.46828378093559131, 14.95139917749708758 ) ) ;
#16091 = CARTESIAN_POINT ( 'NONE',  ( -6.001507490154111224, -18.19774963328904960, -4.892199142591494798 ) ) ;
#16092 = CARTESIAN_POINT ( 'NONE',  ( 5.860006189529246790, 3.171667470663204647, -48.12869875779304607 ) ) ;
#16093 = B_SPLINE_CURVE_WITH_KNOTS ( 'NONE', 3,
 ( #38117, #28995, #37487, #37813, #5470, #23372, #24607, #33097, #56563, #13677, #32786, #51863, #8961, #42498, #57162, #52170, #14296, #9262, #28371 ),
 .UNSPECIFIED., .F., .F.,
 ( 4, 3, 3, 3, 3, 3, 4 ),
 ( 1.250973872328959472E-17, 0.0002732106629380605888, 0.0004098138914053748357, 0.0005464171197651485328, 0.0006830203481512556575, 0.0008196235766963574530, 0.001011968216111140293 ),
 .UNSPECIFIED. ) ;
#16094 = CARTESIAN_POINT ( 'NONE',  ( 1.827326673878743035, -20.44853789448427506, -37.88339879236853136 ) ) ;
#16095 = CARTESIAN_POINT ( 'NONE',  ( 0.8554163680231738898, 39.89400665120432876, 24.69157156653835017 ) ) ;
#16096 = DIRECTION ( 'NONE',  ( 0.1024043820194936449, -0.8679729669084581545, -0.4859385467930429359 ) ) ;
#16097 = DIRECTION ( 'NONE',  ( -0.000000000000000000, -1.000000000000000000, -0.000000000000000000 ) ) ;
#16098 = CARTESIAN_POINT ( 'NONE',  ( 0.5830081025819920937, -14.15482648850689529, -44.70875665305972291 ) ) ;
#16099 = CARTESIAN_POINT ( 'NONE',  ( 0.8744876279028263033, -38.80702141274021955, -30.07266432244763621 ) ) ;
#16100 = CONTEXT_DEPENDENT_SHAPE_REPRESENTATION ( #59566, #44412 ) ;
#16101 = CARTESIAN_POINT ( 'NONE',  ( 0.9752570700956788574, -26.30364510018335267, 33.90066715551964194 ) ) ;
#16102 = EDGE_CURVE ( 'NONE', #29930, #28235, #9290, .T. ) ;
#16103 = CARTESIAN_POINT ( 'NONE',  ( 0.2230388203127608715, 43.11276071378623698, -0.7599700551095819323 ) ) ;
#16105 =( BOUNDED_SURFACE ( )  B_SPLINE_SURFACE ( 3, 1, ( 
 ( #10314, #38843 ),
 ( #48221, #58826 ),
 ( #29714, #15947 ),
 ( #29407, #35371 ) ),
 .UNSPECIFIED., .F., .F., .F. ) 
 B_SPLINE_SURFACE_WITH_KNOTS ( ( 4, 4 ),
 ( 2, 2 ),
 ( 0.000000000000000000, 1.000000000000000000 ),
 ( 0.000000000000000000, 1.000000000000000000 ),
 .UNSPECIFIED. ) 
 GEOMETRIC_REPRESENTATION_ITEM ( )  RATIONAL_B_SPLINE_SURFACE ( (
 ( 1.000000000000000000, 1.000000000000000000),
 ( 0.9751682680413298332, 0.9999560080971552356),
 ( 0.9751682680413298332, 0.9999560080971552356),
 ( 1.000000000000000000, 1.000000000000000000) ) ) 
 REPRESENTATION_ITEM ( '' )  SURFACE ( )  );
#16104 = FACE_OUTER_BOUND ( 'NONE', #21433, .T. ) ;
#16106 = CARTESIAN_POINT ( 'NONE',  ( 0.6029442701453591180, 49.00093189689916073, -3.233248891398188718 ) ) ;
#16108 = ORIENTED_EDGE ( 'NONE', *, *, #3103, .T. ) ;
#16107 = CARTESIAN_POINT ( 'NONE',  ( 1.231276596079887931, 38.25526645152051941, -17.14092645516095104 ) ) ;
#16109 = ORIENTED_EDGE ( 'NONE', *, *, #56062, .F. ) ;
#16110 = CARTESIAN_POINT ( 'NONE',  ( 0.8760168074887076939, 46.68716261866160266, 11.58706983520341893 ) ) ;
#16111 = CARTESIAN_POINT ( 'NONE',  ( 0.7413678028165011646, 43.93608276952824809, -3.755891723600084831 ) ) ;
#16112 = CARTESIAN_POINT ( 'NONE',  ( 0.5987334363312688534, -34.85272424572811900, -34.59552744392418333 ) ) ;
#16113 = ORIENTED_EDGE ( 'NONE', *, *, #34215, .T. ) ;
#16114 = ORIENTED_EDGE ( 'NONE', *, *, #23346, .T. ) ;
#16115 = CARTESIAN_POINT ( 'NONE',  ( 3.680882792899938138, -32.59085259319712691, 35.20667105325160406 ) ) ;
#16116 = CARTESIAN_POINT ( 'NONE',  ( 6.890143360408123030, -11.60930335864404306, 0.000000000000000000 ) ) ;
#16117 = CARTESIAN_POINT ( 'NONE',  ( 0.1103878639767399417, -37.32258098927782441, 21.60424693647491878 ) ) ;
#16118 = ORIENTED_EDGE ( 'NONE', *, *, #21428, .T. ) ;
#16119 = VERTEX_POINT ( 'NONE', #8386 ) ;
#16120 = CARTESIAN_POINT ( 'NONE',  ( 0.3676999524040366896, 29.04098611012985742, -33.20499524279568249 ) ) ;
#16121 =( BOUNDED_SURFACE ( )  B_SPLINE_SURFACE ( 3, 1, ( 
 ( #54591, #11720 ),
 ( #1978, #41164 ),
 ( #31429, #26727 ),
 ( #7927, #59928 ) ),
 .UNSPECIFIED., .F., .F., .F. ) 
 B_SPLINE_SURFACE_WITH_KNOTS ( ( 4, 4 ),
 ( 2, 2 ),
 ( 0.000000000000000000, 1.000000000000000000 ),
 ( 0.000000000000000000, 1.000000000000000000 ),
 .UNSPECIFIED. ) 
 GEOMETRIC_REPRESENTATION_ITEM ( )  RATIONAL_B_SPLINE_SURFACE ( (
 ( 1.000000000000000000, 1.000000000000000000),
 ( 0.9751682680413298332, 0.9999560080971552356),
 ( 0.9751682680413298332, 0.9999560080971552356),
 ( 1.000000000000000000, 1.000000000000000000) ) ) 
 REPRESENTATION_ITEM ( '' )  SURFACE ( )  );
#16122 = CARTESIAN_POINT ( 'NONE',  ( 0.7413678028165013867, -40.51427950544401568, 17.40917137387654989 ) ) ;
#16123 = CARTESIAN_POINT ( 'NONE',  ( 0.5806925824938502512, 17.36345040154772690, 43.56297685531322372 ) ) ;
#16124 = FACE_OUTER_BOUND ( 'NONE', #46360, .T. ) ;
#16125 =( BOUNDED_SURFACE ( )  B_SPLINE_SURFACE ( 3, 1, ( 
 ( #11827, #6761 ),
 ( #7386, #45041 ),
 ( #12750, #21511 ),
 ( #30588, #40649 ) ),
 .UNSPECIFIED., .F., .F., .F. ) 
 B_SPLINE_SURFACE_WITH_KNOTS ( ( 4, 4 ),
 ( 2, 2 ),
 ( 0.000000000000000000, 1.000000000000000000 ),
 ( 0.000000000000000000, 1.000000000000000000 ),
 .UNSPECIFIED. ) 
 GEOMETRIC_REPRESENTATION_ITEM ( )  RATIONAL_B_SPLINE_SURFACE ( (
 ( 1.000000000000000000, 1.000000000000000000),
 ( 0.9953485035131437453, 0.8621029689291515030),
 ( 0.9953485035131437453, 0.8621029689291515030),
 ( 1.000000000000000000, 1.000000000000000000) ) ) 
 REPRESENTATION_ITEM ( '' )  SURFACE ( )  );
#16126 = EDGE_LOOP ( 'NONE', ( #37310, #61065, #23238, #37045 ) ) ;
#16127 = CARTESIAN_POINT ( 'NONE',  ( 0.1119898979215349644, 4.795286723730743716, 43.86304291187561688 ) ) ;
#16128 = DIRECTION ( 'NONE',  ( 0.000000000000000000, 0.000000000000000000, -1.000000000000000000 ) ) ;
#16129 = EDGE_CURVE ( 'NONE', #30020, #50038, #23202, .T. ) ;
#16130 = CARTESIAN_POINT ( 'NONE',  ( 0.9752570700956806338, 42.51066151201240473, 5.829291291128810393 ) ) ;
#16131 = EDGE_CURVE ( 'NONE', #55350, #22095, #7166, .T. ) ;
#16132 = VERTEX_POINT ( 'NONE', #46637 ) ;
#16133 = ORIENTED_EDGE ( 'NONE', *, *, #1777, .F. ) ;
#16134 = ADVANCED_FACE ( 'NONE', ( #17814 ), #42555, .F. ) ;
#16135 = CARTESIAN_POINT ( 'NONE',  ( 0.7764139734771257073, 27.10005299892409170, 38.28351601358438216 ) ) ;
#16136 = CARTESIAN_POINT ( 'NONE',  ( 0.08486401232817714080, 0.000000000000000000, 0.000000000000000000 ) ) ;
#16137 = ORIENTED_EDGE ( 'NONE', *, *, #14049, .T. ) ;
#16138 = CARTESIAN_POINT ( 'NONE',  ( 1.227938101723756947, 20.72293514920803048, -37.58536632582757875 ) ) ;
#16139 = CARTESIAN_POINT ( 'NONE',  ( 0.5806925824938499181, -38.35106547415185929, -26.98922265166007861 ) ) ;
#16140 = EDGE_CURVE ( 'NONE', #56839, #43658, #8498, .T. ) ;
#16141 = CARTESIAN_POINT ( 'NONE',  ( 0.8560838555295223751, 17.70877843982779609, 43.43698884880053157 ) ) ;
#16142 = CARTESIAN_POINT ( 'NONE',  ( 0.5997462898726536595, -8.352924653000716404, 48.39194436975645175 ) ) ;
#16143 = ORIENTED_EDGE ( 'NONE', *, *, #22204, .F. ) ;
#16144 = CARTESIAN_POINT ( 'NONE',  ( 5.901764892641288895, -48.86589420182303201, 3.180542610297211858 ) ) ;
#16145 = LINE ( 'NONE', #59966, #32783 ) ;
#16146 = VECTOR ( 'NONE', #58281, 1000.000000000000114 ) ;
#16147 = CARTESIAN_POINT ( 'NONE',  ( 4.956653778116982600, -45.35992544608539845, 15.97476558431867844 ) ) ;
#16148 = ORIENTED_EDGE ( 'NONE', *, *, #6842, .T. ) ;
#16149 = CARTESIAN_POINT ( 'NONE',  ( 5.959828726073459926, -19.82504517499716812, 5.316791119500744678 ) ) ;
#16150 = CARTESIAN_POINT ( 'NONE',  ( 0.9762797500689124330, 3.691134646838137190, -41.74566217230977117 ) ) ;
#16151 = ORIENTED_EDGE ( 'NONE', *, *, #19292, .F. ) ;
#16152 = CARTESIAN_POINT ( 'NONE',  ( 4.691466044806102076, -44.46979273209132799, -3.249105306918271374 ) ) ;
#16153 = CARTESIAN_POINT ( 'NONE',  ( 5.896782393890504181, -19.93252920631905667, 2.687073932226298201 ) ) ;
#16154 = EDGE_CURVE ( 'NONE', #35697, #1749, #49086, .T. ) ;
#16155 = ORIENTED_EDGE ( 'NONE', *, *, #45632, .F. ) ;
#16156 = CARTESIAN_POINT ( 'NONE',  ( 0.2885697896453124911, 39.51953439758086262, 17.24062360132728955 ) ) ;
#16157 = CARTESIAN_POINT ( 'NONE',  ( 0.9730545539215883499, -37.40983423658458662, -21.01499094264588763 ) ) ;
#16158 = ADVANCED_FACE ( 'NONE', ( #34690 ), #9997, .F. ) ;
#16159 = CARTESIAN_POINT ( 'NONE',  ( 4.967162193818130511, 28.07411493385340862, -32.68434214048137676 ) ) ;
#16160 = B_SPLINE_CURVE_WITH_KNOTS ( 'NONE', 3,
 ( #29534, #1319, #21382, #55808 ),
 .UNSPECIFIED., .F., .F.,
 ( 4, 4 ),
 ( 0.000000000000000000, 0.005013413432710148512 ),
 .UNSPECIFIED. ) ;
#16161 = FACE_OUTER_BOUND ( 'NONE', #41120, .T. ) ;
#16162 = CARTESIAN_POINT ( 'NONE',  ( 4.956445790444004018, -45.27177431812791042, 12.96165499572219737 ) ) ;
#16163 = CARTESIAN_POINT ( 'NONE',  ( 5.896278296736517710, -7.233829247026454468, 18.76695750619285974 ) ) ;
#16164 = B_SPLINE_CURVE_WITH_KNOTS ( 'NONE', 3,
 ( #23249, #13867, #46766, #4719 ),
 .UNSPECIFIED., .F., .F.,
 ( 4, 4 ),
 ( 0.000000000000000000, 0.005004741218457429280 ),
 .UNSPECIFIED. ) ;
#16165 = CARTESIAN_POINT ( 'NONE',  ( 0.7762777257811898091, 47.89627391089018715, 0.8897018348887656414 ) ) ;
#16166 = CARTESIAN_POINT ( 'NONE',  ( 0.1084644655670281982, -41.75632203164224876, -10.77688306151788922 ) ) ;
#16167 = CARTESIAN_POINT ( 'NONE',  ( 5.901764892641307547, -16.87177170878291221, -45.97102116384180448 ) ) ;
#16168 = DIRECTION ( 'NONE',  ( 1.000000000000000000, 0.000000000000000000, 0.000000000000000000 ) ) ;
#16169 = CARTESIAN_POINT ( 'NONE',  ( 0.9790850452238860635, 15.10954715382613678, 39.09013833525667536 ) ) ;
#16170 = ORIENTED_EDGE ( 'NONE', *, *, #19412, .F. ) ;
#16171 = CARTESIAN_POINT ( 'NONE',  ( -17.83468216677388796, -12.32233744059949565, 2.099999999999995648 ) ) ;
#16172 = LINE ( 'NONE', #44092, #46379 ) ;
#16173 = CARTESIAN_POINT ( 'NONE',  ( 4.956445790444040433, 46.94638516972321440, -3.684422564748698115 ) ) ;
#16174 = CARTESIAN_POINT ( 'NONE',  ( 0.5807400328401574052, 41.20655774453003772, -24.41979442053125737 ) ) ;
#16175 = CARTESIAN_POINT ( 'NONE',  ( 1.154321485836934391, 41.23280395520824726, -11.90271791109269550 ) ) ;
#16176 = DIRECTION ( 'NONE',  ( 6.799271724612909333E-15, 1.000000000000000000, 3.491481338843132172E-15 ) ) ;
#16177 = CARTESIAN_POINT ( 'NONE',  ( 3.660087539127329759, -8.130906407639741929, -47.34518630204118494 ) ) ;
#16178 = ADVANCED_FACE ( 'NONE', ( #19062 ), #31580, .F. ) ;
#16179 = DIRECTION ( 'NONE',  ( 0.000000000000000000, -1.000000000000000000, 0.000000000000000000 ) ) ;
#16180 = CARTESIAN_POINT ( 'NONE',  ( 0.08486401232817714080, 9.539392014169456147, -3.000000000000000000 ) ) ;
#16182 = ORIENTED_EDGE ( 'NONE', *, *, #28199, .F. ) ;
#16181 = CARTESIAN_POINT ( 'NONE',  ( 0.8560838555295158248, 37.37287335782446718, -28.34856559090329142 ) ) ;
#16183 = ORIENTED_EDGE ( 'NONE', *, *, #12026, .F. ) ;
#16184 = CARTESIAN_POINT ( 'NONE',  ( -6.057079549204054558, 0.6087215340721632284, -19.24735538181013084 ) ) ;
#16185 = CARTESIAN_POINT ( 'NONE',  ( 5.974727161628369032, -14.52429704002373789, 14.50236057684819535 ) ) ;
#16186 = CARTESIAN_POINT ( 'NONE',  ( 0.1103310638050661874, 16.42686748615350112, 39.87325896099748235 ) ) ;
#16187 = ORIENTED_EDGE ( 'NONE', *, *, #14351, .F. ) ;
#16188 = CARTESIAN_POINT ( 'NONE',  ( 0.6001305935487315502, 41.92422178329169924, -23.60027211631785349 ) ) ;
#16189 = CARTESIAN_POINT ( 'NONE',  ( 5.896782393890504181, 3.351618377817072947, 19.83160964539921167 ) ) ;
#16190 = CARTESIAN_POINT ( 'NONE',  ( -6.017396004339687465, -14.95000090562889383, 11.47005965438133046 ) ) ;
#16191 = VECTOR ( 'NONE', #31984, 999.9999999999998863 ) ;
#16192 = ORIENTED_EDGE ( 'NONE', *, *, #8342, .T. ) ;
#16193 = VERTEX_POINT ( 'NONE', #5830 ) ;
#16194 = CARTESIAN_POINT ( 'NONE',  ( 0.8744876279028263033, 21.91587810745035725, 43.93226988398016886 ) ) ;
#16195 = CARTESIAN_POINT ( 'NONE',  ( 0.1102847568649952675, -11.25043675627769701, -41.63105453442833692 ) ) ;
#16196 = CARTESIAN_POINT ( 'NONE',  ( 0.6016117650947689910, 37.61761104844107706, 31.56685592916568694 ) ) ;
#16197 = VERTEX_POINT ( 'NONE', #5225 ) ;
#16198 = CARTESIAN_POINT ( 'NONE',  ( 4.975610109902397937, 0.000000000000000000, 48.91267123290010943 ) ) ;
#16199 = DIRECTION ( 'NONE',  ( -1.000000000000000000, -0.000000000000000000, -0.000000000000000000 ) ) ;
#16200 =( BOUNDED_SURFACE ( )  B_SPLINE_SURFACE ( 3, 1, ( 
 ( #50210, #45850 ),
 ( #60516, #36443 ),
 ( #51426, #41769 ),
 ( #17632, #55827 ) ),
 .UNSPECIFIED., .F., .F., .F. ) 
 B_SPLINE_SURFACE_WITH_KNOTS ( ( 4, 4 ),
 ( 2, 2 ),
 ( 0.000000000000000000, 1.000000000000000000 ),
 ( 0.000000000000000000, 1.000000000000000000 ),
 .UNSPECIFIED. ) 
 GEOMETRIC_REPRESENTATION_ITEM ( )  RATIONAL_B_SPLINE_SURFACE ( (
 ( 1.000000000000000000, 1.000000000000000000),
 ( 0.9953485035131437453, 0.8621029689291523912),
 ( 0.9953485035131437453, 0.8621029689291523912),
 ( 1.000000000000000000, 1.000000000000000000) ) ) 
 REPRESENTATION_ITEM ( '' )  SURFACE ( )  );
#16201 = ORIENTED_EDGE ( 'NONE', *, *, #59116, .F. ) ;
#16202 = CARTESIAN_POINT ( 'NONE',  ( 0.6000166863083106206, -13.47152005829798327, -47.22649287240508897 ) ) ;
#16203 = CARTESIAN_POINT ( 'NONE',  ( 0.9757787079277445708, 41.45659305953935814, -11.06737752163053834 ) ) ;
#16204 = EDGE_CURVE ( 'NONE', #59574, #19392, #53317, .T. ) ;
#16205 = ORIENTED_EDGE ( 'NONE', *, *, #29933, .T. ) ;
#16206 = CARTESIAN_POINT ( 'NONE',  ( 0.5830081025819898732, -34.59664839919615531, 31.65918435343287385 ) ) ;
#16207 = CARTESIAN_POINT ( 'NONE',  ( 0.9722240750034577550, 42.90442369954359947, -0.5819398758581642017 ) ) ;
#16208 = ORIENTED_EDGE ( 'NONE', *, *, #20241, .F. ) ;
#16209 = FACE_OUTER_BOUND ( 'NONE', #3179, .T. ) ;
#16210 = DIRECTION ( 'NONE',  ( 0.000000000000000000, 0.000000000000000000, 1.000000000000000000 ) ) ;
#16211 = EDGE_CURVE ( 'NONE', #11980, #46288, #57219, .T. ) ;
#16212 = CARTESIAN_POINT ( 'NONE',  ( 0.8744876279028306332, 49.04340454744548339, 2.257104511336577968 ) ) ;
#16213 = CARTESIAN_POINT ( 'NONE',  ( 5.901764892641288895, -41.06410928599452603, -26.67827573115581430 ) ) ;
#16214 = ORIENTED_EDGE ( 'NONE', *, *, #13379, .F. ) ;
#16215 = CARTESIAN_POINT ( 'NONE',  ( 0.1147471544378676211, 39.61889945511968847, -19.42408284677457075 ) ) ;
#16216 = ORIENTED_EDGE ( 'NONE', *, *, #27805, .F. ) ;
#16217 = FACE_OUTER_BOUND ( 'NONE', #42744, .T. ) ;
#16218 = VERTEX_POINT ( 'NONE', #47868 ) ;
#16219 = CARTESIAN_POINT ( 'NONE',  ( 0.9775691876210979014, 3.818852833867097729, 41.73427933992938677 ) ) ;
#16220 = VERTEX_POINT ( 'NONE', #43806 ) ;
#16221 = CARTESIAN_POINT ( 'NONE',  ( 0.5997462898726536595, 10.41743419021273631, 47.98988117339838055 ) ) ;
#16222 = LINE ( 'NONE', #19693, #35442 ) ;
#16223 = VERTEX_POINT ( 'NONE', #52538 ) ;
#16224 = CARTESIAN_POINT ( 'NONE',  ( 0.2940135542859019235, 41.60821252483800947, -14.66278279111214822 ) ) ;
#16225 = LINE ( 'NONE', #54099, #18793 ) ;
#16226 = ADVANCED_FACE ( 'NONE', ( #19984, #39098 ), #4915, .T. ) ;
#16227 = CARTESIAN_POINT ( 'NONE',  ( 5.894904586330512508, -7.227592724925631984, -18.76942501687904041 ) ) ;
#16228 = EDGE_LOOP ( 'NONE', ( #4075, #49035, #60662, #57700 ) ) ;
#16229 = B_SPLINE_CURVE_WITH_KNOTS ( 'NONE', 3,
 ( #41142, #21390, #50199, #11375 ),
 .UNSPECIFIED., .F., .F.,
 ( 4, 4 ),
 ( 0.000000000000000000, 0.005004741218457415403 ),
 .UNSPECIFIED. ) ;
#16230 = VECTOR ( 'NONE', #12031, 1000.000000000000114 ) ;
#16231 = ORIENTED_EDGE ( 'NONE', *, *, #58797, .T. ) ;
#16232 = VECTOR ( 'NONE', #36441, 1000.000000000000114 ) ;
#16233 = CARTESIAN_POINT ( 'NONE',  ( 0.9775691876210976794, -30.82697754998653039, -28.39068798255189208 ) ) ;
#16234 = CARTESIAN_POINT ( 'NONE',  ( -1.500000000000001332, 0.000000000000000000, -7.400000000000021672 ) ) ;
#16235 = CARTESIAN_POINT ( 'NONE',  ( 0.9762797500689124330, 38.38274741215490593, -16.82526333465304091 ) ) ;
#16236 = CARTESIAN_POINT ( 'NONE',  ( 0.1103744047535531458, -5.590449877750299557, -42.76053735246610188 ) ) ;
#16237 = LINE ( 'NONE', #41834, #43578 ) ;
#16238 = CARTESIAN_POINT ( 'NONE',  ( 0.9787464366903561030, 38.51372612363144299, 16.52352543994085110 ) ) ;
#16239 = ORIENTED_EDGE ( 'NONE', *, *, #50456, .T. ) ;
#16240 = DIRECTION ( 'NONE',  ( -1.000000000000000000, -3.135800716341489291E-16, 1.298891185607901956E-16 ) ) ;
#16241 = CARTESIAN_POINT ( 'NONE',  ( 4.691466044806103852, -19.42108863068406066, 40.13652286047860684 ) ) ;
#16242 = VERTEX_POINT ( 'NONE', #34384 ) ;
#16243 = CARTESIAN_POINT ( 'NONE',  ( 4.553261556744873317, -33.30082861731504096, 28.64601855797499042 ) ) ;
#16244 = CARTESIAN_POINT ( 'NONE',  ( 0.6021447746440204973, -20.11649849682114777, -44.79807615641413321 ) ) ;
#16245 = CARTESIAN_POINT ( 'NONE',  ( 5.959828726073459926, -10.25888482581871841, 17.77796293532155048 ) ) ;
#16246 = CARTESIAN_POINT ( 'NONE',  ( 4.967162193818130511, -40.65506779172153529, -14.26841313271325795 ) ) ;
#16247 = CARTESIAN_POINT ( 'NONE',  ( 4.975801465491695552, -20.67815041659169495, 43.22084481528186473 ) ) ;
#16248 = CARTESIAN_POINT ( 'NONE',  ( 5.974727161628367256, -19.82156119440448805, 5.327229920347082093 ) ) ;
#16249 = EDGE_CURVE ( 'NONE', #34782, #40429, #24980, .T. ) ;
#16250 = CARTESIAN_POINT ( 'NONE',  ( 0.6021448801613057400, 37.56148455560388300, -31.63346355690565304 ) ) ;
#16251 = CARTESIAN_POINT ( 'NONE',  ( 0.1139756605157202229, 29.95793622539913414, 32.39563669400465784 ) ) ;
#16252 = LINE ( 'NONE', #53517, #60831 ) ;
#16253 = SURFACE_STYLE_FILL_AREA ( #12495 ) ;
#16254 = CARTESIAN_POINT ( 'NONE',  ( 1.479689385636123067, -21.82878006710240015, 38.27647065822245764 ) ) ;
#16255 = PRODUCT ( 'needle roller bearing_nh_iso_ISO 3245 - 2521D - 24,SI,NC,24', 'needle roller bearing_nh_iso_ISO 3245 - 2521D - 24,SI,NC,24', '', ( #17404 ) ) ;
#16256 = CARTESIAN_POINT ( 'NONE',  ( 0.5807400328401637335, 34.25275203086236075, 33.48217046439123834 ) ) ;
#16257 = DIRECTION ( 'NONE',  ( -2.280301054154487250E-31, 0.000000000000000000, 1.000000000000000000 ) ) ;
#16258 = EDGE_CURVE ( 'NONE', #22153, #14826, #19732, .T. ) ;
#16259 = EDGE_LOOP ( 'NONE', ( #4678, #12622, #35857, #47314 ) ) ;
#16260 = ADVANCED_FACE ( 'NONE', ( #24048 ), #57155, .F. ) ;
#16261 = DIRECTION ( 'NONE',  ( 1.000000000000000000, 1.836909530733573776E-16, 0.000000000000000000 ) ) ;
#16262 = CARTESIAN_POINT ( 'NONE',  ( 0.1102144999581332885, 43.12427761225339395, 0.1260305566213565931 ) ) ;
#16263 = CARTESIAN_POINT ( 'NONE',  ( 0.1129192098497447394, -38.68182264534125636, -21.22895156665819627 ) ) ;
#16264 = CARTESIAN_POINT ( 'NONE',  ( 4.956445790444035104, 41.78282513192535674, -21.71942849465849079 ) ) ;
#16265 = CARTESIAN_POINT ( 'NONE',  ( 0.1102847568649952675, -41.63105453442844350, 11.25043675627726181 ) ) ;
#16266 = EDGE_LOOP ( 'NONE', ( #33612, #14257, #5424, #54782 ) ) ;
#16267 = CARTESIAN_POINT ( 'NONE',  ( 2.528100132419517809, -33.91014296975959041, 24.74582757562452784 ) ) ;
#16268 = CARTESIAN_POINT ( 'NONE',  ( 0.6027444965799114707, 28.20219763130657498, -40.20167365486376099 ) ) ;
#16269 =( GEOMETRIC_REPRESENTATION_CONTEXT ( 3 ) GLOBAL_UNCERTAINTY_ASSIGNED_CONTEXT ( ( #36784 ) ) GLOBAL_UNIT_ASSIGNED_CONTEXT ( ( #43873, #53828, #44795 ) ) REPRESENTATION_CONTEXT ( 'NONE', 'WORKASPACE' ) );
#16270 = CARTESIAN_POINT ( 'NONE',  ( -2.739355103387247858, 8.323596231104264831, 12.39214722042002848 ) ) ;
#16271 = ORIENTED_EDGE ( 'NONE', *, *, #11848, .F. ) ;
#16272 = DIRECTION ( 'NONE',  ( -0.1011922191286467460, -0.9018493587347873319, 0.4200331759962215306 ) ) ;
#16273 = B_SPLINE_CURVE_WITH_KNOTS ( 'NONE', 3,
 ( #48915, #39237, #48602, #58286 ),
 .UNSPECIFIED., .F., .F.,
 ( 4, 4 ),
 ( 8.673617379884035472E-19, 0.004050076154993002484 ),
 .UNSPECIFIED. ) ;
#16274 = DIRECTION ( 'NONE',  ( 0.07500201931887537365, 0.8144017028153685001, 0.5754342391181805905 ) ) ;
#16275 = EDGE_CURVE ( 'NONE', #12288, #4388, #49550, .T. ) ;
#16276 = ORIENTED_EDGE ( 'NONE', *, *, #61491, .F. ) ;
#16277 = CARTESIAN_POINT ( 'NONE',  ( 4.549368137175248350, 0.000000000000000000, 0.000000000000000000 ) ) ;
#16278 = VERTEX_POINT ( 'NONE', #1445 ) ;
#16279 = CARTESIAN_POINT ( 'NONE',  ( 0.8551540677456739292, -29.88829867897839421, 37.45266983663486826 ) ) ;
#16281 = ORIENTED_EDGE ( 'NONE', *, *, #19061, .F. ) ;
#16280 = EDGE_CURVE ( 'NONE', #5623, #43495, #13751, .T. ) ;
#16282 = DIRECTION ( 'NONE',  ( 0.000000000000000000, 0.000000000000000000, -1.000000000000000000 ) ) ;
#16283 = CARTESIAN_POINT ( 'NONE',  ( 0.1147471544378675795, 20.68395129688062895, 38.97597140831149432 ) ) ;
#16284 = ORIENTED_EDGE ( 'NONE', *, *, #25020, .F. ) ;
#16285 = ORIENTED_EDGE ( 'NONE', *, *, #19201, .T. ) ;
#16286 = EDGE_CURVE ( 'NONE', #18521, #35798, #7068, .T. ) ;
#16287 = CARTESIAN_POINT ( 'NONE',  ( 7.000000000000007105, -2.650000000000277467, 80.00000000000000000 ) ) ;
#16288 = TOROIDAL_SURFACE ( 'NONE', #12321, 12.55882000000000076, 0.05882000000000109363 ) ;
#16289 = ORIENTED_EDGE ( 'NONE', *, *, #11207, .F. ) ;
#16290 = ORIENTED_EDGE ( 'NONE', *, *, #24116, .F. ) ;
#16291 = DIRECTION ( 'NONE',  ( 0.000000000000000000, 0.000000000000000000, 1.000000000000000000 ) ) ;
#16292 = CARTESIAN_POINT ( 'NONE',  ( -6.078457390727109555, -17.35098001992631822, 8.350928294843967592 ) ) ;
#16293 = CARTESIAN_POINT ( 'NONE',  ( 3.783278058412224976, -20.00643011788481829, 38.10568111914496825 ) ) ;
#16294 = DIRECTION ( 'NONE',  ( -0.1024043820194934507, -0.5950744814819135531, -0.7971196296869356157 ) ) ;
#16295 = CARTESIAN_POINT ( 'NONE',  ( 0.5786265663353196143, 17.66171603226080222, 44.52624106864148246 ) ) ;
#16296 = ORIENTED_EDGE ( 'NONE', *, *, #47913, .F. ) ;
#16297 = CARTESIAN_POINT ( 'NONE',  ( -6.078726893082806448, -18.27395335922917141, -6.070969436048653911 ) ) ;
#16298 = EDGE_CURVE ( 'NONE', #34962, #43681, #28201, .T. ) ;
#16299 = ORIENTED_EDGE ( 'NONE', *, *, #13006, .F. ) ;
#16300 = CARTESIAN_POINT ( 'NONE',  ( 4.956653778116966613, 0.000000000000000000, 0.000000000000000000 ) ) ;
#16301 = ORIENTED_EDGE ( 'NONE', *, *, #47729, .T. ) ;
#16302 = CARTESIAN_POINT ( 'NONE',  ( 0.09136607875274982415, 0.000000000000000000, 3.000000000000000000 ) ) ;
#16303 = DIRECTION ( 'NONE',  ( 0.000000000000000000, 0.7071067811865382469, 0.7071067811865566766 ) ) ;
#16304 = VERTEX_POINT ( 'NONE', #49693 ) ;
#16305 = LINE ( 'NONE', #49197, #44606 ) ;
#16306 = CARTESIAN_POINT ( 'NONE',  ( 0.8753041380234530822, 36.80657072176735056, -32.50253343320360244 ) ) ;
#16307 = CARTESIAN_POINT ( 'NONE',  ( 0.7954190325252782356, -0.8690070772085950468, -48.09103420665682194 ) ) ;
#16308 = DIRECTION ( 'NONE',  ( 0.000000000000000000, 0.000000000000000000, -1.000000000000000000 ) ) ;
#16309 = ORIENTED_EDGE ( 'NONE', *, *, #42453, .T. ) ;
#16310 = CARTESIAN_POINT ( 'NONE',  ( 0.8760168074887090262, -33.37827814204149490, 34.63873394077429424 ) ) ;
#16311 = ORIENTED_EDGE ( 'NONE', *, *, #9148, .F. ) ;
#16312 = CARTESIAN_POINT ( 'NONE',  ( 4.975610109902397937, 0.000000000000000000, 0.000000000000000000 ) ) ;
#16313 = CARTESIAN_POINT ( 'NONE',  ( 3.673643420401900173, 2.497823135841254150, -5.351519936625005691 ) ) ;
#16314 = AXIS2_PLACEMENT_3D ( 'NONE', #37362, #37996, #36 ) ;
#16315 = CARTESIAN_POINT ( 'NONE',  ( -6.078457390727109555, -18.27642172158497758, -6.063573211587741874 ) ) ;
#16316 =( BOUNDED_SURFACE ( )  B_SPLINE_SURFACE ( 3, 1, ( 
 ( #49565, #54249 ),
 ( #25450, #58329 ),
 ( #29537, #11368 ),
 ( #16375, #48645 ) ),
 .UNSPECIFIED., .F., .F., .F. ) 
 B_SPLINE_SURFACE_WITH_KNOTS ( ( 4, 4 ),
 ( 2, 2 ),
 ( 0.000000000000000000, 1.000000000000000000 ),
 ( 0.000000000000000000, 1.000000000000000000 ),
 .UNSPECIFIED. ) 
 GEOMETRIC_REPRESENTATION_ITEM ( )  RATIONAL_B_SPLINE_SURFACE ( (
 ( 1.000000000000000000, 1.000000000000000000),
 ( 0.9953390228620291325, 0.8624445117761032620),
 ( 0.9953390228620291325, 0.8624445117761032620),
 ( 1.000000000000000000, 1.000000000000000000) ) ) 
 REPRESENTATION_ITEM ( '' )  SURFACE ( )  );
#16317 = CARTESIAN_POINT ( 'NONE',  ( 4.549368137175248350, 0.000000000000000000, 0.000000000000000000 ) ) ;
#16318 = DIRECTION ( 'NONE',  ( -1.000000000000000000, -1.836909530733573776E-16, 1.925929944387235853E-32 ) ) ;
#16319 = EDGE_CURVE ( 'NONE', #29746, #18686, #51103, .T. ) ;
#16320 = CARTESIAN_POINT ( 'NONE',  ( 4.834790513006555379, -47.18049212391682090, -2.567197668549027423 ) ) ;
#16321 = DIRECTION ( 'NONE',  ( 0.07906939808003032866, 0.8860534191553557370, 0.4567902896191699535 ) ) ;
#16322 = ADVANCED_FACE ( 'NONE', ( #7377 ), #8210, .T. ) ;
#16323 = FACE_OUTER_BOUND ( 'NONE', #7075, .T. ) ;
#16324 = CIRCLE ( 'NONE', #56329, 0.02570000000000870199 ) ;
#16325 = CARTESIAN_POINT ( 'NONE',  ( 2.526552050251864134, 27.11558601691313797, -33.34585601411836109 ) ) ;
#16326 = ADVANCED_FACE ( 'NONE', ( #31841 ), #40270, .T. ) ;
#16327 = B_SPLINE_CURVE_WITH_KNOTS ( 'NONE', 3,
 ( #30036, #36535, #6199, #1830, #41238, #55601 ),
 .UNSPECIFIED., .F., .F.,
 ( 4, 2, 4 ),
 ( 1.843143693225357538E-18, 0.0002447193893791703586, 0.0004894387787583388740 ),
 .UNSPECIFIED. ) ;
#16328 = ADVANCED_FACE ( 'NONE', ( #45957 ), #20783, .F. ) ;
#16329 = CARTESIAN_POINT ( 'NONE',  ( 0.1310142868023689566, 33.82067078731310517, 26.75450212504333436 ) ) ;
#16330 = CARTESIAN_POINT ( 'NONE',  ( 0.1158403557922069033, 36.95925186148238595, 24.10298755389733572 ) ) ;
#16331 = ORIENTED_EDGE ( 'NONE', *, *, #44797, .T. ) ;
#16332 = LINE ( 'NONE', #50161, #51898 ) ;
#16333 = CARTESIAN_POINT ( 'NONE',  ( 3.678834586032788234, 48.95863180854046703, -1.290248450541623182 ) ) ;
#16334 = CARTESIAN_POINT ( 'NONE',  ( 3.678834586032788234, -44.67002089670381793, -20.07988054537172928 ) ) ;
#16335 = ORIENTED_EDGE ( 'NONE', *, *, #56160, .T. ) ;
#16336 = CARTESIAN_POINT ( 'NONE',  ( 3.680882792899938138, -22.36818923730799114, 42.44216617524777746 ) ) ;
#16337 = LINE ( 'NONE', #54524, #50948 ) ;
#16338 = B_SPLINE_CURVE_WITH_KNOTS ( 'NONE', 3,
 ( #10589, #29682, #39118, #10906 ),
 .UNSPECIFIED., .F., .F.,
 ( 4, 4 ),
 ( 1.301042606982605321E-18, 0.004446298630425058948 ),
 .UNSPECIFIED. ) ;
#16339 = B_SPLINE_CURVE_WITH_KNOTS ( 'NONE', 3,
 ( #59021, #35250, #15826, #20829, #29910, #44057 ),
 .UNSPECIFIED., .F., .F.,
 ( 4, 2, 4 ),
 ( 0.000000000000000000, 0.0002293801035737105375, 0.0004587602071474210751 ),
 .UNSPECIFIED. ) ;
#16340 = CARTESIAN_POINT ( 'NONE',  ( 1.827326673878743479, -42.82501343454098475, 4.394636550975911327 ) ) ;
#16341 = EDGE_LOOP ( 'NONE', ( #49112, #23294 ) ) ;
#16343 = CARTESIAN_POINT ( 'NONE',  ( 5.960721111146673579, 12.50019045452716426, 16.28018152803696950 ) ) ;
#16342 = B_SPLINE_CURVE_WITH_KNOTS ( 'NONE', 3,
 ( #19276, #23351, #61836, #48083, #38394, #18979 ),
 .UNSPECIFIED., .F., .F.,
 ( 4, 2, 4 ),
 ( 5.421010862427522170E-19, 0.0002293801035737082065, 0.0004587602071474158709 ),
 .UNSPECIFIED. ) ;
#16344 = CARTESIAN_POINT ( 'NONE',  ( 0.9740398440564304039, -41.55177796653840261, -10.70454588197330814 ) ) ;
#16345 = ADVANCED_FACE ( 'NONE', ( #37169 ), #13668, .F. ) ;
#16346 = ORIENTED_EDGE ( 'NONE', *, *, #21046, .F. ) ;
#16347 = CARTESIAN_POINT ( 'NONE',  ( 0.5807400328401574052, -47.41494605191447675, 6.791881299635412539 ) ) ;
#16349 = ORIENTED_EDGE ( 'NONE', *, *, #17076, .T. ) ;
#16348 = EDGE_CURVE ( 'NONE', #16747, #30367, #8018, .T. ) ;
#16350 = VERTEX_POINT ( 'NONE', #36864 ) ;
#16351 = CARTESIAN_POINT ( 'NONE',  ( -6.072942160501519027, 7.781335985898283347, 17.61405610765404717 ) ) ;
#16352 = VERTEX_POINT ( 'NONE', #26824 ) ;
#16353 = DIRECTION ( 'NONE',  ( 0.07836865515943411409, 0.5052769534812749930, -0.8593913859058531779 ) ) ;
#16354 = AXIS2_PLACEMENT_3D ( 'NONE', #46376, #17865, #3423 ) ;
#16355 = CARTESIAN_POINT ( 'NONE',  ( -6.017396004339686577, 16.31924478664274858, 9.420565012089484824 ) ) ;
#16356 = VERTEX_POINT ( 'NONE', #56239 ) ;
#16357 = CARTESIAN_POINT ( 'NONE',  ( 0.1097557419366048670, 0.2231007852153696347, 43.12388302211984126 ) ) ;
#16358 = EDGE_CURVE ( 'NONE', #33849, #45637, #27154, .T. ) ;
#16359 = CARTESIAN_POINT ( 'NONE',  ( 5.895596859100789899, -19.93390588528923857, 2.677233529021818104 ) ) ;
#16360 = ORIENTED_EDGE ( 'NONE', *, *, #30598, .F. ) ;
#16361 = CARTESIAN_POINT ( 'NONE',  ( 0.5998501479064699549, -17.92509395669137362, 44.64337787626217846 ) ) ;
#16362 = DIRECTION ( 'NONE',  ( 0.000000000000000000, 0.000000000000000000, 1.000000000000000000 ) ) ;
#16363 = CARTESIAN_POINT ( 'NONE',  ( 0.1100053167205930771, -30.36644426605161229, 30.62023953839029744 ) ) ;
#16364 = CARTESIAN_POINT ( 'NONE',  ( 0.9780303403264775097, 36.22227486202688596, 21.07810278974036677 ) ) ;
#16365 = ORIENTED_EDGE ( 'NONE', *, *, #59609, .F. ) ;
#16366 = EDGE_CURVE ( 'NONE', #18623, #6436, #42240, .T. ) ;
#16367 = AXIS2_PLACEMENT_3D ( 'NONE', #53099, #5165, #44359 ) ;
#16368 = ORIENTED_EDGE ( 'NONE', *, *, #29906, .F. ) ;
#16369 = CARTESIAN_POINT ( 'NONE',  ( 0.1081432562775999223, 41.54352569227145864, 11.56998286599550241 ) ) ;
#16370 =( BOUNDED_SURFACE ( )  B_SPLINE_SURFACE ( 3, 1, ( 
 ( #21076, #59270 ),
 ( #35191, #15770 ),
 ( #34880, #58643 ),
 ( #39589, #39904 ) ),
 .UNSPECIFIED., .F., .F., .F. ) 
 B_SPLINE_SURFACE_WITH_KNOTS ( ( 4, 4 ),
 ( 2, 2 ),
 ( 0.000000000000000000, 1.000000000000000000 ),
 ( 0.000000000000000000, 1.000000000000000000 ),
 .UNSPECIFIED. ) 
 GEOMETRIC_REPRESENTATION_ITEM ( )  RATIONAL_B_SPLINE_SURFACE ( (
 ( 1.000000000000000000, 1.000000000000000000),
 ( 0.7282232189291694135, 0.9929344683865672927),
 ( 0.7282232189291694135, 0.9929344683865672927),
 ( 1.000000000000000000, 1.000000000000000000) ) ) 
 REPRESENTATION_ITEM ( '' )  SURFACE ( )  );
#16371 = EDGE_CURVE ( 'NONE', #56097, #4099, #24149, .T. ) ;
#16372 = DIRECTION ( 'NONE',  ( 1.000000000000000000, 1.836970198721027962E-16, -2.033782021272921061E-31 ) ) ;
#16373 = CARTESIAN_POINT ( 'NONE',  ( 3.894904216938898323, 13.07376739574732660, -41.96666461083243860 ) ) ;
#16374 = ORIENTED_EDGE ( 'NONE', *, *, #40172, .F. ) ;
#16375 = CARTESIAN_POINT ( 'NONE',  ( 5.960721111146673579, -17.77882586010660049, -10.25731071096576486 ) ) ;
#16376 = CARTESIAN_POINT ( 'NONE',  ( 0.6253024248130463203, 48.06489359206558021, 10.06032958709880099 ) ) ;
#16377 = CARTESIAN_POINT ( 'NONE',  ( 3.727782113643637096, 7.686874865524217171, -43.28613785853096374 ) ) ;
#16378 = CARTESIAN_POINT ( 'NONE',  ( 0.8557997880470690211, 41.93815086860257679, 23.15977007032337553 ) ) ;
#16379 = ORIENTED_EDGE ( 'NONE', *, *, #42254, .T. ) ;
#16380 = ORIENTED_EDGE ( 'NONE', *, *, #54284, .T. ) ;
#16381 = CARTESIAN_POINT ( 'NONE',  ( 0.9780106845699476636, -39.48577557688840045, -14.04296170852301628 ) ) ;
#16382 = CARTESIAN_POINT ( 'NONE',  ( 0.5998501479064699549, 28.86886762351124958, -38.48283596222000114 ) ) ;
#16383 = CARTESIAN_POINT ( 'NONE',  ( 0.1097557419366048670, -39.75589591229798714, 16.70891382096300148 ) ) ;
#16384 = CARTESIAN_POINT ( 'NONE',  ( 3.661921753702027438, 35.71933374875705880, -30.60654048367672786 ) ) ;
#16385 = B_SPLINE_CURVE_WITH_KNOTS ( 'NONE', 3,
 ( #50276, #39994, #10850, #1719 ),
 .UNSPECIFIED., .F., .F.,
 ( 4, 4 ),
 ( 0.000000000000000000, 0.005013413432710142441 ),
 .UNSPECIFIED. ) ;
#16386 = CARTESIAN_POINT ( 'NONE',  ( 0.3676999524040366896, 16.00695768809390884, 41.10629986868691077 ) ) ;
#16387 =( BOUNDED_SURFACE ( )  B_SPLINE_SURFACE ( 3, 1, ( 
 ( #38863, #15045 ),
 ( #1520, #30047 ),
 ( #34765, #47937 ),
 ( #34152, #4983 ) ),
 .UNSPECIFIED., .F., .F., .F. ) 
 B_SPLINE_SURFACE_WITH_KNOTS ( ( 4, 4 ),
 ( 2, 2 ),
 ( 0.000000000000000000, 1.000000000000000000 ),
 ( 0.000000000000000000, 1.000000000000000000 ),
 .UNSPECIFIED. ) 
 GEOMETRIC_REPRESENTATION_ITEM ( )  RATIONAL_B_SPLINE_SURFACE ( (
 ( 1.000000000000000000, 1.000000000000000000),
 ( 0.9952954269826590483, 0.8620686068821307169),
 ( 0.9952954269826590483, 0.8620686068821307169),
 ( 1.000000000000000000, 1.000000000000000000) ) ) 
 REPRESENTATION_ITEM ( '' )  SURFACE ( )  );
#16388 = CARTESIAN_POINT ( 'NONE',  ( 0.9268187852002115479, -41.22770443219307168, -15.62148264923511576 ) ) ;
#16389 = CARTESIAN_POINT ( 'NONE',  ( -6.015611763856276717, -14.95313250337437871, 11.46610900684717471 ) ) ;
#16390 = CARTESIAN_POINT ( 'NONE',  ( 0.5782707292762442330, -30.83005644796828904, 35.34464560754155826 ) ) ;
#16391 = CARTESIAN_POINT ( 'NONE',  ( 4.833616638992205949, -20.04871863793778175, -41.67905425467698421 ) ) ;
#16392 = CARTESIAN_POINT ( 'NONE',  ( 0.6000166863083090663, -48.77118664543507975, -5.761495891223787247 ) ) ;
#16393 = FACE_OUTER_BOUND ( 'NONE', #16603, .T. ) ;
#16394 = EDGE_CURVE ( 'NONE', #7929, #40951, #24946, .T. ) ;
#16395 = CARTESIAN_POINT ( 'NONE',  ( 0.7245667037590742821, 5.464144792999380940, -47.79072416626839725 ) ) ;
#16396 = CARTESIAN_POINT ( 'NONE',  ( 0.5782707292762423457, -34.29472224813918757, 31.99388034656949031 ) ) ;
#16397 = CIRCLE ( 'NONE', #29405, 48.09070567114147110 ) ;
#16398 = CARTESIAN_POINT ( 'NONE',  ( 0.5830082357119548142, -13.63298622686205874, -44.87063317445529975 ) ) ;
#16399 = CARTESIAN_POINT ( 'NONE',  ( 4.975801465491694664, 21.70134120755201224, -42.71626295676241369 ) ) ;
#16400 = CONTEXT_DEPENDENT_SHAPE_REPRESENTATION ( #28381, #53345 ) ;
#16402 = EDGE_CURVE ( 'NONE', #21513, #437, #25786, .T. ) ;
#16401 = CARTESIAN_POINT ( 'NONE',  ( 4.975801465491694664, -36.39623109580487892, 31.15993731089061924 ) ) ;
#16403 = CARTESIAN_POINT ( 'NONE',  ( 0.5980271706414711508, 11.60998973146016766, -47.72061798926175413 ) ) ;
#16404 = ADVANCED_FACE ( 'NONE', ( #7911 ), #27187, .F. ) ;
#16405 = CARTESIAN_POINT ( 'NONE',  ( 0.5848930533535030563, 46.50190038545807880, 6.070118856208002178 ) ) ;
#16406 = CARTESIAN_POINT ( 'NONE',  ( 0.6026112563231247332, 48.16826574472209899, 9.558199100774150025 ) ) ;
#16407 = EDGE_CURVE ( 'NONE', #15433, #35962, #42935, .T. ) ;
#16409 = VERTEX_POINT ( 'NONE', #50207 ) ;
#16408 = CARTESIAN_POINT ( 'NONE',  ( 4.962356264823609031, 37.75702904547822669, -18.59145920903629090 ) ) ;
#16410 = ORIENTED_EDGE ( 'NONE', *, *, #47959, .F. ) ;
#16411 = FACE_BOUND ( 'NONE', #49120, .T. ) ;
#16412 = CARTESIAN_POINT ( 'NONE',  ( 0.1064266418746774023, 30.88821921809848092, -30.09411284098539952 ) ) ;
#16413 = EDGE_CURVE ( 'NONE', #21601, #35431, #11226, .T. ) ;
#16414 = DIRECTION ( 'NONE',  ( 1.000000000000000000, 0.000000000000000000, 0.000000000000000000 ) ) ;
#16415 = ORIENTED_EDGE ( 'NONE', *, *, #37814, .T. ) ;
#16416 = ORIENTED_EDGE ( 'NONE', *, *, #5497, .F. ) ;
#16417 = CARTESIAN_POINT ( 'NONE',  ( 4.553261556744875094, -29.69864478935419072, 32.36556910513705532 ) ) ;
#16418 = CARTESIAN_POINT ( 'NONE',  ( 4.335381028904216727, 8.818319717467909769, -48.18707383754342999 ) ) ;
#16419 = CARTESIAN_POINT ( 'NONE',  ( 0.1100247026804066219, -37.43141430507386502, 21.41511734445733595 ) ) ;
#16420 = ORIENTED_EDGE ( 'NONE', *, *, #51367, .T. ) ;
#16421 = ORIENTED_EDGE ( 'NONE', *, *, #6746, .T. ) ;
#16422 = ADVANCED_FACE ( 'NONE', ( #17322 ), #7271, .F. ) ;
#16423 = CARTESIAN_POINT ( 'NONE',  ( 0.6009453534118440743, -23.67490308139376509, -41.87889766923446189 ) ) ;
#16424 = CARTESIAN_POINT ( 'NONE',  ( 1.227938101723756947, -4.762198645644731165, 42.65467462194916948 ) ) ;
#16425 = CARTESIAN_POINT ( 'NONE',  ( 0.7764146366350200834, 17.68681966478046874, 43.44210956911165766 ) ) ;
#16426 = ORIENTED_EDGE ( 'NONE', *, *, #20926, .T. ) ;
#16427 = LINE ( 'NONE', #20514, #33067 ) ;
#16428 = CARTESIAN_POINT ( 'NONE',  ( 2.618530812446111078, -44.84885430744879642, 14.08215383055557446 ) ) ;
#16429 = CARTESIAN_POINT ( 'NONE',  ( 0.9730545539215883499, 42.47233286818616449, 6.101350888304794218 ) ) ;
#16430 = ORIENTED_EDGE ( 'NONE', *, *, #43234, .F. ) ;
#16431 = ORIENTED_EDGE ( 'NONE', *, *, #35461, .F. ) ;
#16432 = CARTESIAN_POINT ( 'NONE',  ( 0.3676999524040323597, 43.44964275340426951, -7.620966337964178550 ) ) ;
#16433 = CARTESIAN_POINT ( 'NONE',  ( 5.880360259849752858, 26.61251048557193499, 39.91356965504157017 ) ) ;
#16434 = ORIENTED_EDGE ( 'NONE', *, *, #32514, .T. ) ;
#16435 = DIRECTION ( 'NONE',  ( -1.000000000000000000, -0.000000000000000000, -0.000000000000000000 ) ) ;
#16436 = CARTESIAN_POINT ( 'NONE',  ( 0.8560838555295158248, 3.785103201470073397, 46.75516899590838449 ) ) ;
#16437 = CARTESIAN_POINT ( 'NONE',  ( 4.999999999999997335, 0.000000000000000000, 0.000000000000000000 ) ) ;
#16438 = CARTESIAN_POINT ( 'NONE',  ( 0.5827357941260201679, 12.04516435546866937, -46.35666768646123614 ) ) ;
#16439 = ADVANCED_FACE ( 'NONE', ( #45531 ), #59596, .T. ) ;
#16440 = ORIENTED_EDGE ( 'NONE', *, *, #37798, .F. ) ;
#16441 = DIRECTION ( 'NONE',  ( 0.000000000000000000, 0.000000000000000000, 1.000000000000000000 ) ) ;
#16442 = CARTESIAN_POINT ( 'NONE',  ( 0.6028777368367060907, -35.33680725117163490, 34.10058478390973136 ) ) ;
#16443 = EDGE_CURVE ( 'NONE', #47692, #44331, #35514, .T. ) ;
#16444 = DIRECTION ( 'NONE',  ( 0.1011922191286467876, -0.9655114622251689260, -0.2398911234281835836 ) ) ;
#16445 = AXIS2_PLACEMENT_3D ( 'NONE', #12298, #21676, #59883 ) ;
#16446 = ORIENTED_EDGE ( 'NONE', *, *, #14014, .T. ) ;
#16447 = LINE ( 'NONE', #6700, #47546 ) ;
#16448 = CARTESIAN_POINT ( 'NONE',  ( 0.5797568665920710407, 5.319645520859431542, 46.59320422694997887 ) ) ;
#16449 = VERTEX_POINT ( 'NONE', #26093 ) ;
#16450 = DIRECTION ( 'NONE',  ( 0.000000000000000000, 0.000000000000000000, 1.000000000000000000 ) ) ;
#16451 =( NAMED_UNIT ( * ) PLANE_ANGLE_UNIT ( ) SI_UNIT ( $, .RADIAN. ) );
#16452 = ORIENTED_EDGE ( 'NONE', *, *, #11252, .T. ) ;
#16453 = CARTESIAN_POINT ( 'NONE',  ( 0.6845945791218034371, 37.34424629630233028, -28.38685944719937027 ) ) ;
#16454 = PRODUCT_DEFINITION ( 'UNKNOWN', '', #55895, #34227 ) ;
#16455 = CARTESIAN_POINT ( 'NONE',  ( 0.2940133293163015304, -42.46217173550956403, -11.96680914371648896 ) ) ;
#16456 = CONICAL_SURFACE ( 'NONE', #47496, 43.12527911185304674, 0.04450589592585017101 ) ;
#16457 = B_SPLINE_CURVE_WITH_KNOTS ( 'NONE', 3,
 ( #3777, #32011, #3168, #41426 ),
 .UNSPECIFIED., .F., .F.,
 ( 4, 4 ),
 ( 1.854207614396248247E-17, 0.004444306975806115896 ),
 .UNSPECIFIED. ) ;
#16458 = CARTESIAN_POINT ( 'NONE',  ( 0.5997462898726536595, -14.47257175146244457, -46.92649887902442885 ) ) ;
#16459 = CARTESIAN_POINT ( 'NONE',  ( 0.000000000000000000, 0.000000000000000000, 0.000000000000000000 ) ) ;
#16460 = CARTESIAN_POINT ( 'NONE',  ( 0.5827357941260221663, 46.16863402900295910, -12.74691551863582717 ) ) ;
#16461 = CARTESIAN_POINT ( 'NONE',  ( 0.5809828226811553087, -47.55412398569202281, -5.711058609465819558 ) ) ;
#16462 = CARTESIAN_POINT ( 'NONE',  ( 0.1095718737110178143, -41.58781525899402709, -11.40943879390634308 ) ) ;
#16463 = CARTESIAN_POINT ( 'NONE',  ( 4.975610109902397937, -48.11736577406850301, -8.784561349451310619 ) ) ;
#16464 = CARTESIAN_POINT ( 'NONE',  ( -6.077587904424778920, -4.290907484552072049, -18.77189746277518623 ) ) ;
#16465 =( BOUNDED_SURFACE ( )  B_SPLINE_SURFACE ( 3, 1, ( 
 ( #58, #52072 ),
 ( #15114, #19208 ),
 ( #38623, #14504 ),
 ( #33305, #5059 ) ),
 .UNSPECIFIED., .F., .F., .F. ) 
 B_SPLINE_SURFACE_WITH_KNOTS ( ( 4, 4 ),
 ( 2, 2 ),
 ( 0.000000000000000000, 1.000000000000000000 ),
 ( 0.000000000000000000, 1.000000000000000000 ),
 .UNSPECIFIED. ) 
 GEOMETRIC_REPRESENTATION_ITEM ( )  RATIONAL_B_SPLINE_SURFACE ( (
 ( 1.000000000000000000, 1.000000000000000000),
 ( 0.9953485035131437453, 0.8621029689291523912),
 ( 0.9953485035131437453, 0.8621029689291523912),
 ( 1.000000000000000000, 1.000000000000000000) ) ) 
 REPRESENTATION_ITEM ( '' )  SURFACE ( )  );
#16466 = CARTESIAN_POINT ( 'NONE',  ( 0.5837799406558231707, 27.74442806126372929, -37.80860035931723928 ) ) ;
#16467 = ORIENTED_EDGE ( 'NONE', *, *, #60018, .T. ) ;
#16468 = CARTESIAN_POINT ( 'NONE',  ( -15.88737024819575439, -12.49768255930560024, -0.2758842803416746703 ) ) ;
#16469 = CARTESIAN_POINT ( 'NONE',  ( 4.694002226626920127, 7.615834493546986828, 44.94756763622514484 ) ) ;
#16470 = CARTESIAN_POINT ( 'NONE',  ( 4.975610109902397937, -43.81605102859474954, 21.73943604138237973 ) ) ;
#16471 = CARTESIAN_POINT ( 'NONE',  ( 0.1158516988532803799, 44.03032832662167806, -2.876168681196155319 ) ) ;
#16472 = CARTESIAN_POINT ( 'NONE',  ( 0.7245667037590702853, -28.62745028382845902, 38.65590879674336122 ) ) ;
#16473 = CARTESIAN_POINT ( 'NONE',  ( 5.910764540655177868, 5.973554503640923663, -19.20463186476622397 ) ) ;
#16474 = CARTESIAN_POINT ( 'NONE',  ( 14.99999999999999289, 56.56854249492396036, -56.56854249492366193 ) ) ;
#16476 = EDGE_CURVE ( 'NONE', #49170, #45083, #11519, .T. ) ;
#16475 = CARTESIAN_POINT ( 'NONE',  ( 0.3676999524040323597, -13.34038000160386339, 42.04741186726771929 ) ) ;
#16477 = AXIS2_PLACEMENT_3D ( 'NONE', #59149, #9458, #30644 ) ;
#16478 = CARTESIAN_POINT ( 'NONE',  ( 0.6027935024548038978, 41.74929432965617337, -23.90242449907770350 ) ) ;
#16479 = EDGE_CURVE ( 'NONE', #41130, #7712, #22723, .T. ) ;
#16480 = DIRECTION ( 'NONE',  ( 0.000000000000000000, 0.000000000000000000, 1.000000000000000000 ) ) ;
#16481 = EDGE_CURVE ( 'NONE', #47629, #51544, #57089, .T. ) ;
#16483 = ORIENTED_EDGE ( 'NONE', *, *, #25181, .T. ) ;
#16482 = CARTESIAN_POINT ( 'NONE',  ( 4.291220156522060236, 44.16776250362654821, 16.38895215469672095 ) ) ;
#16484 = ORIENTED_EDGE ( 'NONE', *, *, #20595, .F. ) ;
#16485 = CARTESIAN_POINT ( 'NONE',  ( 0.2224561200757598778, -34.66601556960367247, 25.64288022150822499 ) ) ;
#16486 = CARTESIAN_POINT ( 'NONE',  ( 0.8560838555295223751, -24.46533024579953164, 40.02274915651970133 ) ) ;
#16487 = ADVANCED_FACE ( 'NONE', ( #39921 ), #49138, .F. ) ;
#16488 = DIRECTION ( 'NONE',  ( -1.000000000000000000, -0.000000000000000000, -0.000000000000000000 ) ) ;
#16489 =( BOUNDED_SURFACE ( )  B_SPLINE_SURFACE ( 3, 1, ( 
 ( #46065, #3107 ),
 ( #22238, #17534 ),
 ( #14083, #4019 ),
 ( #33186, #37905 ) ),
 .UNSPECIFIED., .F., .F., .F. ) 
 B_SPLINE_SURFACE_WITH_KNOTS ( ( 4, 4 ),
 ( 2, 2 ),
 ( 0.000000000000000000, 1.000000000000000000 ),
 ( 0.000000000000000000, 1.000000000000000000 ),
 .UNSPECIFIED. ) 
 GEOMETRIC_REPRESENTATION_ITEM ( )  RATIONAL_B_SPLINE_SURFACE ( (
 ( 1.000000000000000000, 1.000000000000000000),
 ( 0.9953485035131437453, 0.8621029689291515030),
 ( 0.9953485035131437453, 0.8621029689291515030),
 ( 1.000000000000000000, 1.000000000000000000) ) ) 
 REPRESENTATION_ITEM ( '' )  SURFACE ( )  );
#16490 = ORIENTED_EDGE ( 'NONE', *, *, #10807, .T. ) ;
#16491 = CARTESIAN_POINT ( 'NONE',  ( 1.830465331921978134, 44.02103255007548199, -1.588945909584584593 ) ) ;
#16492 = CARTESIAN_POINT ( 'NONE',  ( 0.5838002273316433843, -47.50378804015149115, 6.116619957188576429 ) ) ;
#16493 = FACE_OUTER_BOUND ( 'NONE', #10429, .T. ) ;
#16494 = VERTEX_POINT ( 'NONE', #46769 ) ;
#16495 = ORIENTED_EDGE ( 'NONE', *, *, #17908, .F. ) ;
#16496 = AXIS2_PLACEMENT_3D ( 'NONE', #38904, #23850, #32959 ) ;
#16497 = CARTESIAN_POINT ( 'NONE',  ( 0.5980894510889448457, -17.76188940524917115, -44.71414919659899567 ) ) ;
#16498 = EDGE_CURVE ( 'NONE', #35841, #18005, #48249, .T. ) ;
#16500 = CARTESIAN_POINT ( 'NONE',  ( 0.6039202388192953519, 48.16848798300492263, -9.558267535495215128 ) ) ;
#16499 = AXIS2_PLACEMENT_3D ( 'NONE', #49849, #55149, #44871 ) ;
#16501 = CARTESIAN_POINT ( 'NONE',  ( 3.376099380956838925, 10.79965495504299433, -7.942029745857318801 ) ) ;
#16502 = VERTEX_POINT ( 'NONE', #23550 ) ;
#16503 = CIRCLE ( 'NONE', #25522, 43.92652462719577500 ) ;
#16504 = ORIENTED_EDGE ( 'NONE', *, *, #52381, .F. ) ;
#16505 = CARTESIAN_POINT ( 'NONE',  ( 0.3622758884714730732, 36.91764744403321430, -22.26738722580129348 ) ) ;
#16506 = CARTESIAN_POINT ( 'NONE',  ( 0.5848930533535030563, -25.38746244141833230, 39.43031616882030477 ) ) ;
#16507 = ORIENTED_EDGE ( 'NONE', *, *, #45361, .F. ) ;
#16508 = CARTESIAN_POINT ( 'NONE',  ( 0.5809828226811617480, 34.25055090842200656, -33.48000389720580472 ) ) ;
#16509 = DIRECTION ( 'NONE',  ( 0.000000000000000000, 0.000000000000000000, 1.000000000000000000 ) ) ;
#16510 = EDGE_LOOP ( 'NONE', ( #55816, #51558, #11656, #21112 ) ) ;
#16511 = CARTESIAN_POINT ( 'NONE',  ( 0.2111111111111110827, -9.497654031326126400, -1.199999999999999956 ) ) ;
#16512 = CARTESIAN_POINT ( 'NONE',  ( 4.960386119450149955, 13.41207489487474724, -41.64796167505215863 ) ) ;
#16513 = ORIENTED_EDGE ( 'NONE', *, *, #15280, .F. ) ;
#16514 = DIRECTION ( 'NONE',  ( 0.000000000000000000, 0.7071067811865395791, 0.7071067811865553443 ) ) ;
#16515 = CARTESIAN_POINT ( 'NONE',  ( 0.5817216825391118284, -19.32621644266162519, 42.72858890975519586 ) ) ;
#16516 = DIRECTION ( 'NONE',  ( -0.07906939808003035641, 0.2389416749771256232, 0.9678093336222726162 ) ) ;
#16517 = CARTESIAN_POINT ( 'NONE',  ( -6.063463321072276813, 16.78636876910481845, 9.436009539370578736 ) ) ;
#16518 = ORIENTED_EDGE ( 'NONE', *, *, #9612, .F. ) ;
#16519 = CARTESIAN_POINT ( 'NONE',  ( 0.7056555295713285991, -33.27140645154220522, 34.46100226633724617 ) ) ;
#16520 = CARTESIAN_POINT ( 'NONE',  ( 0.1129192098497447394, 39.54191224844646513, -19.58032082273713570 ) ) ;
#16521 = EDGE_LOOP ( 'NONE', ( #29108, #33495, #39431, #47266 ) ) ;
#16522 = CARTESIAN_POINT ( 'NONE',  ( 4.553261556744875094, 0.000000000000000000, 0.000000000000000000 ) ) ;
#16523 = CIRCLE ( 'NONE', #9489, 48.09070567114147110 ) ;
#16524 = EDGE_CURVE ( 'NONE', #4627, #41301, #16735, .T. ) ;
#16525 = VERTEX_POINT ( 'NONE', #22635 ) ;
#16526 = CARTESIAN_POINT ( 'NONE',  ( 0.5809828226811565299, -17.82437196699712700, 44.45562576850595349 ) ) ;
#16527 = ORIENTED_EDGE ( 'NONE', *, *, #7992, .T. ) ;
#16528 = FACE_OUTER_BOUND ( 'NONE', #13199, .T. ) ;
#16529 = CARTESIAN_POINT ( 'NONE',  ( 0.5809828226811553087, -47.55412398569202281, -5.711058609465819558 ) ) ;
#16530 = CARTESIAN_POINT ( 'NONE',  ( 4.549368137175248350, 35.57418903283115696, -24.02461520945233531 ) ) ;
#16531 = ORIENTED_EDGE ( 'NONE', *, *, #17196, .T. ) ;
#16532 = CARTESIAN_POINT ( 'NONE',  ( 0.1157506346131639274, 43.32810245082073664, 8.343632171543594822 ) ) ;
#16533 = FACE_OUTER_BOUND ( 'NONE', #38889, .T. ) ;
#16534 = CARTESIAN_POINT ( 'NONE',  ( 0.1073791018717483448, 10.69234304550053949, -41.77800844988504991 ) ) ;
#16535 = ORIENTED_EDGE ( 'NONE', *, *, #7696, .F. ) ;
#16536 = B_SPLINE_CURVE_WITH_KNOTS ( 'NONE', 3,
 ( #57186, #5187, #24319, #19635, #38753, #5491 ),
 .UNSPECIFIED., .F., .F.,
 ( 4, 2, 4 ),
 ( 1.870559545977334001E-17, 0.0002293319059085096288, 0.0004586638118170005551 ),
 .UNSPECIFIED. ) ;
#16537 = ORIENTED_EDGE ( 'NONE', *, *, #6004, .F. ) ;
#16538 = DIRECTION ( 'NONE',  ( 0.000000000000000000, 0.7071067811865421326, 0.7071067811865527908 ) ) ;
#16539 = CARTESIAN_POINT ( 'NONE',  ( 3.050102900204245682, 30.89180545305748993, 31.32286074145379473 ) ) ;
#16540 = CARTESIAN_POINT ( 'NONE',  ( 0.9787464366903561030, 38.65195219007281935, -16.19754872771774501 ) ) ;
#16541 = CARTESIAN_POINT ( 'NONE',  ( 3.270143674763207553, 10.69018354892899403, -8.548517033725143932 ) ) ;
#16542 = CARTESIAN_POINT ( 'NONE',  ( 0.5837799406558220605, -30.34692608210707121, -35.75342818450186400 ) ) ;
#16544 = VECTOR ( 'NONE', #23370, 1000.000000000000114 ) ;
#16543 = LINE ( 'NONE', #49742, #52771 ) ;
#16545 = ORIENTED_EDGE ( 'NONE', *, *, #4438, .F. ) ;
#16546 = CARTESIAN_POINT ( 'NONE',  ( 0.5800708057587363742, -23.40241940841928781, -41.78924035064549969 ) ) ;
#16547 = CARTESIAN_POINT ( 'NONE',  ( 4.975801465491695552, -20.67815041659169495, 43.22084481528186473 ) ) ;
#16548 = ORIENTED_EDGE ( 'NONE', *, *, #16402, .T. ) ;
#16549 = VECTOR ( 'NONE', #39804, 1000.000000000000114 ) ;
#16550 = CARTESIAN_POINT ( 'NONE',  ( 4.975610109902397937, 42.33317580307156192, -24.50207406657668230 ) ) ;
#16551 = CARTESIAN_POINT ( 'NONE',  ( 0.5326698147273788431, 0.000000000000000000, -41.88877248453276536 ) ) ;
#16552 = CARTESIAN_POINT ( 'NONE',  ( 0.5997462898726536595, 44.46857747280011353, 20.83500054451363326 ) ) ;
#16553 = VECTOR ( 'NONE', #28622, 1000.000000000000000 ) ;
#16554 = CARTESIAN_POINT ( 'NONE',  ( 5.959547316686252039, -10.25972575517542396, 17.77749189599199653 ) ) ;
#16555 = CARTESIAN_POINT ( 'NONE',  ( 0.3676999524040323597, 24.55639947020961600, 36.64606156713607277 ) ) ;
#16556 = CARTESIAN_POINT ( 'NONE',  ( 0.8560838555295158248, 37.37287335782446718, -28.34856559090329142 ) ) ;
#16557 = CARTESIAN_POINT ( 'NONE',  ( 0.1156495703730067576, -12.68516895305341308, -42.26144154975737877 ) ) ;
#16558 = CARTESIAN_POINT ( 'NONE',  ( 5.439999999999997726, 15.43999999999999950, 0.000000000000000000 ) ) ;
#16559 = CARTESIAN_POINT ( 'NONE',  ( 0.1365634738349441879, 30.13243411101788993, -32.23195672261324773 ) ) ;
#16560 = EDGE_CURVE ( 'NONE', #694, #2809, #21238, .T. ) ;
#16561 = LINE ( 'NONE', #55368, #30849 ) ;
#16562 = CARTESIAN_POINT ( 'NONE',  ( 4.549368137175248350, 0.000000000000000000, 0.000000000000000000 ) ) ;
#16563 = CARTESIAN_POINT ( 'NONE',  ( 5.910764540655178756, 3.329973395294576477, -19.83462920388967987 ) ) ;
#16564 = EDGE_CURVE ( 'NONE', #16052, #19210, #30134, .T. ) ;
#16565 = CARTESIAN_POINT ( 'NONE',  ( 0.1129192098497447394, -17.41650932123218354, 40.54154647825593827 ) ) ;
#16566 = B_SPLINE_CURVE_WITH_KNOTS ( 'NONE', 3,
 ( #59858, #16976, #26974, #30416 ),
 .UNSPECIFIED., .F., .F.,
 ( 4, 4 ),
 ( 0.000000000000000000, 0.004442905043737217438 ),
 .UNSPECIFIED. ) ;
#16567 = CARTESIAN_POINT ( 'NONE',  ( -6.016489644550736315, -18.68142234211826036, 2.463898142942696268 ) ) ;
#16568 = CARTESIAN_POINT ( 'NONE',  ( 0.3622758884714600280, -17.25816669465019615, 39.50828911766968332 ) ) ;
#16569 =( BOUNDED_SURFACE ( )  B_SPLINE_SURFACE ( 3, 1, ( 
 ( #3796, #51408 ),
 ( #47062, #23851 ),
 ( #25, #4098 ),
 ( #46751, #22937 ) ),
 .UNSPECIFIED., .F., .F., .F. ) 
 B_SPLINE_SURFACE_WITH_KNOTS ( ( 4, 4 ),
 ( 2, 2 ),
 ( 0.000000000000000000, 1.000000000000000000 ),
 ( 0.000000000000000000, 1.000000000000000000 ),
 .UNSPECIFIED. ) 
 GEOMETRIC_REPRESENTATION_ITEM ( )  RATIONAL_B_SPLINE_SURFACE ( (
 ( 1.000000000000000000, 1.000000000000000000),
 ( 0.9953390228620291325, 0.8624445117761032620),
 ( 0.9953390228620291325, 0.8624445117761032620),
 ( 1.000000000000000000, 1.000000000000000000) ) ) 
 REPRESENTATION_ITEM ( '' )  SURFACE ( )  );
#16570 = ORIENTED_EDGE ( 'NONE', *, *, #774, .T. ) ;
#16571 = CARTESIAN_POINT ( 'NONE',  ( 0.1084644655670281843, 10.77688306151803666, -41.75632203164222034 ) ) ;
#16572 = EDGE_CURVE ( 'NONE', #19565, #26674, #28710, .T. ) ;
#16573 = FACE_BOUND ( 'NONE', #15605, .T. ) ;
#16574 = CARTESIAN_POINT ( 'NONE',  ( 0.9757892942422820015, -26.16173342773518584, -34.01031843153919709 ) ) ;
#16575 = LINE ( 'NONE', #46034, #32246 ) ;
#16576 = CARTESIAN_POINT ( 'NONE',  ( 0.5804410086790514622, 46.55025363952961470, 5.709092568075557317 ) ) ;
#16577 = ORIENTED_EDGE ( 'NONE', *, *, #27745, .T. ) ;
#16578 = ADVANCED_FACE ( 'NONE', ( #28251 ), #23251, .F. ) ;
#16579 = CARTESIAN_POINT ( 'NONE',  ( 0.8557997880470599172, -29.88293891557496096, 37.44587306708088192 ) ) ;
#16580 = CARTESIAN_POINT ( 'NONE',  ( 0.6029443449137436017, 28.13086200025576389, -40.25163526002264547 ) ) ;
#16581 = B_SPLINE_CURVE_WITH_KNOTS ( 'NONE', 3,
 ( #20701, #29783, #39841, #6559, #11005, #58894, #40449, #30703, #49819, #1883, #35126, #16012, #58575, #16623, #11301, #30389, #54184, #59512, #58266, #1568, #53882, #48894, #5945, #26018, #25084, #2183, #44537, #44230, #15397, #54491, #49506, #15704 ),
 .UNSPECIFIED., .F., .F.,
 ( 4, 2, 2, 2, 2, 2, 2, 2, 2, 2, 2, 2, 2, 2, 2, 4 ),
 ( 0.000000000000000000, 0.0005192934025038106532, 0.001038586805007621306, 0.001557880207511431851, 0.002077173610015242613, 0.003115760415022862835, 0.003635053817526677066, 0.004154347220030491297, 0.004673640622534305095, 0.005192934025038119759, 0.005712227427541933557, 0.006231520830045749089, 0.006750814232549562886, 0.007270107635053377551, 0.007789401037557191348, 0.008308694440061006881 ),
 .UNSPECIFIED. ) ;
#16582 = B_SPLINE_CURVE_WITH_KNOTS ( 'NONE', 3,
 ( #29202, #43028, #53603, #48317 ),
 .UNSPECIFIED., .F., .F.,
 ( 4, 4 ),
 ( 0.000000000000000000, 0.005013413432710148512 ),
 .UNSPECIFIED. ) ;
#16583 = LINE ( 'NONE', #16270, #3503 ) ;
#16584 = ORIENTED_EDGE ( 'NONE', *, *, #37344, .T. ) ;
#16585 = VECTOR ( 'NONE', #42726, 999.9999999999998863 ) ;
#16586 = CARTESIAN_POINT ( 'NONE',  ( -6.072942160501519915, -16.14637491494715960, -10.49279464179992516 ) ) ;
#16587 = ORIENTED_EDGE ( 'NONE', *, *, #40157, .F. ) ;
#16588 = CARTESIAN_POINT ( 'NONE',  ( 0.5997462898726536595, 48.97040376101512749, 3.667585803694950464 ) ) ;
#16589 = CARTESIAN_POINT ( 'NONE',  ( 0.8560838555295158248, -44.60403252362548443, 14.52078223488980768 ) ) ;
#16590 = VECTOR ( 'NONE', #35169, 1000.000000000000114 ) ;
#16591 = VERTEX_POINT ( 'NONE', #27953 ) ;
#16592 = CARTESIAN_POINT ( 'NONE',  ( 0.6039202388192953519, -35.15506827346180785, 34.28826165814228943 ) ) ;
#16593 = ORIENTED_EDGE ( 'NONE', *, *, #50017, .T. ) ;
#16594 = CARTESIAN_POINT ( 'NONE',  ( 4.999999999999997335, 9.184547653667864935E-16, -9.629649721936170507E-32 ) ) ;
#16595 = CARTESIAN_POINT ( 'NONE',  ( 0.1084644655670281566, -26.56696682929032249, -33.96951444491416083 ) ) ;
#16596 = ORIENTED_EDGE ( 'NONE', *, *, #20237, .T. ) ;
#16597 = AXIS2_PLACEMENT_3D ( 'NONE', #7435, #54744, #21875 ) ;
#16598 = ORIENTED_EDGE ( 'NONE', *, *, #49006, .T. ) ;
#16599 = CARTESIAN_POINT ( 'NONE',  ( 4.694002226626921015, 1.805541223688327701, -45.55244002614676191 ) ) ;
#16600 = ORIENTED_EDGE ( 'NONE', *, *, #10181, .F. ) ;
#16601 = CARTESIAN_POINT ( 'NONE',  ( 5.895881250540457863, 16.58446435569129918, -11.37906954206300014 ) ) ;
#16602 = EDGE_CURVE ( 'NONE', #35847, #1029, #46250, .T. ) ;
#16603 = EDGE_LOOP ( 'NONE', ( #25058, #23124, #38492, #40690 ) ) ;
#16604 = ORIENTED_EDGE ( 'NONE', *, *, #53172, .F. ) ;
#16605 = DIRECTION ( 'NONE',  ( 1.000000000000000000, -0.000000000000000000, -0.000000000000000000 ) ) ;
#16607 = CIRCLE ( 'NONE', #48604, 48.91267123290010943 ) ;
#16606 = CARTESIAN_POINT ( 'NONE',  ( -6.078457390727109555, -16.13585499094672926, 10.50850582854895698 ) ) ;
#16608 = CARTESIAN_POINT ( 'NONE',  ( 4.956653778116975495, 15.97476558431885252, 45.35992544608534160 ) ) ;
#16609 = B_SPLINE_CURVE_WITH_KNOTS ( 'NONE', 3,
 ( #13930, #28005, #13299, #8572, #60571, #26767 ),
 .UNSPECIFIED., .F., .F.,
 ( 4, 2, 4 ),
 ( 2.032850612904068153E-17, 0.0002293319059085113093, 0.0004586638118170022899 ),
 .UNSPECIFIED. ) ;
#16610 = CARTESIAN_POINT ( 'NONE',  ( 0.7764139734771235979, -34.18255399381159521, -32.11842887451099671 ) ) ;
#16611 = DIRECTION ( 'NONE',  ( 1.000000000000000000, 0.000000000000000000, 0.000000000000000000 ) ) ;
#16612 = ORIENTED_EDGE ( 'NONE', *, *, #51244, .T. ) ;
#16613 = FACE_OUTER_BOUND ( 'NONE', #31810, .T. ) ;
#16614 = CARTESIAN_POINT ( 'NONE',  ( -6.063463321072278589, 19.09660126457254492, 2.477957348582926045 ) ) ;
#16615 = ORIENTED_EDGE ( 'NONE', *, *, #4088, .F. ) ;
#16616 = ORIENTED_EDGE ( 'NONE', *, *, #35747, .F. ) ;
#16617 = CARTESIAN_POINT ( 'NONE',  ( 0.6001305935487422083, -48.10757715638248300, -0.5236757026887532973 ) ) ;
#16618 = LINE ( 'NONE', #55423, #56761 ) ;
#16619 = CARTESIAN_POINT ( 'NONE',  ( 0.5830082357119569236, -44.39002986412761231, 15.12472424873239518 ) ) ;
#16620 = ORIENTED_EDGE ( 'NONE', *, *, #23807, .F. ) ;
#16621 = CARTESIAN_POINT ( 'NONE',  ( 0.1101816497532063094, -42.77304337559939285, -5.494186916735566584 ) ) ;
#16622 = CARTESIAN_POINT ( 'NONE',  ( 0.5998501479064699549, 37.84527566984857572, -29.69975237324574024 ) ) ;
#16623 = CARTESIAN_POINT ( 'NONE',  ( 53.13300907242233251, 12.49636441417896116, -0.3467375140025887870 ) ) ;
#16624 = CARTESIAN_POINT ( 'NONE',  ( -20.07361639412344800, -12.49998595421523184, -0.1399944396052446860 ) ) ;
#16625 = ORIENTED_EDGE ( 'NONE', *, *, #23256, .T. ) ;
#16626 = CARTESIAN_POINT ( 'NONE',  ( 1.231276596079887264, 40.19859528295904738, -11.88905834349085922 ) ) ;
#16627 = ORIENTED_EDGE ( 'NONE', *, *, #17116, .T. ) ;
#16628 = FACE_OUTER_BOUND ( 'NONE', #20067, .T. ) ;
#16629 = CARTESIAN_POINT ( 'NONE',  ( 0.8744876279028306332, -26.20733431478126008, -41.51536677536140729 ) ) ;
#16630 = SURFACE_SIDE_STYLE ('',( #25399 ) ) ;
#16631 = CARTESIAN_POINT ( 'NONE',  ( 0.7044674535452954967, 46.33602660604208978, 16.27191940660552660 ) ) ;
#16632 = ORIENTED_EDGE ( 'NONE', *, *, #29359, .T. ) ;
#16633 = CARTESIAN_POINT ( 'NONE',  ( 1.231276596079887264, 10.53918392497828727, 40.57341954055075917 ) ) ;
#16634 = CARTESIAN_POINT ( 'NONE',  ( 4.975801465491695552, 45.18341283946458020, -15.94009207553003016 ) ) ;
#16635 = ADVANCED_FACE ( 'NONE', ( #42379 ), #56745, .F. ) ;
#16636 = CARTESIAN_POINT ( 'NONE',  ( 0.5786265663353196143, 6.967625775956395984, -47.39171391660384813 ) ) ;
#16637 = CARTESIAN_POINT ( 'NONE',  ( 0.5980271706414711508, 23.33483692714806068, -43.21498152753358823 ) ) ;
#16638 = CIRCLE ( 'NONE', #25653, 43.92652462719577500 ) ;
#16639 = CONICAL_SURFACE ( 'NONE', #33688, 48.91267123290010943, 0.04450589592585339760 ) ;
#16640 = CARTESIAN_POINT ( 'NONE',  ( 0.9747592971366223491, 36.99691261380240803, -21.73404615330581890 ) ) ;
#16641 = ADVANCED_FACE ( 'NONE', ( #33284 ), #13551, .F. ) ;
#16642 = CARTESIAN_POINT ( 'NONE',  ( 0.5837800304671216800, 32.56903879203510854, 33.74159220224218103 ) ) ;
#16643 = CARTESIAN_POINT ( 'NONE',  ( 0.5980894510889457338, -23.44630161211615871, 42.01322166096878874 ) ) ;
#16644 = CARTESIAN_POINT ( 'NONE',  ( 4.335381028904216727, 6.815065961880201861, 48.51094436928195819 ) ) ;
#16645 = CARTESIAN_POINT ( 'NONE',  ( 4.960386119450149955, 35.80440191905969272, 25.14918026279933017 ) ) ;
#16646 = EDGE_CURVE ( 'NONE', #22519, #12427, #33159, .T. ) ;
#16647 = CARTESIAN_POINT ( 'NONE',  ( 4.956445790443989807, 46.03642002599014660, 9.908889005849758291 ) ) ;
#16648 = CARTESIAN_POINT ( 'NONE',  ( 0.6029443449137436017, -45.53481268790790182, 18.38804969159247449 ) ) ;
#16649 = CIRCLE ( 'NONE', #14650, 42.08604991992415023 ) ;
#16650 = ORIENTED_EDGE ( 'NONE', *, *, #52862, .F. ) ;
#16651 = CARTESIAN_POINT ( 'NONE',  ( 3.050102900204245682, -3.218072654074529027, -43.87561119313505031 ) ) ;
#16652 = CARTESIAN_POINT ( 'NONE',  ( 0.6846871229502899947, 43.92355552798064622, -19.12907057981156811 ) ) ;
#16653 = CARTESIAN_POINT ( 'NONE',  ( 3.894904216938898323, -41.89961406944992461, 13.28708671257003537 ) ) ;
#16654 = ORIENTED_EDGE ( 'NONE', *, *, #40618, .T. ) ;
#16655 = EDGE_CURVE ( 'NONE', #10433, #49383, #18970, .T. ) ;
#16656 = CARTESIAN_POINT ( 'NONE',  ( 4.549368137175248350, 42.84816078363926550, 2.596185425822091553 ) ) ;
#16657 = FACE_BOUND ( 'NONE', #53248, .T. ) ;
#16658 = LINE ( 'NONE', #30736, #45713 ) ;
#16659 = B_SPLINE_CURVE_WITH_KNOTS ( 'NONE', 3,
 ( #26760, #12999, #3550, #8256, #18306, #22684, #17370, #31782, #59961, #60879, #27691, #12373, #37415, #36804, #50558, #37114 ),
 .UNSPECIFIED., .F., .F.,
 ( 4, 3, 3, 3, 3, 4 ),
 ( 1.962735358247464152E-17, 0.0002618515315864422478, 0.0003927756766341962565, 0.0005236998216950601668, 0.0007855159896329882725, 0.001047349442285927870 ),
 .UNSPECIFIED. ) ;
#16660 = VERTEX_POINT ( 'NONE', #50557 ) ;
#16661 = CARTESIAN_POINT ( 'NONE',  ( 1.827326673878742813, 37.88339879236860952, -20.44853789448414361 ) ) ;
#16662 = CARTESIAN_POINT ( 'NONE',  ( 0.9747592971366237924, -41.52905920980975907, -10.79247637456163034 ) ) ;
#16663 = ORIENTED_EDGE ( 'NONE', *, *, #35823, .F. ) ;
#16664 = CARTESIAN_POINT ( 'NONE',  ( 0.6029443199889047422, 10.92745038804929791, 47.87617852200740742 ) ) ;
#16665 = ORIENTED_EDGE ( 'NONE', *, *, #26186, .F. ) ;
#16666 = ORIENTED_EDGE ( 'NONE', *, *, #13606, .T. ) ;
#16667 = CARTESIAN_POINT ( 'NONE',  ( 0.9730545539215883499, -26.52009130076748278, -33.73144377768585400 ) ) ;
#16668 = ORIENTED_EDGE ( 'NONE', *, *, #28591, .F. ) ;
#16669 = CARTESIAN_POINT ( 'NONE',  ( -6.078726893082806448, 19.25601281685051802, -0.003415553934477524867 ) ) ;
#16670 = VERTEX_POINT ( 'NONE', #26759 ) ;
#16671 = CARTESIAN_POINT ( 'NONE',  ( 0.9762797500689124330, -22.12212327108638377, 35.59405072711678741 ) ) ;
#16672 = CARTESIAN_POINT ( 'NONE',  ( 1.154321485836934169, 39.95809831208277529, 15.65787964449878444 ) ) ;
#16673 = VECTOR ( 'NONE', #15860, 1000.000000000000114 ) ;
#16674 = ORIENTED_EDGE ( 'NONE', *, *, #38884, .T. ) ;
#16675 = CARTESIAN_POINT ( 'NONE',  ( 0.1158816050234198897, 15.24427584951536296, 41.40717444029529304 ) ) ;
#16676 = CARTESIAN_POINT ( 'NONE',  ( 3.240649175237395152, -30.30232522355354874, -31.89097056289822518 ) ) ;
#16677 = CARTESIAN_POINT ( 'NONE',  ( 0.1103310638050662151, -30.55179781598017641, 30.43528225250887331 ) ) ;
#16678 = CIRCLE ( 'NONE', #28701, 48.09070567114147110 ) ;
#16679 = CARTESIAN_POINT ( 'NONE',  ( 0.5988103564986354543, 13.03604522143292854, 46.30780741915673104 ) ) ;
#16680 = ORIENTED_EDGE ( 'NONE', *, *, #19278, .F. ) ;
#16681 = EDGE_CURVE ( 'NONE', #53909, #31128, #3860, .T. ) ;
#16683 = ORIENTED_EDGE ( 'NONE', *, *, #44099, .T. ) ;
#16682 = B_SPLINE_CURVE_WITH_KNOTS ( 'NONE', 3,
 ( #12118, #40630, #36537, #3287 ),
 .UNSPECIFIED., .F., .F.,
 ( 4, 4 ),
 ( 2.168404344971008868E-19, 0.004048833967417086489 ),
 .UNSPECIFIED. ) ;
#16684 = CARTESIAN_POINT ( 'NONE',  ( 0.1092565886968784733, 41.73439049602436057, 10.86136484717984274 ) ) ;
#16685 = EDGE_CURVE ( 'NONE', #17824, #29827, #22270, .T. ) ;
#16686 = DIRECTION ( 'NONE',  ( -0.1024043820194934645, 0.6940285268068259183, 0.7126273545981466340 ) ) ;
#16687 =( BOUNDED_SURFACE ( )  B_SPLINE_SURFACE ( 3, 1, ( 
 ( #220, #48475 ),
 ( #29070, #19680 ),
 ( #5539, #37887 ),
 ( #61939, #57542 ) ),
 .UNSPECIFIED., .F., .F., .F. ) 
 B_SPLINE_SURFACE_WITH_KNOTS ( ( 4, 4 ),
 ( 2, 2 ),
 ( 0.000000000000000000, 1.000000000000000000 ),
 ( 0.000000000000000000, 1.000000000000000000 ),
 .UNSPECIFIED. ) 
 GEOMETRIC_REPRESENTATION_ITEM ( )  RATIONAL_B_SPLINE_SURFACE ( (
 ( 1.000000000000000000, 1.000000000000000000),
 ( 0.7223157951917476005, 0.9931996967497186413),
 ( 0.7223157951917476005, 0.9931996967497186413),
 ( 1.000000000000000000, 1.000000000000000000) ) ) 
 REPRESENTATION_ITEM ( '' )  SURFACE ( )  );
#16688 = CARTESIAN_POINT ( 'NONE',  ( 0.8751705887134423323, -47.79200036674284036, 5.393078191591890835 ) ) ;
#16689 = ORIENTED_EDGE ( 'NONE', *, *, #26186, .T. ) ;
#16690 = CARTESIAN_POINT ( 'NONE',  ( 4.975801465491695552, 0.000000000000000000, 47.91270532121795611 ) ) ;
#16691 = DIRECTION ( 'NONE',  ( 0.000000000000000000, 0.000000000000000000, 1.000000000000000000 ) ) ;
#16692 = ADVANCED_FACE ( 'NONE', ( #12684 ), #29185, .F. ) ;
#16693 = CARTESIAN_POINT ( 'NONE',  ( 3.050102900204245682, 8.016424753797352309, -43.25693219987711302 ) ) ;
#16694 = DIRECTION ( 'NONE',  ( 0.000000000000000000, 0.000000000000000000, 1.000000000000000000 ) ) ;
#16695 = VECTOR ( 'NONE', #54201, 1000.000000000000114 ) ;
#16696 = ORIENTED_EDGE ( 'NONE', *, *, #59404, .T. ) ;
#16697 = ORIENTED_EDGE ( 'NONE', *, *, #2826, .T. ) ;
#16698 = CARTESIAN_POINT ( 'NONE',  ( 0.9783242366443549720, -39.50104640422178193, -14.00006511335010906 ) ) ;
#16699 = CARTESIAN_POINT ( 'NONE',  ( 0.1073791018717578927, -37.58707531572220262, 21.14095454447495115 ) ) ;
#16700 = CARTESIAN_POINT ( 'NONE',  ( 0.9757892942422827787, -16.37293303864333893, 39.66188497122489309 ) ) ;
#16701 = CARTESIAN_POINT ( 'NONE',  ( 0.7044674535452954967, 49.05595398932693740, -2.305667150293843282 ) ) ;
#16702 = AXIS2_PLACEMENT_3D ( 'NONE', #20638, #54430, #39155 ) ;
#16703 = B_SPLINE_CURVE_WITH_KNOTS ( 'NONE', 3,
 ( #56441, #13555, #37685, #5044, #43310, #14484 ),
 .UNSPECIFIED., .F., .F.,
 ( 4, 2, 4 ),
 ( 1.554159946372743606E-17, 0.0002293319059085096559, 0.0004586638118170038077 ),
 .UNSPECIFIED. ) ;
#16704 = CARTESIAN_POINT ( 'NONE',  ( 58.00000000000000000, 8.437969416220405915E-15, -2.995852231480068572E-16 ) ) ;
#16705 = CARTESIAN_POINT ( 'NONE',  ( 2.528190830796654964, -2.611642835106711136, 41.89789323885920425 ) ) ;
#16706 = EDGE_CURVE ( 'NONE', #21206, #46227, #12601, .T. ) ;
#16707 = CARTESIAN_POINT ( 'NONE',  ( 0.6031356219577718170, 12.36679943215660948, -46.49081620741443999 ) ) ;
#16708 = CARTESIAN_POINT ( 'NONE',  ( -6.063463321072276813, -12.93474753578269798, 14.26578980165603383 ) ) ;
#16709 = CARTESIAN_POINT ( 'NONE',  ( 4.962356264823602814, -15.53171314616136200, -39.11523340858015274 ) ) ;
#16710 = CARTESIAN_POINT ( 'NONE',  ( 0.9789233960466705575, 32.80823903839893774, 26.07596935938558502 ) ) ;
#16711 = CARTESIAN_POINT ( 'NONE',  ( 0.5809828226811548646, 29.58751527316178809, 37.66417181417562432 ) ) ;
#16712 = CARTESIAN_POINT ( 'NONE',  ( 3.559346040607745287, 41.03794546218089323, -15.78978510889415077 ) ) ;
#16713 = CARTESIAN_POINT ( 'NONE',  ( 0.6017667736363749853, -33.76945004754892921, -34.26315558341178757 ) ) ;
#16714 = CARTESIAN_POINT ( 'NONE',  ( 0.9722240750034580881, 42.61332880321398164, 5.023189755349083185 ) ) ;
#16715 = EDGE_CURVE ( 'NONE', #52796, #34886, #17029, .T. ) ;
#16716 = CARTESIAN_POINT ( 'NONE',  ( 0.1313383488274129651, 43.11882601516400371, -0.6377633466096090942 ) ) ;
#16717 = VECTOR ( 'NONE', #54574, 1000.000000000000114 ) ;
#16718 = FACE_OUTER_BOUND ( 'NONE', #32933, .T. ) ;
#16719 = CARTESIAN_POINT ( 'NONE',  ( 0.6008122571543323964, 48.28333758046749580, 8.959568212583292279 ) ) ;
#16721 = ORIENTED_EDGE ( 'NONE', *, *, #37074, .T. ) ;
#16720 = CARTESIAN_POINT ( 'NONE',  ( 0.7056759521545029612, 23.27569225635726724, -40.71843537151615777 ) ) ;
#16722 = EDGE_LOOP ( 'NONE', ( #47589, #56280, #38162, #44070 ) ) ;
#16723 = CARTESIAN_POINT ( 'NONE',  ( 0.5997462898726536595, 17.44942740672471260, -45.90282249842328355 ) ) ;
#16724 = B_SPLINE_CURVE_WITH_KNOTS ( 'NONE', 3,
 ( #30285, #25284, #44430, #16830 ),
 .UNSPECIFIED., .F., .F.,
 ( 4, 4 ),
 ( 0.000000000000000000, 0.005013413432710150247 ),
 .UNSPECIFIED. ) ;
#16725 = DIRECTION ( 'NONE',  ( 0.000000000000000000, 0.000000000000000000, 1.000000000000000000 ) ) ;
#16726 = CONICAL_SURFACE ( 'NONE', #1667, 42.92674063221959813, 1.485477209440487556 ) ;
#16727 = FACE_OUTER_BOUND ( 'NONE', #13618, .T. ) ;
#16728 = ORIENTED_EDGE ( 'NONE', *, *, #6697, .T. ) ;
#16729 = EDGE_CURVE ( 'NONE', #12652, #33929, #35291, .T. ) ;
#16730 = VERTEX_POINT ( 'NONE', #46498 ) ;
#16731 = CARTESIAN_POINT ( 'NONE',  ( 0.6000166863083106206, -31.02657807334564666, 38.06803035050592854 ) ) ;
#16732 = CARTESIAN_POINT ( 'NONE',  ( 0.1098349054025746230, -37.45309339978498286, 21.37724154645436769 ) ) ;
#16733 = VERTEX_POINT ( 'NONE', #3549 ) ;
#16734 = ORIENTED_EDGE ( 'NONE', *, *, #40918, .F. ) ;
#16735 = B_SPLINE_CURVE_WITH_KNOTS ( 'NONE', 3,
 ( #47076, #12948, #32660, #32046, #28554, #36754 ),
 .UNSPECIFIED., .F., .F.,
 ( 4, 2, 4 ),
 ( 0.000000000000000000, 0.0002291459268755699637, 0.0004582918537511399275 ),
 .UNSPECIFIED. ) ;
#16736 = CARTESIAN_POINT ( 'NONE',  ( 0.5827359174754830340, 47.89462060834303259, 0.3632382226752371990 ) ) ;
#16737 = VECTOR ( 'NONE', #37625, 1000.000000000000227 ) ;
#16738 = CARTESIAN_POINT ( 'NONE',  ( 2.526464513654346433, -4.405490210168683696, 42.75268905308553258 ) ) ;
#16739 = CARTESIAN_POINT ( 'NONE',  ( 0.6000166863083090663, 46.77044519531233391, -14.97828220927684839 ) ) ;
#16740 = B_SPLINE_CURVE_WITH_KNOTS ( 'NONE', 3,
 ( #1815, #44170, #6187, #53810 ),
 .UNSPECIFIED., .F., .F.,
 ( 4, 4 ),
 ( 0.000000000000000000, 0.005014147105413707325 ),
 .UNSPECIFIED. ) ;
#16741 = ORIENTED_EDGE ( 'NONE', *, *, #18216, .T. ) ;
#16742 = CARTESIAN_POINT ( 'NONE',  ( 3.238931869106854489, 40.38337734129182621, 14.74782013370860767 ) ) ;
#16743 = CARTESIAN_POINT ( 'NONE',  ( 4.975610109902397937, -32.45573888811600227, -36.59336579715246529 ) ) ;
#16744 =( BOUNDED_SURFACE ( )  B_SPLINE_SURFACE ( 3, 1, ( 
 ( #38135, #23391 ),
 ( #24006, #18391 ),
 ( #41907, #18700 ),
 ( #56885, #37512 ) ),
 .UNSPECIFIED., .F., .F., .F. ) 
 B_SPLINE_SURFACE_WITH_KNOTS ( ( 4, 4 ),
 ( 2, 2 ),
 ( 0.000000000000000000, 1.000000000000000000 ),
 ( 0.000000000000000000, 1.000000000000000000 ),
 .UNSPECIFIED. ) 
 GEOMETRIC_REPRESENTATION_ITEM ( )  RATIONAL_B_SPLINE_SURFACE ( (
 ( 1.000000000000000000, 1.000000000000000000),
 ( 0.7282232189291694135, 0.9929344683865672927),
 ( 0.7282232189291694135, 0.9929344683865672927),
 ( 1.000000000000000000, 1.000000000000000000) ) ) 
 REPRESENTATION_ITEM ( '' )  SURFACE ( )  );
#16745 = B_SPLINE_CURVE_WITH_KNOTS ( 'NONE', 3,
 ( #55628, #27145, #8033, #46273 ),
 .UNSPECIFIED., .F., .F.,
 ( 4, 4 ),
 ( 0.000000000000000000, 0.004446090762761381598 ),
 .UNSPECIFIED. ) ;
#16746 = CARTESIAN_POINT ( 'NONE',  ( 0.9741495583595156660, 42.48790363482606125, 5.992561317325313830 ) ) ;
#16747 = VERTEX_POINT ( 'NONE', #32709 ) ;
#16748 = VECTOR ( 'NONE', #9230, 1000.000000000000000 ) ;
#16749 = ORIENTED_EDGE ( 'NONE', *, *, #44109, .T. ) ;
#16750 = B_SPLINE_CURVE_WITH_KNOTS ( 'NONE', 3,
 ( #38342, #37413, #56793, #24213, #14531, #52095, #9192, #4462, #28299, #23915, #13923, #383, #33634, #47725, #42130, #38049, #4773, #4163, #56486, #23601, #52404, #23001, #43350, #33333, #23300 ),
 .UNSPECIFIED., .F., .F.,
 ( 4, 3, 3, 3, 3, 3, 3, 3, 4 ),
 ( 6.992893892674702526E-18, 0.0005656085177311382306, 0.001131215744874499839, 0.001696821861372765482, 0.002262427090022498151, 0.002828031679238744191, 0.003393635864401604429, 0.003977030878808129888, 0.004561030005651157265 ),
 .UNSPECIFIED. ) ;
#16751 = CARTESIAN_POINT ( 'NONE',  ( 0.6039202388192953519, 4.542059820466915809, -48.89717175293773010 ) ) ;
#16752 = CARTESIAN_POINT ( 'NONE',  ( 0.2940133293163014749, -40.58327630480741277, -17.29850380656375108 ) ) ;
#16753 = ORIENTED_EDGE ( 'NONE', *, *, #55805, .F. ) ;
#16754 = CARTESIAN_POINT ( 'NONE',  ( 0.6001305935487422083, -12.95698906763841052, 46.33281397023041848 ) ) ;
#16755 = CARTESIAN_POINT ( 'NONE',  ( 0.6029443449137436017, -7.880500877275125937, 48.47099384071466943 ) ) ;
#16756 = CARTESIAN_POINT ( 'NONE',  ( -6.078075953587585900, 15.43522972334815258, -11.51298647765233518 ) ) ;
#16757 = CARTESIAN_POINT ( 'NONE',  ( 2.706805983486679779, -43.82831923521022333, -3.981776781319652514 ) ) ;
#16758 = EDGE_CURVE ( 'NONE', #39044, #26356, #31214, .T. ) ;
#16759 = ORIENTED_EDGE ( 'NONE', *, *, #17407, .F. ) ;
#16760 = CARTESIAN_POINT ( 'NONE',  ( 0.5998501479064699549, -18.89267974119636406, -44.24259072156078787 ) ) ;
#16761 = CARTESIAN_POINT ( 'NONE',  ( 0.6845945791218023269, -13.06825445484081349, 45.05138450944075146 ) ) ;
#16762 = EDGE_CURVE ( 'NONE', #29999, #58236, #45444, .T. ) ;
#16763 =( BOUNDED_SURFACE ( )  B_SPLINE_SURFACE ( 3, 1, ( 
 ( #16189, #15576 ),
 ( #11487, #35002 ),
 ( #40327, #6432 ),
 ( #54991, #11808 ) ),
 .UNSPECIFIED., .F., .F., .F. ) 
 B_SPLINE_SURFACE_WITH_KNOTS ( ( 4, 4 ),
 ( 2, 2 ),
 ( 0.000000000000000000, 1.000000000000000000 ),
 ( 0.000000000000000000, 1.000000000000000000 ),
 .UNSPECIFIED. ) 
 GEOMETRIC_REPRESENTATION_ITEM ( )  RATIONAL_B_SPLINE_SURFACE ( (
 ( 1.000000000000000000, 1.000000000000000000),
 ( 0.7282232189291694135, 0.9929344683865672927),
 ( 0.7282232189291694135, 0.9929344683865672927),
 ( 1.000000000000000000, 1.000000000000000000) ) ) 
 REPRESENTATION_ITEM ( '' )  SURFACE ( )  );
#16764 = FACE_OUTER_BOUND ( 'NONE', #4585, .T. ) ;
#16765 = CARTESIAN_POINT ( 'NONE',  ( 5.917102823773431552, -19.39960706793709733, 5.305182717059529374 ) ) ;
#16766 = ORIENTED_EDGE ( 'NONE', *, *, #25585, .F. ) ;
#16767 = CARTESIAN_POINT ( 'NONE',  ( 5.960721111146673579, -19.82454228767749527, 5.318514366754590661 ) ) ;
#16768 = ADVANCED_FACE ( 'NONE', ( #23002 ), #42029, .F. ) ;
#16769 = CARTESIAN_POINT ( 'NONE',  ( 4.963659409799332067, -44.62477100936216345, -3.403493583737785322 ) ) ;
#16770 = CARTESIAN_POINT ( 'NONE',  ( -1.400000000000000355, 0.000000000000000000, -5.100000000000000533 ) ) ;
#16771 = ADVANCED_FACE ( 'NONE', ( #42426 ), #10723, .F. ) ;
#16772 = CONICAL_SURFACE ( 'NONE', #11768, 43.08621763946400307, 1.568696531533066763 ) ;
#16773 = VERTEX_POINT ( 'NONE', #28603 ) ;
#16774 = CARTESIAN_POINT ( 'NONE',  ( 0.1368894036331286812, -11.94180260692783335, 42.47651911845537853 ) ) ;
#16775 = VECTOR ( 'NONE', #15374, 999.9999999999998863 ) ;
#16776 = EDGE_CURVE ( 'NONE', #24375, #36534, #41291, .T. ) ;
#16777 = CARTESIAN_POINT ( 'NONE',  ( 4.956653778116988818, -43.37017594958040689, -20.77844580450608447 ) ) ;
#16778 = CARTESIAN_POINT ( 'NONE',  ( -6.015611763856276717, -0.006214430185273883862, 18.84324252354755203 ) ) ;
#16779 = PRODUCT ( 'Input Eccentric Shaft', 'Input Eccentric Shaft', '', ( #21797 ) ) ;
#16780 = LINE ( 'NONE', #35891, #56462 ) ;
#16781 = CARTESIAN_POINT ( 'NONE',  ( 0.5848930533535030563, 22.69711449001784231, 41.03795896745572946 ) ) ;
#16782 = B_SPLINE_CURVE_WITH_KNOTS ( 'NONE', 3,
 ( #19681, #61940, #23753, #19371 ),
 .UNSPECIFIED., .F., .F.,
 ( 4, 4 ),
 ( 1.999757930724971929E-17, 0.004444306975806117631 ),
 .UNSPECIFIED. ) ;
#16783 = EDGE_CURVE ( 'NONE', #54358, #33554, #47268, .T. ) ;
#16784 = CARTESIAN_POINT ( 'NONE',  ( 0.5809828226811617480, 46.40184912890855884, -11.86925843957117799 ) ) ;
#16785 = CARTESIAN_POINT ( 'NONE',  ( 3.240649175237394708, 35.83975900205959420, 25.51032324514801175 ) ) ;
#16786 = CARTESIAN_POINT ( 'NONE',  ( 5.960221823109900008, -5.317678907195300120, -19.82478916873573027 ) ) ;
#16787 = CARTESIAN_POINT ( 'NONE',  ( 1.231276596079887264, 38.91607545535247681, 15.58254928345742840 ) ) ;
#16788 = ADVANCED_FACE ( 'NONE', ( #33334 ), #29924, .F. ) ;
#16789 = DIRECTION ( 'NONE',  ( 0.000000000000000000, 0.000000000000000000, 1.000000000000000000 ) ) ;
#16790 = CARTESIAN_POINT ( 'NONE',  ( 0.6253024248130445439, 33.51950167461898644, -35.88714581717047736 ) ) ;
#16791 = ORIENTED_EDGE ( 'NONE', *, *, #20670, .F. ) ;
#16792 = CARTESIAN_POINT ( 'NONE',  ( 0.5807400328401637335, -41.75144119563869793, -23.47602859900758432 ) ) ;
#16793 = CARTESIAN_POINT ( 'NONE',  ( 4.553261556744873317, 7.233533384970671776, 43.32684572631789166 ) ) ;
#16794 = CARTESIAN_POINT ( 'NONE',  ( 0.7762783648524365088, -13.25585403815088270, -46.03397615175199320 ) ) ;
#16795 = CARTESIAN_POINT ( 'NONE',  ( 0.5835871038041859915, -34.68875627993142530, -31.55827372739225467 ) ) ;
#16796 = CARTESIAN_POINT ( 'NONE',  ( 5.958863334805807099, -17.77512673691326128, 10.26388325355056885 ) ) ;
#16797 = AXIS2_PLACEMENT_3D ( 'NONE', #10851, #24948, #29943 ) ;
#16798 = CARTESIAN_POINT ( 'NONE',  ( 0.9791128995231611620, -31.07823802939244118, 28.11548603945144009 ) ) ;
#16799 = APPLICATION_PROTOCOL_DEFINITION ( 'draft international standard', 'automotive_design', 1998, #10377 ) ;
#16800 = CARTESIAN_POINT ( 'NONE',  ( 3.345653888883671101, -2.687187980154741140, -0.1391502195351564664 ) ) ;
#16801 = CARTESIAN_POINT ( 'NONE',  ( 2.879087469061463178, 35.90367940211508824, -25.43673489608120164 ) ) ;
#16802 = VECTOR ( 'NONE', #26185, 1000.000000000000114 ) ;
#16803 = CARTESIAN_POINT ( 'NONE',  ( 4.956445790444011124, -17.42806872899762993, -43.74700527484106516 ) ) ;
#16805 = ORIENTED_EDGE ( 'NONE', *, *, #12884, .T. ) ;
#16804 = CARTESIAN_POINT ( 'NONE',  ( 2.281448460670571610, -38.84544723616124884, -28.15071835136437883 ) ) ;
#16806 = ORIENTED_EDGE ( 'NONE', *, *, #50824, .T. ) ;
#16807 = CARTESIAN_POINT ( 'NONE',  ( 4.967162193818130511, 0.000000000000000000, 0.000000000000000000 ) ) ;
#16808 = B_SPLINE_CURVE_WITH_KNOTS ( 'NONE', 3,
 ( #18839, #18212, #38261, #37641 ),
 .UNSPECIFIED., .F., .F.,
 ( 4, 4 ),
 ( 0.000000000000000000, 0.005013413432710148512 ),
 .UNSPECIFIED. ) ;
#16809 = CARTESIAN_POINT ( 'NONE',  ( -6.015611763856276717, 7.216738110653281524, 17.40650793417846032 ) ) ;
#16810 = LINE ( 'NONE', #26495, #51785 ) ;
#16811 = EDGE_CURVE ( 'NONE', #24826, #33742, #48635, .T. ) ;
#16812 = LINE ( 'NONE', #27423, #54500 ) ;
#16813 = CARTESIAN_POINT ( 'NONE',  ( 0.5834872094924171693, -47.51530820063771188, 6.026535573893953668 ) ) ;
#16814 = CARTESIAN_POINT ( 'NONE',  ( 0.1101816497532062955, 41.61967362528556436, -11.29256821151170342 ) ) ;
#16816 = EDGE_CURVE ( 'NONE', #26055, #5134, #18926, .T. ) ;
#16815 = ORIENTED_EDGE ( 'NONE', *, *, #57315, .F. ) ;
#16817 = VERTEX_POINT ( 'NONE', #38050 ) ;
#16818 = DIRECTION ( 'NONE',  ( 0.000000000000000000, 0.000000000000000000, -1.000000000000000000 ) ) ;
#16819 = VECTOR ( 'NONE', #58039, 1000.000000000000114 ) ;
#16820 = CARTESIAN_POINT ( 'NONE',  ( 0.1084644655670279484, -11.54510651093232454, -41.55047717876500712 ) ) ;
#16821 = CARTESIAN_POINT ( 'NONE',  ( 5.960721111146673579, 7.860635756377893912, -18.96073515164540879 ) ) ;
#16822 = ORIENTED_EDGE ( 'NONE', *, *, #58464, .T. ) ;
#16823 = B_SPLINE_CURVE_WITH_KNOTS ( 'NONE', 3,
 ( #8499, #60813, #57036, #37052, #14163, #51104 ),
 .UNSPECIFIED., .F., .F.,
 ( 4, 2, 4 ),
 ( 8.583542049204267543E-17, 0.0002293366620881436024, 0.0004586733241762013360 ),
 .UNSPECIFIED. ) ;
#16824 = ORIENTED_EDGE ( 'NONE', *, *, #59109, .T. ) ;
#16825 = CARTESIAN_POINT ( 'NONE',  ( 7.000000000000007105, -2.649999999999153477, -80.00000000000004263 ) ) ;
#16826 = CARTESIAN_POINT ( 'NONE',  ( 4.960156602257182357, 45.62767441207063968, -8.553784487772425393 ) ) ;
#16827 = B_SPLINE_CURVE_WITH_KNOTS ( 'NONE', 3,
 ( #11295, #40150, #54485, #25385 ),
 .UNSPECIFIED., .F., .F.,
 ( 4, 4 ),
 ( 3.252606517456513784E-19, 0.004446298630425062418 ),
 .UNSPECIFIED. ) ;
#16828 = ORIENTED_EDGE ( 'NONE', *, *, #54707, .T. ) ;
#16829 = CARTESIAN_POINT ( 'NONE',  ( 2.526552050251864134, -29.52128340070579426, -31.23611603144895099 ) ) ;
#16830 = CARTESIAN_POINT ( 'NONE',  ( 4.975610109902397937, -22.11219452748616021, 43.62912170003406942 ) ) ;
#16831 = ORIENTED_EDGE ( 'NONE', *, *, #5571, .F. ) ;
#16832 = CARTESIAN_POINT ( 'NONE',  ( -31.75000000000000000, 15.14599999999999369, 0.000000000000000000 ) ) ;
#16833 = CARTESIAN_POINT ( 'NONE',  ( 0.5850706913938534814, -0.1816364388696994903, -47.89601588673689037 ) ) ;
#16834 = ORIENTED_EDGE ( 'NONE', *, *, #16857, .T. ) ;
#16835 = CARTESIAN_POINT ( 'NONE',  ( -6.057079549204054558, 17.85280408805624219, -7.218629876453069194 ) ) ;
#16836 = CARTESIAN_POINT ( 'NONE',  ( 0.6253024248130475415, 11.59571641818049059, -47.71774919426502493 ) ) ;
#16837 = CARTESIAN_POINT ( 'NONE',  ( 0.9722240741986378776, 42.61332881199394507, -5.023189681690327646 ) ) ;
#16838 = FILL_AREA_STYLE_COLOUR ( '', #26379 ) ;
#16839 = EDGE_CURVE ( 'NONE', #56316, #56726, #19846, .T. ) ;
#16840 = ORIENTED_EDGE ( 'NONE', *, *, #47112, .T. ) ;
#16841 = DIRECTION ( 'NONE',  ( 0.000000000000000000, 0.000000000000000000, 1.000000000000000000 ) ) ;
#16842 = CARTESIAN_POINT ( 'NONE',  ( 0.7056313189692687837, -18.97455749483731324, 42.89189680851932707 ) ) ;
#16843 = EDGE_CURVE ( 'NONE', #48540, #51786, #29526, .T. ) ;
#16844 = VERTEX_POINT ( 'NONE', #58017 ) ;
#16845 = CARTESIAN_POINT ( 'NONE',  ( 0.1064266418746777354, -30.88821921809869053, 30.09411284098518280 ) ) ;
#16846 = MECHANICAL_DESIGN_GEOMETRIC_PRESENTATION_REPRESENTATION (  '', ( #59841 ), #27828 ) ;
#16847 = ORIENTED_EDGE ( 'NONE', *, *, #44258, .T. ) ;
#16848 = CARTESIAN_POINT ( 'NONE',  ( 0.9790850452238883950, 4.245257672208578192, 41.69310635536467657 ) ) ;
#16850 = ORIENTED_EDGE ( 'NONE', *, *, #6384, .F. ) ;
#16849 = ADVANCED_FACE ( 'NONE', ( #57097 ), #55522, .F. ) ;
#16851 = CARTESIAN_POINT ( 'NONE',  ( 4.214292481396495482, -11.25702090725073035, -1.199999999999999956 ) ) ;
#16852 = CARTESIAN_POINT ( 'NONE',  ( 0.9762797500689124330, 24.45014227842982635, 34.03697001423955726 ) ) ;
#16853 = EDGE_CURVE ( 'NONE', #19785, #40624, #26008, .T. ) ;
#16854 = CARTESIAN_POINT ( 'NONE',  ( 0.1100053167205930355, -26.10991185395913305, 34.32189548568238280 ) ) ;
#16855 = ORIENTED_EDGE ( 'NONE', *, *, #12365, .F. ) ;
#16856 = CARTESIAN_POINT ( 'NONE',  ( 0.1129192098497455998, -27.13044910148877165, -34.79785222304216319 ) ) ;
#16857 = EDGE_CURVE ( 'NONE', #48312, #12101, #43351, .T. ) ;
#16858 = CARTESIAN_POINT ( 'NONE',  ( 5.959547316686252039, -14.51632612601538952, 14.51128755440516116 ) ) ;
#16859 = ORIENTED_EDGE ( 'NONE', *, *, #43789, .F. ) ;
#16860 = B_SPLINE_CURVE_WITH_KNOTS ( 'NONE', 3,
 ( #46831, #22693, #50880, #46209 ),
 .UNSPECIFIED., .F., .F.,
 ( 4, 4 ),
 ( 0.000000000000000000, 0.004041751736740992543 ),
 .UNSPECIFIED. ) ;
#16861 = ORIENTED_EDGE ( 'NONE', *, *, #39638, .T. ) ;
#16862 = CARTESIAN_POINT ( 'NONE',  ( 2.500000000000000000, 2.357898499370431722, -2.818925648462311528E-15 ) ) ;
#16863 = CARTESIAN_POINT ( 'NONE',  ( 0.7413678028165008316, 30.33017393467367739, 32.00885253898809424 ) ) ;
#16864 = CARTESIAN_POINT ( 'NONE',  ( 3.407937589446174087, 12.08659953757617878, -6.447869442558038067 ) ) ;
#16865 = CARTESIAN_POINT ( 'NONE',  ( 0.1095718737110177449, 30.31138510522951535, 30.67477146794383458 ) ) ;
#16866 = CARTESIAN_POINT ( 'NONE',  ( 1.084202172485504434E-14, 4.618802153517020059, -0.3572655899081733644 ) ) ;
#16867 = DIRECTION ( 'NONE',  ( 0.000000000000000000, -1.224646799147332007E-16, 1.000000000000000000 ) ) ;
#16868 = ORIENTED_EDGE ( 'NONE', *, *, #47859, .F. ) ;
#16869 = CARTESIAN_POINT ( 'NONE',  ( 1.231276596079881047, 14.27346765619277846, 39.41503383336979027 ) ) ;
#16870 = ORIENTED_EDGE ( 'NONE', *, *, #24415, .F. ) ;
#16871 = AXIS2_PLACEMENT_3D ( 'NONE', #41530, #60595, #17711 ) ;
#16872 = CARTESIAN_POINT ( 'NONE',  ( 5.959828726073459926, -7.850628836606978744, 18.96492317065680666 ) ) ;
#16873 = CARTESIAN_POINT ( 'NONE',  ( 0.3676999524040323597, 44.06746933160595603, -2.002181318164867552 ) ) ;
#16874 = CARTESIAN_POINT ( 'NONE',  ( 0.6026777506516367566, 44.31962571317131250, 21.14987393063190879 ) ) ;
#16875 = FACE_OUTER_BOUND ( 'NONE', #27852, .T. ) ;
#16876 = CARTESIAN_POINT ( 'NONE',  ( 0.7762783648524376190, -47.37038525648364384, 7.133808749409267236 ) ) ;
#16877 = CARTESIAN_POINT ( 'NONE',  ( 0.3622758884714600280, 33.69533458712307095, 26.89560658783397074 ) ) ;
#16878 = CARTESIAN_POINT ( 'NONE',  ( 0.6024113833632039894, 4.498702367898188115, 48.90095649479604134 ) ) ;
#16879 = CARTESIAN_POINT ( 'NONE',  ( 5.860006189529246790, -9.426589201135824325, 47.30296539008822521 ) ) ;
#16880 = SHAPE_REPRESENTATION ( 'straight bevel gear(static)_iso_ISO - Straight bevel gear 2M 48GT 49PT 20PA 5FW ---48O25H100MD16.0N', ( #14677 ), #24677 ) ;
#16881 = CARTESIAN_POINT ( 'NONE',  ( 2.528190830796659405, -33.91013147734389577, -24.74585054796578376 ) ) ;
#16882 = FACE_OUTER_BOUND ( 'NONE', #7643, .T. ) ;
#16883 = B_SPLINE_CURVE_WITH_KNOTS ( 'NONE', 3,
 ( #50747, #7206, #45468, #60757, #21640, #26959 ),
 .UNSPECIFIED., .F., .F.,
 ( 4, 2, 4 ),
 ( 1.870625823323990238E-17, 0.0002293755540694317793, 0.0004587511081388448561 ),
 .UNSPECIFIED. ) ;
#16884 = CARTESIAN_POINT ( 'NONE',  ( 5.959547316686252039, 7.858107265727752200, -18.96183906913535466 ) ) ;
#16885 = B_SPLINE_CURVE_WITH_KNOTS ( 'NONE', 3,
 ( #53096, #9892, #61254, #61559, #5162, #4237, #24293, #18680, #33712, #14606, #43427, #14918, #57784, #19609, #19001, #38730, #61861, #52790, #47190 ),
 .UNSPECIFIED., .F., .F.,
 ( 4, 3, 3, 3, 3, 3, 4 ),
 ( 5.204329244184724719E-18, 0.0002612768053151714380, 0.0003919133833142906002, 0.0005225499612322623798, 0.0006531865391693369343, 0.0008112755173415195321, 0.0009693688056799705131 ),
 .UNSPECIFIED. ) ;
#16886 = CARTESIAN_POINT ( 'NONE',  ( 2.624215991343620935, -19.66774719432946483, -43.79392271049091079 ) ) ;
#16887 = VECTOR ( 'NONE', #43071, 1000.000000000000000 ) ;
#16888 = CARTESIAN_POINT ( 'NONE',  ( 3.783278058412224087, -35.16831859152115669, -24.80906179324477279 ) ) ;
#16889 = CARTESIAN_POINT ( 'NONE',  ( 1.231276596079881047, -27.70544295162376258, 31.45926257674180704 ) ) ;
#16890 = CARTESIAN_POINT ( 'NONE',  ( 5.895596859100789899, -19.93295055289977213, 2.684337063064242912 ) ) ;
#16891 = CARTESIAN_POINT ( 'NONE',  ( 1.227938101723748288, 29.74462687941226235, 30.94118573761323177 ) ) ;
#16892 = CARTESIAN_POINT ( 'NONE',  ( 4.956653778116966613, 0.000000000000000000, 0.000000000000000000 ) ) ;
#16893 = AXIS2_PLACEMENT_3D ( 'NONE', #5809, #39082, #6419 ) ;
#16894 = EDGE_CURVE ( 'NONE', #23349, #5776, #1345, .T. ) ;
#16895 = ORIENTED_EDGE ( 'NONE', *, *, #14173, .F. ) ;
#16896 = CARTESIAN_POINT ( 'NONE',  ( 0.1098349054025745952, 11.36734385884004972, -41.59932877996187273 ) ) ;
#16897 = CARTESIAN_POINT ( 'NONE',  ( 0.5824935313925958535, -20.06998985431518534, -42.38435659888590834 ) ) ;
#16898 = CARTESIAN_POINT ( 'NONE',  ( 0.6016117650947689910, -47.58864192223926182, -12.11908471137122234 ) ) ;
#16899 = CARTESIAN_POINT ( 'NONE',  ( 0.5806925824938499181, 32.99217760300705748, -33.32774488853398509 ) ) ;
#16900 = CARTESIAN_POINT ( 'NONE',  ( 0.9747592971366254577, 39.51726118357611739, -16.71904224817861362 ) ) ;
#16901 = CONICAL_SURFACE ( 'NONE', #720, 42.92674063221959813, 1.485477209440487556 ) ;
#16902 = VERTEX_POINT ( 'NONE', #24522 ) ;
#16903 = CARTESIAN_POINT ( 'NONE',  ( 0.7762783648524385072, 17.50713302551388395, -44.59086139387524383 ) ) ;
#16904 = CARTESIAN_POINT ( 'NONE',  ( 0.6000166863083090663, -35.63988196839337519, -33.78790160675033860 ) ) ;
#16905 = DIRECTION ( 'NONE',  ( -1.000000000000000000, -0.000000000000000000, -0.000000000000000000 ) ) ;
#16906 = EDGE_LOOP ( 'NONE', ( #30058, #32365, #28446, #18138 ) ) ;
#16907 = B_SPLINE_CURVE_WITH_KNOTS ( 'NONE', 3,
 ( #39032, #28985, #19291, #61853 ),
 .UNSPECIFIED., .F., .F.,
 ( 4, 4 ),
 ( 8.673617379884035472E-19, 0.004446298630425055479 ),
 .UNSPECIFIED. ) ;
#16908 = CARTESIAN_POINT ( 'NONE',  ( 1.088313998177383501, 41.24258460930637682, 11.85828975620022696 ) ) ;
#16909 = ORIENTED_EDGE ( 'NONE', *, *, #40054, .F. ) ;
#16910 = CIRCLE ( 'NONE', #14903, 48.09070567114147110 ) ;
#16912 = CARTESIAN_POINT ( 'NONE',  ( 5.917102823773431552, 3.336722021764336521, 19.83320458728783109 ) ) ;
#16911 = VECTOR ( 'NONE', #10767, 1000.000000000000000 ) ;
#16913 = ORIENTED_EDGE ( 'NONE', *, *, #26243, .F. ) ;
#16914 = CARTESIAN_POINT ( 'NONE',  ( 0.7954196712028465122, -46.67728755034892174, 11.60747899261438398 ) ) ;
#16915 = ORIENTED_EDGE ( 'NONE', *, *, #39060, .T. ) ;
#16916 = CARTESIAN_POINT ( 'NONE',  ( 5.960721111146673579, 14.50930005615016682, -14.51823969584084573 ) ) ;
#16917 = CARTESIAN_POINT ( 'NONE',  ( 4.956445790444004018, -45.55738122058057371, -11.91902120403893761 ) ) ;
#16918 = ORIENTED_EDGE ( 'NONE', *, *, #54547, .F. ) ;
#16919 = LINE ( 'NONE', #17219, #12760 ) ;
#16920 = EDGE_CURVE ( 'NONE', #28607, #25211, #34226, .T. ) ;
#16921 = ORIENTED_EDGE ( 'NONE', *, *, #44659, .T. ) ;
#16922 = CARTESIAN_POINT ( 'NONE',  ( 0.5809828226811617480, -37.66417181417530458, -29.58751527316218954 ) ) ;
#16924 = EDGE_CURVE ( 'NONE', #9944, #16995, #7214, .T. ) ;
#16923 = VERTEX_POINT ( 'NONE', #25441 ) ;
#16925 = ORIENTED_EDGE ( 'NONE', *, *, #50853, .T. ) ;
#16926 = CARTESIAN_POINT ( 'NONE',  ( 4.691466044806103852, 43.66525414675643191, -9.025781474741004118 ) ) ;
#16927 = CARTESIAN_POINT ( 'NONE',  ( 3.376099380956842921, 5.244649644334445249, 12.33701883520689258 ) ) ;
#16928 = AXIS2_PLACEMENT_3D ( 'NONE', #43300, #5037, #5645 ) ;
#16929 = B_SPLINE_CURVE_WITH_KNOTS ( 'NONE', 3,
 ( #14254, #8918, #37140, #9523, #61818, #28631, #28329, #52430, #47754, #8279, #18022, #4804, #108, #19257, #13322, #47445, #41841, #32426, #46526 ),
 .UNSPECIFIED., .F., .F.,
 ( 4, 3, 3, 3, 3, 3, 4 ),
 ( 8.891118888688803850E-18, 0.0002732106629380615104, 0.0004098138914053764620, 0.0005464171197651473402, 0.0006830203481512575007, 0.0008196235766963647171, 0.001011968216111141594 ),
 .UNSPECIFIED. ) ;
#16930 = CARTESIAN_POINT ( 'NONE',  ( 1.227938101723748288, -11.92353943227977986, 41.23019537246705823 ) ) ;
#16931 = CARTESIAN_POINT ( 'NONE',  ( 0.6031357023905875581, 44.42879114414631658, 18.45021748202297829 ) ) ;
#16932 = ORIENTED_EDGE ( 'NONE', *, *, #40798, .T. ) ;
#16933 = DIRECTION ( 'NONE',  ( 1.000000000000000000, 0.000000000000000000, 0.000000000000000000 ) ) ;
#16934 = EDGE_CURVE ( 'NONE', #25309, #58463, #21375, .T. ) ;
#16935 = DIRECTION ( 'NONE',  ( 0.000000000000000000, 0.000000000000000000, 1.000000000000000000 ) ) ;
#16936 = CARTESIAN_POINT ( 'NONE',  ( 4.335381028904216727, -41.60039470203984280, 25.86820458205096784 ) ) ;
#16937 = EDGE_LOOP ( 'NONE', ( #2481, #43040, #23045, #37926 ) ) ;
#16938 = ORIENTED_EDGE ( 'NONE', *, *, #59562, .T. ) ;
#16939 = CARTESIAN_POINT ( 'NONE',  ( 0.1064266418746777076, -33.86837517279528953, -26.69589626339699961 ) ) ;
#16940 = CARTESIAN_POINT ( 'NONE',  ( 3.238741278300274029, -23.06029422819029051, 36.28414388564855386 ) ) ;
#16941 = CARTESIAN_POINT ( 'NONE',  ( 4.549368137175248350, -2.596185425822241211, 42.84816078363925840 ) ) ;
#16942 = VERTEX_POINT ( 'NONE', #30759 ) ;
#16943 = DIRECTION ( 'NONE',  ( 0.000000000000000000, 0.000000000000000000, 1.000000000000000000 ) ) ;
#16944 = CARTESIAN_POINT ( 'NONE',  ( 3.390910168358336918, -34.03117032279242693, 27.85635624044769898 ) ) ;
#16945 = CARTESIAN_POINT ( 'NONE',  ( 2.299652685299201860, 46.11347781897552522, 16.66819991171828619 ) ) ;
#16946 = ADVANCED_FACE ( 'NONE', ( #20759 ), #61918, .F. ) ;
#16947 = ORIENTED_EDGE ( 'NONE', *, *, #16681, .F. ) ;
#16948 = CARTESIAN_POINT ( 'NONE',  ( -6.016104459813374383, -14.94608397322076243, -11.47525878590931825 ) ) ;
#16949 = ORIENTED_EDGE ( 'NONE', *, *, #34244, .T. ) ;
#16950 = EDGE_CURVE ( 'NONE', #9174, #15318, #49190, .T. ) ;
#16951 = CARTESIAN_POINT ( 'NONE',  ( 0.5998501479064708430, 44.24259072156059602, 18.89267974119682947 ) ) ;
#16952 = CARTESIAN_POINT ( 'NONE',  ( 0.6064515330803585957, -44.06399544130436396, 16.05299479180740363 ) ) ;
#16953 = FACE_OUTER_BOUND ( 'NONE', #54800, .T. ) ;
#16954 = SURFACE_SIDE_STYLE ('',( #6888 ) ) ;
#16955 = CARTESIAN_POINT ( 'NONE',  ( 0.5997462898726536595, 11.43624519451647714, 47.75734421002918140 ) ) ;
#16956 =( BOUNDED_SURFACE ( )  B_SPLINE_SURFACE ( 3, 1, ( 
 ( #24496, #5367 ),
 ( #43636, #678 ),
 ( #10411, #19820 ),
 ( #57992, #53298 ) ),
 .UNSPECIFIED., .F., .F., .F. ) 
 B_SPLINE_SURFACE_WITH_KNOTS ( ( 4, 4 ),
 ( 2, 2 ),
 ( 0.000000000000000000, 1.000000000000000000 ),
 ( 0.000000000000000000, 1.000000000000000000 ),
 .UNSPECIFIED. ) 
 GEOMETRIC_REPRESENTATION_ITEM ( )  RATIONAL_B_SPLINE_SURFACE ( (
 ( 1.000000000000000000, 1.000000000000000000),
 ( 0.9953390228620291325, 0.8624445117760984880),
 ( 0.9953390228620291325, 0.8624445117760984880),
 ( 1.000000000000000000, 1.000000000000000000) ) ) 
 REPRESENTATION_ITEM ( '' )  SURFACE ( )  );
#16957 = AXIS2_PLACEMENT_3D ( 'NONE', #49657, #55272, #17095 ) ;
#16958 = ORIENTED_EDGE ( 'NONE', *, *, #60103, .T. ) ;
#16959 = CARTESIAN_POINT ( 'NONE',  ( 0.9736507210033060744, 21.84312502845843085, -36.93248879681188868 ) ) ;
#16960 = CARTESIAN_POINT ( 'NONE',  ( 0.8744876279028263033, 33.66006955981258386, -35.74003032466635688 ) ) ;
#16961 = CARTESIAN_POINT ( 'NONE',  ( 5.965394784446460541, -16.29267539192351322, 12.48356622107649194 ) ) ;
#16962 = CARTESIAN_POINT ( 'NONE',  ( 0.1073791018717483448, 21.14095454447559419, -37.58707531572184735 ) ) ;
#16963 = VECTOR ( 'NONE', #28241, 1000.000000000000114 ) ;
#16964 = CARTESIAN_POINT ( 'NONE',  ( 5.958863334805807099, -5.311251202228990387, 19.82657410201433734 ) ) ;
#16965 = CARTESIAN_POINT ( 'NONE',  ( 0.7245667037590793891, -44.12005358974319336, 19.16327388243984231 ) ) ;
#16966 = CARTESIAN_POINT ( 'NONE',  ( 0.5806925824938499181, 37.13995815321135296, -28.63295078613577971 ) ) ;
#16967 = CARTESIAN_POINT ( 'NONE',  ( 0.5848930533535030563, -14.06811673146533614, 44.73657534967806981 ) ) ;
#16968 = DIRECTION ( 'NONE',  ( -1.000000000000000000, -0.000000000000000000, -0.000000000000000000 ) ) ;
#16969 = EDGE_CURVE ( 'NONE', #37162, #35170, #16066, .T. ) ;
#16970 = CARTESIAN_POINT ( 'NONE',  ( 5.965394784446460541, -7.868087674481078153, 18.95742317323932014 ) ) ;
#16971 = CARTESIAN_POINT ( 'NONE',  ( -6.078726893082806448, -11.01948708261742738, 15.79129335123464983 ) ) ;
#16972 = ORIENTED_EDGE ( 'NONE', *, *, #3725, .T. ) ;
#16973 = CIRCLE ( 'NONE', #46045, 12.49999999999999822 ) ;
#16974 = CARTESIAN_POINT ( 'NONE',  ( 3.661933894777865017, 31.32117021671156820, 35.09437933925365627 ) ) ;
#16975 = CARTESIAN_POINT ( 'NONE',  ( 5.895596859100789899, -4.666058297670689470, 19.56415301451167466 ) ) ;
#16976 = CARTESIAN_POINT ( 'NONE',  ( 2.299746137290199943, 15.71953357350441216, -46.44542606024415221 ) ) ;
#16977 = EDGE_LOOP ( 'NONE', ( #16416, #21342 ) ) ;
#16978 = ADVANCED_FACE ( 'NONE', ( #43982 ), #6285, .F. ) ;
#16979 = DIRECTION ( 'NONE',  ( -3.273063162220399693E-16, 1.000000000000000000, 1.047380211910527902E-14 ) ) ;
#16980 = CARTESIAN_POINT ( 'NONE',  ( 0.6028777368367060907, 44.28197450755376252, -21.22843760203353014 ) ) ;
#16981 = VERTEX_POINT ( 'NONE', #2242 ) ;
#16982 = CARTESIAN_POINT ( 'NONE',  ( 1.231276596079881047, -6.136529359146127405, -41.46829847537036784 ) ) ;
#16983 = CARTESIAN_POINT ( 'NONE',  ( 0.6067375320500740798, -41.12099578548233580, -24.55990317723900418 ) ) ;
#16984 = ORIENTED_EDGE ( 'NONE', *, *, #22281, .F. ) ;
#16985 = CARTESIAN_POINT ( 'NONE',  ( 4.956445790443988031, 47.01859095792194410, 2.605792484304518375 ) ) ;
#16986 = VERTEX_POINT ( 'NONE', #1940 ) ;
#16987 = ORIENTED_EDGE ( 'NONE', *, *, #292, .T. ) ;
#16988 = CARTESIAN_POINT ( 'NONE',  ( 0.9745511491811739146, -5.938142320543633446, 42.49552597049456892 ) ) ;
#16989 = ORIENTED_EDGE ( 'NONE', *, *, #52427, .F. ) ;
#16990 = B_SPLINE_CURVE_WITH_KNOTS ( 'NONE', 3,
 ( #9715, #58230, #52931, #38871 ),
 .UNSPECIFIED., .F., .F.,
 ( 4, 4 ),
 ( 7.152448122690996019E-18, 0.005014147105413701254 ),
 .UNSPECIFIED. ) ;
#16991 = ORIENTED_EDGE ( 'NONE', *, *, #55168, .F. ) ;
#16992 = CARTESIAN_POINT ( 'NONE',  ( -6.079354080745853928, 16.77752703747123064, 9.450266755763248483 ) ) ;
#16993 = CARTESIAN_POINT ( 'NONE',  ( 0.9736507210033069626, 16.00326134587917437, 39.81239086052219278 ) ) ;
#16994 = EDGE_CURVE ( 'NONE', #9584, #23847, #11035, .T. ) ;
#16995 = VERTEX_POINT ( 'NONE', #29838 ) ;
#16996 = CARTESIAN_POINT ( 'NONE',  ( 2.528190830796656741, -35.27991276599423287, 22.75042618011462636 ) ) ;
#16997 = VECTOR ( 'NONE', #16274, 999.9999999999998863 ) ;
#16998 = CARTESIAN_POINT ( 'NONE',  ( -6.077587904424778920, -14.66646125808257395, 12.47761738310216550 ) ) ;
#16999 = CARTESIAN_POINT ( 'NONE',  ( 3.678748215320119197, -43.55036755802045434, -22.40487223486901414 ) ) ;
#17000 = CARTESIAN_POINT ( 'NONE',  ( 0.5817216825391123836, -29.92823674778196974, 36.10450937730870180 ) ) ;
#17001 = VERTEX_POINT ( 'NONE', #48955 ) ;
#17002 = EDGE_CURVE ( 'NONE', #55634, #26582, #38022, .T. ) ;
#17003 = CARTESIAN_POINT ( 'NONE',  ( 0.5838002273316423851, 44.19779719735699786, 18.45474575185529886 ) ) ;
#17004 = ORIENTED_EDGE ( 'NONE', *, *, #20916, .T. ) ;
#17005 = CARTESIAN_POINT ( 'NONE',  ( 4.834790513006553603, -35.67803047646607695, -30.97850032271963272 ) ) ;
#17006 = CARTESIAN_POINT ( 'NONE',  ( 0.1154773475650540115, -12.38201431068792679, 42.35126151197906808 ) ) ;
#17007 = DIRECTION ( 'NONE',  ( 0.000000000000000000, 0.000000000000000000, 1.000000000000000000 ) ) ;
#17008 = ORIENTED_EDGE ( 'NONE', *, *, #5983, .F. ) ;
#17009 = CARTESIAN_POINT ( 'NONE',  ( 0.3676999524040366896, 19.66859742988788184, -39.48540057367844724 ) ) ;
#17010 = CARTESIAN_POINT ( 'NONE',  ( 4.553261556744875094, -20.11719049292643646, -39.04917684785361587 ) ) ;
#17011 = CARTESIAN_POINT ( 'NONE',  ( 5.895881250540457863, -20.11287301435476849, -0.004551564636875675592 ) ) ;
#17012 = CARTESIAN_POINT ( 'NONE',  ( 0.6017666602106489515, -41.83584962818300568, -23.75081624637607192 ) ) ;
#17013 = ORIENTED_EDGE ( 'NONE', *, *, #10328, .T. ) ;
#17014 = ORIENTED_EDGE ( 'NONE', *, *, #13193, .T. ) ;
#17015 = CARTESIAN_POINT ( 'NONE',  ( 0.7056313189692682286, 21.79704775904467340, -41.52875332763414207 ) ) ;
#17016 = CARTESIAN_POINT ( 'NONE',  ( 0.7413678028165008316, 42.13455360898415591, 13.00636320967101511 ) ) ;
#17017 = CARTESIAN_POINT ( 'NONE',  ( 0.9745511491811755800, -16.73445648040599210, 39.51062171155255953 ) ) ;
#17018 = EDGE_CURVE ( 'NONE', #37493, #30663, #6002, .T. ) ;
#17019 = CARTESIAN_POINT ( 'NONE',  ( 0.6041374136657475802, -47.71861871402593636, 6.106202762792685590 ) ) ;
#17020 = B_SPLINE_CURVE_WITH_KNOTS ( 'NONE', 3,
 ( #53487, #39749, #10293, #48493 ),
 .UNSPECIFIED., .F., .F.,
 ( 4, 4 ),
 ( 0.000000000000000000, 0.004446090762761359914 ),
 .UNSPECIFIED. ) ;
#17021 = B_SPLINE_CURVE_WITH_KNOTS ( 'NONE', 3,
 ( #29971, #39709, #39093, #58758, #49080, #38468, #24974, #1143, #43481, #29658, #524, #25272, #57523, #19663, #58149, #33769, #34081, #33459, #44415 ),
 .UNSPECIFIED., .F., .F.,
 ( 4, 3, 3, 3, 3, 3, 4 ),
 ( 1.734776414728241573E-18, 0.0002612768053151691612, 0.0003919133833142924433, 0.0005225499612322612956, 0.0006531865391693340069, 0.0008112755173415185563, 0.0009693688056799734405 ),
 .UNSPECIFIED. ) ;
#17022 = B_SPLINE_CURVE_WITH_KNOTS ( 'NONE', 3,
 ( #14424, #24419, #38861, #19132, #20052, #57915 ),
 .UNSPECIFIED., .F., .F.,
 ( 4, 2, 4 ),
 ( 1.523470724839017254E-16, 0.0002445252820015216292, 0.0004890505640028909281 ),
 .UNSPECIFIED. ) ;
#17023 = CARTESIAN_POINT ( 'NONE',  ( 0.8760168074887076939, 37.61398439004533856, -29.98565522133307226 ) ) ;
#17024 = DIRECTION ( 'NONE',  ( 1.000000000000000000, 0.000000000000000000, 0.000000000000000000 ) ) ;
#17025 = CARTESIAN_POINT ( 'NONE',  ( 0.8760168074887090262, 33.37827814204125332, -34.63873394077453582 ) ) ;
#17026 = CARTESIAN_POINT ( 'NONE',  ( -6.078726893082806448, 19.09748444646205456, 2.465791776663210033 ) ) ;
#17027 = CARTESIAN_POINT ( 'NONE',  ( 0.9787284016396589070, 33.00560649245351641, 25.82568370816429493 ) ) ;
#17028 = CARTESIAN_POINT ( 'NONE',  ( -6.015611763856276717, -17.41126425312542736, 7.205255340944552778 ) ) ;
#17029 = B_SPLINE_CURVE_WITH_KNOTS ( 'NONE', 3,
 ( #18305, #51170, #8255, #13603 ),
 .UNSPECIFIED., .F., .F.,
 ( 4, 4 ),
 ( 1.409462824231155764E-18, 0.004444878191957670442 ),
 .UNSPECIFIED. ) ;
#17030 = CARTESIAN_POINT ( 'NONE',  ( 2.009741617377216460, 41.34405726916381951, -15.17145365965789772 ) ) ;
#17031 = CARTESIAN_POINT ( 'NONE',  ( 0.5837157313716019313, -13.80717013915596958, -44.81739747386527739 ) ) ;
#17032 = CARTESIAN_POINT ( 'NONE',  ( 0.5988103564986355654, -18.96890181990859858, -44.21009236284874078 ) ) ;
#17033 = DIRECTION ( 'NONE',  ( 0.000000000000000000, 0.000000000000000000, 1.000000000000000000 ) ) ;
#17034 = CARTESIAN_POINT ( 'NONE',  ( 0.1092565886968785011, -0.3103822814776921457, -43.12345370280014123 ) ) ;
#17035 = CARTESIAN_POINT ( 'NONE',  ( 0.3676999524040366896, 43.96170928169366476, -3.649479463524768263 ) ) ;
#17036 = FACE_OUTER_BOUND ( 'NONE', #50778, .T. ) ;
#17038 = ORIENTED_EDGE ( 'NONE', *, *, #26132, .F. ) ;
#17037 = CARTESIAN_POINT ( 'NONE',  ( -5.995132425357893702, -18.68405145320025795, 2.451215106828278589 ) ) ;
#17039 = ORIENTED_EDGE ( 'NONE', *, *, #46537, .T. ) ;
#17040 = B_SPLINE_CURVE_WITH_KNOTS ( 'NONE', 3,
 ( #8206, #45526, #7583, #41453, #60823, #2581, #50510, #21702, #3197, #40845, #55198, #60510, #12023, #50203, #12634, #17943 ),
 .UNSPECIFIED., .F., .F.,
 ( 4, 3, 3, 3, 3, 4 ),
 ( 1.995049841954898532E-17, 0.0002618515315864428442, 0.0003927756766341985875, 0.0005236998216950575647, 0.0007855159896329908745, 0.001047349442285928304 ),
 .UNSPECIFIED. ) ;
#17041 = CARTESIAN_POINT ( 'NONE',  ( 1.092182651088186018, -11.67010021001421016, 40.25630317764550625 ) ) ;
#17042 = CARTESIAN_POINT ( 'NONE',  ( 2.879087469061463178, 2.498337803474706131, -43.93017169330331484 ) ) ;
#17043 = CARTESIAN_POINT ( 'NONE',  ( 1.231276596079887264, -23.26513148155214594, -34.87134107206314582 ) ) ;
#17044 = ORIENTED_EDGE ( 'NONE', *, *, #2589, .T. ) ;
#17045 = EDGE_LOOP ( 'NONE', ( #44266, #31686 ) ) ;
#17046 = CARTESIAN_POINT ( 'NONE',  ( 0.5987334308729317378, 36.99765834705322476, -32.29142584966560747 ) ) ;
#17047 = DIRECTION ( 'NONE',  ( 0.1011922191286467876, 0.3314939457937465250, -0.9380148712520033349 ) ) ;
#17048 = ADVANCED_FACE ( 'NONE', ( #45822 ), #3784, .T. ) ;
#17050 = VERTEX_POINT ( 'NONE', #60488 ) ;
#17049 = VECTOR ( 'NONE', #3610, 1000.000000000000000 ) ;
#17051 = VERTEX_POINT ( 'NONE', #36116 ) ;
#17052 = CARTESIAN_POINT ( 'NONE',  ( 0.5832366564991502411, 47.89515933308369000, -0.2724446024279091327 ) ) ;
#17053 = EDGE_CURVE ( 'NONE', #16986, #15504, #2799, .T. ) ;
#17054 = AXIS2_PLACEMENT_3D ( 'NONE', #33982, #4811, #114 ) ;
#17055 = CARTESIAN_POINT ( 'NONE',  ( 0.7044674535452954967, 46.86672925371332354, -14.67352758780377009 ) ) ;
#17056 = ORIENTED_EDGE ( 'NONE', *, *, #36675, .T. ) ;
#17057 = DIRECTION ( 'NONE',  ( -1.000000000000000000, -1.836909530733573776E-16, 1.925929944387235853E-32 ) ) ;
#17058 = B_SPLINE_CURVE_WITH_KNOTS ( 'NONE', 3,
 ( #55668, #12798, #23718, #13099, #8363, #3968 ),
 .UNSPECIFIED., .F., .F.,
 ( 4, 2, 4 ),
 ( 0.000000000000000000, 0.0002293801035737084775, 0.0004587602071474169551 ),
 .UNSPECIFIED. ) ;
#17059 = CARTESIAN_POINT ( 'NONE',  ( 4.999999999999997335, 9.184547653667862963E-16, -9.629649721936174886E-32 ) ) ;
#17060 = CARTESIAN_POINT ( 'NONE',  ( 0.1087620492084205859, 0.3620418170786780521, -43.12302841504342155 ) ) ;
#17061 = VERTEX_POINT ( 'NONE', #55484 ) ;
#17062 = EDGE_CURVE ( 'NONE', #20594, #27771, #54375, .T. ) ;
#17063 = ORIENTED_EDGE ( 'NONE', *, *, #6210, .F. ) ;
#17064 = CARTESIAN_POINT ( 'NONE',  ( 0.5998501479064708430, 48.10473956285918717, 0.5236536531316605680 ) ) ;
#17065 = CARTESIAN_POINT ( 'NONE',  ( 0.8753041380234530822, -0.6841799139051543133, 49.09857661601188283 ) ) ;
#17066 = ORIENTED_EDGE ( 'NONE', *, *, #5964, .T. ) ;
#17067 = CARTESIAN_POINT ( 'NONE',  ( 0.6845945791218034371, -35.36481895536458353, 30.81778870990308405 ) ) ;
#17068 = CARTESIAN_POINT ( 'NONE',  ( 4.322998006666165516, -2.120302895116613850, 47.94177812210860878 ) ) ;
#17069 = DIRECTION ( 'NONE',  ( -1.000000000000000000, -0.000000000000000000, -0.000000000000000000 ) ) ;
#17070 = CYLINDRICAL_SURFACE ( 'NONE', #21765, 12.50000000000000000 ) ;
#17071 = CARTESIAN_POINT ( 'NONE',  ( 0.8744876279028306332, 41.62483489565916983, 26.03311679935014666 ) ) ;
#17072 = EDGE_CURVE ( 'NONE', #5670, #24199, #47643, .T. ) ;
#17073 = EDGE_LOOP ( 'NONE', ( #61687, #20984, #5190, #55660 ) ) ;
#17074 = CARTESIAN_POINT ( 'NONE',  ( 3.376099380956842921, -3.529868236344322341, 12.93245583275328592 ) ) ;
#17075 = DIRECTION ( 'NONE',  ( 0.09835009131224566048, -0.4908642831975305043, -0.8656670924898598463 ) ) ;
#17076 = EDGE_CURVE ( 'NONE', #8104, #53799, #52174, .T. ) ;
#17077 = CARTESIAN_POINT ( 'NONE',  ( 0.5804410086790514622, -34.41390132670994717, 31.86225427258510834 ) ) ;
#17078 = FACE_OUTER_BOUND ( 'NONE', #49235, .T. ) ;
#17079 = ORIENTED_EDGE ( 'NONE', *, *, #59875, .T. ) ;
#17080 = CARTESIAN_POINT ( 'NONE',  ( 1.157644175074338033, -21.85425510640531144, -35.76861486307988969 ) ) ;
#17081 = FACE_OUTER_BOUND ( 'NONE', #38220, .T. ) ;
#17082 = CARTESIAN_POINT ( 'NONE',  ( 0.8744876279028306332, -48.57046782678520458, 7.159588358747709158 ) ) ;
#17083 = CARTESIAN_POINT ( 'NONE',  ( 0.9722240741986374335, 36.86535088273205929, 21.95618662952198719 ) ) ;
#17084 = AXIS2_PLACEMENT_3D ( 'NONE', #12352, #39627, #30495 ) ;
#17085 = ORIENTED_EDGE ( 'NONE', *, *, #3895, .F. ) ;
#17086 = CARTESIAN_POINT ( 'NONE',  ( 5.960721111146673579, 10.25731071096558011, 17.77882586010670707 ) ) ;
#17087 = CARTESIAN_POINT ( 'NONE',  ( 1.091591847532191961, 20.82376294252117077, -36.37485241027820138 ) ) ;
#17088 = CARTESIAN_POINT ( 'NONE',  ( 0.5980894510889457338, -0.7015180096001567556, -48.10766805928368939 ) ) ;
#17089 = EDGE_CURVE ( 'NONE', #44899, #40739, #23792, .T. ) ;
#17090 = CARTESIAN_POINT ( 'NONE',  ( 0.8551540677456715978, 46.03951182599445957, -13.28067116677154225 ) ) ;
#17091 = CARTESIAN_POINT ( 'NONE',  ( 5.894904586330512508, -9.666977479134271078, -17.63743060878067581 ) ) ;
#17092 = VECTOR ( 'NONE', #4759, 1000.000000000000000 ) ;
#17093 = CARTESIAN_POINT ( 'NONE',  ( 0.9762797500689124330, 4.697980241568662230, 41.64437257103935508 ) ) ;
#17094 = CARTESIAN_POINT ( 'NONE',  ( 2.648799415243708655, 46.95584109391743510, 14.13033794544112354 ) ) ;
#17095 = DIRECTION ( 'NONE',  ( -3.273063162220399693E-16, 1.000000000000000000, 1.047380211910527902E-14 ) ) ;
#17096 = CARTESIAN_POINT ( 'NONE',  ( 0.6029443449137434907, 41.18007799215122589, -26.75333090558397586 ) ) ;
#17097 = CARTESIAN_POINT ( 'NONE',  ( 4.956653778116987041, -47.27023054223747067, -8.845409907521421644 ) ) ;
#17098 = VERTEX_POINT ( 'NONE', #52638 ) ;
#17099 = FACE_OUTER_BOUND ( 'NONE', #60910, .T. ) ;
#17100 = CARTESIAN_POINT ( 'NONE',  ( 1.231276596079887264, -41.76121777166943616, 3.643825084340432952 ) ) ;
#17101 = CARTESIAN_POINT ( 'NONE',  ( 3.782542959838390839, 41.39849740043850801, 7.307685432642670342 ) ) ;
#17102 = CARTESIAN_POINT ( 'NONE',  ( 1.227938101723756947, -37.58536632582764980, -20.72293514920789903 ) ) ;
#17103 = CARTESIAN_POINT ( 'NONE',  ( -5.995132425357893702, 0.008513469643070757306, -18.84415457712583475 ) ) ;
#17104 = PRODUCT_CONTEXT ( 'NONE', #38386, 'mechanical' ) ;
#17105 = CARTESIAN_POINT ( 'NONE',  ( 0.1064266418746776244, 37.06314021531080272, 22.04679912212841941 ) ) ;
#17106 = CARTESIAN_POINT ( 'NONE',  ( 0.9762797500689124330, -41.77809974471938403, -3.303810967047359881 ) ) ;
#17107 = CARTESIAN_POINT ( 'NONE',  ( 0.8560838555295167129, -41.44626783305055540, -21.96769712083564841 ) ) ;
#17108 = ADVANCED_FACE ( 'NONE', ( #9421 ), #19154, .F. ) ;
#17110 = ORIENTED_EDGE ( 'NONE', *, *, #13492, .F. ) ;
#17109 = CARTESIAN_POINT ( 'NONE',  ( 0.8751705887134423323, -48.08707113907595243, -0.8911681664086732457 ) ) ;
#17111 = ORIENTED_EDGE ( 'NONE', *, *, #48509, .T. ) ;
#17112 = PLANE ( 'NONE',  #60050 ) ;
#17113 = CARTESIAN_POINT ( 'NONE',  ( -6.010958268070873523, -18.19761767765833227, 4.891065400978321875 ) ) ;
#17114 = CARTESIAN_POINT ( 'NONE',  ( 4.967162193818130511, 0.000000000000000000, 0.000000000000000000 ) ) ;
#17115 = DIRECTION ( 'NONE',  ( -1.000000000000000000, -0.000000000000000000, -0.000000000000000000 ) ) ;
#17116 = EDGE_CURVE ( 'NONE', #22756, #43281, #6550, .T. ) ;
#17117 = DIRECTION ( 'NONE',  ( 1.000000000000000000, 1.836909530733573776E-16, -1.925929944387235853E-32 ) ) ;
#17118 = CARTESIAN_POINT ( 'NONE',  ( 5.901764892641307547, 13.97448418306336926, -46.93298689894976405 ) ) ;
#17119 = CARTESIAN_POINT ( 'NONE',  ( 0.1073791018717483448, 41.52698815987167791, -11.62916352156108779 ) ) ;
#17120 = EDGE_CURVE ( 'NONE', #5475, #60728, #42651, .T. ) ;
#17121 =( BOUNDED_SURFACE ( )  B_SPLINE_SURFACE ( 3, 1, ( 
 ( #55902, #17393 ),
 ( #36515, #55581 ),
 ( #12710, #35898 ),
 ( #49978, #25859 ) ),
 .UNSPECIFIED., .F., .F., .F. ) 
 B_SPLINE_SURFACE_WITH_KNOTS ( ( 4, 4 ),
 ( 2, 2 ),
 ( 0.000000000000000000, 1.000000000000000000 ),
 ( 0.000000000000000000, 1.000000000000000000 ),
 .UNSPECIFIED. ) 
 GEOMETRIC_REPRESENTATION_ITEM ( )  RATIONAL_B_SPLINE_SURFACE ( (
 ( 1.000000000000000000, 1.000000000000000000),
 ( 0.7282232189291693025, 0.9929344683865674037),
 ( 0.7282232189291693025, 0.9929344683865674037),
 ( 1.000000000000000000, 1.000000000000000000) ) ) 
 REPRESENTATION_ITEM ( '' )  SURFACE ( )  );
#17122 = ORIENTED_EDGE ( 'NONE', *, *, #40172, .T. ) ;
#17123 = ORIENTED_EDGE ( 'NONE', *, *, #18060, .F. ) ;
#17124 = CARTESIAN_POINT ( 'NONE',  ( 4.956445790444031552, 34.56007374686835476, -31.98654955994249960 ) ) ;
#17125 = ADVANCED_FACE ( 'NONE', ( #37653 ), #51134, .F. ) ;
#17126 = CARTESIAN_POINT ( 'NONE',  ( 0.1103744047535531458, -39.82693656558422646, -16.53879706351759538 ) ) ;
#17127 = CARTESIAN_POINT ( 'NONE',  ( 0.9790724872846771065, 32.91492816068598160, -25.94113941519019306 ) ) ;
#17128 = ORIENTED_EDGE ( 'NONE', *, *, #10005, .T. ) ;
#17129 = CARTESIAN_POINT ( 'NONE',  ( 1.500000000000001332, 6.775741118407465085E-16, -5.453125000000000000 ) ) ;
#17130 = CARTESIAN_POINT ( 'NONE',  ( 0.8744876279028306332, -0.6840263623749832655, 49.09055060105833235 ) ) ;
#17131 = ORIENTED_EDGE ( 'NONE', *, *, #15978, .F. ) ;
#17132 =( BOUNDED_SURFACE ( )  B_SPLINE_SURFACE ( 3, 1, ( 
 ( #55673, #60079 ),
 ( #41613, #18105 ),
 ( #13724, #55366 ),
 ( #17798, #12489 ) ),
 .UNSPECIFIED., .F., .F., .F. ) 
 B_SPLINE_SURFACE_WITH_KNOTS ( ( 4, 4 ),
 ( 2, 2 ),
 ( 0.000000000000000000, 1.000000000000000000 ),
 ( 0.000000000000000000, 1.000000000000000000 ),
 .UNSPECIFIED. ) 
 GEOMETRIC_REPRESENTATION_ITEM ( )  RATIONAL_B_SPLINE_SURFACE ( (
 ( 1.000000000000000000, 1.000000000000000000),
 ( 0.9754377213608244057, 0.9999580625633939235),
 ( 0.9754377213608244057, 0.9999580625633939235),
 ( 1.000000000000000000, 1.000000000000000000) ) ) 
 REPRESENTATION_ITEM ( '' )  SURFACE ( )  );
#17133 = AXIS2_PLACEMENT_3D ( 'NONE', #48911, #1278, #14184 ) ;
#17134 = DIRECTION ( 'NONE',  ( 0.000000000000000000, 0.000000000000000000, 1.000000000000000000 ) ) ;
#17135 = DIRECTION ( 'NONE',  ( -0.07500201931887527651, -0.9957672615368104996, -0.05312492776063274663 ) ) ;
#17136 = EDGE_LOOP ( 'NONE', ( #34197, #32308, #45035, #31144 ) ) ;
#17137 = EDGE_CURVE ( 'NONE', #51465, #6174, #57525, .T. ) ;
#17138 = DIRECTION ( 'NONE',  ( 0.000000000000000000, 0.000000000000000000, -1.000000000000000000 ) ) ;
#17139 = CARTESIAN_POINT ( 'NONE',  ( -6.016761891674565099, -18.84319130225482297, -0.003433883959981760738 ) ) ;
#17140 = ORIENTED_EDGE ( 'NONE', *, *, #53307, .T. ) ;
#17141 = EDGE_CURVE ( 'NONE', #5234, #46104, #6215, .T. ) ;
#17142 = CARTESIAN_POINT ( 'NONE',  ( -6.078726893082806448, -18.27395335922917141, -6.070969436048653911 ) ) ;
#17143 = CARTESIAN_POINT ( 'NONE',  ( 1.154321713695927842, 42.64911660416112227, -4.782433421669653129 ) ) ;
#17144 = ORIENTED_EDGE ( 'NONE', *, *, #39913, .T. ) ;
#17145 = CARTESIAN_POINT ( 'NONE',  ( 4.962356264823608143, -28.94323483023595145, -30.55363735178127271 ) ) ;
#17146 = DIRECTION ( 'NONE',  ( 0.000000000000000000, 0.000000000000000000, -1.000000000000000000 ) ) ;
#17147 = ORIENTED_EDGE ( 'NONE', *, *, #35691, .F. ) ;
#17148 = EDGE_CURVE ( 'NONE', #2619, #46035, #40240, .T. ) ;
#17149 = CARTESIAN_POINT ( 'NONE',  ( 0.1073791018717483448, 42.81622261970987608, 5.147744207007008299 ) ) ;
#17150 = APPLICATION_CONTEXT ( 'automotive_design' ) ;
#17151 = ORIENTED_EDGE ( 'NONE', *, *, #34529, .T. ) ;
#17152 = CARTESIAN_POINT ( 'NONE',  ( 4.975801465491694664, 39.51822597168457918, 27.09127437476394817 ) ) ;
#17153 = ORIENTED_EDGE ( 'NONE', *, *, #14403, .T. ) ;
#17154 = CARTESIAN_POINT ( 'NONE',  ( 0.5786265663353153954, -0.7221568112303078379, -47.89572889566446889 ) ) ;
#17155 = CARTESIAN_POINT ( 'NONE',  ( 0.6029442701453591180, -48.71537682882689069, -6.193325890317136206 ) ) ;
#17156 = CARTESIAN_POINT ( 'NONE',  ( 0.1102144999581333024, -26.35238362727865891, 34.13606714958004318 ) ) ;
#17157 = ORIENTED_EDGE ( 'NONE', *, *, #53388, .T. ) ;
#17158 = CARTESIAN_POINT ( 'NONE',  ( 0.1155031312995260795, 43.27794838057445048, 8.600047470807512084 ) ) ;
#17159 = CARTESIAN_POINT ( 'NONE',  ( 0.8551540677456715978, 33.23105123575947317, -34.52115452272894913 ) ) ;
#17160 = CARTESIAN_POINT ( 'NONE',  ( 4.335381028904216727, 0.5556724879607355394, 48.98416147848679003 ) ) ;
#17162 = ORIENTED_EDGE ( 'NONE', *, *, #34117, .T. ) ;
#17161 = ADVANCED_FACE ( 'NONE', ( #8811 ), #1918, .F. ) ;
#17163 = ORIENTED_EDGE ( 'NONE', *, *, #36184, .T. ) ;
#17164 = CARTESIAN_POINT ( 'NONE',  ( 4.975610109902397937, 48.58133226360775581, 5.683622315980952244 ) ) ;
#17165 = CARTESIAN_POINT ( 'NONE',  ( 1.231276596079887931, -40.90292846002456173, 9.177538581350681568 ) ) ;
#17167 = EDGE_CURVE ( 'NONE', #2188, #22415, #33455, .T. ) ;
#17166 = CARTESIAN_POINT ( 'NONE',  ( 0.5797568665920710407, 27.30868362185057308, -38.12428500894856143 ) ) ;
#17168 = CARTESIAN_POINT ( 'NONE',  ( 0.1073791018717578927, 41.77800844988514939, -10.69234304550012027 ) ) ;
#17169 = FACE_OUTER_BOUND ( 'NONE', #11746, .T. ) ;
#17170 = EDGE_LOOP ( 'NONE', ( #34605, #11921, #4371, #14437 ) ) ;
#17171 = FACE_OUTER_BOUND ( 'NONE', #36432, .T. ) ;
#17172 = CARTESIAN_POINT ( 'NONE',  ( 4.553261556744875094, -33.59363643963393997, 28.30206982864213217 ) ) ;
#17173 = ORIENTED_EDGE ( 'NONE', *, *, #34382, .T. ) ;
#17174 = CARTESIAN_POINT ( 'NONE',  ( 0.9757787079277440156, -30.36877398309923137, 30.31292661677481348 ) ) ;
#17175 = CARTESIAN_POINT ( 'NONE',  ( 2.648799415243708655, 43.56092747588142799, -22.51584021817966885 ) ) ;
#17176 = CARTESIAN_POINT ( 'NONE',  ( 0.5824936645240093025, 45.13218602318958972, 12.74064220549800552 ) ) ;
#17177 = CARTESIAN_POINT ( 'NONE',  ( 5.959547316686252039, 2.675599016784261597, 20.35048796920737857 ) ) ;
#17178 = CARTESIAN_POINT ( 'NONE',  ( 5.896782393890504181, 17.95394716461040829, 9.065421561537570838 ) ) ;
#17179 = VECTOR ( 'NONE', #51635, 1000.000000000000114 ) ;
#17180 = CARTESIAN_POINT ( 'NONE',  ( 5.901463166500145796, -2.027578129543060381, 20.01016734735707914 ) ) ;
#17181 = CARTESIAN_POINT ( 'NONE',  ( 5.974727161628369032, 5.327229920347426706, -19.82156119440440278 ) ) ;
#17182 = DIRECTION ( 'NONE',  ( -0.07500201931887526263, -0.1791611824598981217, -0.9809566594899399306 ) ) ;
#17183 = DIRECTION ( 'NONE',  ( 1.000000000000000000, -0.000000000000000000, -0.000000000000000000 ) ) ;
#17184 = CARTESIAN_POINT ( 'NONE',  ( 0.5807400328401574052, -17.82553128098440354, 44.45848844984437420 ) ) ;
#17185 = CARTESIAN_POINT ( 'NONE',  ( 0.3676999524040323597, 43.96170928169360081, 3.649479463525401535 ) ) ;
#17186 = DIRECTION ( 'NONE',  ( 0.1736481776669316079, -0.9848077530122079093, -5.551115123125822145E-17 ) ) ;
#17187 = CARTESIAN_POINT ( 'NONE',  ( 4.322998006666165516, 39.32552843303850665, -27.50295597456410590 ) ) ;
#17188 = CARTESIAN_POINT ( 'NONE',  ( 0.5804410086790514622, -38.97211966759181934, 26.09010809617889493 ) ) ;
#17189 = ADVANCED_FACE ( 'NONE', ( #57319 ), #8316, .F. ) ;
#17190 = CARTESIAN_POINT ( 'NONE',  ( 11.40403086437694569, 0.6959691356230525150, -1.199999999999999956 ) ) ;
#17191 = CARTESIAN_POINT ( 'NONE',  ( 0.5786265663353196143, -24.57327059187427309, 41.11783955080230868 ) ) ;
#17192 = EDGE_CURVE ( 'NONE', #15999, #45432, #8022, .T. ) ;
#17193 = ORIENTED_EDGE ( 'NONE', *, *, #57768, .T. ) ;
#17194 = CARTESIAN_POINT ( 'NONE',  ( 0.5782707292762423457, 3.973746573564317597, -46.73270473529971269 ) ) ;
#17195 = EDGE_CURVE ( 'NONE', #40357, #19147, #25071, .T. ) ;
#17196 = EDGE_CURVE ( 'NONE', #57388, #58295, #1245, .T. ) ;
#17197 = CARTESIAN_POINT ( 'NONE',  ( -6.010958268070873523, 18.68413620842264322, 2.445171577615829150 ) ) ;
#17198 = CARTESIAN_POINT ( 'NONE',  ( 2.624215991343620935, -47.39206852872462861, 7.662883702704499811 ) ) ;
#17199 = CARTESIAN_POINT ( 'NONE',  ( 4.553261556744873317, -25.31600221269608397, -35.89762663172042068 ) ) ;
#17200 = EDGE_CURVE ( 'NONE', #14965, #35032, #4338, .T. ) ;
#17201 = ORIENTED_EDGE ( 'NONE', *, *, #48309, .F. ) ;
#17202 = CARTESIAN_POINT ( 'NONE',  ( 0.9754292580325136797, -0.8180783604022585642, -41.90057535046801007 ) ) ;
#17203 = CARTESIAN_POINT ( 'NONE',  ( 5.960721111146673579, 14.50930005615016682, -14.51823969584084573 ) ) ;
#17204 = CARTESIAN_POINT ( 'NONE',  ( 0.5782707292762442330, 45.03824936633908038, 13.08787407194444619 ) ) ;
#17205 = ORIENTED_EDGE ( 'NONE', *, *, #43914, .F. ) ;
#17206 = EDGE_CURVE ( 'NONE', #37185, #41488, #32009, .T. ) ;
#17207 = CARTESIAN_POINT ( 'NONE',  ( 0.8751705887134553219, 34.63284514348538323, 33.37254303619566542 ) ) ;
#17208 = VERTEX_POINT ( 'NONE', #20380 ) ;
#17209 =( BOUNDED_SURFACE ( )  B_SPLINE_SURFACE ( 3, 1, ( 
 ( #53086, #24283 ),
 ( #18993, #9882 ),
 ( #38110, #47794 ),
 ( #8951, #27752 ) ),
 .UNSPECIFIED., .F., .F., .F. ) 
 B_SPLINE_SURFACE_WITH_KNOTS ( ( 4, 4 ),
 ( 2, 2 ),
 ( 0.000000000000000000, 1.000000000000000000 ),
 ( 0.000000000000000000, 1.000000000000000000 ),
 .UNSPECIFIED. ) 
 GEOMETRIC_REPRESENTATION_ITEM ( )  RATIONAL_B_SPLINE_SURFACE ( (
 ( 1.000000000000000000, 1.000000000000000000),
 ( 0.9952954269826590483, 0.8620686068821307169),
 ( 0.9952954269826590483, 0.8620686068821307169),
 ( 1.000000000000000000, 1.000000000000000000) ) ) 
 REPRESENTATION_ITEM ( '' )  SURFACE ( )  );
#17210 = CARTESIAN_POINT ( 'NONE',  ( 0.5837374860065632776, -0.1816420316512093458, -47.89569815517036488 ) ) ;
#17211 = FACE_OUTER_BOUND ( 'NONE', #22164, .T. ) ;
#17212 = ORIENTED_EDGE ( 'NONE', *, *, #52828, .F. ) ;
#17213 = CARTESIAN_POINT ( 'NONE',  ( 0.5786265663353153954, 28.58414684753542900, -38.43785771743173996 ) ) ;
#17214 = EDGE_LOOP ( 'NONE', ( #5856, #13676, #51033, #20136 ) ) ;
#17215 = CARTESIAN_POINT ( 'NONE',  ( 2.156380492024271511, -0.2527577876543339874, -46.96604096131991213 ) ) ;
#17216 = CARTESIAN_POINT ( 'NONE',  ( 0.1158403557922069033, 20.37552838888686679, 39.13793747832765035 ) ) ;
#17217 = AXIS2_PLACEMENT_3D ( 'NONE', #4975, #30034, #28803 ) ;
#17218 = VERTEX_POINT ( 'NONE', #5621 ) ;
#17219 = CARTESIAN_POINT ( 'NONE',  ( 3.238018933889920792, -11.19612451184691615, -7.352162150202732782 ) ) ;
#17220 = ORIENTED_EDGE ( 'NONE', *, *, #56869, .T. ) ;
#17221 = CARTESIAN_POINT ( 'NONE',  ( 5.880360259849752858, -3.090325311464535485, -47.87242051977165147 ) ) ;
#17222 = AXIS2_PLACEMENT_3D ( 'NONE', #51302, #31913, #4292 ) ;
#17223 = ORIENTED_EDGE ( 'NONE', *, *, #21014, .T. ) ;
#17224 = VERTEX_POINT ( 'NONE', #40434 ) ;
#17225 = DIRECTION ( 'NONE',  ( 0.000000000000000000, 0.000000000000000000, 1.000000000000000000 ) ) ;
#17226 = DIRECTION ( 'NONE',  ( 0.000000000000000000, -0.8660254037844390407, -0.4999999999999993339 ) ) ;
#17227 = CARTESIAN_POINT ( 'NONE',  ( 0.6016118706126976079, -25.15846823153664147, -42.17348137190825241 ) ) ;
#17228 = LINE ( 'NONE', #12232, #36277 ) ;
#17229 = CARTESIAN_POINT ( 'NONE',  ( 0.9730545539215892381, -16.88610103448586131, 39.44597740938055352 ) ) ;
#17230 = ORIENTED_EDGE ( 'NONE', *, *, #26170, .T. ) ;
#17231 = CARTESIAN_POINT ( 'NONE',  ( 0.9745511491811755800, 10.77620558745937096, 41.53317535253976445 ) ) ;
#17232 = CARTESIAN_POINT ( 'NONE',  ( 0.9787464366903567692, -17.80123337693228081, 37.94008543941954059 ) ) ;
#17233 = FACE_OUTER_BOUND ( 'NONE', #46069, .T. ) ;
#17235 = VERTEX_POINT ( 'NONE', #49185 ) ;
#17234 = B_SPLINE_CURVE_WITH_KNOTS ( 'NONE', 3,
 ( #54766, #7143, #16900, #36015, #55080, #15969, #39370, #48435, #33743, #5496, #34352, #10853, #1415, #6407, #29025, #24635, #10535, #5191, #29627 ),
 .UNSPECIFIED., .F., .F.,
 ( 4, 3, 3, 3, 3, 3, 4 ),
 ( 9.813676791237319219E-18, 0.0002724573126191672987, 0.0004086839781548454414, 0.0005449106435901818115, 0.0006811373090491508074, 0.0008459866663933726270, 0.001010840725717207728 ),
 .UNSPECIFIED. ) ;
#17236 = B_SPLINE_CURVE_WITH_KNOTS ( 'NONE', 3,
 ( #45483, #26351, #1916, #11650, #11977, #40800 ),
 .UNSPECIFIED., .F., .F.,
 ( 4, 2, 4 ),
 ( 1.951563910473907981E-18, 0.0002447193893791694912, 0.0004894387787583370309 ),
 .UNSPECIFIED. ) ;
#17237 = ORIENTED_EDGE ( 'NONE', *, *, #43887, .T. ) ;
#17238 = CARTESIAN_POINT ( 'NONE',  ( 0.1092565886968784872, -21.83052579204436938, -37.19081526480817246 ) ) ;
#17240 = EDGE_CURVE ( 'NONE', #28734, #29203, #55832, .T. ) ;
#17239 = CARTESIAN_POINT ( 'NONE',  ( 0.5806925824938499181, 36.46274162637902094, 29.49052111156212774 ) ) ;
#17241 = CARTESIAN_POINT ( 'NONE',  ( 0.5797568665920715958, 36.41064436358183087, -29.55486906806790515 ) ) ;
#17242 = ORIENTED_EDGE ( 'NONE', *, *, #17889, .T. ) ;
#17243 = CARTESIAN_POINT ( 'NONE',  ( -6.078726893082806448, -16.14009859332537999, -10.50196451462564262 ) ) ;
#17244 = CARTESIAN_POINT ( 'NONE',  ( 0.5549461598389364703, -34.81405122074062319, 27.07765745160486404 ) ) ;
#17245 = ORIENTED_EDGE ( 'NONE', *, *, #48055, .T. ) ;
#17246 = CARTESIAN_POINT ( 'NONE',  ( 1.227938101723756947, -41.23019537246717903, 11.92353943227934998 ) ) ;
#17247 = ORIENTED_EDGE ( 'NONE', *, *, #11984, .T. ) ;
#17248 = LINE ( 'NONE', #59837, #43389 ) ;
#17249 = LINE ( 'NONE', #55741, #18833 ) ;
#17250 = CARTESIAN_POINT ( 'NONE',  ( 0.9780106845699489959, 10.02007934243528808, -40.69311067523273806 ) ) ;
#17251 = B_SPLINE_CURVE_WITH_KNOTS ( 'NONE', 3,
 ( #28436, #37562, #33787, #47876, #9966, #47253, #43817, #29067, #540, #38485, #4930, #38800, #5536, #9026, #24061, #57539, #14674, #14062 ),
 .UNSPECIFIED., .F., .F.,
 ( 4, 2, 2, 2, 2, 2, 2, 2, 4 ),
 ( 0.000000000000000000, 0.0005188972795902839106, 0.001037794559180567821, 0.001556691838770851623, 0.002075589118361135643, 0.002594486397951419662, 0.003113383677541703247, 0.003632280957131987266, 0.004151178236722271285 ),
 .UNSPECIFIED. ) ;
#17252 =( NAMED_UNIT ( * ) SI_UNIT ( $, .STERADIAN. ) SOLID_ANGLE_UNIT ( ) );
#17253 = DIRECTION ( 'NONE',  ( -0.07836865515943411409, 0.9893941468723557175, 0.1223011693452884796 ) ) ;
#17254 = ORIENTED_EDGE ( 'NONE', *, *, #36715, .T. ) ;
#17255 = CARTESIAN_POINT ( 'NONE',  ( 5.895881250540457863, 19.00150250643894267, -6.593222588847996057 ) ) ;
#17256 = CARTESIAN_POINT ( 'NONE',  ( 4.975801465491695552, 0.000000000000000000, 0.000000000000000000 ) ) ;
#17257 = CARTESIAN_POINT ( 'NONE',  ( 8.000000000000012434, -80.00000000000001421, -2.147411887991766662E-31 ) ) ;
#17258 = CARTESIAN_POINT ( 'NONE',  ( 4.833616638992205949, -20.86133030530319843, 41.27831852777605093 ) ) ;
#17259 = CARTESIAN_POINT ( 'NONE',  ( 4.956653778116988818, -45.71126949320240840, -14.93973939759935021 ) ) ;
#17260 = CARTESIAN_POINT ( 'NONE',  ( 0.5824936645240081923, 32.33896082458391419, 33.96218178837067114 ) ) ;
#17261 = CARTESIAN_POINT ( 'NONE',  ( 0.5834872094924171693, 6.476680342367262533, -47.45604551759230105 ) ) ;
#17262 = CARTESIAN_POINT ( 'NONE',  ( 4.553261556744875094, 0.000000000000000000, 0.000000000000000000 ) ) ;
#17263 = CARTESIAN_POINT ( 'NONE',  ( 0.7764146366350240802, -6.921054454054549332, 46.39115733534977437 ) ) ;
#17264 = EDGE_CURVE ( 'NONE', #22365, #17224, #41666, .T. ) ;
#17265 = VECTOR ( 'NONE', #26071, 1000.000000000000114 ) ;
#17266 = EDGE_CURVE ( 'NONE', #10962, #17686, #3234, .T. ) ;
#17267 = DIRECTION ( 'NONE',  ( -1.000000000000000000, -0.000000000000000000, -0.000000000000000000 ) ) ;
#17268 = CARTESIAN_POINT ( 'NONE',  ( 0.8753041380234524160, 40.66072100792177935, -27.52896828776786009 ) ) ;
#17269 = ORIENTED_EDGE ( 'NONE', *, *, #12447, .T. ) ;
#17270 = EDGE_CURVE ( 'NONE', #31508, #29077, #52057, .T. ) ;
#17271 = CARTESIAN_POINT ( 'NONE',  ( 0.5549461598389364703, -2.290644651554962774, -44.04509782651307859 ) ) ;
#17272 = CARTESIAN_POINT ( 'NONE',  ( 4.975610109902397937, 0.000000000000000000, 0.000000000000000000 ) ) ;
#17273 = CARTESIAN_POINT ( 'NONE',  ( 1.296416391601052709, -42.33482010800442197, 12.25032164880019891 ) ) ;
#17274 = ADVANCED_FACE ( 'NONE', ( #50419 ), #30824, .F. ) ;
#17275 = ORIENTED_EDGE ( 'NONE', *, *, #57832, .T. ) ;
#17276 = CARTESIAN_POINT ( 'NONE',  ( 1.231276596079887931, -39.86997064245532840, -12.94844438486017779 ) ) ;
#17277 = CARTESIAN_POINT ( 'NONE',  ( 0.6026112563231247332, 44.31956384428061568, -21.14987601753119861 ) ) ;
#17278 = CARTESIAN_POINT ( 'NONE',  ( 43.00000000000000000, 0.000000000000000000, 0.000000000000000000 ) ) ;
#17279 = ORIENTED_EDGE ( 'NONE', *, *, #9460, .T. ) ;
#17280 = CARTESIAN_POINT ( 'NONE',  ( 0.7948884756798509921, -45.17791574701932689, -19.22640302696720482 ) ) ;
#17281 = FACE_OUTER_BOUND ( 'NONE', #14515, .T. ) ;
#17282 = CARTESIAN_POINT ( 'NONE',  ( 2.359973842542475886, -11.07206836914077108, 42.60921492660445864 ) ) ;
#17283 = ORIENTED_EDGE ( 'NONE', *, *, #21003, .F. ) ;
#17284 = EDGE_CURVE ( 'NONE', #40440, #2478, #17228, .T. ) ;
#17285 = CARTESIAN_POINT ( 'NONE',  ( 0.6009453534118439633, 28.93865405070896912, 38.43042294376924417 ) ) ;
#17286 = EDGE_LOOP ( 'NONE', ( #16483, #61670 ) ) ;
#17287 = ORIENTED_EDGE ( 'NONE', *, *, #40139, .T. ) ;
#17288 = CARTESIAN_POINT ( 'NONE',  ( 0.9741495583595162211, -5.992561317325463044, 42.48790363482602572 ) ) ;
#17290 = ORIENTED_EDGE ( 'NONE', *, *, #57194, .F. ) ;
#17289 = EDGE_CURVE ( 'NONE', #53243, #41130, #2205, .T. ) ;
#17291 = CARTESIAN_POINT ( 'NONE',  ( 0.8753041380234465318, -49.09527960836077654, -0.8898584437169343442 ) ) ;
#17292 = PRODUCT_DEFINITION_SHAPE ( 'NONE', 'NONE',  #61984 ) ;
#17293 = ORIENTED_EDGE ( 'NONE', *, *, #23040, .T. ) ;
#17294 = CARTESIAN_POINT ( 'NONE',  ( -6.010958268070873523, 16.31164801516942120, 9.434296419346264173 ) ) ;
#17295 = CARTESIAN_POINT ( 'NONE',  ( 1.657374760986086271, -0.1743100015788275059, 44.05519337462489915 ) ) ;
#17296 = ORIENTED_EDGE ( 'NONE', *, *, #34980, .F. ) ;
#17297 = CARTESIAN_POINT ( 'NONE',  ( 0.8554163680231738898, 45.48289776771382975, -11.51136324522476428 ) ) ;
#17298 = CARTESIAN_POINT ( 'NONE',  ( 5.901463166500146684, 20.06867656024511604, 1.328943738803535224 ) ) ;
#17299 = CARTESIAN_POINT ( 'NONE',  ( 2.359973842542475442, -37.59610043656226708, 22.90565708720059490 ) ) ;
#17300 = CARTESIAN_POINT ( 'NONE',  ( 0.7764146366350240802, 46.89611481693733452, -0.8915653345649677819 ) ) ;
#17301 = ORIENTED_EDGE ( 'NONE', *, *, #5553, .T. ) ;
#17302 = CARTESIAN_POINT ( 'NONE',  ( 4.975610109902397937, 2.142807115709095100, 48.86571174967821918 ) ) ;
#17303 = VERTEX_POINT ( 'NONE', #16930 ) ;
#17304 = CARTESIAN_POINT ( 'NONE',  ( 4.956445790443988031, 0.000000000000000000, 0.000000000000000000 ) ) ;
#17305 =( BOUNDED_SURFACE ( )  B_SPLINE_SURFACE ( 3, 1, ( 
 ( #6264, #11318 ),
 ( #10706, #54508 ),
 ( #53584, #16643 ),
 ( #39230, #58280 ) ),
 .UNSPECIFIED., .F., .F., .F. ) 
 B_SPLINE_SURFACE_WITH_KNOTS ( ( 4, 4 ),
 ( 2, 2 ),
 ( 0.000000000000000000, 1.000000000000000000 ),
 ( 0.000000000000000000, 1.000000000000000000 ),
 .UNSPECIFIED. ) 
 GEOMETRIC_REPRESENTATION_ITEM ( )  RATIONAL_B_SPLINE_SURFACE ( (
 ( 1.000000000000000000, 1.000000000000000000),
 ( 0.9953040768229005630, 0.8617119497784937465),
 ( 0.9953040768229005630, 0.8617119497784937465),
 ( 1.000000000000000000, 1.000000000000000000) ) ) 
 REPRESENTATION_ITEM ( '' )  SURFACE ( )  );
#17306 = CARTESIAN_POINT ( 'NONE',  ( 0.9730545539215883499, 26.52009130076770305, 33.73144377768567637 ) ) ;
#17307 = EDGE_CURVE ( 'NONE', #33349, #12356, #54257, .T. ) ;
#17308 = DIRECTION ( 'NONE',  ( 0.000000000000000000, 0.000000000000000000, 1.000000000000000000 ) ) ;
#17309 = ORIENTED_EDGE ( 'NONE', *, *, #53932, .T. ) ;
#17310 = CARTESIAN_POINT ( 'NONE',  ( 5.959547316686252039, 2.675599016784533823, -20.35048796920733949 ) ) ;
#17311 = CARTESIAN_POINT ( 'NONE',  ( 0.6039202388192952409, -1.748061966039296866, 49.07655236680626132 ) ) ;
#17312 = CARTESIAN_POINT ( 'NONE',  ( 5.981074661064941900, 14.51919955600715539, 14.50705827991451002 ) ) ;
#17313 = CARTESIAN_POINT ( 'NONE',  ( 0.6009453534118438522, -41.44251633523874290, -24.43073772334902927 ) ) ;
#17314 = ORIENTED_EDGE ( 'NONE', *, *, #6330, .T. ) ;
#17315 = ORIENTED_EDGE ( 'NONE', *, *, #40584, .F. ) ;
#17316 = CARTESIAN_POINT ( 'NONE',  ( 0.9789233960466710016, -39.54649551180114031, -13.87124434098955028 ) ) ;
#17317 = CARTESIAN_POINT ( 'NONE',  ( 0.9268187852002115479, 42.14386952154099220, 12.94791854546337539 ) ) ;
#17318 = CARTESIAN_POINT ( 'NONE',  ( -6.016761891674564211, -16.32039929810250456, -9.418621820384668553 ) ) ;
#17319 = CARTESIAN_POINT ( 'NONE',  ( 0.8753041380234530822, 46.31375555491767670, -16.31485134079719401 ) ) ;
#17320 = AXIS2_PLACEMENT_3D ( 'NONE', #12660, #31755, #36469 ) ;
#17321 = CARTESIAN_POINT ( 'NONE',  ( 4.956653778116975495, 9.917440902361160937, 47.05699031914952712 ) ) ;
#17322 = FACE_OUTER_BOUND ( 'NONE', #11951, .T. ) ;
#17323 = CARTESIAN_POINT ( 'NONE',  ( 4.549368137175248350, -18.79584381673505789, -38.59302160394747006 ) ) ;
#17324 = DIRECTION ( 'NONE',  ( -1.000000000000000000, -0.000000000000000000, -0.000000000000000000 ) ) ;
#17325 = CARTESIAN_POINT ( 'NONE',  ( -6.078075953587585900, 19.09727103821293070, 2.467673629183867678 ) ) ;
#17326 = DIRECTION ( 'NONE',  ( -0.07500201931887529039, 0.3457612750068366769, -0.9353201792989060959 ) ) ;
#17327 = CARTESIAN_POINT ( 'NONE',  ( 1.157643937452369487, 35.63734160579004850, -22.06767223490007268 ) ) ;
#17328 = CARTESIAN_POINT ( 'NONE',  ( 1.657374760986086493, 41.40460839256266468, -15.05153982523958334 ) ) ;
#17329 = B_SPLINE_CURVE_WITH_KNOTS ( 'NONE', 3,
 ( #46185, #16742, #40882, #59632 ),
 .UNSPECIFIED., .F., .F.,
 ( 4, 4 ),
 ( 6.254634441385501517E-18, 0.004566006591234648103 ),
 .UNSPECIFIED. ) ;
#17330 = CARTESIAN_POINT ( 'NONE',  ( 11.40403086437694569, 0.6959691356230525150, -1.199999999999999956 ) ) ;
#17331 = CARTESIAN_POINT ( 'NONE',  ( 0.5806925824938499181, -29.85799195566266917, -36.16244846134105018 ) ) ;
#17332 = CARTESIAN_POINT ( 'NONE',  ( 0.6031356755773454870, -6.279306815850496548, -47.69587413076371263 ) ) ;
#17333 = ADVANCED_FACE ( 'NONE', ( #12537 ), #61195, .F. ) ;
#17334 = CARTESIAN_POINT ( 'NONE',  ( 0.5997462898726536595, 17.44942740672405534, 45.90282249842351803 ) ) ;
#17335 = CARTESIAN_POINT ( 'NONE',  ( 0.5326698147273788431, 0.000000000000000000, 0.000000000000000000 ) ) ;
#17337 = ORIENTED_EDGE ( 'NONE', *, *, #39916, .F. ) ;
#17336 = CARTESIAN_POINT ( 'NONE',  ( 0.5804410086790514622, -42.10186154173658934, -20.66284362269238883 ) ) ;
#17338 = ORIENTED_EDGE ( 'NONE', *, *, #33178, .F. ) ;
#17339 = B_SPLINE_CURVE_WITH_KNOTS ( 'NONE', 3,
 ( #51288, #57750, #33674, #23957, #27491, #28960, #47458, #4507, #23646, #18969, #57133, #29259, #14267, #52443, #118, #19269 ),
 .UNSPECIFIED., .F., .F.,
 ( 4, 3, 3, 3, 3, 4 ),
 ( 2.194378057379452319E-17, 0.0002612764279487740844, 0.0003919131003184803835, 0.0005225497727000661232, 0.0007837925190632462217, 0.001045051706266716734 ),
 .UNSPECIFIED. ) ;
#17340 = CARTESIAN_POINT ( 'NONE',  ( 0.9762797500689124330, -11.93232144563832975, 40.17392798947675914 ) ) ;
#17341 = DIRECTION ( 'NONE',  ( -1.000000000000000000, -0.000000000000000000, -0.000000000000000000 ) ) ;
#17342 = CARTESIAN_POINT ( 'NONE',  ( 4.960156602257184133, -46.35381625054454702, -2.524999074838052859 ) ) ;
#17343 = EDGE_CURVE ( 'NONE', #17964, #43366, #46884, .T. ) ;
#17344 = EDGE_LOOP ( 'NONE', ( #61640, #47038, #59009, #2298 ) ) ;
#17345 = ORIENTED_EDGE ( 'NONE', *, *, #14908, .T. ) ;
#17346 = CARTESIAN_POINT ( 'NONE',  ( 4.694002226626920127, -16.06750747807276980, -42.66286411960886937 ) ) ;
#17347 = CARTESIAN_POINT ( 'NONE',  ( 3.376099380956842921, 2.658192826266324804, -13.13934528545670588 ) ) ;
#17348 = AXIS2_PLACEMENT_3D ( 'NONE', #41009, #31891, #36290 ) ;
#17349 = B_SPLINE_CURVE_WITH_KNOTS ( 'NONE', 3,
 ( #37621, #12890, #56685, #3444, #27275, #18192 ),
 .UNSPECIFIED., .F., .F.,
 ( 4, 2, 4 ),
 ( 6.149443329761889321E-18, 0.0002445244328975371855, 0.0004890488657950682995 ),
 .UNSPECIFIED. ) ;
#17350 = UNCERTAINTY_MEASURE_WITH_UNIT (LENGTH_MEASURE( 1.000000000000000082E-05 ), #20710, 'distance_accuracy_value', 'NONE');
#17351 = VERTEX_POINT ( 'NONE', #46062 ) ;
#17352 = ORIENTED_EDGE ( 'NONE', *, *, #12473, .T. ) ;
#17353 = CARTESIAN_POINT ( 'NONE',  ( 0.5782707292762423457, 45.42077932512024319, 11.69141390963249627 ) ) ;
#17354 = EDGE_CURVE ( 'NONE', #8818, #55634, #55719, .T. ) ;
#17355 = CARTESIAN_POINT ( 'NONE',  ( 2.281448460670570277, -34.83871297539680967, -32.98023336626270208 ) ) ;
#17356 = CARTESIAN_POINT ( 'NONE',  ( 4.975801465491695552, -47.76942479135487929, 3.702618843596635401 ) ) ;
#17357 = EDGE_LOOP ( 'NONE', ( #48708, #14427, #6672, #45426 ) ) ;
#17358 = EDGE_CURVE ( 'NONE', #9740, #24079, #22542, .T. ) ;
#17359 = CARTESIAN_POINT ( 'NONE',  ( 0.3676999524040323597, -17.09834788623527047, -40.66444494744902727 ) ) ;
#17360 = AXIS2_PLACEMENT_3D ( 'NONE', #6656, #27040, #35840 ) ;
#17361 = B_SPLINE_CURVE_WITH_KNOTS ( 'NONE', 3,
 ( #49645, #25846, #44985, #2019 ),
 .UNSPECIFIED., .F., .F.,
 ( 4, 4 ),
 ( 0.000000000000000000, 0.005004948556313793158 ),
 .UNSPECIFIED. ) ;
#17362 = CARTESIAN_POINT ( 'NONE',  ( -6.077587904424778920, 5.484810954822209261, 18.45840919970604688 ) ) ;
#17363 = CARTESIAN_POINT ( 'NONE',  ( 0.1103744047535531458, 21.52865142340085569, 37.36621271144544920 ) ) ;
#17364 = EDGE_LOOP ( 'NONE', ( #44500, #42561, #52899, #32869 ) ) ;
#17365 = VERTEX_POINT ( 'NONE', #8120 ) ;
#17366 = CARTESIAN_POINT ( 'NONE',  ( 0.5998501479064699549, 23.59887241503354716, -41.92175333043595487 ) ) ;
#17367 = ORIENTED_EDGE ( 'NONE', *, *, #56579, .T. ) ;
#17368 = CARTESIAN_POINT ( 'NONE',  ( 0.6008122571543323964, -48.64681258932709795, 6.711346762327411675 ) ) ;
#17369 = DIRECTION ( 'NONE',  ( 1.000000000000000000, 1.558861125776144859E-16, -3.851859888774471706E-32 ) ) ;
#17370 = CARTESIAN_POINT ( 'NONE',  ( 0.6029303876144825880, 34.10953954078140526, -33.92442033626747389 ) ) ;
#17371 = CARTESIAN_POINT ( 'NONE',  ( 4.960386119450149955, -21.43901005587166253, 38.14191018416060786 ) ) ;
#17372 = CARTESIAN_POINT ( 'NONE',  ( 0.7056555295713273779, -17.55111680842069788, 44.57023068418421730 ) ) ;
#17373 = EDGE_LOOP ( 'NONE', ( #15734, #44637, #42358, #11354 ) ) ;
#17374 = CARTESIAN_POINT ( 'NONE',  ( 0.8753041380234471980, -48.80600061351585595, 5.395612290228920749 ) ) ;
#17375 = CARTESIAN_POINT ( 'NONE',  ( -6.077587904424778920, 18.62472241188256206, -4.890371813497390363 ) ) ;
#17376 = CARTESIAN_POINT ( 'NONE',  ( 4.956653778116991482, 8.845409907521601056, -47.27023054223744225 ) ) ;
#17377 = EDGE_CURVE ( 'NONE', #15900, #56955, #37117, .T. ) ;
#17378 = ORIENTED_EDGE ( 'NONE', *, *, #25249, .T. ) ;
#17379 = CARTESIAN_POINT ( 'NONE',  ( -1.318516776095820742, -3.857556137907092619, -5.599999999999983658 ) ) ;
#17380 = CARTESIAN_POINT ( 'NONE',  ( 0.2940135542859003137, 30.25014503988288084, 32.11182451617268185 ) ) ;
#17381 = DIRECTION ( 'NONE',  ( -0.07836865515943411409, -0.9873352307081181278, 0.1379401902675529146 ) ) ;
#17382 = CARTESIAN_POINT ( 'NONE',  ( 0.8760168074887076939, 11.58706983520325551, -46.68716261866165240 ) ) ;
#17383 =( BOUNDED_SURFACE ( )  B_SPLINE_SURFACE ( 3, 1, ( 
 ( #56691, #19137 ),
 ( #38246, #14430 ),
 ( #14736, #10338 ),
 ( #7146, #58851 ) ),
 .UNSPECIFIED., .F., .F., .F. ) 
 B_SPLINE_SURFACE_WITH_KNOTS ( ( 4, 4 ),
 ( 2, 2 ),
 ( 0.000000000000000000, 1.000000000000000000 ),
 ( 0.000000000000000000, 1.000000000000000000 ),
 .UNSPECIFIED. ) 
 GEOMETRIC_REPRESENTATION_ITEM ( )  RATIONAL_B_SPLINE_SURFACE ( (
 ( 1.000000000000000000, 1.000000000000000000),
 ( 0.9729067724841187204, 0.9999501103223794596),
 ( 0.9729067724841187204, 0.9999501103223794596),
 ( 1.000000000000000000, 1.000000000000000000) ) ) 
 REPRESENTATION_ITEM ( '' )  SURFACE ( )  );
#17384 = VERTEX_POINT ( 'NONE', #47273 ) ;
#17385 = CARTESIAN_POINT ( 'NONE',  ( -6.063463321072276813, 15.42324870294179995, -11.53012800998644494 ) ) ;
#17386 = CARTESIAN_POINT ( 'NONE',  ( 50.15577769773999961, 12.80000000000000071, -3.000000000000000000 ) ) ;
#17387 = CARTESIAN_POINT ( 'NONE',  ( 1.000433927950263424, 40.58958440049706695, 10.43572306300663044 ) ) ;
#17388 = CARTESIAN_POINT ( 'NONE',  ( 0.5998501479064699549, -41.39809967730504781, 24.50586714782532027 ) ) ;
#17389 = DIRECTION ( 'NONE',  ( -1.000000000000000000, -1.836909530733573776E-16, 1.925929944387235853E-32 ) ) ;
#17390 = CARTESIAN_POINT ( 'NONE',  ( 0.2230388203127612601, 42.64472907182729955, -6.380812898001128275 ) ) ;
#17391 = CARTESIAN_POINT ( 'NONE',  ( 0.8753041380234524160, 46.87455897190329068, 14.62580080072680921 ) ) ;
#17392 = CARTESIAN_POINT ( 'NONE',  ( 5.838029081930955932, 38.95312035650144367, -26.71552867986767055 ) ) ;
#17393 = CARTESIAN_POINT ( 'NONE',  ( 5.838029081930955932, 42.16639215765273008, -21.28521624414380042 ) ) ;
#17394 = CARTESIAN_POINT ( 'NONE',  ( 4.549368137175248350, -35.80950303116083688, -23.67244292351627521 ) ) ;
#17395 = VERTEX_POINT ( 'NONE', #29083 ) ;
#17396 = CARTESIAN_POINT ( 'NONE',  ( 3.270143674763207553, 11.98875605389988941, -6.605065939546689080 ) ) ;
#17397 = CARTESIAN_POINT ( 'NONE',  ( 1.157644175074338477, -18.38970001308658908, 37.66724318168060393 ) ) ;
#17398 = CARTESIAN_POINT ( 'NONE',  ( 0.5800708119828336118, -0.6275298934111632754, -47.89175345941821860 ) ) ;
#17399 = DIRECTION ( 'NONE',  ( -0.1024043820194934507, -0.6940285268068210334, -0.7126273545981514079 ) ) ;
#17400 = AXIS2_PLACEMENT_3D ( 'NONE', #22830, #38491, #51631 ) ;
#17401 = CARTESIAN_POINT ( 'NONE',  ( 4.291220156522059348, 29.64992983783139380, -36.60970715421488109 ) ) ;
#17403 = B_SPLINE_CURVE_WITH_KNOTS ( 'NONE', 3,
 ( #2036, #54039, #1119, #44686 ),
 .UNSPECIFIED., .F., .F.,
 ( 4, 4 ),
 ( 2.189128766608093472E-17, 0.004559932413162187670 ),
 .UNSPECIFIED. ) ;
#17402 = CARTESIAN_POINT ( 'NONE',  ( 5.917102823773431552, 19.70720580609859240, 4.014443593801784615 ) ) ;
#17404 = PRODUCT_CONTEXT ( 'NONE', #26741, 'mechanical' ) ;
#17405 = CARTESIAN_POINT ( 'NONE',  ( 0.5997462898726536595, -2.096122762664449635, -49.06279547180479739 ) ) ;
#17406 = CARTESIAN_POINT ( 'NONE',  ( 2.533389852662419894, 36.00264103935801074, -25.32311927714972200 ) ) ;
#17407 = EDGE_CURVE ( 'NONE', #47199, #40254, #4228, .T. ) ;
#17408 = CARTESIAN_POINT ( 'NONE',  ( 0.6027444965799114707, -1.704510300802369427, 49.07782758560019687 ) ) ;
#17410 = ORIENTED_EDGE ( 'NONE', *, *, #20106, .T. ) ;
#17409 = CARTESIAN_POINT ( 'NONE',  ( 2.618530812446115519, 43.80811722902085847, 17.04627977145057827 ) ) ;
#17411 = EDGE_LOOP ( 'NONE', ( #42146, #21528, #37285, #39968 ) ) ;
#17412 = CARTESIAN_POINT ( 'NONE',  ( 0.8760168074886960365, 46.68716261866176609, -11.58706983520277589 ) ) ;
#17413 = DIRECTION ( 'NONE',  ( -0.07439287786467649322, 0.9262902123089771234, 0.3693942911085679737 ) ) ;
#17414 = LINE ( 'NONE', #22419, #16802 ) ;
#17415 = EDGE_CURVE ( 'NONE', #6162, #23761, #38201, .T. ) ;
#17416 = ORIENTED_EDGE ( 'NONE', *, *, #61071, .F. ) ;
#17417 = DIRECTION ( 'NONE',  ( -0.1024043820194934645, 0.2701391291102920866, -0.9573600124648712351 ) ) ;
#17418 = CARTESIAN_POINT ( 'NONE',  ( 4.335381028904216727, 14.90794766671208471, -46.66379693114267013 ) ) ;
#17419 = CARTESIAN_POINT ( 'NONE',  ( 0.5998501479064708430, -29.69975237324642237, 37.84527566984805702 ) ) ;
#17420 = EDGE_CURVE ( 'NONE', #855, #41374, #11698, .T. ) ;
#17421 = ORIENTED_EDGE ( 'NONE', *, *, #39220, .T. ) ;
#17422 = VERTEX_POINT ( 'NONE', #8736 ) ;
#17423 =( LENGTH_UNIT ( ) NAMED_UNIT ( * ) SI_UNIT ( .MILLI., .METRE. ) );
#17424 = CARTESIAN_POINT ( 'NONE',  ( 4.060580049360325461, 38.04379863422499852, 22.00311523029749239 ) ) ;
#17425 = CARTESIAN_POINT ( 'NONE',  ( 0.9775691876210976794, 33.12264418954459444, -25.67536077415113382 ) ) ;
#17426 = VERTEX_POINT ( 'NONE', #47583 ) ;
#17427 = ADVANCED_FACE ( 'NONE', ( #37272 ), #20060, .F. ) ;
#17428 = CARTESIAN_POINT ( 'NONE',  ( 1.227938101723748288, 42.91134962331487657, 0.8460948827226649760 ) ) ;
#17429 = AXIS2_PLACEMENT_3D ( 'NONE', #46166, #55525, #21720 ) ;
#17430 = CARTESIAN_POINT ( 'NONE',  ( 0.5997462898726536595, 48.09935696025637952, -9.899671214446758682 ) ) ;
#17431 = B_SPLINE_CURVE_WITH_KNOTS ( 'NONE', 3,
 ( #48337, #24523, #5398, #14836 ),
 .UNSPECIFIED., .F., .F.,
 ( 4, 4 ),
 ( 0.000000000000000000, 0.004042984057420971090 ),
 .UNSPECIFIED. ) ;
#17432 = DIRECTION ( 'NONE',  ( 0.000000000000000000, 0.000000000000000000, 1.000000000000000000 ) ) ;
#17433 = CARTESIAN_POINT ( 'NONE',  ( 0.8744876279028306332, -24.68559978112762110, 42.43785119236699188 ) ) ;
#17434 = ORIENTED_EDGE ( 'NONE', *, *, #50075, .F. ) ;
#17435 = CARTESIAN_POINT ( 'NONE',  ( 7.999999999999986677, 54.69470952477936976, 58.44237546506825964 ) ) ;
#17436 = DIRECTION ( 'NONE',  ( 0.000000000000000000, 0.000000000000000000, -1.000000000000000000 ) ) ;
#17437 = ORIENTED_EDGE ( 'NONE', *, *, #34754, .F. ) ;
#17438 = CARTESIAN_POINT ( 'NONE',  ( -6.063463321072278589, 17.85520303107530538, -7.211946838305800966 ) ) ;
#17439 = CARTESIAN_POINT ( 'NONE',  ( 0.8554163680231816613, 21.74163052365391025, -41.57531689939042252 ) ) ;
#17440 = FACE_OUTER_BOUND ( 'NONE', #54773, .T. ) ;
#17441 = CARTESIAN_POINT ( 'NONE',  ( -6.077587904424778920, 16.78120357693980935, 9.443898977818069085 ) ) ;
#17442 =( GEOMETRIC_REPRESENTATION_CONTEXT ( 3 ) GLOBAL_UNCERTAINTY_ASSIGNED_CONTEXT ( ( #12354 ) ) GLOBAL_UNIT_ASSIGNED_CONTEXT ( ( #30532, #16451, #50570 ) ) REPRESENTATION_CONTEXT ( 'NONE', 'WORKASPACE' ) );
#17443 = ORIENTED_EDGE ( 'NONE', *, *, #31687, .T. ) ;
#17444 = ORIENTED_EDGE ( 'NONE', *, *, #40976, .F. ) ;
#17445 = CARTESIAN_POINT ( 'NONE',  ( 1.231276596079887264, -27.70544295162332560, -31.45926257674220494 ) ) ;
#17446 = CARTESIAN_POINT ( 'NONE',  ( -6.078726893082806448, -14.66019907464911043, 12.48489504803213812 ) ) ;
#17447 = EDGE_LOOP ( 'NONE', ( #937, #33625, #24198, #14755, #26392, #61416, #157, #52150, #11926, #51382, #22626, #32069, #54402, #31197, #52930, #50015, #29018, #37464, #42644, #49245, #12246, #12602, #40355, #2548, #32089, #40983, #53188, #55711, #54627, #2379, #6851, #57137, #10417, #38911, #14005, #11105, #45415, #32176, #20741, #59205, #49338, #51007, #33608, #49083, #57100, #51945, #57093, #40122, #29680, #51550, #39880, #33191, #43753, #19520, #52852, #25697, #52936, #14802, #23462, #58970, #49405, #46213, #58760, #59328, #37882, #22692, #31207, #48142, #58700, #33630, #23528, #20048, #45458, #36084, #54640, #30433, #5972, #26116, #35092, #36747, #54786, #12833, #40043, #35282, #8359, #6184, #29091, #15388, #58322, #60534, #54091, #48050, #18750, #38873, #258, #5022, #41580, #44125, #38127, #42038, #3219, #54515, #21892, #56779, #56110, #48741, #49422, #52343, #7801, #35706, #38970, #37806, #25498, #50583, #6232, #55868, #31970, #11801, #52527, #22986, #38354, #8356, #43189, #420, #49933, #27666, #22816, #47099, #20382, #26857, #5942, #54007, #44406, #59859, #61764, #2297, #2172, #45211, #3854, #55787, #19006, #20826, #51980, #53192, #44509, #17748, #9481, #57321 ) ) ;
#17448 = CARTESIAN_POINT ( 'NONE',  ( -6.079354080745853928, 12.00499765711163036, 15.05566293794153232 ) ) ;
#17449 = VERTEX_POINT ( 'NONE', #4016 ) ;
#17450 = CARTESIAN_POINT ( 'NONE',  ( 2.500000000000000000, 2.357898499370431722, -2.818925648462311528E-15 ) ) ;
#17451 = ORIENTED_EDGE ( 'NONE', *, *, #2546, .F. ) ;
#17452 = CARTESIAN_POINT ( 'NONE',  ( 0.6041374136657475802, -0.1745662470647943998, 48.10739871142803992 ) ) ;
#17453 = CARTESIAN_POINT ( 'NONE',  ( 0.7048096507298635682, -17.62869676200438818, 44.76417498422286201 ) ) ;
#17454 = DIRECTION ( 'NONE',  ( -0.1011922191286467321, -0.3556331495180506952, 0.9291314211411062507 ) ) ;
#17455 = ORIENTED_EDGE ( 'NONE', *, *, #45923, .T. ) ;
#17456 = CARTESIAN_POINT ( 'NONE',  ( -6.016104459813374383, 17.41090761020846145, -7.206059014949892649 ) ) ;
#17457 = EDGE_CURVE ( 'NONE', #7691, #29670, #43303, .T. ) ;
#17458 = CARTESIAN_POINT ( 'NONE',  ( 0.8560838555295223751, 45.47430759461099115, 11.50913475776684791 ) ) ;
#17459 = CARTESIAN_POINT ( 'NONE',  ( 0.5804410086790514622, 43.38796872094602719, 17.80460676694676536 ) ) ;
#17460 = ORIENTED_EDGE ( 'NONE', *, *, #37026, .T. ) ;
#17461 = ADVANCED_FACE ( 'NONE', ( #14694 ), #5247, .T. ) ;
#17462 = VERTEX_POINT ( 'NONE', #33806 ) ;
#17463 = DIRECTION ( 'NONE',  ( 0.000000000000000000, -1.000000000000000000, 0.000000000000000000 ) ) ;
#17464 = CARTESIAN_POINT ( 'NONE',  ( 0.7954196712028457350, -24.79809944608804528, 41.21355366240420182 ) ) ;
#17465 = DIRECTION ( 'NONE',  ( 0.000000000000000000, 1.000000000000000000, 0.000000000000000000 ) ) ;
#17466 = CIRCLE ( 'NONE', #50496, 43.08621763946400307 ) ;
#17467 = CARTESIAN_POINT ( 'NONE',  ( 5.910764540655177868, -19.93482381198526454, 2.665340138569279205 ) ) ;
#17468 = CARTESIAN_POINT ( 'NONE',  ( 0.7954196712028480665, -37.62416450255270206, -29.96539649507072056 ) ) ;
#17469 = ORIENTED_EDGE ( 'NONE', *, *, #57312, .T. ) ;
#17470 = EDGE_CURVE ( 'NONE', #17001, #6542, #7223, .T. ) ;
#17471 = CARTESIAN_POINT ( 'NONE',  ( 0.8557997880470599172, -23.15977007032294210, -41.93815086860281127 ) ) ;
#17472 = CARTESIAN_POINT ( 'NONE',  ( 0.7948878604505671408, -48.79909643919308593, -5.417271824151775661 ) ) ;
#17473 = ORIENTED_EDGE ( 'NONE', *, *, #18327, .T. ) ;
#17474 = CARTESIAN_POINT ( 'NONE',  ( 0.9749527285493312379, -30.54214995146794465, 30.13822974582802061 ) ) ;
#17475 = CARTESIAN_POINT ( 'NONE',  ( -6.077587904424778920, -17.35179747939703887, 8.349320069797363075 ) ) ;
#17476 = CARTESIAN_POINT ( 'NONE',  ( 5.838029081930957709, -40.63013578422388150, 24.08852681897441528 ) ) ;
#17477 = CARTESIAN_POINT ( 'NONE',  ( 5.895596859100789899, -17.30333226730986240, 10.25294473112777105 ) ) ;
#17478 = CARTESIAN_POINT ( 'NONE',  ( 5.974727161628369032, -12.50710176110020200, 16.27409205901354383 ) ) ;
#17479 = CARTESIAN_POINT ( 'NONE',  ( 0.7954190325252784577, -47.56618055754181285, 7.138712176114637487 ) ) ;
#17480 = B_SPLINE_CURVE_WITH_KNOTS ( 'NONE', 3,
 ( #10289, #1174, #60047, #40669, #6783, #55028 ),
 .UNSPECIFIED., .F., .F.,
 ( 4, 2, 4 ),
 ( 2.032850612904068461E-17, 0.0002293319059085090867, 0.0004586638118169978446 ),
 .UNSPECIFIED. ) ;
#17481 = CARTESIAN_POINT ( 'NONE',  ( 4.549368137175248350, 32.41327393324100825, 28.14399996863509301 ) ) ;
#17482 = CARTESIAN_POINT ( 'NONE',  ( 0.5832655196449142432, 10.64987127965799374, 45.67072831365889840 ) ) ;
#17483 =( BOUNDED_SURFACE ( )  B_SPLINE_SURFACE ( 3, 1, ( 
 ( #33060, #28034 ),
 ( #4194, #37771 ),
 ( #18640, #56827 ),
 ( #38078, #28333 ) ),
 .UNSPECIFIED., .F., .F., .F. ) 
 B_SPLINE_SURFACE_WITH_KNOTS ( ( 4, 4 ),
 ( 2, 2 ),
 ( 0.000000000000000000, 1.000000000000000000 ),
 ( 0.000000000000000000, 1.000000000000000000 ),
 .UNSPECIFIED. ) 
 GEOMETRIC_REPRESENTATION_ITEM ( )  RATIONAL_B_SPLINE_SURFACE ( (
 ( 1.000000000000000000, 1.000000000000000000),
 ( 0.9754377213608244057, 0.9999580625633939235),
 ( 0.9754377213608244057, 0.9999580625633939235),
 ( 1.000000000000000000, 1.000000000000000000) ) ) 
 REPRESENTATION_ITEM ( '' )  SURFACE ( )  );
#17484 = B_SPLINE_CURVE_WITH_KNOTS ( 'NONE', 3,
 ( #39077, #34358, #4889, #14029, #58130, #56903 ),
 .UNSPECIFIED., .F., .F.,
 ( 4, 2, 4 ),
 ( 4.770489558936219510E-18, 0.0002291472222819935318, 0.0004582944445639822932 ),
 .UNSPECIFIED. ) ;
#17485 = CARTESIAN_POINT ( 'NONE',  ( 0.6041374136657475802, 48.10739871142803992, 0.1745662470646264230 ) ) ;
#17486 = DIRECTION ( 'NONE',  ( -0.000000000000000000, -1.000000000000000000, -0.000000000000000000 ) ) ;
#17487 = EDGE_CURVE ( 'NONE', #4699, #49434, #48296, .T. ) ;
#17488 = CARTESIAN_POINT ( 'NONE',  ( 0.3622758884714730732, -40.13994584881772454, -15.73321244754840720 ) ) ;
#17489 = LINE ( 'NONE', #40392, #54838 ) ;
#17490 = VECTOR ( 'NONE', #40628, 1000.000000000000000 ) ;
#17491 = CARTESIAN_POINT ( 'NONE',  ( 4.956445790443988031, 0.000000000000000000, 0.000000000000000000 ) ) ;
#17492 = EDGE_CURVE ( 'NONE', #47692, #25196, #457, .T. ) ;
#17493 = CARTESIAN_POINT ( 'NONE',  ( 2.528100132419514257, -40.87987497285956806, 9.544087218558223285 ) ) ;
#17494 = CARTESIAN_POINT ( 'NONE',  ( 4.060580049360325461, 17.32852353021683101, 40.38799285210804157 ) ) ;
#17495 = CIRCLE ( 'NONE', #45499, 2.041999999999999815 ) ;
#17496 = CARTESIAN_POINT ( 'NONE',  ( 0.5809828226811617480, 37.66417181417551774, 29.58751527316192664 ) ) ;
#17497 = CARTESIAN_POINT ( 'NONE',  ( 4.956445790443495092, 1.033212179477288384, -47.07940656732829865 ) ) ;
#17498 = ADVANCED_FACE ( 'NONE', ( #44750 ), #46056, .F. ) ;
#17499 =( BOUNDED_SURFACE ( )  B_SPLINE_SURFACE ( 3, 1, ( 
 ( #23571, #61760 ),
 ( #46475, #47386 ),
 ( #18273, #32996 ),
 ( #8859, #3521 ) ),
 .UNSPECIFIED., .F., .F., .F. ) 
 B_SPLINE_SURFACE_WITH_KNOTS ( ( 4, 4 ),
 ( 2, 2 ),
 ( 0.000000000000000000, 1.000000000000000000 ),
 ( 0.000000000000000000, 1.000000000000000000 ),
 .UNSPECIFIED. ) 
 GEOMETRIC_REPRESENTATION_ITEM ( )  RATIONAL_B_SPLINE_SURFACE ( (
 ( 1.000000000000000000, 1.000000000000000000),
 ( 0.7282232189291694135, 0.9929344683865672927),
 ( 0.7282232189291694135, 0.9929344683865672927),
 ( 1.000000000000000000, 1.000000000000000000) ) ) 
 REPRESENTATION_ITEM ( '' )  SURFACE ( )  );
#17500 = EDGE_LOOP ( 'NONE', ( #34785, #53259, #35351, #9191 ) ) ;
#17501 = CARTESIAN_POINT ( 'NONE',  ( 4.975610109902397937, -17.43163075979644816, -45.70106843599929647 ) ) ;
#17502 = CARTESIAN_POINT ( 'NONE',  ( 0.8760168074886960365, 47.56749362999704545, 7.161346975773865253 ) ) ;
#17503 = CARTESIAN_POINT ( 'NONE',  ( 5.917102823773431552, -11.93691330175288989, -16.18640846136587896 ) ) ;
#17504 = CARTESIAN_POINT ( 'NONE',  ( 0.6029443449137436017, -45.50214841125133347, -18.46873108645500494 ) ) ;
#17505 = VERTEX_POINT ( 'NONE', #1479 ) ;
#17506 = DIRECTION ( 'NONE',  ( 0.07906939808003034253, -0.4719801263061979002, -0.8780562571152528140 ) ) ;
#17507 = EDGE_CURVE ( 'NONE', #30486, #52564, #29692, .T. ) ;
#17508 = DIRECTION ( 'NONE',  ( -0.07836865515943411409, -0.9968932487286223942, 0.007886984708653930337 ) ) ;
#17509 = ORIENTED_EDGE ( 'NONE', *, *, #30916, .T. ) ;
#17510 = CIRCLE ( 'NONE', #35544, 47.09074272231896430 ) ;
#17511 = CARTESIAN_POINT ( 'NONE',  ( 0.6064782688330897509, 37.24103942229884012, -28.50332312495426734 ) ) ;
#17512 = VERTEX_POINT ( 'NONE', #1176 ) ;
#17513 = DIRECTION ( 'NONE',  ( 0.1024043820194936588, 0.6940285268068309144, -0.7126273545981417490 ) ) ;
#17514 = B_SPLINE_CURVE_WITH_KNOTS ( 'NONE', 3,
 ( #52589, #9682, #45388, #16246 ),
 .UNSPECIFIED., .F., .F.,
 ( 4, 4 ),
 ( 8.777083671441753062E-17, 0.005004741218457508210 ),
 .UNSPECIFIED. ) ;
#17515 = ORIENTED_EDGE ( 'NONE', *, *, #60803, .F. ) ;
#17516 = CARTESIAN_POINT ( 'NONE',  ( -6.017396004339687465, -7.209881890566424367, -17.40926186480786697 ) ) ;
#17517 = ORIENTED_EDGE ( 'NONE', *, *, #46428, .F. ) ;
#17518 = CARTESIAN_POINT ( 'NONE',  ( 1.000110580585053643, 35.71937538688245439, 21.92130709476230876 ) ) ;
#17519 = CARTESIAN_POINT ( 'NONE',  ( 4.967162193818130511, -36.06913038482782952, -23.56777426397217567 ) ) ;
#17520 = ORIENTED_EDGE ( 'NONE', *, *, #39480, .F. ) ;
#17521 = CARTESIAN_POINT ( 'NONE',  ( 4.975801465491694664, -42.71626295676247764, -21.70134120755185947 ) ) ;
#17522 = ORIENTED_EDGE ( 'NONE', *, *, #25992, .F. ) ;
#17523 = CARTESIAN_POINT ( 'NONE',  ( 0.5819845901640492425, -37.72030663501136871, -29.51612926147656069 ) ) ;
#17524 = CIRCLE ( 'NONE', #40529, 0.1000000000000002554 ) ;
#17525 = ORIENTED_EDGE ( 'NONE', *, *, #60788, .F. ) ;
#17526 = VERTEX_POINT ( 'NONE', #6471 ) ;
#17527 = CARTESIAN_POINT ( 'NONE',  ( 5.896782393890504181, -15.78060201202815094, -12.46991126736615385 ) ) ;
#17528 = CARTESIAN_POINT ( 'NONE',  ( 4.549368137175248350, 0.000000000000000000, 0.000000000000000000 ) ) ;
#17529 = DIRECTION ( 'NONE',  ( -0.07906939808003035641, -0.4122784474075915084, 0.9076202466287580650 ) ) ;
#17530 = AXIS2_PLACEMENT_3D ( 'NONE', #53533, #58538, #33538 ) ;
#17531 = CARTESIAN_POINT ( 'NONE',  ( 4.553261556744875094, 1.182159483579356074, 43.91061448874314976 ) ) ;
#17532 = CARTESIAN_POINT ( 'NONE',  ( 0.6009452777970409887, 44.61081509289878966, 18.00606236585388231 ) ) ;
#17533 = VERTEX_POINT ( 'NONE', #34723 ) ;
#17534 = CARTESIAN_POINT ( 'NONE',  ( 0.7044674535453004927, 3.876803250506410947, -48.95684956538534038 ) ) ;
#17535 = EDGE_CURVE ( 'NONE', #15999, #9808, #49728, .T. ) ;
#17536 = CARTESIAN_POINT ( 'NONE',  ( 0.9780106845699469975, -17.92479137380018273, 37.88183074590216393 ) ) ;
#17537 = CARTESIAN_POINT ( 'NONE',  ( 0.5806925824938494740, -34.41156632303759011, 31.86010774524702072 ) ) ;
#17538 = VECTOR ( 'NONE', #30216, 1000.000000000000000 ) ;
#17539 = VERTEX_POINT ( 'NONE', #34414 ) ;
#17540 = EDGE_CURVE ( 'NONE', #45338, #58089, #22899, .T. ) ;
#17541 = EDGE_LOOP ( 'NONE', ( #17594, #15598, #59008, #50425 ) ) ;
#17542 = CARTESIAN_POINT ( 'NONE',  ( -6.016761891674564211, 18.84319130225482297, -0.003433883959849463787 ) ) ;
#17543 = CARTESIAN_POINT ( 'NONE',  ( 4.962356264823593044, 27.50309822711036034, 31.85616401534038644 ) ) ;
#17544 = CARTESIAN_POINT ( 'NONE',  ( 0.3622758884714730732, -42.62881903538215056, 6.444611261693867554 ) ) ;
#17545 = VERTEX_POINT ( 'NONE', #10291 ) ;
#17546 = DIRECTION ( 'NONE',  ( -0.1024043820194934507, 0.9239750460186177961, -0.3684880688409037930 ) ) ;
#17547 = CARTESIAN_POINT ( 'NONE',  ( 4.390527457369401532, -33.66034041506548391, 28.23414280212042371 ) ) ;
#17548 = EDGE_CURVE ( 'NONE', #33299, #38729, #18461, .T. ) ;
#17549 = EDGE_CURVE ( 'NONE', #57870, #35220, #21281, .T. ) ;
#17550 = ORIENTED_EDGE ( 'NONE', *, *, #256, .T. ) ;
#17551 = CARTESIAN_POINT ( 'NONE',  ( 1.231276596079881047, -37.78837162824498819, 18.14705873423338289 ) ) ;
#17552 = ORIENTED_EDGE ( 'NONE', *, *, #41420, .T. ) ;
#17553 = ADVANCED_FACE ( 'NONE', ( #20017 ), #22060, .F. ) ;
#17554 = FACE_OUTER_BOUND ( 'NONE', #47474, .T. ) ;
#17555 = CARTESIAN_POINT ( 'NONE',  ( 0.8560838555295223751, -44.00447048317975174, 16.24744323198866169 ) ) ;
#17556 = B_SPLINE_CURVE_WITH_KNOTS ( 'NONE', 3,
 ( #1681, #50471, #34616, #25502, #7542, #26666, #17588, #36403, #22286, #6367, #53996, #53682, #50772, #17282, #21981, #44048, #12593, #34934, #29590, #10813, #31685, #46112, #24912, #60781, #12901 ),
 .UNSPECIFIED., .F., .F.,
 ( 4, 3, 3, 3, 3, 3, 3, 3, 4 ),
 ( 4.670885906470169154E-18, 0.0005656085177311400737, 0.001131215744874499622, 0.001696821861372766567, 0.002262427090022498151, 0.002828031679238746359, 0.003393635864401605730, 0.003977030878808132490, 0.004561030005651159867 ),
 .UNSPECIFIED. ) ;
#17557 = CARTESIAN_POINT ( 'NONE',  ( 4.553261556744875094, -43.15908619232990873, 8.175135770534621926 ) ) ;
#17558 = CARTESIAN_POINT ( 'NONE',  ( 0.8557997880470697982, 13.27832040216639520, 46.03118133706031045 ) ) ;
#17559 = B_SPLINE_CURVE_WITH_KNOTS ( 'NONE', 3,
 ( #26062, #51316, #2232, #13437 ),
 .UNSPECIFIED., .F., .F.,
 ( 4, 4 ),
 ( 0.000000000000000000, 0.004445488388166990781 ),
 .UNSPECIFIED. ) ;
#17560 = EDGE_CURVE ( 'NONE', #21995, #33629, #34114, .T. ) ;
#17561 = VERTEX_POINT ( 'NONE', #30611 ) ;
#17562 = DIRECTION ( 'NONE',  ( 0.000000000000000000, 0.000000000000000000, -1.000000000000000000 ) ) ;
#17563 = CARTESIAN_POINT ( 'NONE',  ( 5.901764892641288895, 47.35677775444521131, -12.46302804922470386 ) ) ;
#17564 = EDGE_CURVE ( 'NONE', #54294, #29266, #8676, .T. ) ;
#17565 = CARTESIAN_POINT ( 'NONE',  ( 0.5807400328401637335, 6.791881299636274072, -47.41494605191435596 ) ) ;
#17566 = CARTESIAN_POINT ( 'NONE',  ( -6.078075953587585900, -1.854308114362783311, -19.16655200248976243 ) ) ;
#17567 = CARTESIAN_POINT ( 'NONE',  ( 0.9730545539215883499, 37.40983423658502716, -21.01499094264509893 ) ) ;
#17568 = CARTESIAN_POINT ( 'NONE',  ( 0.6064515330803547100, 32.08788281977977164, -34.20090806076890289 ) ) ;
#17569 = CARTESIAN_POINT ( 'NONE',  ( 0.7764139734771289270, -38.15852734697478610, -27.27576326369334581 ) ) ;
#17570 = LINE ( 'NONE', #51989, #34137 ) ;
#17571 = FACE_OUTER_BOUND ( 'NONE', #29357, .T. ) ;
#17572 = CARTESIAN_POINT ( 'NONE',  ( 0.09136607875274982415, 0.000000000000000000, 0.000000000000000000 ) ) ;
#17573 = EDGE_LOOP ( 'NONE', ( #5452, #14586, #52896, #41125 ) ) ;
#17574 = CARTESIAN_POINT ( 'NONE',  ( 4.335381028904201628, -48.94118403004391382, -2.125406643849441224 ) ) ;
#17575 = AXIS2_PLACEMENT_3D ( 'NONE', #24916, #35244, #16128 ) ;
#17576 = CARTESIAN_POINT ( 'NONE',  ( 1.500000000000001332, 0.000000000000000000, 0.000000000000000000 ) ) ;
#17577 = CARTESIAN_POINT ( 'NONE',  ( 4.549368137175248350, 2.596185425821941894, -42.84816078363927971 ) ) ;
#17578 = CARTESIAN_POINT ( 'NONE',  ( 5.331200000000000827, 0.000000000000000000, 0.000000000000000000 ) ) ;
#17579 = VERTEX_POINT ( 'NONE', #38820 ) ;
#17580 = DIRECTION ( 'NONE',  ( -1.807003620809173399E-16, 1.000000000000000000, 0.000000000000000000 ) ) ;
#17581 = VECTOR ( 'NONE', #5943, 1000.000000000000114 ) ;
#17582 = CARTESIAN_POINT ( 'NONE',  ( 0.9791128995231621612, -41.81543299240070155, -2.794100553704363055 ) ) ;
#17583 = EDGE_CURVE ( 'NONE', #12277, #226, #15463, .T. ) ;
#17584 = ORIENTED_EDGE ( 'NONE', *, *, #47334, .F. ) ;
#17585 = CARTESIAN_POINT ( 'NONE',  ( 0.1155031312995260795, 4.404628064233996554, -43.90376845041404152 ) ) ;
#17586 = EDGE_CURVE ( 'NONE', #28808, #50125, #28106, .T. ) ;
#17587 = CARTESIAN_POINT ( 'NONE',  ( 5.896782393890504181, -18.51439742298342139, 7.857682542699045314 ) ) ;
#17588 = CARTESIAN_POINT ( 'NONE',  ( 3.559346040607745287, -10.52814864373571524, 42.69178337429104886 ) ) ;
#17589 = ORIENTED_EDGE ( 'NONE', *, *, #29484, .F. ) ;
#17590 = CARTESIAN_POINT ( 'NONE',  ( 0.6009452777970413218, 29.63106797105363555, 37.89911497740580870 ) ) ;
#17591 = ORIENTED_EDGE ( 'NONE', *, *, #47014, .T. ) ;
#17592 = ORIENTED_EDGE ( 'NONE', *, *, #26720, .F. ) ;
#17593 = CARTESIAN_POINT ( 'NONE',  ( -6.077587904424778920, 7.788877841491745002, 17.61049128685084142 ) ) ;
#17594 = ORIENTED_EDGE ( 'NONE', *, *, #28272, .F. ) ;
#17595 = CARTESIAN_POINT ( 'NONE',  ( 0.5998501479064708430, 41.92175333043619645, -23.59887241503310307 ) ) ;
#17596 = ORIENTED_EDGE ( 'NONE', *, *, #7977, .F. ) ;
#17597 = CARTESIAN_POINT ( 'NONE',  ( 0.8760168074887090262, -42.09738177923938451, -23.27577685234583527 ) ) ;
#17598 = B_SPLINE_CURVE_WITH_KNOTS ( 'NONE', 3,
 ( #1318, #34875, #1022, #53943 ),
 .UNSPECIFIED., .F., .F.,
 ( 4, 4 ),
 ( 0.000000000000000000, 0.004447772540403845815 ),
 .UNSPECIFIED. ) ;
#17599 =( BOUNDED_SURFACE ( )  B_SPLINE_SURFACE ( 3, 1, ( 
 ( #22406, #45611 ),
 ( #36525, #55591 ),
 ( #3275, #7671 ),
 ( #21174, #26797 ) ),
 .UNSPECIFIED., .F., .F., .F. ) 
 B_SPLINE_SURFACE_WITH_KNOTS ( ( 4, 4 ),
 ( 2, 2 ),
 ( 0.000000000000000000, 1.000000000000000000 ),
 ( 0.000000000000000000, 1.000000000000000000 ),
 .UNSPECIFIED. ) 
 GEOMETRIC_REPRESENTATION_ITEM ( )  RATIONAL_B_SPLINE_SURFACE ( (
 ( 1.000000000000000000, 1.000000000000000000),
 ( 0.9953390228620291325, 0.8624445117761032620),
 ( 0.9953390228620291325, 0.8624445117761032620),
 ( 1.000000000000000000, 1.000000000000000000) ) ) 
 REPRESENTATION_ITEM ( '' )  SURFACE ( )  );
#17600 = CARTESIAN_POINT ( 'NONE',  ( 0.8751705887134553219, 17.57879340691544101, -44.76769609654218129 ) ) ;
#17601 = ORIENTED_EDGE ( 'NONE', *, *, #23551, .T. ) ;
#17602 = CARTESIAN_POINT ( 'NONE',  ( 0.1155031312995260795, 15.08069845605273329, 41.46702505135155548 ) ) ;
#17603 = CARTESIAN_POINT ( 'NONE',  ( 5.910764540655178756, 20.06833201846864512, 1.327888724882238414 ) ) ;
#17604 = CARTESIAN_POINT ( 'NONE',  ( 1.296416391601053153, -37.84290377757003654, 22.58809438083998700 ) ) ;
#17605 = CARTESIAN_POINT ( 'NONE',  ( 0.8557997880470606944, 19.17299735372068525, -43.90420959842161608 ) ) ;
#17606 = ORIENTED_EDGE ( 'NONE', *, *, #28160, .T. ) ;
#17607 = CARTESIAN_POINT ( 'NONE',  ( 0.5839879327111939800, 44.28486549479623591, 18.24507200299058951 ) ) ;
#17608 = ORIENTED_EDGE ( 'NONE', *, *, #42674, .F. ) ;
#17609 = CARTESIAN_POINT ( 'NONE',  ( 4.549368137175248350, -42.06008734272402450, 8.582197505783685898 ) ) ;
#17610 = EDGE_CURVE ( 'NONE', #14671, #58860, #5653, .T. ) ;
#17611 = ORIENTED_EDGE ( 'NONE', *, *, #59120, .T. ) ;
#17612 = CARTESIAN_POINT ( 'NONE',  ( 0.1147471544378677322, -12.25660023001551124, 42.38782772536036703 ) ) ;
#17613 = CARTESIAN_POINT ( 'NONE',  ( 0.7413678028165009426, 14.35015966441118529, -41.69603109860877765 ) ) ;
#17614 = ORIENTED_EDGE ( 'NONE', *, *, #56055, .F. ) ;
#17615 = LINE ( 'NONE', #46443, #56552 ) ;
#17616 = CARTESIAN_POINT ( 'NONE',  ( 0.3676999524040323597, 42.11837424242189343, -13.11461530118710428 ) ) ;
#17617 = CARTESIAN_POINT ( 'NONE',  ( 0.5997462898726536595, 28.52220283460625438, 39.97543715340569292 ) ) ;
#17618 = CARTESIAN_POINT ( 'NONE',  ( 0.5834584762367764910, -1.385012569902221991, -46.87555577477881741 ) ) ;
#17619 = EDGE_CURVE ( 'NONE', #4129, #48896, #2009, .T. ) ;
#17621 = ORIENTED_EDGE ( 'NONE', *, *, #37692, .F. ) ;
#17620 = AXIS2_PLACEMENT_3D ( 'NONE', #22674, #41806, #26751 ) ;
#17622 = ORIENTED_EDGE ( 'NONE', *, *, #37151, .T. ) ;
#17623 = CARTESIAN_POINT ( 'NONE',  ( 4.962356264823608143, 12.05238263218917716, 40.32338863178108568 ) ) ;
#17624 = EDGE_CURVE ( 'NONE', #11002, #45408, #22461, .T. ) ;
#17625 = CARTESIAN_POINT ( 'NONE',  ( 0.6845945791218034371, 46.90049452736489854, 0.8661026512829932411 ) ) ;
#17626 = CARTESIAN_POINT ( 'NONE',  ( -6.017396004339686577, -16.31924478664268463, -9.420565012089598511 ) ) ;
#17627 = AXIS2_PLACEMENT_3D ( 'NONE', #52137, #47454, #9228 ) ;
#17628 = CARTESIAN_POINT ( 'NONE',  ( 4.956445790444002242, -43.14021684453514638, 18.88014143872134554 ) ) ;
#17629 = CARTESIAN_POINT ( 'NONE',  ( 0.3622758884714600280, -0.8252992914331080954, 43.10531414739104150 ) ) ;
#17630 = CARTESIAN_POINT ( 'NONE',  ( 9.999999999999994671, 56.56854249492371878, 56.56854249492391062 ) ) ;
#17631 = AXIS2_PLACEMENT_3D ( 'NONE', #56608, #21881, #8078 ) ;
#17632 = CARTESIAN_POINT ( 'NONE',  ( -6.077587904424778920, -19.21689618909966413, -1.227567615774088017 ) ) ;
#17633 = CARTESIAN_POINT ( 'NONE',  ( 4.549368137175248350, 0.000000000000000000, 0.000000000000000000 ) ) ;
#17634 = CARTESIAN_POINT ( 'NONE',  ( 0.9790320750461898314, 32.83655567964974864, 26.04030997587112850 ) ) ;
#17635 = CARTESIAN_POINT ( 'NONE',  ( -2.708315649062916552, -1.648584381067149218, 14.54141329178159303 ) ) ;
#17636 = CARTESIAN_POINT ( 'NONE',  ( 5.896278296736517710, -18.51903684540627282, 7.846798960905577935 ) ) ;
#17637 = DIRECTION ( 'NONE',  ( 0.000000000000000000, 0.000000000000000000, 1.000000000000000000 ) ) ;
#17638 = DIRECTION ( 'NONE',  ( 0.000000000000000000, 0.000000000000000000, 1.000000000000000000 ) ) ;
#17639 = CARTESIAN_POINT ( 'NONE',  ( 1.129531546211701931, 0.000000000000000000, -6.887500000000022382 ) ) ;
#17640 = CARTESIAN_POINT ( 'NONE',  ( 0.6846871229502899947, -23.20185915381586383, 41.91507847151790855 ) ) ;
#17641 = CARTESIAN_POINT ( 'NONE',  ( 0.8560838555295223751, -14.76796170096679894, -44.52280473286144513 ) ) ;
#17642 = CARTESIAN_POINT ( 'NONE',  ( 0.6029443449137436017, -47.51238410865360606, 12.41422145344172101 ) ) ;
#17644 = ORIENTED_EDGE ( 'NONE', *, *, #2633, .T. ) ;
#17643 = CARTESIAN_POINT ( 'NONE',  ( 0.9749527285493317930, 39.53206838353044361, 16.68386601451053508 ) ) ;
#17646 = ORIENTED_EDGE ( 'NONE', *, *, #50700, .F. ) ;
#17645 = B_SPLINE_CURVE_WITH_KNOTS ( 'NONE', 3,
 ( #13436, #51013, #8105, #3388 ),
 .UNSPECIFIED., .F., .F.,
 ( 4, 4 ),
 ( 0.000000000000000000, 0.005013413432710149380 ),
 .UNSPECIFIED. ) ;
#17647 = CARTESIAN_POINT ( 'NONE',  ( -6.078726893082806448, 13.83492043373111180, -13.39361854993076406 ) ) ;
#17648 = DIRECTION ( 'NONE',  ( -1.000000000000000000, -0.000000000000000000, -0.000000000000000000 ) ) ;
#17649 = CARTESIAN_POINT ( 'NONE',  ( 0.5987334308729317378, 44.50372324553362802, 20.76009450495541486 ) ) ;
#17650 = ORIENTED_EDGE ( 'NONE', *, *, #38858, .T. ) ;
#17651 = ORIENTED_EDGE ( 'NONE', *, *, #38375, .F. ) ;
#17652 = DIRECTION ( 'NONE',  ( 0.1024043820194936311, 0.8679729669084546018, 0.4859385467930489311 ) ) ;
#17653 = CARTESIAN_POINT ( 'NONE',  ( 0.8751705887134553219, 37.60752970653828697, -29.98056538504921065 ) ) ;
#17654 = ORIENTED_EDGE ( 'NONE', *, *, #25784, .F. ) ;
#17655 = ORIENTED_EDGE ( 'NONE', *, *, #20203, .F. ) ;
#17656 = EDGE_CURVE ( 'NONE', #61378, #4827, #55335, .T. ) ;
#17657 = CARTESIAN_POINT ( 'NONE',  ( 0.9762797500689124330, -37.62962005162918899, 18.44821075214967721 ) ) ;
#17658 = CIRCLE ( 'NONE', #52652, 48.09070567114147110 ) ;
#17659 = CARTESIAN_POINT ( 'NONE',  ( 5.958863334805807099, -18.96369761673814835, -7.853699934219834589 ) ) ;
#17660 = CONICAL_SURFACE ( 'NONE', #56635, 43.08621763946400307, 1.568696531533066763 ) ;
#17661 = CARTESIAN_POINT ( 'NONE',  ( 6.189768672337906175, 1.091423221261470733, -2.362915713819767774E-16 ) ) ;
#17662 = AXIS2_PLACEMENT_3D ( 'NONE', #23616, #52415, #53337 ) ;
#17663 = ORIENTED_EDGE ( 'NONE', *, *, #54318, .T. ) ;
#17664 = CARTESIAN_POINT ( 'NONE',  ( 0.1129192098497455998, -17.41650932123162931, -40.54154647825617275 ) ) ;
#17665 = CARTESIAN_POINT ( 'NONE',  ( 2.282816707992309624, -41.31566379231499297, 22.34978505060748333 ) ) ;
#17666 =( BOUNDED_SURFACE ( )  B_SPLINE_SURFACE ( 3, 1, ( 
 ( #41914, #37209 ),
 ( #60981, #26553 ),
 ( #18090, #30949 ),
 ( #7111, #36282 ) ),
 .UNSPECIFIED., .F., .F., .F. ) 
 B_SPLINE_SURFACE_WITH_KNOTS ( ( 4, 4 ),
 ( 2, 2 ),
 ( 0.000000000000000000, 1.000000000000000000 ),
 ( 0.000000000000000000, 1.000000000000000000 ),
 .UNSPECIFIED. ) 
 GEOMETRIC_REPRESENTATION_ITEM ( )  RATIONAL_B_SPLINE_SURFACE ( (
 ( 1.000000000000000000, 1.000000000000000000),
 ( 0.9732289882329797637, 0.9999525324661233672),
 ( 0.9732289882329797637, 0.9999525324661233672),
 ( 1.000000000000000000, 1.000000000000000000) ) ) 
 REPRESENTATION_ITEM ( '' )  SURFACE ( )  );
#17667 = CARTESIAN_POINT ( 'NONE',  ( 0.8560838555295158248, -45.77741231505087427, -10.23725333375899105 ) ) ;
#17668 = ORIENTED_EDGE ( 'NONE', *, *, #9339, .F. ) ;
#17669 = CIRCLE ( 'NONE', #2624, 48.91267123290010943 ) ;
#17670 = ORIENTED_EDGE ( 'NONE', *, *, #29056, .F. ) ;
#17671 = CARTESIAN_POINT ( 'NONE',  ( 0.1129192098497455998, 39.54191224844618802, 19.58032082273768637 ) ) ;
#17672 = EDGE_LOOP ( 'NONE', ( #45157, #1171, #45256, #58887 ) ) ;
#17673 = CARTESIAN_POINT ( 'NONE',  ( 4.967162193818130511, -42.16965968614187688, -8.839793687085657936 ) ) ;
#17674 = CARTESIAN_POINT ( 'NONE',  ( 2.643462169533600914, -1.382267876918794602, 48.01657676222234983 ) ) ;
#17675 = CARTESIAN_POINT ( 'NONE',  ( -1.200000000000006617, 0.000000000000000000, -6.887500000000022382 ) ) ;
#17676 = CARTESIAN_POINT ( 'NONE',  ( 0.5987334308729318488, -30.14260565354317123, 38.76836636982163498 ) ) ;
#17677 = CARTESIAN_POINT ( 'NONE',  ( 0.5997462898726536595, -48.63480578518795738, -6.797594896826151256 ) ) ;
#17678 = EDGE_CURVE ( 'NONE', #54789, #50134, #45269, .T. ) ;
#17679 = B_SPLINE_CURVE_WITH_KNOTS ( 'NONE', 3,
 ( #51561, #61270, #5407, #43362, #51879, #18388, #43677, #34567, #22768, #24537, #28086, #32804, #57717, #717, #38972, #3946, #58030, #15152, #5097 ),
 .UNSPECIFIED., .F., .F.,
 ( 4, 3, 3, 3, 3, 3, 4 ),
 ( 1.355252715606880543E-20, 0.0002612768053151719259, 0.0003919133833142912507, 0.0005225499612322561998, 0.0006531865391693348743, 0.0008112755173415194237, 0.0009693688056799674773 ),
 .UNSPECIFIED. ) ;
#17680 = ORIENTED_EDGE ( 'NONE', *, *, #29634, .F. ) ;
#17681 = CARTESIAN_POINT ( 'NONE',  ( -6.077587904424778920, 12.00112336472187025, -15.05885318935865236 ) ) ;
#17682 = AXIS2_PLACEMENT_3D ( 'NONE', #28407, #23719, #38154 ) ;
#17683 = DIRECTION ( 'NONE',  ( -1.000000000000000000, -3.135800716341471541E-16, -1.298891185607920445E-16 ) ) ;
#17684 = EDGE_CURVE ( 'NONE', #21167, #59165, #57256, .T. ) ;
#17685 = CARTESIAN_POINT ( 'NONE',  ( 4.335381028904201628, -9.909170555161033178, 47.97463065593183273 ) ) ;
#17686 = VERTEX_POINT ( 'NONE', #3330 ) ;
#17687 = CARTESIAN_POINT ( 'NONE',  ( 1.092182651088184242, -34.99132997457212468, -23.07310146150473074 ) ) ;
#17688 = EDGE_CURVE ( 'NONE', #46133, #61654, #43106, .T. ) ;
#17689 = CARTESIAN_POINT ( 'NONE',  ( 5.896278296736517710, 12.98960347168532259, -15.35568888922813180 ) ) ;
#17690 = CARTESIAN_POINT ( 'NONE',  ( 4.967162193818130511, 14.26841313271336809, -40.65506779172149976 ) ) ;
#17691 = CARTESIAN_POINT ( 'NONE',  ( 0.5980271706414711508, -34.78940872470953849, -34.66621241824330468 ) ) ;
#17692 = VERTEX_POINT ( 'NONE', #60652 ) ;
#17693 = B_SPLINE_CURVE_WITH_KNOTS ( 'NONE', 3,
 ( #60065, #36284, #50059, #55352, #41299, #55662, #12792, #12474, #55975, #27175, #50659, #35983, #36910, #41599, #32190, #31883, #50968, #8357, #35673 ),
 .UNSPECIFIED., .F., .F.,
 ( 4, 3, 3, 3, 3, 3, 4 ),
 ( 1.149162571898268292E-16, 0.0002618519381806262963, 0.0003927759815485972221, 0.0005237000248299437553, 0.0006546240681324991262, 0.0007855481115631330344, 0.0009699050456655103998 ),
 .UNSPECIFIED. ) ;
#17694 = LINE ( 'NONE', #49967, #58863 ) ;
#17695 = EDGE_CURVE ( 'NONE', #35106, #56156, #45328, .T. ) ;
#17696 = CARTESIAN_POINT ( 'NONE',  ( 4.975801465491694664, 8.787181743659507660, 47.10002938642145409 ) ) ;
#17697 = CARTESIAN_POINT ( 'NONE',  ( 0.7057020205115017708, -0.8412108057956128038, 47.89404687311021291 ) ) ;
#17698 = CARTESIAN_POINT ( 'NONE',  ( 0.7948878604505658085, -14.79943965969628117, -46.81533117534708310 ) ) ;
#17699 = CARTESIAN_POINT ( 'NONE',  ( 0.5837800005270559200, -46.79127812546623488, 3.132339385674594467 ) ) ;
#17700 = CARTESIAN_POINT ( 'NONE',  ( 2.528100132419516477, -23.59890196031982157, -34.71808757548846103 ) ) ;
#17701 = CARTESIAN_POINT ( 'NONE',  ( 0.9752570700956793015, -5.371905812151864801, -42.57087745267996581 ) ) ;
#17702 = DIRECTION ( 'NONE',  ( -1.000000000000000000, -3.673819061467147552E-16, 1.925929944387234758E-32 ) ) ;
#17703 = CIRCLE ( 'NONE', #42705, 10.00000000000000000 ) ;
#17704 = CARTESIAN_POINT ( 'NONE',  ( 0.6021447746440204973, 41.01325366509355064, -27.00840911440690206 ) ) ;
#17705 = DIRECTION ( 'NONE',  ( 0.000000000000000000, 0.000000000000000000, 1.000000000000000000 ) ) ;
#17707 = ORIENTED_EDGE ( 'NONE', *, *, #700, .F. ) ;
#17706 = EDGE_CURVE ( 'NONE', #15748, #59402, #27434, .T. ) ;
#17708 = AXIS2_PLACEMENT_3D ( 'NONE', #59654, #59035, #44369 ) ;
#17709 = CARTESIAN_POINT ( 'NONE',  ( 0.8551540677456715978, -41.94570365541186874, -23.16399837394590122 ) ) ;
#17710 = FACE_OUTER_BOUND ( 'NONE', #6472, .T. ) ;
#17712 = EDGE_CURVE ( 'NONE', #15568, #27320, #3452, .T. ) ;
#17711 = DIRECTION ( 'NONE',  ( 0.000000000000000000, 0.000000000000000000, 1.000000000000000000 ) ) ;
#17713 = CARTESIAN_POINT ( 'NONE',  ( 0.8751705887134423323, -5.393078191592370452, -47.79200036674278351 ) ) ;
#17714 = B_SPLINE_CURVE_WITH_KNOTS ( 'NONE', 3,
 ( #26403, #49910, #35521, #11709, #6035, #6965 ),
 .UNSPECIFIED., .F., .F.,
 ( 4, 2, 4 ),
 ( 8.583542049204266310E-17, 0.0002293366620881449576, 0.0004586733241762040465 ),
 .UNSPECIFIED. ) ;
#17715 = CARTESIAN_POINT ( 'NONE',  ( 4.553261556744875094, -24.94552653848424129, -36.15605442441715667 ) ) ;
#17716 = CARTESIAN_POINT ( 'NONE',  ( 0.7245667037590787229, 17.64710816761261114, -44.74806999162972687 ) ) ;
#17717 = APPLICATION_PROTOCOL_DEFINITION ( 'draft international standard', 'automotive_design', 1998, #39569 ) ;
#17718 = CARTESIAN_POINT ( 'NONE',  ( 0.6025881611877910160, -44.52856035602921736, 18.20817581200337898 ) ) ;
#17719 = CARTESIAN_POINT ( 'NONE',  ( 0.5809828226811553087, 12.92184523170202937, 46.11980934799343856 ) ) ;
#17720 = CIRCLE ( 'NONE', #32752, 47.91270532121795611 ) ;
#17721 = CARTESIAN_POINT ( 'NONE',  ( 2.282803330402969344, -18.57323392456551758, -43.14547356375118170 ) ) ;
#17723 = ORIENTED_EDGE ( 'NONE', *, *, #45861, .F. ) ;
#17722 = CARTESIAN_POINT ( 'NONE',  ( 5.901463166500145796, -18.51103891486766173, -7.865068889265479868 ) ) ;
#17724 = EDGE_LOOP ( 'NONE', ( #38967, #4478, #27600, #57288 ) ) ;
#17725 = CARTESIAN_POINT ( 'NONE',  ( 1.112077966505211624, -18.79777896220841882, -39.87071395418583819 ) ) ;
#17726 = CARTESIAN_POINT ( 'NONE',  ( 0.5837157313716023754, -7.889940358524325958, 46.22754487014157121 ) ) ;
#17727 = CARTESIAN_POINT ( 'NONE',  ( 3.678834586032786458, -9.636421247177533900, 48.01824398262914428 ) ) ;
#17728 = ORIENTED_EDGE ( 'NONE', *, *, #120, .F. ) ;
#17729 = CARTESIAN_POINT ( 'NONE',  ( 0.5807400328401574052, -12.92266817605982432, -46.12278621143511259 ) ) ;
#17730 = CARTESIAN_POINT ( 'NONE',  ( 3.238018933889920792, 12.43622092696273107, 4.974726266180598877 ) ) ;
#17731 = CARTESIAN_POINT ( 'NONE',  ( 0.1092355843206037486, 5.926758618547972368, -42.71527351115373961 ) ) ;
#17732 = ORIENTED_EDGE ( 'NONE', *, *, #26461, .F. ) ;
#17733 = VERTEX_POINT ( 'NONE', #48047 ) ;
#17734 = EDGE_CURVE ( 'NONE', #30064, #57079, #35682, .T. ) ;
#17735 = CARTESIAN_POINT ( 'NONE',  ( 0.9736507210033049642, 41.32746151989300643, 11.54000710819829045 ) ) ;
#17736 = CARTESIAN_POINT ( 'NONE',  ( 2.009741617377216460, 37.63911818071238002, 22.86483894982449527 ) ) ;
#17737 = DIRECTION ( 'NONE',  ( -1.000000000000000000, -3.135800716341489291E-16, 1.298891185607901956E-16 ) ) ;
#17738 = DIRECTION ( 'NONE',  ( -0.07439287786467652097, -0.3937848822959301165, -0.9161872986448742484 ) ) ;
#17739 = CARTESIAN_POINT ( 'NONE',  ( 0.6021447746440204973, 49.02259406747356962, 2.885551937531610545 ) ) ;
#17740 = FACE_OUTER_BOUND ( 'NONE', #7629, .T. ) ;
#17741 = CARTESIAN_POINT ( 'NONE',  ( 0.2885697896453112699, 11.93479333319024605, -41.43179225254754527 ) ) ;
#17742 = CIRCLE ( 'NONE', #4691, 72.00000000000002842 ) ;
#17743 = VERTEX_POINT ( 'NONE', #5705 ) ;
#17744 =( BOUNDED_SURFACE ( )  B_SPLINE_SURFACE ( 3, 1, ( 
 ( #21828, #45967 ),
 ( #51543, #27758 ),
 ( #37179, #56249 ),
 ( #17139, #40967 ) ),
 .UNSPECIFIED., .F., .F., .F. ) 
 B_SPLINE_SURFACE_WITH_KNOTS ( ( 4, 4 ),
 ( 2, 2 ),
 ( 0.000000000000000000, 1.000000000000000000 ),
 ( 0.000000000000000000, 1.000000000000000000 ),
 .UNSPECIFIED. ) 
 GEOMETRIC_REPRESENTATION_ITEM ( )  RATIONAL_B_SPLINE_SURFACE ( (
 ( 1.000000000000000000, 1.000000000000000000),
 ( 0.9953040768229005630, 0.8617119497784937465),
 ( 0.9953040768229005630, 0.8617119497784937465),
 ( 1.000000000000000000, 1.000000000000000000) ) ) 
 REPRESENTATION_ITEM ( '' )  SURFACE ( )  );
#17745 = CARTESIAN_POINT ( 'NONE',  ( 0.8557997880470606944, -34.51495345639572321, 33.22501220301889191 ) ) ;
#17746 = CARTESIAN_POINT ( 'NONE',  ( 0.6846871229502932144, -47.37786444808388353, -7.109010606687882650 ) ) ;
#17747 = CIRCLE ( 'NONE', #31747, 9.500000000000000000 ) ;
#17748 = ORIENTED_EDGE ( 'NONE', *, *, #20203, .T. ) ;
#17749 = CIRCLE ( 'NONE', #52745, 47.91270532121795611 ) ;
#17750 = CARTESIAN_POINT ( 'NONE',  ( 0.8744876279028263033, -20.68330519280349122, 44.52584571550372061 ) ) ;
#17751 = CARTESIAN_POINT ( 'NONE',  ( 0.1073791018717483448, 34.50606437925512182, 25.86618856530722610 ) ) ;
#17752 = CARTESIAN_POINT ( 'NONE',  ( 3.894904216938897878, 38.58700858884896689, -21.05153440109051388 ) ) ;
#17753 = CARTESIAN_POINT ( 'NONE',  ( 1.227938101723748288, -17.20315230597871903, 39.32113113558960293 ) ) ;
#17754 = EDGE_LOOP ( 'NONE', ( #5167, #59322 ) ) ;
#17755 = EDGE_LOOP ( 'NONE', ( #36945, #59876, #15538, #41636 ) ) ;
#17756 = CARTESIAN_POINT ( 'NONE',  ( 4.303969348037246512, 20.38638383586178904, -43.57722561725938704 ) ) ;
#17757 = CARTESIAN_POINT ( 'NONE',  ( 3.376099380956842921, -7.596917057716699340, -11.04514530688664564 ) ) ;
#17758 = EDGE_LOOP ( 'NONE', ( #16068, #59430, #5722, #11868 ) ) ;
#17759 = CARTESIAN_POINT ( 'NONE',  ( 3.661933894777891663, 18.64962327763467798, -43.18359314084413114 ) ) ;
#17760 = ORIENTED_EDGE ( 'NONE', *, *, #33779, .F. ) ;
#17761 = CARTESIAN_POINT ( 'NONE',  ( 0.000000000000000000, 0.000000000000000000, -1.199999999999999956 ) ) ;
#17762 = EDGE_CURVE ( 'NONE', #41953, #37050, #17679, .T. ) ;
#17763 = ORIENTED_EDGE ( 'NONE', *, *, #39263, .T. ) ;
#17764 = CARTESIAN_POINT ( 'NONE',  ( 3.221118495291109163, 43.49601572552855089, 6.546604896152265596 ) ) ;
#17765 = FACE_OUTER_BOUND ( 'NONE', #52317, .T. ) ;
#17766 =( BOUNDED_SURFACE ( )  B_SPLINE_SURFACE ( 3, 1, ( 
 ( #41931, #42243 ),
 ( #57514, #27807 ),
 ( #51918, #61606 ),
 ( #61303, #52525 ) ),
 .UNSPECIFIED., .F., .F., .F. ) 
 B_SPLINE_SURFACE_WITH_KNOTS ( ( 4, 4 ),
 ( 2, 2 ),
 ( 0.000000000000000000, 1.000000000000000000 ),
 ( 0.000000000000000000, 1.000000000000000000 ),
 .UNSPECIFIED. ) 
 GEOMETRIC_REPRESENTATION_ITEM ( )  RATIONAL_B_SPLINE_SURFACE ( (
 ( 1.000000000000000000, 1.000000000000000000),
 ( 0.9953040768229005630, 0.8617119497784937465),
 ( 0.9953040768229005630, 0.8617119497784937465),
 ( 1.000000000000000000, 1.000000000000000000) ) ) 
 REPRESENTATION_ITEM ( '' )  SURFACE ( )  );
#17767 = B_SPLINE_CURVE_WITH_KNOTS ( 'NONE', 3,
 ( #5946, #58576, #43293, #38287, #52347, #9437, #19476, #28539, #47664, #328, #4710, #30, #57337, #14777, #14471, #33578, #38593, #13087, #16013 ),
 .UNSPECIFIED., .F., .F.,
 ( 4, 3, 3, 3, 3, 3, 4 ),
 ( 9.813676791237319219E-18, 0.0002732106629380678530, 0.0004098138914053834551, 0.0005464171197651561222, 0.0006830203481512647648, 0.0008196235766963767518, 0.001011968216111142462 ),
 .UNSPECIFIED. ) ;
#17768 = CARTESIAN_POINT ( 'NONE',  ( 0.1152339509894530906, -43.73278499344712600, 5.863975372745715120 ) ) ;
#17769 = ORIENTED_EDGE ( 'NONE', *, *, #48499, .F. ) ;
#17770 = CARTESIAN_POINT ( 'NONE',  ( 0.1129192098497455998, 43.21532672376827833, 8.909956450124401073 ) ) ;
#17771 = EDGE_CURVE ( 'NONE', #11109, #10420, #24442, .T. ) ;
#17772 = DIRECTION ( 'NONE',  ( 0.000000000000000000, 0.000000000000000000, -1.000000000000000000 ) ) ;
#17773 =( BOUNDED_SURFACE ( )  B_SPLINE_SURFACE ( 3, 1, ( 
 ( #28621, #57114 ),
 ( #29240, #23624 ),
 ( #9516, #33045 ),
 ( #14857, #53344 ) ),
 .UNSPECIFIED., .F., .F., .F. ) 
 B_SPLINE_SURFACE_WITH_KNOTS ( ( 4, 4 ),
 ( 2, 2 ),
 ( 0.000000000000000000, 1.000000000000000000 ),
 ( 0.000000000000000000, 1.000000000000000000 ),
 .UNSPECIFIED. ) 
 GEOMETRIC_REPRESENTATION_ITEM ( )  RATIONAL_B_SPLINE_SURFACE ( (
 ( 1.000000000000000000, 1.000000000000000000),
 ( 0.7211978278499970862, 0.9934217856018976445),
 ( 0.7211978278499970862, 0.9934217856018976445),
 ( 1.000000000000000000, 1.000000000000000000) ) ) 
 REPRESENTATION_ITEM ( '' )  SURFACE ( )  );
#17774 = CARTESIAN_POINT ( 'NONE',  ( 0.5824936645240085253, -42.01860904020938392, 20.82485710314341532 ) ) ;
#17775 = B_SPLINE_CURVE_WITH_KNOTS ( 'NONE', 3,
 ( #26966, #45472, #55450, #16030 ),
 .UNSPECIFIED., .F., .F.,
 ( 4, 4 ),
 ( 0.000000000000000000, 0.004446090762761376394 ),
 .UNSPECIFIED. ) ;
#17776 = ORIENTED_EDGE ( 'NONE', *, *, #51022, .T. ) ;
#17777 = CARTESIAN_POINT ( 'NONE',  ( 0.7948884756798499929, -38.82350056502001223, -30.05718630341241848 ) ) ;
#17778 = CARTESIAN_POINT ( 'NONE',  ( 0.7762777257811890319, -7.133808567472593509, 47.37038525518532595 ) ) ;
#17779 = CARTESIAN_POINT ( 'NONE',  ( -6.000000000000004441, 15.72000000000000064, 0.000000000000000000 ) ) ;
#17780 = CARTESIAN_POINT ( 'NONE',  ( 0.5800708119828326126, 23.40241990038095921, -41.78924007434301302 ) ) ;
#17781 = VERTEX_POINT ( 'NONE', #43993 ) ;
#17782 = VECTOR ( 'NONE', #18110, 1000.000000000000000 ) ;
#17783 = CARTESIAN_POINT ( 'NONE',  ( 2.301430502907646058, 46.71331171933233151, -11.18388433759668743 ) ) ;
#17784 = DIRECTION ( 'NONE',  ( 0.000000000000000000, -0.7071067811865435759, -0.7071067811865514585 ) ) ;
#17785 = ORIENTED_EDGE ( 'NONE', *, *, #4051, .T. ) ;
#17786 = CARTESIAN_POINT ( 'NONE',  ( 0.6846871229502899947, 17.53234844287802474, -44.58493949243987942 ) ) ;
#17787 = CARTESIAN_POINT ( 'NONE',  ( -6.063463321072278589, -18.28058862190286149, 6.053142334046474282 ) ) ;
#17789 = EDGE_CURVE ( 'NONE', #8183, #45251, #53232, .T. ) ;
#17788 = CARTESIAN_POINT ( 'NONE',  ( 0.6845945791218034371, 3.832784513612765842, 46.75164471530551680 ) ) ;
#17790 = CARTESIAN_POINT ( 'NONE',  ( 1.088313998177382391, 41.64627086748865992, -10.35171213034648119 ) ) ;
#17791 = CARTESIAN_POINT ( 'NONE',  ( 1.231276596079887931, -37.78837162824473950, -18.14705873423390869 ) ) ;
#17792 = CARTESIAN_POINT ( 'NONE',  ( 4.975610109902397937, 34.73360008816130318, 34.43873447229810836 ) ) ;
#17793 = FACE_OUTER_BOUND ( 'NONE', #12830, .T. ) ;
#17794 = B_SPLINE_CURVE_WITH_KNOTS ( 'NONE', 3,
 ( #58004, #36332, #10425, #59480 ),
 .UNSPECIFIED., .F., .F.,
 ( 4, 4 ),
 ( 2.170598744017606518E-17, 0.004559932413162187670 ),
 .UNSPECIFIED. ) ;
#17795 = CARTESIAN_POINT ( 'NONE',  ( 2.624215991343620935, -11.05657803851078036, 46.71702075422648903 ) ) ;
#17796 = B_SPLINE_CURVE_WITH_KNOTS ( 'NONE', 3,
 ( #32849, #43412, #46328, #22813 ),
 .UNSPECIFIED., .F., .F.,
 ( 4, 4 ),
 ( 0.000000000000000000, 0.005013413432710145043 ),
 .UNSPECIFIED. ) ;
#17797 = CARTESIAN_POINT ( 'NONE',  ( -6.017396004339687465, -18.84316306185412415, -0.001173774849179927806 ) ) ;
#17798 = CARTESIAN_POINT ( 'NONE',  ( -6.078726893082806448, 13.83492043373091995, 13.39361854993096124 ) ) ;
#17799 = CARTESIAN_POINT ( 'NONE',  ( 0.1064266379913941102, -40.05351204369895868, -15.98292486309322769 ) ) ;
#17800 = CARTESIAN_POINT ( 'NONE',  ( 5.981074661064941900, 7.846517100474549977, 18.96560215432020158 ) ) ;
#17801 = AXIS2_PLACEMENT_3D ( 'NONE', #43929, #29474, #45163 ) ;
#17802 = CARTESIAN_POINT ( 'NONE',  ( 5.974727161628367256, -10.27590650342025214, -17.76736931401856623 ) ) ;
#17803 = CARTESIAN_POINT ( 'NONE',  ( 20.55500000000001748, 0.000000000000000000, 2.500000000000000888 ) ) ;
#17804 = CARTESIAN_POINT ( 'NONE',  ( 3.559346040607745287, 17.09700346547288063, 40.51077330838793245 ) ) ;
#17805 = PRODUCT_DEFINITION_SHAPE ( 'NONE', 'NONE',  #51660 ) ;
#17806 = LINE ( 'NONE', #27197, #56479 ) ;
#17807 = CARTESIAN_POINT ( 'NONE',  ( 0.5835871038041856584, 46.45916567184898582, 6.385951610933906508 ) ) ;
#17808 = CARTESIAN_POINT ( 'NONE',  ( 1.296416391601052265, 32.82713958318685599, -29.40554847069044442 ) ) ;
#17809 = ORIENTED_EDGE ( 'NONE', *, *, #14810, .F. ) ;
#17810 = DIRECTION ( 'NONE',  ( 0.000000000000000000, 0.000000000000000000, 1.000000000000000000 ) ) ;
#17811 = CARTESIAN_POINT ( 'NONE',  ( -6.010958268070873523, -18.68413620842262191, -2.445171577615958824 ) ) ;
#17813 = AXIS2_PLACEMENT_3D ( 'NONE', #14246, #33653, #61809 ) ;
#17812 = CARTESIAN_POINT ( 'NONE',  ( 7.000000000000006217, 1.285836671513502038E-15, -1.348150961071066192E-31 ) ) ;
#17814 = FACE_OUTER_BOUND ( 'NONE', #56413, .T. ) ;
#17815 = VERTEX_POINT ( 'NONE', #18079 ) ;
#17816 = EDGE_CURVE ( 'NONE', #24396, #27042, #49853, .T. ) ;
#17817 = CARTESIAN_POINT ( 'NONE',  ( 4.956653778116986153, -48.02038484091102077, 2.599733001514167086 ) ) ;
#17818 = EDGE_CURVE ( 'NONE', #29994, #54358, #47528, .T. ) ;
#17819 = CARTESIAN_POINT ( 'NONE',  ( 0.6029303876144825880, 24.16699908817961884, -41.59667219751857914 ) ) ;
#17820 = ORIENTED_EDGE ( 'NONE', *, *, #38482, .T. ) ;
#17821 = EDGE_CURVE ( 'NONE', #61623, #18115, #42994, .T. ) ;
#17822 = CARTESIAN_POINT ( 'NONE',  ( 3.390910168358336474, -25.85228378503758506, 35.57747264255177555 ) ) ;
#17823 = VECTOR ( 'NONE', #24405, 999.9999999999998863 ) ;
#17824 = VERTEX_POINT ( 'NONE', #48964 ) ;
#17825 = CARTESIAN_POINT ( 'NONE',  ( -6.072942160501519915, 12.01744408475423320, 15.04610248399318451 ) ) ;
#17826 = CARTESIAN_POINT ( 'NONE',  ( -0.6554360035617894376, 4.240386000424038571, -5.441324518471509997 ) ) ;
#17827 = EDGE_LOOP ( 'NONE', ( #60870, #49932, #25691, #4321 ) ) ;
#17828 = CARTESIAN_POINT ( 'NONE',  ( 10.00000000000001599, -56.56854249492410958, 56.56854249492351983 ) ) ;
#17829 = CARTESIAN_POINT ( 'NONE',  ( 0.5832366564991499081, -28.94058080282808376, 38.16363840618244296 ) ) ;
#17830 = ORIENTED_EDGE ( 'NONE', *, *, #28775, .F. ) ;
#17831 = CARTESIAN_POINT ( 'NONE',  ( 0.8744876279028306332, -43.20725972823464645, -23.31271664041680580 ) ) ;
#17832 = CARTESIAN_POINT ( 'NONE',  ( 0.2885697896453105482, -15.75356890148129452, -40.13549262224773884 ) ) ;
#17833 = B_SPLINE_CURVE_WITH_KNOTS ( 'NONE', 3,
 ( #31492, #54973, #45609, #17102 ),
 .UNSPECIFIED., .F., .F.,
 ( 4, 4 ),
 ( 5.553824967135426632E-18, 0.004050076154993001616 ),
 .UNSPECIFIED. ) ;
#17834 = ORIENTED_EDGE ( 'NONE', *, *, #23858, .T. ) ;
#17835 = LINE ( 'NONE', #60717, #6708 ) ;
#17836 = ORIENTED_EDGE ( 'NONE', *, *, #61432, .T. ) ;
#17837 = B_SPLINE_CURVE_WITH_KNOTS ( 'NONE', 3,
 ( #55838, #32058, #51137, #24179, #61446, #5051 ),
 .UNSPECIFIED., .F., .F.,
 ( 4, 2, 4 ),
 ( 1.228596259724018017E-16, 0.0002448718616795936384, 0.0004897437233590644368 ),
 .UNSPECIFIED. ) ;
#17838 = EDGE_LOOP ( 'NONE', ( #49745, #58718, #2918, #30829 ) ) ;
#17839 = EDGE_CURVE ( 'NONE', #57673, #2634, #35552, .T. ) ;
#17840 = ORIENTED_EDGE ( 'NONE', *, *, #10963, .T. ) ;
#17841 = CARTESIAN_POINT ( 'NONE',  ( 0.2940133293163016970, 25.89542274635558172, -35.71648961426042490 ) ) ;
#17842 = DIRECTION ( 'NONE',  ( 0.000000000000000000, 0.000000000000000000, 1.000000000000000000 ) ) ;
#17843 = VECTOR ( 'NONE', #22906, 1000.000000000000114 ) ;
#17844 = DIRECTION ( 'NONE',  ( -1.000000000000000000, 0.000000000000000000, -0.000000000000000000 ) ) ;
#17845 = AXIS2_PLACEMENT_3D ( 'NONE', #46939, #19344, #14652 ) ;
#17846 = CARTESIAN_POINT ( 'NONE',  ( 1.830465331921977912, 42.17827523781150489, -12.70311591074435142 ) ) ;
#17847 = CARTESIAN_POINT ( 'NONE',  ( -6.016489644550736315, -16.32089497094054664, -9.417787539062418389 ) ) ;
#17848 = ORIENTED_EDGE ( 'NONE', *, *, #31768, .F. ) ;
#17849 = CARTESIAN_POINT ( 'NONE',  ( 0.3676999524040366896, 5.056646555325087000, 43.82215089355334925 ) ) ;
#17850 = EDGE_CURVE ( 'NONE', #36503, #8614, #1902, .T. ) ;
#17851 = LINE ( 'NONE', #40754, #34795 ) ;
#17852 = CARTESIAN_POINT ( 'NONE',  ( 0.6000166863083090663, 48.30184070261004337, -8.874438937089866641 ) ) ;
#17853 = ORIENTED_EDGE ( 'NONE', *, *, #4488, .T. ) ;
#17854 = ADVANCED_FACE ( 'NONE', ( #44293 ), #54250, .F. ) ;
#17855 =( BOUNDED_SURFACE ( )  B_SPLINE_SURFACE ( 3, 1, ( 
 ( #41604, #8361 ),
 ( #17787, #13097 ),
 ( #51278, #3657 ),
 ( #22788, #48440 ) ),
 .UNSPECIFIED., .F., .F., .F. ) 
 B_SPLINE_SURFACE_WITH_KNOTS ( ( 4, 4 ),
 ( 2, 2 ),
 ( 0.000000000000000000, 1.000000000000000000 ),
 ( 0.000000000000000000, 1.000000000000000000 ),
 .UNSPECIFIED. ) 
 GEOMETRIC_REPRESENTATION_ITEM ( )  RATIONAL_B_SPLINE_SURFACE ( (
 ( 1.000000000000000000, 1.000000000000000000),
 ( 0.7211978278499968642, 0.9934217856018975334),
 ( 0.7211978278499968642, 0.9934217856018975334),
 ( 1.000000000000000000, 1.000000000000000000) ) ) 
 REPRESENTATION_ITEM ( '' )  SURFACE ( )  );
#17856 = ORIENTED_EDGE ( 'NONE', *, *, #17487, .T. ) ;
#17857 = CARTESIAN_POINT ( 'NONE',  ( 0.9757892942422822236, 34.01031843153931078, -26.16173342773506150 ) ) ;
#17858 = CARTESIAN_POINT ( 'NONE',  ( 3.240649175237396484, 21.95100081562274497, -38.12372595366539940 ) ) ;
#17859 = CARTESIAN_POINT ( 'NONE',  ( 0.5809828226811553087, -12.92184523170170607, -46.11980934799353093 ) ) ;
#17860 = CARTESIAN_POINT ( 'NONE',  ( 0.1092355843206037486, -42.71527351115375382, -5.926758618547823154 ) ) ;
#17861 = CARTESIAN_POINT ( 'NONE',  ( 0.5804410086790514622, 5.237717535875084707, 46.60564522533493204 ) ) ;
#17862 = VECTOR ( 'NONE', #29866, 1000.000000000000114 ) ;
#17863 = ORIENTED_EDGE ( 'NONE', *, *, #52684, .T. ) ;
#17864 = CARTESIAN_POINT ( 'NONE',  ( 0.7057020205115032141, 34.46103118762836459, -33.27137945725683466 ) ) ;
#17865 = DIRECTION ( 'NONE',  ( -1.000000000000000000, -0.000000000000000000, -0.000000000000000000 ) ) ;
#17867 = ADVANCED_FACE ( 'NONE', ( #30771 ), #48400, .F. ) ;
#17866 = CARTESIAN_POINT ( 'NONE',  ( -6.016761891674564211, -14.95139917749696501, -11.46828378093574941 ) ) ;
#17868 = CARTESIAN_POINT ( 'NONE',  ( 0.5832655196449141322, -41.75240550830532982, -21.35349660461640298 ) ) ;
#17869 = CARTESIAN_POINT ( 'NONE',  ( 3.727782113643637096, -43.27745144898557328, 7.735630031656845595 ) ) ;
#17870 =( LENGTH_UNIT ( ) NAMED_UNIT ( * ) SI_UNIT ( .MILLI., .METRE. ) );
#17871 = DIRECTION ( 'NONE',  ( 0.000000000000000000, 0.000000000000000000, 1.000000000000000000 ) ) ;
#17872 = PRESENTATION_LAYER_ASSIGNMENT (  '', '', ( #46860 ) ) ;
#17873 =( BOUNDED_SURFACE ( )  B_SPLINE_SURFACE ( 3, 1, ( 
 ( #21887, #41024 ),
 ( #60085, #50376 ),
 ( #60686, #7442 ),
 ( #27496, #17188 ) ),
 .UNSPECIFIED., .F., .F., .F. ) 
 B_SPLINE_SURFACE_WITH_KNOTS ( ( 4, 4 ),
 ( 2, 2 ),
 ( 0.000000000000000000, 1.000000000000000000 ),
 ( 0.000000000000000000, 1.000000000000000000 ),
 .UNSPECIFIED. ) 
 GEOMETRIC_REPRESENTATION_ITEM ( )  RATIONAL_B_SPLINE_SURFACE ( (
 ( 1.000000000000000000, 1.000000000000000000),
 ( 0.9729067724841187204, 0.9999501103223794596),
 ( 0.9729067724841187204, 0.9999501103223794596),
 ( 1.000000000000000000, 1.000000000000000000) ) ) 
 REPRESENTATION_ITEM ( '' )  SURFACE ( )  );
#17874 = EDGE_LOOP ( 'NONE', ( #17650, #53176 ) ) ;
#17875 = CARTESIAN_POINT ( 'NONE',  ( 1.092182651088185352, 41.63662333493258672, 4.811733752737049841 ) ) ;
#17876 = CARTESIAN_POINT ( 'NONE',  ( 4.975610109902397937, 42.33317580307156192, -24.50207406657668230 ) ) ;
#17877 = CARTESIAN_POINT ( 'NONE',  ( 5.960721111146673579, -2.672857320903454514, 20.35079619394241135 ) ) ;
#17878 = CARTESIAN_POINT ( 'NONE',  ( 0.5850706913938534814, 29.01314519953853477, -38.10903744847111341 ) ) ;
#17879 =( GEOMETRIC_REPRESENTATION_CONTEXT ( 3 ) GLOBAL_UNCERTAINTY_ASSIGNED_CONTEXT ( ( #31127 ) ) GLOBAL_UNIT_ASSIGNED_CONTEXT ( ( #1204, #30331, #49443 ) ) REPRESENTATION_CONTEXT ( 'NONE', 'WORKASPACE' ) );
#17880 = CARTESIAN_POINT ( 'NONE',  ( 2.624215991343620935, 19.66774719432979524, 43.79392271049075447 ) ) ;
#17881 = CARTESIAN_POINT ( 'NONE',  ( 0.5819845901640494645, 6.701564444318373504, -47.42480841519682144 ) ) ;
#17882 = CARTESIAN_POINT ( 'NONE',  ( 0.6016118706126977189, -49.10631034723315480, -0.3483372864810193592 ) ) ;
#17883 = B_SPLINE_CURVE_WITH_KNOTS ( 'NONE', 3,
 ( #5729, #48369, #34907, #5431, #33983, #28640 ),
 .UNSPECIFIED., .F., .F.,
 ( 4, 2, 4 ),
 ( 1.268664800107929448E-16, 0.0002450741128632319085, 0.0004901482257263369653 ),
 .UNSPECIFIED. ) ;
#17884 = CARTESIAN_POINT ( 'NONE',  ( 0.5824936645240096356, 22.85612023312696905, -40.94918737812936627 ) ) ;
#17885 = FACE_OUTER_BOUND ( 'NONE', #12049, .T. ) ;
#17886 = CARTESIAN_POINT ( 'NONE',  ( 0.5839879327111933138, -29.22928252017487338, -37.94312859586442244 ) ) ;
#17887 = AXIS2_PLACEMENT_3D ( 'NONE', #673, #28883, #19816 ) ;
#17888 = ORIENTED_EDGE ( 'NONE', *, *, #30145, .T. ) ;
#17889 = EDGE_CURVE ( 'NONE', #17815, #7813, #51944, .T. ) ;
#17890 = CIRCLE ( 'NONE', #13921, 4.000000000000000888 ) ;
#17891 = DIRECTION ( 'NONE',  ( 0.1024043820194936449, -0.01315135725335844948, -0.9946559125373960475 ) ) ;
#17892 = CARTESIAN_POINT ( 'NONE',  ( 0.1365634738349413291, 44.06882432424109908, -2.191196545822806652 ) ) ;
#17893 = CARTESIAN_POINT ( 'NONE',  ( 0.5988103622719994634, -38.53259676306939951, 28.80261254779972901 ) ) ;
#17894 = CARTESIAN_POINT ( 'NONE',  ( 5.981074661064941900, -17.77058762078884868, 10.26976685693792390 ) ) ;
#17895 = ORIENTED_EDGE ( 'NONE', *, *, #23062, .F. ) ;
#17896 = EDGE_CURVE ( 'NONE', #17512, #22171, #1322, .T. ) ;
#17897 = CARTESIAN_POINT ( 'NONE',  ( 4.960386119450145515, -30.75418163181142361, -31.12260877288235861 ) ) ;
#17898 = CARTESIAN_POINT ( 'NONE',  ( 0.9784957157296372277, -41.82994298070580896, -2.566890574853715190 ) ) ;
#17899 = B_SPLINE_CURVE_WITH_KNOTS ( 'NONE', 3,
 ( #14111, #34139, #14717, #24408 ),
 .UNSPECIFIED., .F., .F.,
 ( 4, 4 ),
 ( 0.000000000000000000, 0.004442905043737215703 ),
 .UNSPECIFIED. ) ;
#17900 = ADVANCED_FACE ( 'NONE', ( #26081 ), #47673, .F. ) ;
#17901 = B_SPLINE_CURVE_WITH_KNOTS ( 'NONE', 3,
 ( #21962, #18186, #37300, #36689, #37613, #60761 ),
 .UNSPECIFIED., .F., .F.,
 ( 4, 2, 4 ),
 ( 1.053462964043502403E-17, 0.0002448709889506572109, 0.0004897419779013039050 ),
 .UNSPECIFIED. ) ;
#17902 = ORIENTED_EDGE ( 'NONE', *, *, #59435, .F. ) ;
#17903 = CARTESIAN_POINT ( 'NONE',  ( 0.1158516988532803382, 4.187934451109883049, -43.92497426141537886 ) ) ;
#17904 = CARTESIAN_POINT ( 'NONE',  ( 0.5837799406558236148, -45.97443208162771811, -9.251764391131139575 ) ) ;
#17905 = ADVANCED_FACE ( 'NONE', ( #40835, #21385 ), #40518, .T. ) ;
#17906 = CARTESIAN_POINT ( 'NONE',  ( -6.072942160501519915, -19.21577577016807226, 1.248248308487570402 ) ) ;
#17907 = VERTEX_POINT ( 'NONE', #35811 ) ;
#17908 = EDGE_CURVE ( 'NONE', #52379, #3804, #6309, .T. ) ;
#17909 = DIRECTION ( 'NONE',  ( -0.9848077530122079093, -0.1736481776669314414, 5.551115123125783935E-17 ) ) ;
#17910 = ORIENTED_EDGE ( 'NONE', *, *, #60290, .T. ) ;
#17911 = ORIENTED_EDGE ( 'NONE', *, *, #29414, .T. ) ;
#17912 = CARTESIAN_POINT ( 'NONE',  ( 5.894904586330512508, 8.467339502218957037, -18.24372697164165302 ) ) ;
#17913 = VERTEX_POINT ( 'NONE', #17010 ) ;
#17914 = CARTESIAN_POINT ( 'NONE',  ( -4.915099999999998914, 1.224646799147353256E-15, -10.00000000000000000 ) ) ;
#17915 = B_SPLINE_CURVE_WITH_KNOTS ( 'NONE', 3,
 ( #15299, #25602, #44740, #1780 ),
 .UNSPECIFIED., .F., .F.,
 ( 4, 4 ),
 ( 0.000000000000000000, 0.005014147105413696050 ),
 .UNSPECIFIED. ) ;
#17916 = ORIENTED_EDGE ( 'NONE', *, *, #33544, .T. ) ;
#17917 = CARTESIAN_POINT ( 'NONE',  ( 0.5839879882104920261, 1.006200712814167388E-05, 47.89596766822081264 ) ) ;
#17918 = CARTESIAN_POINT ( 'NONE',  ( 0.9752132459055861124, 16.63533515462578904, 39.55248938404422887 ) ) ;
#17919 = EDGE_CURVE ( 'NONE', #33426, #46173, #22113, .T. ) ;
#17920 = ORIENTED_EDGE ( 'NONE', *, *, #35553, .T. ) ;
#17921 = CARTESIAN_POINT ( 'NONE',  ( 0.1152809850208375703, 15.03117900825671782, 41.48504477653962397 ) ) ;
#17922 = CARTESIAN_POINT ( 'NONE',  ( -6.072942160501519915, -11.00492040199085864, 15.80176854769318595 ) ) ;
#17923 = CARTESIAN_POINT ( 'NONE',  ( 0.5832655196449149093, -44.22601172460468177, -15.59791876849144465 ) ) ;
#17924 = CARTESIAN_POINT ( 'NONE',  ( -6.078726893082806448, 3.076629396955071538, 19.00863995194059086 ) ) ;
#17925 = ORIENTED_EDGE ( 'NONE', *, *, #2763, .T. ) ;
#17926 = DIRECTION ( 'NONE',  ( 0.07439287786467665975, -0.3937848822959491568, 0.9161872986448660328 ) ) ;
#17927 = ORIENTED_EDGE ( 'NONE', *, *, #61372, .F. ) ;
#17928 = CARTESIAN_POINT ( 'NONE',  ( -2.739355103387248747, -2.122549901524039218, 14.77641190771823965 ) ) ;
#17929 = EDGE_CURVE ( 'NONE', #27219, #28691, #4107, .T. ) ;
#17930 = ORIENTED_EDGE ( 'NONE', *, *, #54468, .T. ) ;
#17931 = CARTESIAN_POINT ( 'NONE',  ( 2.528190830796657629, -26.16753660177270646, -32.82551087718047000 ) ) ;
#17932 = CARTESIAN_POINT ( 'NONE',  ( 0.6001305935487422083, -29.70149728382463650, 37.84751346122805415 ) ) ;
#17933 = ORIENTED_EDGE ( 'NONE', *, *, #5521, .T. ) ;
#17934 = DIRECTION ( 'NONE',  ( -1.000000000000000000, -1.836909530733573776E-16, 1.925929944387235853E-32 ) ) ;
#17935 = CARTESIAN_POINT ( 'NONE',  ( 4.960156602257182357, -30.99165383632791659, 34.56254177294259478 ) ) ;
#17936 = CARTESIAN_POINT ( 'NONE',  ( 0.6000166863083106206, 48.10206967781400778, 9.900220927796519632 ) ) ;
#17937 = PLANE ( 'NONE',  #15436 ) ;
#17938 = VECTOR ( 'NONE', #47322, 1000.000000000000000 ) ;
#17939 = ORIENTED_EDGE ( 'NONE', *, *, #12400, .F. ) ;
#17940 = PLANE ( 'NONE',  #5896 ) ;
#17941 = CARTESIAN_POINT ( 'NONE',  ( 0.9762797500689124330, -41.77809974471944088, 3.303810967046753255 ) ) ;
#17942 = CARTESIAN_POINT ( 'NONE',  ( 3.660087539127327538, -14.24113226412018385, -45.87884541725762233 ) ) ;
#17944 = EDGE_CURVE ( 'NONE', #50798, #8991, #30312, .T. ) ;
#17943 = CARTESIAN_POINT ( 'NONE',  ( 0.5998501479064699549, 5.759754759340783181, -47.76154736470751772 ) ) ;
#17945 = CARTESIAN_POINT ( 'NONE',  ( 0.7057020205114974409, -29.82342581815230886, 37.48480537461322371 ) ) ;
#17946 = CARTESIAN_POINT ( 'NONE',  ( 2.648799415243708655, 48.82680556394809201, -4.523330820314529710 ) ) ;
#17947 = EDGE_CURVE ( 'NONE', #22095, #55350, #61278, .T. ) ;
#17948 = DIRECTION ( 'NONE',  ( 0.000000000000000000, 0.000000000000000000, -1.000000000000000000 ) ) ;
#17949 = CARTESIAN_POINT ( 'NONE',  ( 0.9730545539215883499, 39.83279466599061891, -15.95224156741785393 ) ) ;
#17950 = CARTESIAN_POINT ( 'NONE',  ( 5.910764540655177868, -15.79365219732158465, 12.45238084621580121 ) ) ;
#17951 = VECTOR ( 'NONE', #19397, 1000.000000000000000 ) ;
#17952 = CARTESIAN_POINT ( 'NONE',  ( 4.956445790444004018, -46.73954499432459642, -5.740468958468717631 ) ) ;
#17953 = CARTESIAN_POINT ( 'NONE',  ( 0.1073791018717483448, -16.05399293000841254, 40.02496097243031414 ) ) ;
#17954 = CARTESIAN_POINT ( 'NONE',  ( 1.000433927950262314, 35.71901661376694648, -21.92191893512719147 ) ) ;
#17955 = CARTESIAN_POINT ( 'NONE',  ( 0.1101816497532063094, -21.44450189183895006, 37.41460501058178068 ) ) ;
#17956 = CARTESIAN_POINT ( 'NONE',  ( 5.895596859100789899, -19.93295055289977213, 2.684337063064242912 ) ) ;
#17957 = CARTESIAN_POINT ( 'NONE',  ( 0.5850706913938533704, 18.16120156791880902, 44.31965802246111963 ) ) ;
#17958 = DIRECTION ( 'NONE',  ( -0.07439287786467652097, 0.8701500408883644511, 0.4871392060438053950 ) ) ;
#17959 = FACE_OUTER_BOUND ( 'NONE', #45734, .T. ) ;
#17960 = CARTESIAN_POINT ( 'NONE',  ( 4.000000000000000000, 0.000000000000000000, -5.600000000000000533 ) ) ;
#17961 = CARTESIAN_POINT ( 'NONE',  ( 0.6026112563231247332, -47.54525502191918918, 12.28778742511749478 ) ) ;
#17963 = ORIENTED_EDGE ( 'NONE', *, *, #31839, .T. ) ;
#17962 = CARTESIAN_POINT ( 'NONE',  ( 1.114299999999999846, 0.000000000000000000, -5.633200000000004870 ) ) ;
#17964 = VERTEX_POINT ( 'NONE', #17616 ) ;
#17965 = CARTESIAN_POINT ( 'NONE',  ( 0.6008123274975392114, -39.61436965115080255, 29.02165171558021228 ) ) ;
#17966 = CARTESIAN_POINT ( 'NONE',  ( 0.8753041380234471980, 44.61941359694289844, -20.49990873486824583 ) ) ;
#17967 = CARTESIAN_POINT ( 'NONE',  ( 0.5800708057587378175, -34.30831467131380208, 33.42085258735466624 ) ) ;
#17968 = EDGE_LOOP ( 'NONE', ( #26527, #11749, #13511, #54326 ) ) ;
#17969 = ADVANCED_FACE ( 'NONE', ( #46140 ), #5207, .F. ) ;
#17970 = ORIENTED_EDGE ( 'NONE', *, *, #8604, .F. ) ;
#17971 = CARTESIAN_POINT ( 'NONE',  ( 2.009741617377216460, -30.66706143059037615, 31.60752158641105680 ) ) ;
#17972 = CARTESIAN_POINT ( 'NONE',  ( -6.078075953587585900, 15.42887869085103425, 11.52149628260751690 ) ) ;
#17973 = ADVANCED_FACE ( 'NONE', ( #60199 ), #33232, .F. ) ;
#17974 = PRODUCT_DEFINITION_CONTEXT ( 'detailed design', #15591, 'design' ) ;
#17975 = CIRCLE ( 'NONE', #39004, 0.2500000000000002220 ) ;
#17976 = VERTEX_POINT ( 'NONE', #42067 ) ;
#17977 = ORIENTED_EDGE ( 'NONE', *, *, #12884, .F. ) ;
#17978 =( BOUNDED_SURFACE ( )  B_SPLINE_SURFACE ( 3, 1, ( 
 ( #4586, #56612 ),
 ( #57210, #43797 ),
 ( #30569, #45021 ),
 ( #54360, #34372 ) ),
 .UNSPECIFIED., .F., .F., .F. ) 
 B_SPLINE_SURFACE_WITH_KNOTS ( ( 4, 4 ),
 ( 2, 2 ),
 ( 0.000000000000000000, 1.000000000000000000 ),
 ( 0.000000000000000000, 1.000000000000000000 ),
 .UNSPECIFIED. ) 
 GEOMETRIC_REPRESENTATION_ITEM ( )  RATIONAL_B_SPLINE_SURFACE ( (
 ( 1.000000000000000000, 1.000000000000000000),
 ( 0.9953040768229005630, 0.8617119497784937465),
 ( 0.9953040768229005630, 0.8617119497784937465),
 ( 1.000000000000000000, 1.000000000000000000) ) ) 
 REPRESENTATION_ITEM ( '' )  SURFACE ( )  );
#17979 = CARTESIAN_POINT ( 'NONE',  ( 0.9754292589017203863, 19.62773389896157639, -37.02809107808331390 ) ) ;
#17980 = EDGE_CURVE ( 'NONE', #38487, #11037, #46762, .T. ) ;
#17981 = ADVANCED_FACE ( 'NONE', ( #46754 ), #54791, .F. ) ;
#17982 = AXIS2_PLACEMENT_3D ( 'NONE', #22211, #41340, #51310 ) ;
#17983 = CYLINDRICAL_SURFACE ( 'NONE', #41006, 10.00000000000000000 ) ;
#17984 = CARTESIAN_POINT ( 'NONE',  ( 1.231276596079887264, -2.246340108599748309, -41.85965512441022440 ) ) ;
#17985 = ADVANCED_FACE ( 'NONE', ( #61421 ), #48044, .F. ) ;
#17986 = ORIENTED_EDGE ( 'NONE', *, *, #49360, .F. ) ;
#17987 = ORIENTED_EDGE ( 'NONE', *, *, #59393, .F. ) ;
#17988 = DIRECTION ( 'NONE',  ( -0.5000000000000024425, 0.8660254037844372643, 0.000000000000000000 ) ) ;
#17989 = CARTESIAN_POINT ( 'NONE',  ( 2.299652685299201860, -48.77886880766101285, 4.990358975379336925 ) ) ;
#17990 = EDGE_CURVE ( 'NONE', #34487, #1986, #36428, .T. ) ;
#17991 = CARTESIAN_POINT ( 'NONE',  ( 0.6017667736363749853, -48.10631678344241635, -0.3491025323178837403 ) ) ;
#17992 = ORIENTED_EDGE ( 'NONE', *, *, #55762, .T. ) ;
#17993 = ORIENTED_EDGE ( 'NONE', *, *, #29802, .T. ) ;
#17994 = CARTESIAN_POINT ( 'NONE',  ( 0.7056759521545006297, 10.05083851003305995, 45.81189228095935562 ) ) ;
#17995 = VECTOR ( 'NONE', #38370, 999.9999999999998863 ) ;
#17996 = ORIENTED_EDGE ( 'NONE', *, *, #34652, .T. ) ;
#17997 = CARTESIAN_POINT ( 'NONE',  ( 1.154321485836933281, 20.73950273457894511, -37.57248783354748412 ) ) ;
#17998 = CARTESIAN_POINT ( 'NONE',  ( 2.528100132419516477, 23.91661738292092920, -34.49998828392612893 ) ) ;
#17999 = CARTESIAN_POINT ( 'NONE',  ( 4.956653778116970166, 39.67974989265038488, 27.17045123668485829 ) ) ;
#18000 = CARTESIAN_POINT ( 'NONE',  ( 0.5980271706414734822, -31.16543947089364863, -37.95740540958678366 ) ) ;
#18001 = DIRECTION ( 'NONE',  ( 0.1011922191286468015, 0.4487230644346660857, -0.8879232772217329206 ) ) ;
#18002 = EDGE_LOOP ( 'NONE', ( #5818, #35788 ) ) ;
#18003 = CARTESIAN_POINT ( 'NONE',  ( 4.549368137175248350, 24.02461520945223228, 35.57418903283122802 ) ) ;
#18004 = FACE_OUTER_BOUND ( 'NONE', #21237, .T. ) ;
#18005 = VERTEX_POINT ( 'NONE', #28 ) ;
#18006 = CARTESIAN_POINT ( 'NONE',  ( 0.8551540677456715978, -19.17641535420820986, -43.91216198251559888 ) ) ;
#18007 = DIRECTION ( 'NONE',  ( -1.000000000000000000, -5.380183451256670742E-17, 1.298891185607911324E-16 ) ) ;
#18008 = CARTESIAN_POINT ( 'NONE',  ( 5.895596859100789899, 3.348897116308617417, -19.83212220910478507 ) ) ;
#18009 = CARTESIAN_POINT ( 'NONE',  ( 0.5988103622719992414, 46.62176011478423021, -11.86435782853384957 ) ) ;
#18010 = ORIENTED_EDGE ( 'NONE', *, *, #29107, .F. ) ;
#18011 = CARTESIAN_POINT ( 'NONE',  ( 4.967162193818130511, 42.96271701169388990, -3.259922920617310371 ) ) ;
#18012 = CARTESIAN_POINT ( 'NONE',  ( 4.834790513006553603, 7.995814508776146745, -46.56883390493718622 ) ) ;
#18013 = CARTESIAN_POINT ( 'NONE',  ( 4.967162193818130511, 0.000000000000000000, 0.000000000000000000 ) ) ;
#18014 = B_SPLINE_CURVE_WITH_KNOTS ( 'NONE', 3,
 ( #39533, #38, #57652, #660 ),
 .UNSPECIFIED., .F., .F.,
 ( 4, 4 ),
 ( 2.292215966409847588E-17, 0.004564976165746187711 ),
 .UNSPECIFIED. ) ;
#18015 = CARTESIAN_POINT ( 'NONE',  ( 0.8551540677456834771, 34.52115452272929019, 33.23105123575912501 ) ) ;
#18016 = CARTESIAN_POINT ( 'NONE',  ( 0.1156495703730067437, -17.98529708537768812, -40.29233229761928925 ) ) ;
#18017 = CARTESIAN_POINT ( 'NONE',  ( 0.2885700199627501683, -34.69058524452997005, -25.60460887553365694 ) ) ;
#18018 = CARTESIAN_POINT ( 'NONE',  ( 5.958863334805807099, 12.49619391867182294, -16.28335246510355105 ) ) ;
#18019 = EDGE_CURVE ( 'NONE', #96, #50941, #23854, .T. ) ;
#18020 = DIRECTION ( 'NONE',  ( 0.000000000000000000, 1.000000000000000000, 0.000000000000000000 ) ) ;
#18021 = CARTESIAN_POINT ( 'NONE',  ( 3.660087539127323986, -36.93668088065471267, 30.71416465583044442 ) ) ;
#18022 = CARTESIAN_POINT ( 'NONE',  ( 0.9790320750461898314, 41.90858792809413558, 0.08596752522955294906 ) ) ;
#18023 = ORIENTED_EDGE ( 'NONE', *, *, #47688, .T. ) ;
#18024 = CONICAL_SURFACE ( 'NONE', #48927, 43.92652462719577500, 1.486293639869522343 ) ;
#18025 = CARTESIAN_POINT ( 'NONE',  ( -16.15200392031422538, -12.45603944020924381, -1.053615289124667287 ) ) ;
#18026 = CARTESIAN_POINT ( 'NONE',  ( 4.956653778116966613, 0.000000000000000000, 0.000000000000000000 ) ) ;
#18027 = CARTESIAN_POINT ( 'NONE',  ( 4.975801465491694664, -45.55012473237763260, 14.85979367497093762 ) ) ;
#18028 = CARTESIAN_POINT ( 'NONE',  ( 0.6026112563231247332, -39.25096069177133984, -29.51106707113837402 ) ) ;
#18029 = CARTESIAN_POINT ( 'NONE',  ( 4.967162193818130511, 0.000000000000000000, 0.000000000000000000 ) ) ;
#18030 = B_SPLINE_CURVE_WITH_KNOTS ( 'NONE', 3,
 ( #53463, #33468, #19990, #9328, #38480, #57854 ),
 .UNSPECIFIED., .F., .F.,
 ( 4, 2, 4 ),
 ( 7.757919228897728493E-18, 0.0002291978881530148861, 0.0004583957763060220202 ),
 .UNSPECIFIED. ) ;
#18031 = CARTESIAN_POINT ( 'NONE',  ( 0.6846871229502932144, 0.8641397935266237340, -47.90045233486063125 ) ) ;
#18032 = ITEM_DEFINED_TRANSFORMATION ( 'NONE', 'NONE', #19889,  #14677 ) ;
#18033 = DIRECTION ( 'NONE',  ( -1.000000000000000000, -0.000000000000000000, -0.000000000000000000 ) ) ;
#18034 =( BOUNDED_SURFACE ( )  B_SPLINE_SURFACE ( 3, 1, ( 
 ( #13207, #8474 ),
 ( #3770, #56397 ),
 ( #13513, #51704 ),
 ( #24129, #24752 ) ),
 .UNSPECIFIED., .F., .F., .F. ) 
 B_SPLINE_SURFACE_WITH_KNOTS ( ( 4, 4 ),
 ( 2, 2 ),
 ( 0.000000000000000000, 1.000000000000000000 ),
 ( 0.000000000000000000, 1.000000000000000000 ),
 .UNSPECIFIED. ) 
 GEOMETRIC_REPRESENTATION_ITEM ( )  RATIONAL_B_SPLINE_SURFACE ( (
 ( 1.000000000000000000, 1.000000000000000000),
 ( 0.7211978278499970862, 0.9934217856018976445),
 ( 0.7211978278499970862, 0.9934217856018976445),
 ( 1.000000000000000000, 1.000000000000000000) ) ) 
 REPRESENTATION_ITEM ( '' )  SURFACE ( )  );
#18035 = CARTESIAN_POINT ( 'NONE',  ( 2.500000000000000000, -1.178949249685214307, 2.042000000000001592 ) ) ;
#18036 = CARTESIAN_POINT ( 'NONE',  ( 0.6026777506516367566, -1.399865435252327872, 49.08754187571837946 ) ) ;
#18038 = VERTEX_POINT ( 'NONE', #24466 ) ;
#18037 = DIRECTION ( 'NONE',  ( -0.7071067811865364705, 8.659560562355067211E-17, -0.7071067811865584529 ) ) ;
#18039 = ORIENTED_EDGE ( 'NONE', *, *, #16776, .T. ) ;
#18040 = CONICAL_SURFACE ( 'NONE', #44089, 43.12527911185304674, 0.04450589592585017101 ) ;
#18041 = CARTESIAN_POINT ( 'NONE',  ( 0.1156495703730067853, -6.907609969323758037, 43.58013168569789286 ) ) ;
#18042 = CARTESIAN_POINT ( 'NONE',  ( 3.660176727303398270, 43.62748706623523276, 20.10773453922302423 ) ) ;
#18043 = DIRECTION ( 'NONE',  ( 0.000000000000000000, 0.000000000000000000, 1.000000000000000000 ) ) ;
#18044 = EDGE_CURVE ( 'NONE', #16356, #47431, #34769, .T. ) ;
#18045 = ORIENTED_EDGE ( 'NONE', *, *, #55566, .T. ) ;
#18046 = CARTESIAN_POINT ( 'NONE',  ( 0.5806925824938499181, 22.05663578530122493, 41.38510819338441138 ) ) ;
#18047 = CARTESIAN_POINT ( 'NONE',  ( 0.5988103622719994634, -29.76496569135189674, 37.79415722405543931 ) ) ;
#18048 = ADVANCED_FACE ( 'NONE', ( #57960 ), #52411, .F. ) ;
#18049 =( BOUNDED_SURFACE ( )  B_SPLINE_SURFACE ( 3, 1, ( 
 ( #23414, #23725 ),
 ( #13723, #42853 ),
 ( #61300, #43160 ),
 ( #32833, #23114 ) ),
 .UNSPECIFIED., .F., .F., .F. ) 
 B_SPLINE_SURFACE_WITH_KNOTS ( ( 4, 4 ),
 ( 2, 2 ),
 ( 0.000000000000000000, 1.000000000000000000 ),
 ( 0.000000000000000000, 1.000000000000000000 ),
 .UNSPECIFIED. ) 
 GEOMETRIC_REPRESENTATION_ITEM ( )  RATIONAL_B_SPLINE_SURFACE ( (
 ( 1.000000000000000000, 1.000000000000000000),
 ( 0.9953485035131437453, 0.8621029689291515030),
 ( 0.9953485035131437453, 0.8621029689291515030),
 ( 1.000000000000000000, 1.000000000000000000) ) ) 
 REPRESENTATION_ITEM ( '' )  SURFACE ( )  );
#18050 = ORIENTED_EDGE ( 'NONE', *, *, #50754, .T. ) ;
#18051 = ORIENTED_EDGE ( 'NONE', *, *, #2157, .F. ) ;
#18052 = EDGE_CURVE ( 'NONE', #2310, #45554, #9748, .T. ) ;
#18053 = ADVANCED_FACE ( 'NONE', ( #52345 ), #12025, .F. ) ;
#18054 = CARTESIAN_POINT ( 'NONE',  ( 0.6025881611877910160, 41.55278713510049471, 24.24244696985822856 ) ) ;
#18055 = ADVANCED_FACE ( 'NONE', ( #42664 ), #32765, .T. ) ;
#18056 = CARTESIAN_POINT ( 'NONE',  ( 2.881901170002227897, 8.474399077991585715E-12, -49.00591519830774700 ) ) ;
#18057 = CARTESIAN_POINT ( 'NONE',  ( 0.1147471544378676767, -42.75889291922428015, -10.89170623894889189 ) ) ;
#18058 = CARTESIAN_POINT ( 'NONE',  ( 0.8753041380234465318, 17.79089796329371964, -45.76704357430848802 ) ) ;
#18059 = ORIENTED_EDGE ( 'NONE', *, *, #31551, .T. ) ;
#18060 = EDGE_CURVE ( 'NONE', #48571, #43165, #13142, .T. ) ;
#18061 = B_SPLINE_CURVE_WITH_KNOTS ( 'NONE', 3,
 ( #16891, #59783, #50990, #26891 ),
 .UNSPECIFIED., .F., .F.,
 ( 4, 4 ),
 ( 8.673617379884035472E-19, 0.004048833967417087357 ),
 .UNSPECIFIED. ) ;
#18062 = VERTEX_POINT ( 'NONE', #29468 ) ;
#18063 = CARTESIAN_POINT ( 'NONE',  ( 0.6031356219577718170, -47.70727206974381573, -6.192730535895980992 ) ) ;
#18064 = CARTESIAN_POINT ( 'NONE',  ( 0.7044674535452954967, -43.19749584530718778, 23.36191506502784421 ) ) ;
#18065 = CARTESIAN_POINT ( 'NONE',  ( 1.296416391601052709, 39.21237564904568274, -20.11708154863144316 ) ) ;
#18066 = DIRECTION ( 'NONE',  ( 0.000000000000000000, 0.000000000000000000, 1.000000000000000000 ) ) ;
#18067 = EDGE_CURVE ( 'NONE', #13798, #48102, #58695, .T. ) ;
#18068 = VERTEX_POINT ( 'NONE', #5635 ) ;
#18069 = VERTEX_POINT ( 'NONE', #9131 ) ;
#18070 = CARTESIAN_POINT ( 'NONE',  ( 5.959547316686252039, 7.858107265727752200, -18.96183906913535466 ) ) ;
#18071 = FACE_OUTER_BOUND ( 'NONE', #60323, .T. ) ;
#18072 = VECTOR ( 'NONE', #696, 1000.000000000000000 ) ;
#18073 = EDGE_LOOP ( 'NONE', ( #58395, #45522, #34717, #30437 ) ) ;
#18074 = CARTESIAN_POINT ( 'NONE',  ( 0.6001305935487422083, -33.64689939321966250, 34.38748867424655487 ) ) ;
#18075 = EDGE_LOOP ( 'NONE', ( #19117, #26623, #18211, #16855 ) ) ;
#18076 = CARTESIAN_POINT ( 'NONE',  ( -6.016761891674564211, 0.003433883959783673098, 18.84319130225482297 ) ) ;
#18077 = CARTESIAN_POINT ( 'NONE',  ( 4.956445790444004018, -46.59545590650535019, -6.811867512257778756 ) ) ;
#18078 = B_SPLINE_CURVE_WITH_KNOTS ( 'NONE', 3,
 ( #61207, #59436, #13315, #20932, #37438, #2105, #56509, #13625, #55045, #6798, #16542, #54732, #28021, #11866, #59126, #51811 ),
 .UNSPECIFIED., .F., .F.,
 ( 4, 3, 3, 3, 3, 4 ),
 ( 1.250973872328959318E-17, 0.0002732102107931907043, 0.0004098135523333788777, 0.0005464168938824937212, 0.0008195847345945476720, 0.001092771384553104397 ),
 .UNSPECIFIED. ) ;
#18079 = CARTESIAN_POINT ( 'NONE',  ( 1.227938101723748288, -37.58536632582793402, 20.72293514920737323 ) ) ;
#18080 = ORIENTED_EDGE ( 'NONE', *, *, #24546, .T. ) ;
#18081 = CARTESIAN_POINT ( 'NONE',  ( 0.5782707292762442330, 40.71812376972700775, -23.27596937574910285 ) ) ;
#18082 = CARTESIAN_POINT ( 'NONE',  ( -6.077587904424778920, 19.25606354205735116, 0.006185319731012296589 ) ) ;
#18083 = CARTESIAN_POINT ( 'NONE',  ( 0.5837800005270538106, -41.85555320131619794, 21.15060105182773498 ) ) ;
#18084 = ORIENTED_EDGE ( 'NONE', *, *, #2563, .T. ) ;
#18085 = CARTESIAN_POINT ( 'NONE',  ( 0.5834872094924169472, -18.11905305011485368, -44.33648115256919198 ) ) ;
#18086 = CARTESIAN_POINT ( 'NONE',  ( 4.967162193818130511, 42.96271701169385437, 3.259922920617894793 ) ) ;
#18087 = CARTESIAN_POINT ( 'NONE',  ( 4.960156602257180580, 14.43621227656587536, -44.12083041402437544 ) ) ;
#18088 = DIRECTION ( 'NONE',  ( 0.000000000000000000, 0.000000000000000000, 1.000000000000000000 ) ) ;
#18089 = EDGE_CURVE ( 'NONE', #25770, #11233, #30388, .T. ) ;
#18090 = CARTESIAN_POINT ( 'NONE',  ( 5.958863334805807099, -19.82594244347356494, 5.313608583996176193 ) ) ;
#18091 = ORIENTED_EDGE ( 'NONE', *, *, #61036, .F. ) ;
#18092 = CARTESIAN_POINT ( 'NONE',  ( 0.5797568599927147570, -42.13545938030424765, 20.58709235131896520 ) ) ;
#18093 = CARTESIAN_POINT ( 'NONE',  ( 4.956653778116974607, -32.11725092155068495, 35.79382859084104496 ) ) ;
#18094 = ORIENTED_EDGE ( 'NONE', *, *, #21356, .F. ) ;
#18095 = FACE_OUTER_BOUND ( 'NONE', #27168, .T. ) ;
#18096 = CARTESIAN_POINT ( 'NONE',  ( 0.9791128995231611620, -27.05351454939415490, 32.00694900754963612 ) ) ;
#18097 = CARTESIAN_POINT ( 'NONE',  ( 0.7056555295713324849, 19.10539864320401549, 43.92642606846683861 ) ) ;
#18098 = CARTESIAN_POINT ( 'NONE',  ( -2.569797478183790229, -8.547745408040713144, -11.87678401312191845 ) ) ;
#18099 = CARTESIAN_POINT ( 'NONE',  ( 4.549368137175248350, -32.13400537129904677, -28.46244473166662559 ) ) ;
#18100 = CARTESIAN_POINT ( 'NONE',  ( -6.010958268070873523, -18.84344976839986785, 0.01451635840156647282 ) ) ;
#18101 = CARTESIAN_POINT ( 'NONE',  ( 0.5827357941260208340, -47.89462047563812064, 0.3632531319012696214 ) ) ;
#18102 = CARTESIAN_POINT ( 'NONE',  ( 7.000000000000006217, -2.780326704359372228E-13, 80.00000000000001421 ) ) ;
#18103 = B_SPLINE_CURVE_WITH_KNOTS ( 'NONE', 3,
 ( #39509, #58562, #15692, #34796, #10991, #6236, #45439, #40435, #16931, #13154, #7486, #55412, #41064, #3105, #17532, #54799 ),
 .UNSPECIFIED., .F., .F.,
 ( 4, 3, 3, 3, 3, 4 ),
 ( 2.194378057379452319E-17, 0.0002618515315864391579, 0.0003927756766341943049, 0.0005236998216950536616, 0.0007855159896329885977, 0.001047349442285928304 ),
 .UNSPECIFIED. ) ;
#18104 = CARTESIAN_POINT ( 'NONE',  ( 3.680882792899937694, -10.62117075007680711, 46.78529781139670263 ) ) ;
#18105 = CARTESIAN_POINT ( 'NONE',  ( 0.6039202388192953519, -35.39742030259981931, -34.03801329058565983 ) ) ;
#18106 = CARTESIAN_POINT ( 'NONE',  ( 0.1104177457020372871, -5.624018123398955460, 42.75615561261992070 ) ) ;
#18107 = ORIENTED_EDGE ( 'NONE', *, *, #46382, .T. ) ;
#18108 = CARTESIAN_POINT ( 'NONE',  ( 4.962356264823594820, 34.94214251265108118, 23.45809613945535332 ) ) ;
#18109 = CARTESIAN_POINT ( 'NONE',  ( 0.8557997880470690211, 0.9121262075946178216, 47.89938907511594124 ) ) ;
#18110 = DIRECTION ( 'NONE',  ( -1.000000000000000000, -1.836909530733573776E-16, 1.925929944387235579E-32 ) ) ;
#18111 = DIRECTION ( 'NONE',  ( 0.9848077530122080203, 0.1736481776669315524, -2.220446049250313574E-16 ) ) ;
#18112 = CARTESIAN_POINT ( 'NONE',  ( 4.958415959904823644, -10.03736369554698271, 44.29960816831176373 ) ) ;
#18113 = DIRECTION ( 'NONE',  ( -0.9914448613738110483, -0.1305261922200468827, 0.000000000000000000 ) ) ;
#18114 = CIRCLE ( 'NONE', #53104, 6.887500000000022382 ) ;
#18115 = VERTEX_POINT ( 'NONE', #15703 ) ;
#18116 = EDGE_CURVE ( 'NONE', #56965, #4682, #7907, .T. ) ;
#18117 = CARTESIAN_POINT ( 'NONE',  ( 0.9754642270333695464, 11.27515941577631686, -41.40054989430066001 ) ) ;
#18118 =( BOUNDED_SURFACE ( )  B_SPLINE_SURFACE ( 3, 1, ( 
 ( #14263, #22405 ),
 ( #41533, #60597 ),
 ( #14876, #19883 ),
 ( #10470, #29254 ) ),
 .UNSPECIFIED., .F., .F., .F. ) 
 B_SPLINE_SURFACE_WITH_KNOTS ( ( 4, 4 ),
 ( 2, 2 ),
 ( 0.000000000000000000, 1.000000000000000000 ),
 ( 0.000000000000000000, 1.000000000000000000 ),
 .UNSPECIFIED. ) 
 GEOMETRIC_REPRESENTATION_ITEM ( )  RATIONAL_B_SPLINE_SURFACE ( (
 ( 1.000000000000000000, 1.000000000000000000),
 ( 0.9754377213608244057, 0.9999580625633939235),
 ( 0.9754377213608244057, 0.9999580625633939235),
 ( 1.000000000000000000, 1.000000000000000000) ) ) 
 REPRESENTATION_ITEM ( '' )  SURFACE ( )  );
#18119 = CARTESIAN_POINT ( 'NONE',  ( -6.015611763856276717, 18.68284711750058591, 2.453375430804133117 ) ) ;
#18120 = B_SPLINE_CURVE_WITH_KNOTS ( 'NONE', 3,
 ( #55751, #46088, #50147, #55444, #32278, #31038 ),
 .UNSPECIFIED., .F., .F.,
 ( 4, 2, 4 ),
 ( 1.870559545977334001E-17, 0.0002293319059085111467, 0.0004586638118170035909 ),
 .UNSPECIFIED. ) ;
#18121 = CARTESIAN_POINT ( 'NONE',  ( 2.185380717157383135, 28.52207511433232057, -33.54565596675051609 ) ) ;
#18122 = CARTESIAN_POINT ( 'NONE',  ( 0.6026112563231247332, -45.45287008515247607, -18.58971747839269284 ) ) ;
#18123 = ORIENTED_EDGE ( 'NONE', *, *, #55497, .F. ) ;
#18124 = EDGE_CURVE ( 'NONE', #32624, #52129, #45994, .T. ) ;
#18125 = CARTESIAN_POINT ( 'NONE',  ( 3.238018933889920792, -13.17791601574917770, -2.397920317590707118 ) ) ;
#18126 = B_SPLINE_CURVE_WITH_KNOTS ( 'NONE', 3,
 ( #22647, #51132, #13256, #32055 ),
 .UNSPECIFIED., .F., .F.,
 ( 4, 4 ),
 ( 2.194270917860438266E-17, 0.004559932413162187670 ),
 .UNSPECIFIED. ) ;
#18127 = CARTESIAN_POINT ( 'NONE',  ( 0.6023142530420679819, 23.82662387835867079, -41.79260242564376426 ) ) ;
#18128 = B_SPLINE_CURVE_WITH_KNOTS ( 'NONE', 3,
 ( #24491, #44254, #20419, #58600, #40475, #49528, #55455, #2531, #30730, #16651, #49224, #60158, #45181, #6583, #25729, #11972, #1910, #58923, #26346, #54516, #36085, #55148, #44870, #17271, #21035 ),
 .UNSPECIFIED., .F., .F.,
 ( 4, 3, 3, 3, 3, 3, 3, 3, 4 ),
 ( 5.057544569639794935E-18, 0.0005656085177311401821, 0.001131215744874499622, 0.001696821861372766567, 0.002262427090022498585, 0.002828031679238746359, 0.003393635864401605730, 0.003977030878808131623, 0.004561030005651158133 ),
 .UNSPECIFIED. ) ;
#18129 = ORIENTED_EDGE ( 'NONE', *, *, #14948, .F. ) ;
#18130 = DIRECTION ( 'NONE',  ( -1.000000000000000000, -0.000000000000000000, -0.000000000000000000 ) ) ;
#18131 = VERTEX_POINT ( 'NONE', #54183 ) ;
#18132 =( BOUNDED_SURFACE ( )  B_SPLINE_SURFACE ( 3, 1, ( 
 ( #36596, #21871 ),
 ( #60671, #50664 ),
 ( #45386, #59444 ),
 ( #7119, #17476 ) ),
 .UNSPECIFIED., .F., .F., .F. ) 
 B_SPLINE_SURFACE_WITH_KNOTS ( ( 4, 4 ),
 ( 2, 2 ),
 ( 0.000000000000000000, 1.000000000000000000 ),
 ( 0.000000000000000000, 1.000000000000000000 ),
 .UNSPECIFIED. ) 
 GEOMETRIC_REPRESENTATION_ITEM ( )  RATIONAL_B_SPLINE_SURFACE ( (
 ( 1.000000000000000000, 1.000000000000000000),
 ( 0.7282232189291694135, 0.9929344683865672927),
 ( 0.7282232189291694135, 0.9929344683865672927),
 ( 1.000000000000000000, 1.000000000000000000) ) ) 
 REPRESENTATION_ITEM ( '' )  SURFACE ( )  );
#18133 = CARTESIAN_POINT ( 'NONE',  ( 4.962356264823600149, -40.47344704301802665, 11.53844366967928892 ) ) ;
#18134 = CARTESIAN_POINT ( 'NONE',  ( 0.7242003506640004584, 17.72439838236845588, 45.79145527398227955 ) ) ;
#18135 = ORIENTED_EDGE ( 'NONE', *, *, #54076, .F. ) ;
#18136 = CARTESIAN_POINT ( 'NONE',  ( -6.016761891674564211, -7.214149619366230226, -17.40752468084790650 ) ) ;
#18137 = DIRECTION ( 'NONE',  ( -1.000000000000000000, -0.000000000000000000, -0.000000000000000000 ) ) ;
#18138 = ORIENTED_EDGE ( 'NONE', *, *, #44294, .F. ) ;
#18139 = CARTESIAN_POINT ( 'NONE',  ( 0.5835871038041854364, -7.665477966243003927, -46.26526667436971252 ) ) ;
#18140 = CARTESIAN_POINT ( 'NONE',  ( 5.895596859100789899, 12.98270243688412329, 15.36156309259609642 ) ) ;
#18141 =( BOUNDED_SURFACE ( )  B_SPLINE_SURFACE ( 3, 1, ( 
 ( #50046, #45669 ),
 ( #17456, #2723 ),
 ( #12460, #21850 ),
 ( #40990, #60053 ) ),
 .UNSPECIFIED., .F., .F., .F. ) 
 B_SPLINE_SURFACE_WITH_KNOTS ( ( 4, 4 ),
 ( 2, 2 ),
 ( 0.000000000000000000, 1.000000000000000000 ),
 ( 0.000000000000000000, 1.000000000000000000 ),
 .UNSPECIFIED. ) 
 GEOMETRIC_REPRESENTATION_ITEM ( )  RATIONAL_B_SPLINE_SURFACE ( (
 ( 1.000000000000000000, 1.000000000000000000),
 ( 0.9953040768229005630, 0.8617119497784937465),
 ( 0.9953040768229005630, 0.8617119497784937465),
 ( 1.000000000000000000, 1.000000000000000000) ) ) 
 REPRESENTATION_ITEM ( '' )  SURFACE ( )  );
#18142 = ADVANCED_FACE ( 'NONE', ( #49505 ), #12784, .F. ) ;
#18143 = ORIENTED_EDGE ( 'NONE', *, *, #29937, .T. ) ;
#18144 = B_SPLINE_CURVE_WITH_KNOTS ( 'NONE', 3,
 ( #58109, #44372, #19624, #2955, #26153, #45290 ),
 .UNSPECIFIED., .F., .F.,
 ( 4, 2, 4 ),
 ( 1.426045310262811165E-18, 0.0002450742804987334172, 0.0004901485609974654250 ),
 .UNSPECIFIED. ) ;
#18145 = CARTESIAN_POINT ( 'NONE',  ( 0.9787284016396597952, -7.155203276473740992, -41.29332954608010198 ) ) ;
#18146 = VERTEX_POINT ( 'NONE', #25389 ) ;
#18147 = CARTESIAN_POINT ( 'NONE',  ( -2.601141883200665639, 13.24771294992759607, 6.877029087164693522 ) ) ;
#18148 = B_SPLINE_CURVE_WITH_KNOTS ( 'NONE', 3,
 ( #53356, #1651, #1968, #11090 ),
 .UNSPECIFIED., .F., .F.,
 ( 4, 4 ),
 ( 0.000000000000000000, 0.005014147105413696050 ),
 .UNSPECIFIED. ) ;
#18149 = ORIENTED_EDGE ( 'NONE', *, *, #5242, .F. ) ;
#18150 = ORIENTED_EDGE ( 'NONE', *, *, #34117, .F. ) ;
#18151 = CARTESIAN_POINT ( 'NONE',  ( 0.9722240741986378776, -42.46141200043695108, -6.177112427866298994 ) ) ;
#18152 = CARTESIAN_POINT ( 'NONE',  ( 0.8557997880470697982, 46.50333260518559086, 11.51622788066474534 ) ) ;
#18153 = CARTESIAN_POINT ( 'NONE',  ( 0.5839254288179547281, 29.08514953649819290, 38.05364096126326956 ) ) ;
#18154 = CARTESIAN_POINT ( 'NONE',  ( 2.282816707992305627, 46.71114623179644809, 4.956388213174406587 ) ) ;
#18155 = CARTESIAN_POINT ( 'NONE',  ( 0.6846871229502932144, -37.47592888575227477, -29.84551600520671855 ) ) ;
#18156 = ORIENTED_EDGE ( 'NONE', *, *, #15164, .T. ) ;
#18157 = CARTESIAN_POINT ( 'NONE',  ( 3.727782113643637096, 6.344544998048565532, 43.50315534158083608 ) ) ;
#18158 = CARTESIAN_POINT ( 'NONE',  ( 4.975801465491694664, -27.09127437476410805, 39.51822597168447260 ) ) ;
#18159 = CARTESIAN_POINT ( 'NONE',  ( -6.078457390727109555, -18.90008989325098199, 3.685256173529869006 ) ) ;
#18160 = VERTEX_POINT ( 'NONE', #34812 ) ;
#18161 = EDGE_LOOP ( 'NONE', ( #41113, #12996, #29518, #15233 ) ) ;
#18162 = AXIS2_PLACEMENT_3D ( 'NONE', #8380, #56923, #27500 ) ;
#18163 = VECTOR ( 'NONE', #11248, 1000.000000000000114 ) ;
#18164 = FACE_OUTER_BOUND ( 'NONE', #5259, .T. ) ;
#18165 = CARTESIAN_POINT ( 'NONE',  ( 4.549368137175248350, 0.000000000000000000, 0.000000000000000000 ) ) ;
#18166 = CARTESIAN_POINT ( 'NONE',  ( 0.000000000000000000, 0.000000000000000000, -0.2800830152838832965 ) ) ;
#18167 = EDGE_CURVE ( 'NONE', #11343, #59975, #43784, .T. ) ;
#18168 = CARTESIAN_POINT ( 'NONE',  ( 0.1073791018717483448, -33.91564619577824402, 26.63563652260111070 ) ) ;
#18169 = DIRECTION ( 'NONE',  ( 0.07500201931887538753, -0.8647811570515562263, 0.4965161100172509334 ) ) ;
#18170 = ORIENTED_EDGE ( 'NONE', *, *, #58271, .T. ) ;
#18171 = CARTESIAN_POINT ( 'NONE',  ( 4.834790513006553603, 38.14091330549818792, -27.89014293880282835 ) ) ;
#18172 = DIRECTION ( 'NONE',  ( 0.000000000000000000, 0.000000000000000000, 1.000000000000000000 ) ) ;
#18173 = CARTESIAN_POINT ( 'NONE',  ( 4.390527457369402420, 42.57725424673462555, -10.83340931736345958 ) ) ;
#18174 = CARTESIAN_POINT ( 'NONE',  ( 0.5837800005270582515, -41.85558187593742474, -21.15054430667160545 ) ) ;
#18175 = CARTESIAN_POINT ( 'NONE',  ( 0.5549461598389368033, -43.62161577359375997, 6.509403411047773425 ) ) ;
#18176 = EDGE_CURVE ( 'NONE', #44946, #41577, #27325, .T. ) ;
#18177 = CARTESIAN_POINT ( 'NONE',  ( 0.1073791018717483448, 39.65380858626214433, -16.95003405440273525 ) ) ;
#18178 = ORIENTED_EDGE ( 'NONE', *, *, #25166, .T. ) ;
#18179 = CARTESIAN_POINT ( 'NONE',  ( -6.078726893082806448, -19.21623043802544828, -1.237145513439781075 ) ) ;
#18180 = CARTESIAN_POINT ( 'NONE',  ( 4.291220156522060236, -17.85566473792967557, 43.59546116366188784 ) ) ;
#18181 = ADVANCED_FACE ( 'NONE', ( #44843 ), #18764, .F. ) ;
#18182 = FACE_OUTER_BOUND ( 'NONE', #51567, .T. ) ;
#18183 = LINE ( 'NONE', #55445, #839 ) ;
#18184 = CARTESIAN_POINT ( 'NONE',  ( 5.958863334805807099, -7.853699934220021106, 18.96369761673806664 ) ) ;
#18185 = CARTESIAN_POINT ( 'NONE',  ( 0.5839254288179547281, 6.341681103465229619, -47.47429404163003142 ) ) ;
#18186 = CARTESIAN_POINT ( 'NONE',  ( 0.5797568665920713737, -8.419848931671534586, -46.13384281164643141 ) ) ;
#18187 = CARTESIAN_POINT ( 'NONE',  ( 50.50000000000000000, 12.21587082446438011, 2.649999999999992806 ) ) ;
#18188 = ADVANCED_FACE ( 'NONE', ( #11617 ), #44052, .F. ) ;
#18189 = CARTESIAN_POINT ( 'NONE',  ( 4.962356264823608143, 0.000000000000000000, 0.000000000000000000 ) ) ;
#18190 = ORIENTED_EDGE ( 'NONE', *, *, #29628, .F. ) ;
#18191 = B_SPLINE_CURVE_WITH_KNOTS ( 'NONE', 3,
 ( #30606, #58792, #15916, #12154, #2407, #35033, #49111, #16848, #59108, #6466, #35651, #11850, #6163, #25608, #21529, #26218, #16219, #35340, #54401 ),
 .UNSPECIFIED., .F., .F.,
 ( 4, 3, 3, 3, 3, 3, 4 ),
 ( 9.541595121948225732E-18, 0.0002732106629380579325, 0.0004098138914053724505, 0.0005464171197651436539, 0.0006830203481512533807, 0.0008196235766963599467, 0.001011968216111139643 ),
 .UNSPECIFIED. ) ;
#18192 = CARTESIAN_POINT ( 'NONE',  ( 0.8557997880470690211, 47.89938907511594124, -0.9121262075947851322 ) ) ;
#18193 = CARTESIAN_POINT ( 'NONE',  ( 0.5819845079324649229, 46.37938935563231269, 11.95724301473523710 ) ) ;
#18194 = CARTESIAN_POINT ( 'NONE',  ( 4.975610109902397937, -46.59897809419034331, -14.86555238512655919 ) ) ;
#18195 = CARTESIAN_POINT ( 'NONE',  ( 4.956445790444011124, -17.42806872899762993, -43.74700527484106516 ) ) ;
#18196 = ORIENTED_EDGE ( 'NONE', *, *, #54172, .T. ) ;
#18197 = EDGE_CURVE ( 'NONE', #34712, #38898, #1567, .T. ) ;
#18198 = FACE_OUTER_BOUND ( 'NONE', #10987, .T. ) ;
#18199 = CARTESIAN_POINT ( 'NONE',  ( 0.9775691876211000109, -41.78811875591999581, -3.175978562760820356 ) ) ;
#18200 = AXIS2_PLACEMENT_3D ( 'NONE', #47087, #24180, #47379 ) ;
#18201 = ADVANCED_FACE ( 'NONE', ( #35745 ), #18416, .F. ) ;
#18202 = SHAPE_REPRESENTATION_RELATIONSHIP ( 'NONE' , 'NONE' ,  #27649, #51224 ) ;
#18203 = CIRCLE ( 'NONE', #52213, 48.09070567114147110 ) ;
#18204 = ORIENTED_EDGE ( 'NONE', *, *, #43734, .F. ) ;
#18205 = CARTESIAN_POINT ( 'NONE',  ( -79.49999999999975842, 4.999999999999996447, 1.500000000000000444 ) ) ;
#18206 = CARTESIAN_POINT ( 'NONE',  ( 0.5837800304671223461, -45.94722522548352828, -9.385618054139468924 ) ) ;
#18207 = CARTESIAN_POINT ( 'NONE',  ( 0.5997462898726536595, 23.17609050332868037, 43.29457771044576475 ) ) ;
#18208 = ORIENTED_EDGE ( 'NONE', *, *, #11040, .F. ) ;
#18209 = CARTESIAN_POINT ( 'NONE',  ( 0.6025881611877910160, 29.11258673756362114, 38.29866377863849891 ) ) ;
#18210 = ORIENTED_EDGE ( 'NONE', *, *, #16843, .T. ) ;
#18211 = ORIENTED_EDGE ( 'NONE', *, *, #58835, .F. ) ;
#18212 = CARTESIAN_POINT ( 'NONE',  ( 4.694002226626920127, -10.47998749083556191, -44.36726984656667128 ) ) ;
#18213 = CARTESIAN_POINT ( 'NONE',  ( 0.2230388203127624258, 40.12182516270778621, 15.79641846944932304 ) ) ;
#18214 = ORIENTED_EDGE ( 'NONE', *, *, #27942, .F. ) ;
#18215 = CARTESIAN_POINT ( 'NONE',  ( 5.959828726073459926, 20.52560994243598813, 0.004526594003449061453 ) ) ;
#18216 = EDGE_CURVE ( 'NONE', #39044, #47897, #4717, .T. ) ;
#18217 = B_SPLINE_CURVE_WITH_KNOTS ( 'NONE', 3,
 ( #49783, #54775, #58859, #30665, #31605, #31296 ),
 .UNSPECIFIED., .F., .F.,
 ( 4, 2, 4 ),
 ( 1.910620358896493634E-17, 0.0002293755540694311288, 0.0004587511081388431214 ),
 .UNSPECIFIED. ) ;
#18218 = ORIENTED_EDGE ( 'NONE', *, *, #24526, .T. ) ;
#18219 = CARTESIAN_POINT ( 'NONE',  ( 4.962356264823608143, 42.01891079680549268, -2.376285612557975213 ) ) ;
#18220 =( BOUNDED_SURFACE ( )  B_SPLINE_SURFACE ( 3, 1, ( 
 ( #26007, #59193 ),
 ( #35421, #6239 ),
 ( #49189, #53869 ),
 ( #30078, #26310 ) ),
 .UNSPECIFIED., .F., .F., .F. ) 
 B_SPLINE_SURFACE_WITH_KNOTS ( ( 4, 4 ),
 ( 2, 2 ),
 ( 0.000000000000000000, 1.000000000000000000 ),
 ( 0.000000000000000000, 1.000000000000000000 ),
 .UNSPECIFIED. ) 
 GEOMETRIC_REPRESENTATION_ITEM ( )  RATIONAL_B_SPLINE_SURFACE ( (
 ( 1.000000000000000000, 1.000000000000000000),
 ( 0.7211978278499970862, 0.9934217856018976445),
 ( 0.7211978278499970862, 0.9934217856018976445),
 ( 1.000000000000000000, 1.000000000000000000) ) ) 
 REPRESENTATION_ITEM ( '' )  SURFACE ( )  );
#18221 = CARTESIAN_POINT ( 'NONE',  ( 2.526552050251864134, 15.32056541070842748, 40.15571433620791453 ) ) ;
#18222 = CARTESIAN_POINT ( 'NONE',  ( 4.975801465491694664, 15.94009207553051510, -45.18341283946441678 ) ) ;
#18223 = ORIENTED_EDGE ( 'NONE', *, *, #41201, .T. ) ;
#18224 =( BOUNDED_SURFACE ( )  B_SPLINE_SURFACE ( 3, 1, ( 
 ( #53947, #15151 ),
 ( #1321, #54556 ),
 ( #58641, #16077 ),
 ( #11686, #39277 ) ),
 .UNSPECIFIED., .F., .F., .F. ) 
 B_SPLINE_SURFACE_WITH_KNOTS ( ( 4, 4 ),
 ( 2, 2 ),
 ( 0.000000000000000000, 1.000000000000000000 ),
 ( 0.000000000000000000, 1.000000000000000000 ),
 .UNSPECIFIED. ) 
 GEOMETRIC_REPRESENTATION_ITEM ( )  RATIONAL_B_SPLINE_SURFACE ( (
 ( 1.000000000000000000, 1.000000000000000000),
 ( 0.9953390228620291325, 0.8624445117760984880),
 ( 0.9953390228620291325, 0.8624445117760984880),
 ( 1.000000000000000000, 1.000000000000000000) ) ) 
 REPRESENTATION_ITEM ( '' )  SURFACE ( )  );
#18225 = DIRECTION ( 'NONE',  ( 0.000000000000000000, 0.000000000000000000, 1.000000000000000000 ) ) ;
#18226 = CARTESIAN_POINT ( 'NONE',  ( 4.975801465491694664, -32.01766832630337944, 35.64402118370901462 ) ) ;
#18227 = DIRECTION ( 'NONE',  ( 0.000000000000000000, 0.000000000000000000, 1.000000000000000000 ) ) ;
#18228 = DIRECTION ( 'NONE',  ( 1.000000000000000000, -0.000000000000000000, -0.000000000000000000 ) ) ;
#18229 = EDGE_LOOP ( 'NONE', ( #20084, #8323, #24370, #49611 ) ) ;
#18230 = CARTESIAN_POINT ( 'NONE',  ( 4.962356264823603702, -4.645793755590432283, -41.82884409403234116 ) ) ;
#18231 = DIRECTION ( 'NONE',  ( 0.000000000000000000, 0.000000000000000000, 1.000000000000000000 ) ) ;
#18232 = VERTEX_POINT ( 'NONE', #7187 ) ;
#18233 = CARTESIAN_POINT ( 'NONE',  ( 4.967162193818130511, 23.56777426397178132, 36.06913038482807821 ) ) ;
#18234 = EDGE_LOOP ( 'NONE', ( #38462, #36088, #61051, #1841 ) ) ;
#18235 = CARTESIAN_POINT ( 'NONE',  ( 4.962356264823602814, -25.31392337492848554, -33.62202970123303203 ) ) ;
#18236 = CARTESIAN_POINT ( 'NONE',  ( 0.5817217712918340000, 11.31382783192066199, -45.51079271775027024 ) ) ;
#18237 = VERTEX_POINT ( 'NONE', #26318 ) ;
#18238 = CARTESIAN_POINT ( 'NONE',  ( 0.1064266379913938465, -37.62465837278060121, -21.07422113734149605 ) ) ;
#18239 = CARTESIAN_POINT ( 'NONE',  ( 4.956653778116974607, -32.11725092155068495, 35.79382859084104496 ) ) ;
#18240 = CARTESIAN_POINT ( 'NONE',  ( 0.7762783648524335112, 24.71864151483714167, 41.03453896757949337 ) ) ;
#18241 = CARTESIAN_POINT ( 'NONE',  ( 0.5832655196449136881, -1.339497008067653150, -46.87686989058363451 ) ) ;
#18242 = ORIENTED_EDGE ( 'NONE', *, *, #8364, .T. ) ;
#18243 = PLANE ( 'NONE',  #13971 ) ;
#18244 = CARTESIAN_POINT ( 'NONE',  ( 9.999999999999994671, 58.44237546506882808, -54.69470952477875869 ) ) ;
#18245 = EDGE_CURVE ( 'NONE', #22599, #29776, #54929, .T. ) ;
#18246 = CARTESIAN_POINT ( 'NONE',  ( 0.8760168074886960365, -19.22870327415332525, 44.09317760313719958 ) ) ;
#18247 = CARTESIAN_POINT ( 'NONE',  ( 0.6845945791218023269, 45.00526092843262660, -13.22622430921391690 ) ) ;
#18248 = AXIS2_PLACEMENT_3D ( 'NONE', #49291, #6347, #25483 ) ;
#18249 = EDGE_CURVE ( 'NONE', #47523, #48721, #4892, .T. ) ;
#18250 = CARTESIAN_POINT ( 'NONE',  ( 0.6000166863083090663, -25.90381862410858460, -41.72308308835457069 ) ) ;
#18251 = CARTESIAN_POINT ( 'NONE',  ( 4.975801465491695552, 0.000000000000000000, 0.000000000000000000 ) ) ;
#18252 = AXIS2_PLACEMENT_3D ( 'NONE', #36575, #11855, #51258 ) ;
#18253 = CARTESIAN_POINT ( 'NONE',  ( 1.088313998177379949, 39.93881167962123158, -15.69908095455111940 ) ) ;
#18254 = EDGE_CURVE ( 'NONE', #26937, #5500, #32265, .T. ) ;
#18255 = FACE_OUTER_BOUND ( 'NONE', #28344, .T. ) ;
#18256 = CARTESIAN_POINT ( 'NONE',  ( 0.5806925824938499181, 40.62497527030964051, -23.42720099863178973 ) ) ;
#18257 = CARTESIAN_POINT ( 'NONE',  ( 0.8551540677456715978, -46.03951182599436720, 13.28067116677186199 ) ) ;
#18258 = CARTESIAN_POINT ( 'NONE',  ( 0.8551540677456715978, -11.51835730326447127, -46.51172240253133339 ) ) ;
#18259 = CARTESIAN_POINT ( 'NONE',  ( 1.227938101723756947, 36.73927144310543014, -22.18841447410681411 ) ) ;
#18260 = CARTESIAN_POINT ( 'NONE',  ( 4.967162193818130511, -23.56777426397153974, -36.06913038482822742 ) ) ;
#18261 = CARTESIAN_POINT ( 'NONE',  ( 0.5850706913938534814, 18.49682194437964355, 44.18063951072227269 ) ) ;
#18262 = B_SPLINE_CURVE_WITH_KNOTS ( 'NONE', 3,
 ( #3028, #55333, #1789, #12456 ),
 .UNSPECIFIED., .F., .F.,
 ( 4, 4 ),
 ( 2.168404344971008868E-19, 0.004048833967417083887 ),
 .UNSPECIFIED. ) ;
#18263 = CARTESIAN_POINT ( 'NONE',  ( 2.706805983486679335, -21.38196053433432198, 38.46541143713302802 ) ) ;
#18264 = DIRECTION ( 'NONE',  ( 0.000000000000000000, 3.491481338843138088E-15, -1.000000000000000000 ) ) ;
#18265 = ADVANCED_FACE ( 'NONE', ( #12551 ), #54411, .F. ) ;
#18266 = CARTESIAN_POINT ( 'NONE',  ( 0.5835226383429291674, 45.18136229812504467, -12.56530840972593133 ) ) ;
#18267 = CARTESIAN_POINT ( 'NONE',  ( 0.5997462898726536595, -47.36625756029543055, 12.96106765957438789 ) ) ;
#18269 = ORIENTED_EDGE ( 'NONE', *, *, #17470, .F. ) ;
#18268 = CARTESIAN_POINT ( 'NONE',  ( -6.016489644550737204, -9.417787539062134172, -16.32089497094071717 ) ) ;
#18270 = ORIENTED_EDGE ( 'NONE', *, *, #45409, .T. ) ;
#18271 = FACE_OUTER_BOUND ( 'NONE', #7578, .T. ) ;
#18272 = CARTESIAN_POINT ( 'NONE',  ( 2.648799415243696664, 44.76338677751291328, -20.01890774983441545 ) ) ;
#18274 = EDGE_CURVE ( 'NONE', #19530, #41175, #31643, .T. ) ;
#18273 = CARTESIAN_POINT ( 'NONE',  ( 5.910764540655178756, -2.028561139976813976, -20.00965212517547087 ) ) ;
#18275 = ORIENTED_EDGE ( 'NONE', *, *, #23611, .F. ) ;
#18276 = ORIENTED_EDGE ( 'NONE', *, *, #19804, .T. ) ;
#18277 = LINE ( 'NONE', #28575, #48301 ) ;
#18278 = CARTESIAN_POINT ( 'NONE',  ( 0.1365634738349408572, 43.18335443710246579, 9.058726134663299234 ) ) ;
#18279 = EDGE_CURVE ( 'NONE', #4396, #49329, #21939, .T. ) ;
#18280 = VERTEX_POINT ( 'NONE', #60427 ) ;
#18281 = ORIENTED_EDGE ( 'NONE', *, *, #50552, .T. ) ;
#18282 = CARTESIAN_POINT ( 'NONE',  ( 0.6017667736363749853, -37.95278695280790515, -29.56223180955317886 ) ) ;
#18283 = DIRECTION ( 'NONE',  ( 0.000000000000000000, 0.000000000000000000, 1.000000000000000000 ) ) ;
#18284 = CARTESIAN_POINT ( 'NONE',  ( 4.975801465491695552, -8.787181743660504196, 47.10002938642126935 ) ) ;
#18285 = B_SPLINE_CURVE_WITH_KNOTS ( 'NONE', 3,
 ( #14672, #19672, #23748, #53761, #10578, #33785 ),
 .UNSPECIFIED., .F., .F.,
 ( 4, 2, 4 ),
 ( 1.511413994009955268E-16, 0.0002445252820015196235, 0.0004890505640028881091 ),
 .UNSPECIFIED. ) ;
#18286 = EDGE_LOOP ( 'NONE', ( #19621, #50971, #10799, #44867 ) ) ;
#18287 = ORIENTED_EDGE ( 'NONE', *, *, #25997, .F. ) ;
#18288 = CARTESIAN_POINT ( 'NONE',  ( 0.5839879327111923146, -12.48412918464404875, -46.24044206955234415 ) ) ;
#18289 = ORIENTED_EDGE ( 'NONE', *, *, #2318, .T. ) ;
#18290 = DIRECTION ( 'NONE',  ( 0.09835009131224564660, 0.1222230102474879260, 0.9876177374393978470 ) ) ;
#18291 = FACE_OUTER_BOUND ( 'NONE', #19814, .T. ) ;
#18292 = ADVANCED_FACE ( 'NONE', ( #41372 ), #831, .F. ) ;
#18293 = VECTOR ( 'NONE', #35454, 1000.000000000000000 ) ;
#18294 = CARTESIAN_POINT ( 'NONE',  ( 0.1102847568649952675, -30.55869130182088611, -30.42833243501139862 ) ) ;
#18295 = EDGE_LOOP ( 'NONE', ( #35724, #43954, #11531, #49496 ) ) ;
#18296 = EDGE_CURVE ( 'NONE', #27020, #20580, #49733, .T. ) ;
#18297 = B_SPLINE_CURVE_WITH_KNOTS ( 'NONE', 3,
 ( #19739, #39798, #29121, #5293, #28813, #43555, #48533, #25044, #39474, #44490, #4982, #598, #47936, #15662, #53528, #38862, #24114, #58531, #5590, #52923, #34764, #58222, #48240, #34151, #52608 ),
 .UNSPECIFIED., .F., .F.,
 ( 4, 3, 3, 3, 3, 3, 3, 3, 4 ),
 ( 5.553824967135426632E-18, 0.0005656085177311407242, 0.001131215744874500707, 0.001696821861372765916, 0.002262427090022498151, 0.002828031679238745492, 0.003393635864401604862, 0.003977030878808131623, 0.004561030005651159000 ),
 .UNSPECIFIED. ) ;
#18298 = CARTESIAN_POINT ( 'NONE',  ( 0.6027935024548037868, -48.10716172909472022, -0.1745403365869804269 ) ) ;
#18299 = VERTEX_POINT ( 'NONE', #26945 ) ;
#18300 = EDGE_LOOP ( 'NONE', ( #42494, #38339, #9119, #37561 ) ) ;
#18301 = CARTESIAN_POINT ( 'NONE',  ( 0.7044674535453004927, -0.7321618212258587111, 49.10465010442948852 ) ) ;
#18302 = B_SPLINE_CURVE_WITH_KNOTS ( 'NONE', 3,
 ( #59284, #8437, #27563, #3427, #12872, #45233 ),
 .UNSPECIFIED., .F., .F.,
 ( 4, 2, 4 ),
 ( 1.056081928668503685E-17, 0.0002291978881530153469, 0.0004583957763060201229 ),
 .UNSPECIFIED. ) ;
#18303 = ORIENTED_EDGE ( 'NONE', *, *, #3995, .T. ) ;
#18304 = CARTESIAN_POINT ( 'NONE',  ( 0.6064782688330874194, -8.500301393622592627, 46.12027019257743632 ) ) ;
#18305 = CARTESIAN_POINT ( 'NONE',  ( 0.8557997880470697982, 29.88293891557470516, 37.44587306708108088 ) ) ;
#18306 = CARTESIAN_POINT ( 'NONE',  ( 0.6025881611877910160, 34.17105830828415236, -33.86250327239859814 ) ) ;
#18307 = CARTESIAN_POINT ( 'NONE',  ( 0.5837157313716027085, -38.71448089223815003, 26.46556314962047907 ) ) ;
#18308 = CARTESIAN_POINT ( 'NONE',  ( 0.3676999524040366896, -43.84864779214676389, -4.821480075983068048 ) ) ;
#18309 = ORIENTED_EDGE ( 'NONE', *, *, #48130, .F. ) ;
#18310 = CARTESIAN_POINT ( 'NONE',  ( 0.5797568599927134247, 16.26612221817008930, 43.98452655939994571 ) ) ;
#18311 = CARTESIAN_POINT ( 'NONE',  ( 4.975801465491695552, 0.000000000000000000, 0.000000000000000000 ) ) ;
#18312 = CARTESIAN_POINT ( 'NONE',  ( 0.1101816497532063371, 39.78963561881064948, -16.62841624476636682 ) ) ;
#18313 = VECTOR ( 'NONE', #41479, 1000.000000000000000 ) ;
#18314 = VERTEX_POINT ( 'NONE', #46075 ) ;
#18315 = CARTESIAN_POINT ( 'NONE',  ( 1.091591847532197734, -21.89140366521357350, -35.74248783342470404 ) ) ;
#18316 = CARTESIAN_POINT ( 'NONE',  ( 0.9968887458511631605, -26.64009929991527059, 33.63815526548975043 ) ) ;
#18317 = CARTESIAN_POINT ( 'NONE',  ( 4.553261556744875094, 40.80044851610500700, -16.27461110774390818 ) ) ;
#18318 = CARTESIAN_POINT ( 'NONE',  ( -6.078726893082806448, 13.83492043373091995, 13.39361854993096124 ) ) ;
#18319 = B_SPLINE_CURVE_WITH_KNOTS ( 'NONE', 3,
 ( #25913, #39730, #58779, #35022 ),
 .UNSPECIFIED., .F., .F.,
 ( 4, 4 ),
 ( 1.999757930724972237E-17, 0.004444306975806117631 ),
 .UNSPECIFIED. ) ;
#18320 = ORIENTED_EDGE ( 'NONE', *, *, #44937, .F. ) ;
#18321 = CARTESIAN_POINT ( 'NONE',  ( 4.963659409799330291, 44.62477100936222030, -3.403493583736868278 ) ) ;
#18322 = CARTESIAN_POINT ( 'NONE',  ( 0.1073791018717483448, -5.147744207007177053, 42.81622261970985477 ) ) ;
#18323 = EDGE_CURVE ( 'NONE', #30839, #32393, #60933, .T. ) ;
#18324 = CARTESIAN_POINT ( 'NONE',  ( 5.959547316686252039, -10.26589671991350983, -17.77392908783930636 ) ) ;
#18325 = PRODUCT_DEFINITION_SHAPE ( 'NONE', 'NONE',  #16454 ) ;
#18326 = CARTESIAN_POINT ( 'NONE',  ( 0.5998501479064699549, -6.798102206413803472, -47.62484632993685807 ) ) ;
#18327 = EDGE_CURVE ( 'NONE', #11505, #38319, #51160, .T. ) ;
#18328 = CARTESIAN_POINT ( 'NONE',  ( -5.995132425357893702, -4.885449473615459226, 18.19985213254570766 ) ) ;
#18329 = CARTESIAN_POINT ( 'NONE',  ( 5.974727161628369032, 10.27590650342037293, -17.76736931401850228 ) ) ;
#18330 = CARTESIAN_POINT ( 'NONE',  ( -2.708315649062916552, 9.116606751444184198, 11.44805714186574619 ) ) ;
#18331 = CARTESIAN_POINT ( 'NONE',  ( -2.569797478183783568, -14.24379821351254982, -3.352038560005866863 ) ) ;
#18332 = CARTESIAN_POINT ( 'NONE',  ( 0.5998501479064699549, 29.69975237324562656, 37.84527566984866809 ) ) ;
#18333 = ADVANCED_FACE ( 'NONE', ( #46995 ), #58809, .F. ) ;
#18334 = CARTESIAN_POINT ( 'NONE',  ( 0.9789233960466705575, -1.268941605393027805, -41.88945588133657338 ) ) ;
#18335 = EDGE_CURVE ( 'NONE', #3780, #52994, #56971, .T. ) ;
#18336 = CARTESIAN_POINT ( 'NONE',  ( 5.958863334805807099, 10.26388325355063103, 17.77512673691322576 ) ) ;
#18337 = ORIENTED_EDGE ( 'NONE', *, *, #269, .F. ) ;
#18338 = ADVANCED_FACE ( 'NONE', ( #5265 ), #4029, .F. ) ;
#18339 = CARTESIAN_POINT ( 'NONE',  ( 0.5997462898726536595, 32.62638226927734308, -36.70246327105708417 ) ) ;
#18340 = CARTESIAN_POINT ( 'NONE',  ( 0.8760168074886965917, 29.98565522133346661, -37.61398439004502592 ) ) ;
#18341 = CARTESIAN_POINT ( 'NONE',  ( 2.301430502907646058, -4.990893951996671518, -47.77346269870098894 ) ) ;
#18342 = CARTESIAN_POINT ( 'NONE',  ( 3.270143674763207553, -3.806843787666013945, 13.14781761974168006 ) ) ;
#18343 = VECTOR ( 'NONE', #38714, 1000.000000000000114 ) ;
#18344 = CARTESIAN_POINT ( 'NONE',  ( 0.8551540677456715978, 0.9122407826482503701, -47.90804413217340141 ) ) ;
#18345 = LINE ( 'NONE', #56527, #59886 ) ;
#18346 = EDGE_CURVE ( 'NONE', #42579, #6671, #14093, .T. ) ;
#18347 =( BOUNDED_SURFACE ( )  B_SPLINE_SURFACE ( 3, 1, ( 
 ( #22700, #60901 ),
 ( #26552, #40375 ),
 ( #46839, #31256 ),
 ( #8911, #18015 ) ),
 .UNSPECIFIED., .F., .F., .F. ) 
 B_SPLINE_SURFACE_WITH_KNOTS ( ( 4, 4 ),
 ( 2, 2 ),
 ( 0.000000000000000000, 1.000000000000000000 ),
 ( 0.000000000000000000, 1.000000000000000000 ),
 .UNSPECIFIED. ) 
 GEOMETRIC_REPRESENTATION_ITEM ( )  RATIONAL_B_SPLINE_SURFACE ( (
 ( 1.000000000000000000, 1.000000000000000000),
 ( 0.7269869731126817891, 0.9931720237060910339),
 ( 0.7269869731126817891, 0.9931720237060910339),
 ( 1.000000000000000000, 1.000000000000000000) ) ) 
 REPRESENTATION_ITEM ( '' )  SURFACE ( )  );
#18348 = CARTESIAN_POINT ( 'NONE',  ( 6.999999999999991118, 80.00000000000001421, -7.414830285890871171E-32 ) ) ;
#18349 = CARTESIAN_POINT ( 'NONE',  ( 0.6039202388192953519, -42.70269169458240555, 24.24961514924382655 ) ) ;
#18351 = ORIENTED_EDGE ( 'NONE', *, *, #26090, .T. ) ;
#18350 = CARTESIAN_POINT ( 'NONE',  ( 1.154321713695927842, -6.418927679455929791, 42.43366804783613588 ) ) ;
#18352 = VERTEX_POINT ( 'NONE', #33197 ) ;
#18353 = CARTESIAN_POINT ( 'NONE',  ( 0.1092565886968784594, -43.12345370280014123, 0.3103822814778426920 ) ) ;
#18354 = CARTESIAN_POINT ( 'NONE',  ( 0.7044674535453004927, -7.005514063659647128, 48.60787483026567912 ) ) ;
#18355 = FACE_OUTER_BOUND ( 'NONE', #49393, .T. ) ;
#18356 = ORIENTED_EDGE ( 'NONE', *, *, #36962, .F. ) ;
#18357 = CARTESIAN_POINT ( 'NONE',  ( 0.5806925824938502512, 23.01490136172913026, 40.85996423950273737 ) ) ;
#18359 = DIRECTION ( 'NONE',  ( 1.000000000000000000, 0.000000000000000000, -0.000000000000000000 ) ) ;
#18358 = VECTOR ( 'NONE', #39389, 1000.000000000000114 ) ;
#18360 = CARTESIAN_POINT ( 'NONE',  ( 0.6031357023905875581, -44.42879114414645159, -18.45021748202266920 ) ) ;
#18361 = ORIENTED_EDGE ( 'NONE', *, *, #23229, .F. ) ;
#18362 = ORIENTED_EDGE ( 'NONE', *, *, #48926, .F. ) ;
#18363 = CARTESIAN_POINT ( 'NONE',  ( 0.9752132459055862235, 41.50604997043411970, 10.88033124649634686 ) ) ;
#18364 = CARTESIAN_POINT ( 'NONE',  ( 0.7242003506640013466, -20.62185031759747389, -44.56176571461944746 ) ) ;
#18365 = CARTESIAN_POINT ( 'NONE',  ( 5.000000000000007994, -56.56854249492410958, 56.56854249492351983 ) ) ;
#18366 = DIRECTION ( 'NONE',  ( -1.000000000000000000, -0.000000000000000000, -0.000000000000000000 ) ) ;
#18367 = EDGE_CURVE ( 'NONE', #35355, #18514, #1126, .T. ) ;
#18368 = CARTESIAN_POINT ( 'NONE',  ( 0.5804410086790514622, 42.96136033320073011, -18.81067170986419157 ) ) ;
#18369 = EDGE_CURVE ( 'NONE', #40746, #60982, #37596, .T. ) ;
#18370 = CARTESIAN_POINT ( 'NONE',  ( 0.7048096507298635682, 17.62869676200410396, -44.76417498422297570 ) ) ;
#18371 = EDGE_LOOP ( 'NONE', ( #14098, #56883, #20608, #20746 ) ) ;
#18372 = CARTESIAN_POINT ( 'NONE',  ( 4.549368137175248350, -42.82045902618774136, 3.018832571115817487 ) ) ;
#18373 = EDGE_LOOP ( 'NONE', ( #57095, #48313, #6237, #3454 ) ) ;
#18374 = DIRECTION ( 'NONE',  ( 0.000000000000000000, 0.000000000000000000, 1.000000000000000000 ) ) ;
#18375 = CARTESIAN_POINT ( 'NONE',  ( 0.7044674535453004927, 44.60554499456272026, 20.54624244354541673 ) ) ;
#18376 = CARTESIAN_POINT ( 'NONE',  ( 4.549368137175248350, 42.14271863032822552, 8.166781970325878603 ) ) ;
#18377 = B_SPLINE_CURVE_WITH_KNOTS ( 'NONE', 3,
 ( #39584, #54247, #38659, #57714 ),
 .UNSPECIFIED., .F., .F.,
 ( 4, 4 ),
 ( 0.000000000000000000, 0.005013413432710142441 ),
 .UNSPECIFIED. ) ;
#18378 = ORIENTED_EDGE ( 'NONE', *, *, #25168, .T. ) ;
#18379 = EDGE_LOOP ( 'NONE', ( #32883, #4917, #59902, #18351 ) ) ;
#18380 = CARTESIAN_POINT ( 'NONE',  ( 0.9757954354143116849, 5.207268878499845415E-15, 42.90846090505964128 ) ) ;
#18381 = PLANE ( 'NONE',  #50996 ) ;
#18382 = CARTESIAN_POINT ( 'NONE',  ( 0.6039202388192952409, 16.79650288729614616, 46.14586875990139703 ) ) ;
#18383 = ORIENTED_EDGE ( 'NONE', *, *, #42592, .T. ) ;
#18384 = FACE_OUTER_BOUND ( 'NONE', #56191, .T. ) ;
#18385 = VERTEX_POINT ( 'NONE', #13787 ) ;
#18386 = DIRECTION ( 'NONE',  ( -0.000000000000000000, 0.000000000000000000, -1.000000000000000000 ) ) ;
#18387 = CARTESIAN_POINT ( 'NONE',  ( 0.5830082357119567016, 27.59734378305546798, 37.91594191178936768 ) ) ;
#18388 = CARTESIAN_POINT ( 'NONE',  ( 0.1156495703730067715, 36.90540492852111498, -24.18540965733181736 ) ) ;
#18389 = EDGE_LOOP ( 'NONE', ( #54253, #25615, #49485, #31408 ) ) ;
#18390 = CARTESIAN_POINT ( 'NONE',  ( 0.5819845079324659221, -47.54334065046000291, -5.801222053075574259 ) ) ;
#18391 = CARTESIAN_POINT ( 'NONE',  ( 2.618530812446111078, -2.977833924574445401, 46.91331681213611660 ) ) ;
#18392 = CARTESIAN_POINT ( 'NONE',  ( 0.5837157313716014873, -41.89656481236102792, 21.06928856192482158 ) ) ;
#18393 = EDGE_CURVE ( 'NONE', #45374, #21079, #45827, .T. ) ;
#18394 =( BOUNDED_SURFACE ( )  B_SPLINE_SURFACE ( 3, 1, ( 
 ( #36042, #55104 ),
 ( #31312, #50415 ),
 ( #26607, #21922 ),
 ( #9043, #13772 ) ),
 .UNSPECIFIED., .F., .F., .F. ) 
 B_SPLINE_SURFACE_WITH_KNOTS ( ( 4, 4 ),
 ( 2, 2 ),
 ( 0.000000000000000000, 1.000000000000000000 ),
 ( 0.000000000000000000, 1.000000000000000000 ),
 .UNSPECIFIED. ) 
 GEOMETRIC_REPRESENTATION_ITEM ( )  RATIONAL_B_SPLINE_SURFACE ( (
 ( 1.000000000000000000, 1.000000000000000000),
 ( 0.9751682680413298332, 0.9999560080971552356),
 ( 0.9751682680413298332, 0.9999560080971552356),
 ( 1.000000000000000000, 1.000000000000000000) ) ) 
 REPRESENTATION_ITEM ( '' )  SURFACE ( )  );
#18395 = ORIENTED_EDGE ( 'NONE', *, *, #32993, .T. ) ;
#18396 = CARTESIAN_POINT ( 'NONE',  ( 0.5998501479064699549, -29.69975237324587169, -37.84527566984847624 ) ) ;
#18397 = DIRECTION ( 'NONE',  ( -1.836909530733573776E-16, 1.000000000000000000, 0.000000000000000000 ) ) ;
#18398 = LINE ( 'NONE', #36279, #51176 ) ;
#18399 = CARTESIAN_POINT ( 'NONE',  ( 0.8557997880470697982, -11.51622788066490166, 46.50333260518556244 ) ) ;
#18400 = CARTESIAN_POINT ( 'NONE',  ( 0.1100053167205930910, 16.33707796615706442, -39.91014771056761390 ) ) ;
#18401 = VERTEX_POINT ( 'NONE', #574 ) ;
#18402 = ADVANCED_FACE ( 'NONE', ( #33506 ), #45674, .F. ) ;
#18403 = CARTESIAN_POINT ( 'NONE',  ( 0.6064782688330866423, -42.17225498498755343, 20.51427200511784577 ) ) ;
#18404 = EDGE_CURVE ( 'NONE', #17462, #15825, #25102, .T. ) ;
#18405 = CARTESIAN_POINT ( 'NONE',  ( 2.500000000000000000, 1.178949249685212974, -2.042000000000001148 ) ) ;
#18406 = ORIENTED_EDGE ( 'NONE', *, *, #48030, .T. ) ;
#18407 = EDGE_CURVE ( 'NONE', #37210, #38521, #16543, .T. ) ;
#18408 = CARTESIAN_POINT ( 'NONE',  ( 5.895596859100789899, 10.82540956478658423, 16.95106754653271608 ) ) ;
#18409 = CARTESIAN_POINT ( 'NONE',  ( 0.9780303403264778428, -26.80931777084100887, 32.21180054044096863 ) ) ;
#18410 = CARTESIAN_POINT ( 'NONE',  ( 0.9747592971366236814, 5.279515277919996308, -42.58247319705097311 ) ) ;
#18411 = CARTESIAN_POINT ( 'NONE',  ( 0.5797568599927138688, -7.179075611191181316, -46.34313522022226550 ) ) ;
#18412 = CARTESIAN_POINT ( 'NONE',  ( 7.000000000000021316, -80.00000000000001421, 2.649999999999999467 ) ) ;
#18413 = CARTESIAN_POINT ( 'NONE',  ( 53.01450034489953111, 15.47727011842658307, 0.8544031610831416268 ) ) ;
#18414 = DIRECTION ( 'NONE',  ( 0.000000000000000000, 0.000000000000000000, 1.000000000000000000 ) ) ;
#18415 = CARTESIAN_POINT ( 'NONE',  ( 0.6031356755773454870, 47.69588082432148468, 6.279255973231509635 ) ) ;
#18416 =( BOUNDED_SURFACE ( )  B_SPLINE_SURFACE ( 3, 1, ( 
 ( #20700, #16306 ),
 ( #58893, #16011 ),
 ( #35433, #49818 ),
 ( #31024, #6879 ) ),
 .UNSPECIFIED., .F., .F., .F. ) 
 B_SPLINE_SURFACE_WITH_KNOTS ( ( 4, 4 ),
 ( 2, 2 ),
 ( 0.000000000000000000, 1.000000000000000000 ),
 ( 0.000000000000000000, 1.000000000000000000 ),
 .UNSPECIFIED. ) 
 GEOMETRIC_REPRESENTATION_ITEM ( )  RATIONAL_B_SPLINE_SURFACE ( (
 ( 1.000000000000000000, 1.000000000000000000),
 ( 0.9953485035131437453, 0.8621029689291515030),
 ( 0.9953485035131437453, 0.8621029689291515030),
 ( 1.000000000000000000, 1.000000000000000000) ) ) 
 REPRESENTATION_ITEM ( '' )  SURFACE ( )  );
#18417 = DIRECTION ( 'NONE',  ( 0.000000000000000000, 0.000000000000000000, -1.000000000000000000 ) ) ;
#18418 = CARTESIAN_POINT ( 'NONE',  ( 0.1084644655670280594, -5.234391617064312108, 42.80575641816238885 ) ) ;
#18419 = ORIENTED_EDGE ( 'NONE', *, *, #51327, .F. ) ;
#18420 = CARTESIAN_POINT ( 'NONE',  ( 7.999999999999996447, 1.469527624586858429E-15, -1.540743955509788245E-31 ) ) ;
#18421 = CARTESIAN_POINT ( 'NONE',  ( 5.959547316686252039, 18.96183906913532269, 7.858107265727816149 ) ) ;
#18422 = CARTESIAN_POINT ( 'NONE',  ( 47.98575327796820744, 15.47722964620001385, -0.8550501376822413624 ) ) ;
#18423 = CARTESIAN_POINT ( 'NONE',  ( 1.231276596079881047, -16.87422718933157739, -38.37365278131454005 ) ) ;
#18424 = FACE_OUTER_BOUND ( 'NONE', #56301, .T. ) ;
#18425 = CARTESIAN_POINT ( 'NONE',  ( 1.657374760986085827, 32.73027908137574826, -29.48930786755600408 ) ) ;
#18426 = EDGE_LOOP ( 'NONE', ( #12286, #40116, #11, #45663 ) ) ;
#18427 = CARTESIAN_POINT ( 'NONE',  ( 0.9730545539215883499, -29.98130006528840141, -30.69604515769682251 ) ) ;
#18428 = B_SPLINE_CURVE_WITH_KNOTS ( 'NONE', 3,
 ( #57618, #14750, #18213, #32936, #33865, #10042 ),
 .UNSPECIFIED., .F., .F.,
 ( 4, 2, 4 ),
 ( 8.461795104084953648E-17, 0.0002293366620881437921, 0.0004586733241762029623 ),
 .UNSPECIFIED. ) ;
#18429 = CARTESIAN_POINT ( 'NONE',  ( 1.479689385636123067, 28.74311660336230645, -33.39786060802713052 ) ) ;
#18430 = CARTESIAN_POINT ( 'NONE',  ( 1.830465331921978134, -18.95265478904632062, 39.76396524902450835 ) ) ;
#18431 = ORIENTED_EDGE ( 'NONE', *, *, #28422, .F. ) ;
#18432 = CARTESIAN_POINT ( 'NONE',  ( 4.960156602257181468, -20.07163247083176572, 41.85906677498953599 ) ) ;
#18433 = VECTOR ( 'NONE', #6092, 1000.000000000000227 ) ;
#18434 = CARTESIAN_POINT ( 'NONE',  ( 0.6845945791218034371, 45.00526092843242054, 13.22622430921456349 ) ) ;
#18435 = ORIENTED_EDGE ( 'NONE', *, *, #56390, .F. ) ;
#18436 = EDGE_CURVE ( 'NONE', #40643, #19013, #58646, .T. ) ;
#18437 = LINE ( 'NONE', #23134, #21997 ) ;
#18438 = EDGE_LOOP ( 'NONE', ( #41725, #51784, #34600 ) ) ;
#18439 = CARTESIAN_POINT ( 'NONE',  ( 4.322998006666179727, 47.94177812210864431, -2.120302895115782515 ) ) ;
#18440 = CARTESIAN_POINT ( 'NONE',  ( -1.321505333908964186, 3.855830693249140850, -5.565789719053469753 ) ) ;
#18441 = ORIENTED_EDGE ( 'NONE', *, *, #17415, .F. ) ;
#18442 = CARTESIAN_POINT ( 'NONE',  ( 3.782542959838398389, -29.99487845573544931, -29.45411889400579142 ) ) ;
#18443 = CARTESIAN_POINT ( 'NONE',  ( 4.967162193818130511, 0.000000000000000000, 0.000000000000000000 ) ) ;
#18444 = ORIENTED_EDGE ( 'NONE', *, *, #45080, .F. ) ;
#18445 = CARTESIAN_POINT ( 'NONE',  ( 0.5817216825391123836, -8.248784698831615358, -46.16484055208877635 ) ) ;
#18446 = CARTESIAN_POINT ( 'NONE',  ( -6.078457390727109555, 19.09737280526037040, -2.466751502362881876 ) ) ;
#18447 =( REPRESENTATION_RELATIONSHIP ('NONE','NONE', #44881, #53251 ) REPRESENTATION_RELATIONSHIP_WITH_TRANSFORMATION ( #29875 )SHAPE_REPRESENTATION_RELATIONSHIP( ) );
#18448 = ORIENTED_EDGE ( 'NONE', *, *, #45014, .T. ) ;
#18449 = CARTESIAN_POINT ( 'NONE',  ( 4.999999999999997335, 0.000000000000000000, 0.000000000000000000 ) ) ;
#18450 = EDGE_LOOP ( 'NONE', ( #20386, #43809, #55922, #6461, #36152 ) ) ;
#18451 = DIRECTION ( 'NONE',  ( 0.07906939808003035641, -0.7773121955653229387, -0.6241264142084348432 ) ) ;
#18452 = ORIENTED_EDGE ( 'NONE', *, *, #53573, .T. ) ;
#18453 = ORIENTED_EDGE ( 'NONE', *, *, #29071, .T. ) ;
#18454 = CARTESIAN_POINT ( 'NONE',  ( 0.5997462898726536595, -43.04230894295718457, -23.64130434225950950 ) ) ;
#18455 = CARTESIAN_POINT ( 'NONE',  ( 5.960721111146673579, -18.96073515164554379, 7.860635756377555516 ) ) ;
#18456 = CARTESIAN_POINT ( 'NONE',  ( 0.9757787079277447928, 34.01751575780821213, 26.15233402543277208 ) ) ;
#18457 = CARTESIAN_POINT ( 'NONE',  ( 3.782625744892854414, 41.39849240246781648, -7.307730899384353940 ) ) ;
#18458 = VERTEX_POINT ( 'NONE', #1192 ) ;
#18459 = CARTESIAN_POINT ( 'NONE',  ( 0.8554163680231738898, -30.98316862405949124, 35.23136010892731207 ) ) ;
#18460 = DIRECTION ( 'NONE',  ( 1.000000000000000000, -0.000000000000000000, -0.000000000000000000 ) ) ;
#18461 = B_SPLINE_CURVE_WITH_KNOTS ( 'NONE', 3,
 ( #6167, #29386, #11218, #20614 ),
 .UNSPECIFIED., .F., .F.,
 ( 4, 4 ),
 ( 8.673617379884035472E-19, 0.004048833967417084755 ),
 .UNSPECIFIED. ) ;
#18462 = EDGE_LOOP ( 'NONE', ( #55432, #2946, #18444, #35383 ) ) ;
#18463 = ADVANCED_FACE ( 'NONE', ( #5874 ), #43672, .F. ) ;
#18464 = ORIENTED_EDGE ( 'NONE', *, *, #51799, .T. ) ;
#18465 = CARTESIAN_POINT ( 'NONE',  ( 4.975801465491694664, -47.84403947906841381, 2.564218696447319257 ) ) ;
#18466 = CARTESIAN_POINT ( 'NONE',  ( 4.956445790443495092, 1.033212179477288384, -47.07940656732829865 ) ) ;
#18467 = DIRECTION ( 'NONE',  ( -0.1736481776669312471, 0.9848077530122077983, -5.551115123125779621E-17 ) ) ;
#18469 = AXIS2_PLACEMENT_3D ( 'NONE', #15380, #1551, #34483 ) ;
#18468 = CARTESIAN_POINT ( 'NONE',  ( 0.2940135542859019235, -42.46217170869496726, 11.96680920181833763 ) ) ;
#18470 = ADVANCED_FACE ( 'NONE', ( #10615 ), #9244, .F. ) ;
#18471 = VERTEX_POINT ( 'NONE', #5569 ) ;
#18472 = EDGE_CURVE ( 'NONE', #61919, #10554, #47406, .T. ) ;
#18473 = CARTESIAN_POINT ( 'NONE',  ( -6.057079549204054558, 7.787131596469658135, -17.61226313109710517 ) ) ;
#18474 = CARTESIAN_POINT ( 'NONE',  ( 49.32574372153255382, 15.31603864467538934, 2.381899414255259639 ) ) ;
#18475 = CIRCLE ( 'NONE', #36507, 15.71999999999999709 ) ;
#18476 = CARTESIAN_POINT ( 'NONE',  ( 0.5835871038041861025, -41.79378696274027050, -21.27237232220663543 ) ) ;
#18477 = CARTESIAN_POINT ( 'NONE',  ( 0.5998501479064708430, 24.50586714782604858, -41.39809967730462859 ) ) ;
#18478 =( LENGTH_UNIT ( ) NAMED_UNIT ( * ) SI_UNIT ( .MILLI., .METRE. ) );
#18479 = CARTESIAN_POINT ( 'NONE',  ( 4.549368137175248350, -42.14271863032838894, 8.166781970325002860 ) ) ;
#18480 = ORIENTED_EDGE ( 'NONE', *, *, #13606, .F. ) ;
#18481 = CARTESIAN_POINT ( 'NONE',  ( -1.500000000000001332, 6.775741118407465085E-16, 5.453125000000000000 ) ) ;
#18482 = LINE ( 'NONE', #42309, #26609 ) ;
#18483 =( BOUNDED_SURFACE ( )  B_SPLINE_SURFACE ( 3, 1, ( 
 ( #24557, #38987 ),
 ( #18953, #107 ),
 ( #19255, #57420 ),
 ( #48664, #33661 ) ),
 .UNSPECIFIED., .F., .F., .F. ) 
 B_SPLINE_SURFACE_WITH_KNOTS ( ( 4, 4 ),
 ( 2, 2 ),
 ( 0.000000000000000000, 1.000000000000000000 ),
 ( 0.000000000000000000, 1.000000000000000000 ),
 .UNSPECIFIED. ) 
 GEOMETRIC_REPRESENTATION_ITEM ( )  RATIONAL_B_SPLINE_SURFACE ( (
 ( 1.000000000000000000, 1.000000000000000000),
 ( 0.9952954269826590483, 0.8620686068821339365),
 ( 0.9952954269826590483, 0.8620686068821339365),
 ( 1.000000000000000000, 1.000000000000000000) ) ) 
 REPRESENTATION_ITEM ( '' )  SURFACE ( )  );
#18484 = CARTESIAN_POINT ( 'NONE',  ( 2.282803330402962683, -9.105509439560925955, 46.08238931851357023 ) ) ;
#18486 = ADVANCED_FACE ( 'NONE', ( #39446 ), #28819, .F. ) ;
#18485 = CARTESIAN_POINT ( 'NONE',  ( 4.975801465491695552, 21.70134120755140827, 42.71626295676271212 ) ) ;
#18487 = CARTESIAN_POINT ( 'NONE',  ( 0.9790320750461898314, 29.07273748896853860, 30.18464953316030730 ) ) ;
#18488 = CARTESIAN_POINT ( 'NONE',  ( 4.691466044806102076, -36.88741755356052465, -25.04870410140776116 ) ) ;
#18489 = EDGE_CURVE ( 'NONE', #7406, #22531, #34429, .T. ) ;
#18490 = CARTESIAN_POINT ( 'NONE',  ( 7.000000000000022204, -85.00000000000001421, -1.348150961071066192E-31 ) ) ;
#18491 = B_SPLINE_CURVE_WITH_KNOTS ( 'NONE', 3,
 ( #19805, #24170, #43621, #34209, #10397, #32983, #56750, #9147, #23873, #28872, #18883, #28255, #10085, #29180, #4417, #29488, #52056, #13875, #23557 ),
 .UNSPECIFIED., .F., .F.,
 ( 4, 3, 3, 3, 3, 3, 4 ),
 ( 0.000000000000000000, 0.0002724573126191776528, 0.0004086839781548526514, 0.0005449106435901898346, 0.0006811373090491660946, 0.0008459866663933752291, 0.001010840725717213149 ),
 .UNSPECIFIED. ) ;
#18492 = CARTESIAN_POINT ( 'NONE',  ( 4.956653778116991482, -2.599733001514001440, -48.02038484091103498 ) ) ;
#18493 = CIRCLE ( 'NONE', #12512, 43.92652462719577500 ) ;
#18494 = DIRECTION ( 'NONE',  ( 0.000000000000000000, 0.000000000000000000, 1.000000000000000000 ) ) ;
#18495 = EDGE_LOOP ( 'NONE', ( #5526, #46709, #2068, #56186 ) ) ;
#18496 =( BOUNDED_SURFACE ( )  B_SPLINE_SURFACE ( 3, 1, ( 
 ( #19568, #29562 ),
 ( #53357, #10467 ),
 ( #33981, #38997 ),
 ( #26034, #53055 ) ),
 .UNSPECIFIED., .F., .F., .F. ) 
 B_SPLINE_SURFACE_WITH_KNOTS ( ( 4, 4 ),
 ( 2, 2 ),
 ( 0.000000000000000000, 1.000000000000000000 ),
 ( 0.000000000000000000, 1.000000000000000000 ),
 .UNSPECIFIED. ) 
 GEOMETRIC_REPRESENTATION_ITEM ( )  RATIONAL_B_SPLINE_SURFACE ( (
 ( 1.000000000000000000, 1.000000000000000000),
 ( 0.7211978278499968642, 0.9934217856018975334),
 ( 0.7211978278499968642, 0.9934217856018975334),
 ( 1.000000000000000000, 1.000000000000000000) ) ) 
 REPRESENTATION_ITEM ( '' )  SURFACE ( )  );
#18497 = LINE ( 'NONE', #22274, #52882 ) ;
#18498 = CARTESIAN_POINT ( 'NONE',  ( 0.9783242366443545279, 19.90500434199885760, 36.87987652299737107 ) ) ;
#18499 = CARTESIAN_POINT ( 'NONE',  ( -6.015611763856276717, 16.32183393015609951, -9.416239407363130809 ) ) ;
#18500 = ORIENTED_EDGE ( 'NONE', *, *, #53581, .F. ) ;
#18501 =( BOUNDED_SURFACE ( )  B_SPLINE_SURFACE ( 3, 1, ( 
 ( #39959, #6066 ),
 ( #60172, #45804 ),
 ( #25201, #59014 ),
 ( #44642, #29900 ) ),
 .UNSPECIFIED., .F., .F., .F. ) 
 B_SPLINE_SURFACE_WITH_KNOTS ( ( 4, 4 ),
 ( 2, 2 ),
 ( 0.000000000000000000, 1.000000000000000000 ),
 ( 0.000000000000000000, 1.000000000000000000 ),
 .UNSPECIFIED. ) 
 GEOMETRIC_REPRESENTATION_ITEM ( )  RATIONAL_B_SPLINE_SURFACE ( (
 ( 1.000000000000000000, 1.000000000000000000),
 ( 0.9953485035131437453, 0.8621029689291515030),
 ( 0.9953485035131437453, 0.8621029689291515030),
 ( 1.000000000000000000, 1.000000000000000000) ) ) 
 REPRESENTATION_ITEM ( '' )  SURFACE ( )  );
#18502 = CARTESIAN_POINT ( 'NONE',  ( 4.833616638992208614, 9.466882727841500866, 45.27110352095250789 ) ) ;
#18503 = DIRECTION ( 'NONE',  ( -1.000000000000000000, 0.000000000000000000, 0.000000000000000000 ) ) ;
#18504 = PRESENTATION_STYLE_ASSIGNMENT (( #23201 ) ) ;
#18505 = ORIENTED_EDGE ( 'NONE', *, *, #21420, .T. ) ;
#18506 = CARTESIAN_POINT ( 'NONE',  ( -2.601141883200665639, -11.68881050534876387, -9.282625514337903283 ) ) ;
#18507 = EDGE_CURVE ( 'NONE', #20977, #13708, #29704, .T. ) ;
#18508 = DIRECTION ( 'NONE',  ( 0.000000000000000000, -0.7071067811865553443, 0.7071067811865395791 ) ) ;
#18509 = AXIS2_PLACEMENT_3D ( 'NONE', #13227, #41747, #26693 ) ;
#18510 = FACE_OUTER_BOUND ( 'NONE', #10742, .T. ) ;
#18511 = EDGE_LOOP ( 'NONE', ( #5495, #30502, #42483, #24901 ) ) ;
#18512 = CARTESIAN_POINT ( 'NONE',  ( 4.549368137175248350, 2.596185425821941894, -42.84816078363927971 ) ) ;
#18513 = CONICAL_SURFACE ( 'NONE', #60474, 42.08604991992415023, 1.569615340895231137 ) ;
#18514 = VERTEX_POINT ( 'NONE', #25627 ) ;
#18515 = ORIENTED_EDGE ( 'NONE', *, *, #26763, .F. ) ;
#18516 = CARTESIAN_POINT ( 'NONE',  ( 0.5809828226811553087, -6.791453954330003207, -47.41188724015886180 ) ) ;
#18517 = DIRECTION ( 'NONE',  ( 0.000000000000000000, 0.000000000000000000, 1.000000000000000000 ) ) ;
#18518 = ORIENTED_EDGE ( 'NONE', *, *, #61136, .T. ) ;
#18519 = CARTESIAN_POINT ( 'NONE',  ( 0.6846871229502899947, -47.90045233486065968, 0.8641397935257868479 ) ) ;
#18520 = VECTOR ( 'NONE', #45969, 1000.000000000000000 ) ;
#18521 = VERTEX_POINT ( 'NONE', #44765 ) ;
#18522 = CARTESIAN_POINT ( 'NONE',  ( -6.079354080745853928, -1.850179728782696875, 19.16689307684904264 ) ) ;
#18523 = CARTESIAN_POINT ( 'NONE',  ( 4.549368137175248350, 35.57418903283115696, -24.02461520945233531 ) ) ;
#18524 = ORIENTED_EDGE ( 'NONE', *, *, #39217, .T. ) ;
#18525 = CARTESIAN_POINT ( 'NONE',  ( 4.958415959904818315, 45.28449214630087738, -3.538181012081164312 ) ) ;
#18526 = CARTESIAN_POINT ( 'NONE',  ( 0.8753041380234524160, -47.71532843791157319, -11.59248721954040739 ) ) ;
#18527 = CARTESIAN_POINT ( 'NONE',  ( 4.303969348037246512, -8.413118729224382975, 47.36875205922770249 ) ) ;
#18528 = FACE_OUTER_BOUND ( 'NONE', #7312, .T. ) ;
#18529 = EDGE_LOOP ( 'NONE', ( #1193, #18985, #45824, #14989 ) ) ;
#18530 = FACE_OUTER_BOUND ( 'NONE', #43991, .T. ) ;
#18531 = ORIENTED_EDGE ( 'NONE', *, *, #12697, .T. ) ;
#18532 = CARTESIAN_POINT ( 'NONE',  ( 0.5837799406558225046, 43.13924169579550494, -18.39155717955778968 ) ) ;
#18533 = VERTEX_POINT ( 'NONE', #36585 ) ;
#18534 = CARTESIAN_POINT ( 'NONE',  ( 3.783198216974387851, 12.79806054635192147, -41.09147814699330326 ) ) ;
#18535 = CARTESIAN_POINT ( 'NONE',  ( 0.6027444965799114707, 46.64666970468664431, -15.35013750261902743 ) ) ;
#18536 = VERTEX_POINT ( 'NONE', #55349 ) ;
#18537 = CARTESIAN_POINT ( 'NONE',  ( 0.8554163680231708922, 39.89400665120431455, 24.69157156653835372 ) ) ;
#18538 = DIRECTION ( 'NONE',  ( 1.000000000000000000, 1.836909530733573776E-16, -1.925929944387235853E-32 ) ) ;
#18539 = CARTESIAN_POINT ( 'NONE',  ( 0.5809828226811553087, 24.41822904836923058, 41.20389530892317254 ) ) ;
#18540 = CARTESIAN_POINT ( 'NONE',  ( 0.5837800005270554760, -1.567060691030147446, -46.86981522720579107 ) ) ;
#18541 = EDGE_CURVE ( 'NONE', #35847, #16005, #33794, .T. ) ;
#18542 = ORIENTED_EDGE ( 'NONE', *, *, #46403, .T. ) ;
#18543 = CARTESIAN_POINT ( 'NONE',  ( 0.1073791018717483448, 30.83464511437097499, 30.14884492832400298 ) ) ;
#18544 = CARTESIAN_POINT ( 'NONE',  ( 0.9790724872846771065, -41.81774720698464876, 2.758845503862258575 ) ) ;
#18545 = EDGE_CURVE ( 'NONE', #3481, #56877, #44502, .T. ) ;
#18546 = CARTESIAN_POINT ( 'NONE',  ( -6.010958268070873523, 7.197664668556679857, -17.41463273278770885 ) ) ;
#18548 = B_SPLINE_CURVE_WITH_KNOTS ( 'NONE', 3,
 ( #59606, #40541, #12037, #26407 ),
 .UNSPECIFIED., .F., .F.,
 ( 4, 4 ),
 ( 0.001844835322069226938, 0.004559932413162187670 ),
 .UNSPECIFIED. ) ;
#18547 = CARTESIAN_POINT ( 'NONE',  ( 0.5819845901640494645, -44.07435474487832039, -18.74765780149875027 ) ) ;
#18549 = EDGE_CURVE ( 'NONE', #44283, #56469, #44438, .T. ) ;
#18550 = CARTESIAN_POINT ( 'NONE',  ( 0.5809828226811617480, -29.58751527316205809, 37.66417181417541826 ) ) ;
#18551 = CARTESIAN_POINT ( 'NONE',  ( -6.016489644550737204, -16.32089497094068520, 9.417787539062191016 ) ) ;
#18552 = VECTOR ( 'NONE', #18290, 1000.000000000000000 ) ;
#18553 = CARTESIAN_POINT ( 'NONE',  ( 0.5819845901640494645, -46.37938751183692432, 11.95725023767341355 ) ) ;
#18554 = LINE ( 'NONE', #24167, #37918 ) ;
#18555 = CARTESIAN_POINT ( 'NONE',  ( 0.09136607875274982415, 1.224646799147353256E-15, -10.00000000000000000 ) ) ;
#18556 = CARTESIAN_POINT ( 'NONE',  ( 4.975610109902397937, 0.000000000000000000, 0.000000000000000000 ) ) ;
#18557 = CARTESIAN_POINT ( 'NONE',  ( 0.8760168074886960365, 42.09738177923954083, -23.27577685234554394 ) ) ;
#18558 = EDGE_CURVE ( 'NONE', #18600, #51070, #2731, .T. ) ;
#18559 = AXIS2_PLACEMENT_3D ( 'NONE', #55189, #36742, #59581 ) ;
#18560 = CARTESIAN_POINT ( 'NONE',  ( 0.8744876279028263033, 16.11801507201566253, 46.37412684372363714 ) ) ;
#18561 = B_SPLINE_CURVE_WITH_KNOTS ( 'NONE', 3,
 ( #30309, #6787, #49417, #1793, #54406, #59425, #16532, #53189, #8050, #50958, #26854, #60654, #17158, #50342, #22160, #27163, #46289, #45991, #17770 ),
 .UNSPECIFIED., .F., .F.,
 ( 4, 3, 3, 3, 3, 3, 4 ),
 ( 3.469552829456483146E-18, 0.0002612768053151726306, 0.0003919133833142900581, 0.0005225499612322590188, 0.0006531865391693349827, 0.0008112755173415182311, 0.0009693688056799727899 ),
 .UNSPECIFIED. ) ;
#18562 = CARTESIAN_POINT ( 'NONE',  ( 3.782542959838397056, 37.99691774666566602, 17.98532999835400759 ) ) ;
#18563 = CARTESIAN_POINT ( 'NONE',  ( 4.956653778116982600, -47.27023054223759857, 8.845409907520762616 ) ) ;
#18564 = CARTESIAN_POINT ( 'NONE',  ( 3.221118495291109607, -21.16578580483263750, 38.55866868715381202 ) ) ;
#18565 = B_SPLINE_CURVE_WITH_KNOTS ( 'NONE', 3,
 ( #23440, #47254, #41960, #18134, #51938, #61625 ),
 .UNSPECIFIED., .F., .F.,
 ( 4, 2, 4 ),
 ( 0.000000000000000000, 0.0002447195606305753424, 0.0004894391212611506848 ),
 .UNSPECIFIED. ) ;
#18566 = B_SPLINE_CURVE_WITH_KNOTS ( 'NONE', 3,
 ( #5292, #29425, #47935, #15044, #25043, #44187, #34150, #57290, #38241, #1217, #15661, #39473, #20352, #43248, #34763, #33533 ),
 .UNSPECIFIED., .F., .F.,
 ( 4, 3, 3, 3, 3, 4 ),
 ( 1.250973872328959318E-17, 0.0002724568934985569023, 0.0004086836638483783580, 0.0005449104342063597903, 0.0008173270854453586502, 0.001089761613562687925 ),
 .UNSPECIFIED. ) ;
#18567 = CARTESIAN_POINT ( 'NONE',  ( 5.959547316686252039, -14.51128755440531393, -14.51632612601523853 ) ) ;
#18568 = CARTESIAN_POINT ( 'NONE',  ( 0.5824936645240085253, 45.32464743504566229, -12.03804443957227477 ) ) ;
#18569 = CARTESIAN_POINT ( 'NONE',  ( 0.8744876279028306332, -39.87136468799875644, -28.64654129726831044 ) ) ;
#18571 = ORIENTED_EDGE ( 'NONE', *, *, #9760, .F. ) ;
#18570 = CARTESIAN_POINT ( 'NONE',  ( 0.9756354156337464500, 39.59221474545864083, 16.54067710771375488 ) ) ;
#18572 = CARTESIAN_POINT ( 'NONE',  ( 0.6029443199889047422, -39.35533208240347136, 29.37167817027392402 ) ) ;
#18573 = CARTESIAN_POINT ( 'NONE',  ( 4.322998006666179727, -45.75942687572307932, 14.45630056002860364 ) ) ;
#18574 = CARTESIAN_POINT ( 'NONE',  ( 4.975801465491695552, -32.01766832630288206, -35.64402118370946937 ) ) ;
#18575 = ORIENTED_EDGE ( 'NONE', *, *, #49230, .F. ) ;
#18576 = ORIENTED_EDGE ( 'NONE', *, *, #56371, .F. ) ;
#18577 = CARTESIAN_POINT ( 'NONE',  ( 0.5838002273316419410, -33.96372661229960244, 33.77111476497762510 ) ) ;
#18578 = CARTESIAN_POINT ( 'NONE',  ( 0.8560838555295223751, 17.70877843982779609, 43.43698884880053157 ) ) ;
#18579 = B_SPLINE_CURVE_WITH_KNOTS ( 'NONE', 3,
 ( #37020, #22897, #56082, #13194, #61385, #42026 ),
 .UNSPECIFIED., .F., .F.,
 ( 4, 2, 4 ),
 ( 3.529906531158615134E-18, 0.0002445244328975369687, 0.0004890488657950704679 ),
 .UNSPECIFIED. ) ;
#18580 =( BOUNDED_SURFACE ( )  B_SPLINE_SURFACE ( 3, 1, ( 
 ( #43136, #5181 ),
 ( #8982, #47511 ),
 ( #58116, #43767 ),
 ( #43446, #19947 ) ),
 .UNSPECIFIED., .F., .F., .F. ) 
 B_SPLINE_SURFACE_WITH_KNOTS ( ( 4, 4 ),
 ( 2, 2 ),
 ( 0.000000000000000000, 1.000000000000000000 ),
 ( 0.000000000000000000, 1.000000000000000000 ),
 .UNSPECIFIED. ) 
 GEOMETRIC_REPRESENTATION_ITEM ( )  RATIONAL_B_SPLINE_SURFACE ( (
 ( 1.000000000000000000, 1.000000000000000000),
 ( 0.9729067724841187204, 0.9999501103223794596),
 ( 0.9729067724841187204, 0.9999501103223794596),
 ( 1.000000000000000000, 1.000000000000000000) ) ) 
 REPRESENTATION_ITEM ( '' )  SURFACE ( )  );
#18581 = UNCERTAINTY_MEASURE_WITH_UNIT (LENGTH_MEASURE( 1.000000000000000082E-05 ), #15714, 'distance_accuracy_value', 'NONE');
#18582 = ORIENTED_EDGE ( 'NONE', *, *, #42881, .F. ) ;
#18583 = ORIENTED_EDGE ( 'NONE', *, *, #48873, .F. ) ;
#18584 = DIRECTION ( 'NONE',  ( 0.000000000000000000, 0.000000000000000000, 1.000000000000000000 ) ) ;
#18585 = ORIENTED_EDGE ( 'NONE', *, *, #48302, .T. ) ;
#18586 = DIRECTION ( 'NONE',  ( -1.000000000000000000, 0.000000000000000000, 0.000000000000000000 ) ) ;
#18588 = CARTESIAN_POINT ( 'NONE',  ( 0.9752570700956797456, -41.50550328400875344, 10.88256294660697243 ) ) ;
#18587 = B_SPLINE_CURVE_WITH_KNOTS ( 'NONE', 3,
 ( #11011, #24786, #16019, #57968, #15093, #35131 ),
 .UNSPECIFIED., .F., .F.,
 ( 4, 2, 4 ),
 ( 3.471140604459641645E-18, 0.0002291966416970808403, 0.0004583932833941582112 ),
 .UNSPECIFIED. ) ;
#18589 = VERTEX_POINT ( 'NONE', #22170 ) ;
#18590 = EDGE_CURVE ( 'NONE', #60753, #38461, #335, .T. ) ;
#18591 = ORIENTED_EDGE ( 'NONE', *, *, #51336, .T. ) ;
#18592 = CARTESIAN_POINT ( 'NONE',  ( 0.5819845079324665882, -12.83441846783097873, -46.14435090135489048 ) ) ;
#18593 = VERTEX_POINT ( 'NONE', #60352 ) ;
#18594 = CARTESIAN_POINT ( 'NONE',  ( 5.901463166500146684, -4.676581321913868550, -19.56137667650625289 ) ) ;
#18595 = FACE_BOUND ( 'NONE', #26023, .T. ) ;
#18596 = EDGE_CURVE ( 'NONE', #58608, #2051, #36287, .T. ) ;
#18597 = CARTESIAN_POINT ( 'NONE',  ( 4.956653778116982600, -45.71126949320260735, 14.93973939759871072 ) ) ;
#18598 = ORIENTED_EDGE ( 'NONE', *, *, #49471, .T. ) ;
#18599 = CARTESIAN_POINT ( 'NONE',  ( 0.9789233960466710016, -39.63276750765551526, 13.62279217034692991 ) ) ;
#18600 = VERTEX_POINT ( 'NONE', #41596 ) ;
#18601 = EDGE_CURVE ( 'NONE', #61780, #20011, #48190, .T. ) ;
#18602 = VERTEX_POINT ( 'NONE', #3045 ) ;
#18603 = CARTESIAN_POINT ( 'NONE',  ( -6.015611763856276717, 11.46610900684744472, -14.95313250337417799 ) ) ;
#18604 = AXIS2_PLACEMENT_3D ( 'NONE', #38111, #47182, #4532 ) ;
#18605 = VERTEX_POINT ( 'NONE', #59752 ) ;
#18606 = CARTESIAN_POINT ( 'NONE',  ( 0.7056759521544981872, -8.631168086166848497, 46.10045299761512894 ) ) ;
#18607 = DIRECTION ( 'NONE',  ( 0.000000000000000000, -0.5000000000000013323, -0.8660254037844380415 ) ) ;
#18608 = CARTESIAN_POINT ( 'NONE',  ( 0.9752570700956796346, -0.2306661201224228797, 42.90785210525869786 ) ) ;
#18609 = FACE_OUTER_BOUND ( 'NONE', #37917, .T. ) ;
#18610 = VECTOR ( 'NONE', #39599, 1000.000000000000000 ) ;
#18611 = ORIENTED_EDGE ( 'NONE', *, *, #56371, .T. ) ;
#18612 = CARTESIAN_POINT ( 'NONE',  ( 0.8560838555295158248, 16.00311602465144745, 44.09391240957503300 ) ) ;
#18613 = CARTESIAN_POINT ( 'NONE',  ( 0.8751705887134423323, 24.81530984069208401, -41.19904111682483716 ) ) ;
#18614 = CARTESIAN_POINT ( 'NONE',  ( 5.917102823773431552, 18.99629506471987384, 6.605338134103467596 ) ) ;
#18615 = ORIENTED_EDGE ( 'NONE', *, *, #19186, .F. ) ;
#18616 = CARTESIAN_POINT ( 'NONE',  ( 3.680974057930773924, -47.94008194857089222, -1.849713332883580197 ) ) ;
#18617 = CARTESIAN_POINT ( 'NONE',  ( 0.5848930533535030563, -7.979791871080650800, 46.21250917318592855 ) ) ;
#18618 = CARTESIAN_POINT ( 'NONE',  ( -6.078457390727109555, 13.83560117034693526, 13.39293288613821176 ) ) ;
#18619 = EDGE_CURVE ( 'NONE', #60972, #36056, #35981, .T. ) ;
#18621 = AXIS2_PLACEMENT_3D ( 'NONE', #13178, #51051, #60441 ) ;
#18620 = B_SPLINE_CURVE_WITH_KNOTS ( 'NONE', 3,
 ( #9854, #39931, #58989, #28956, #34908, #24569, #43390, #19571, #57745, #33984, #29255, #48370, #5432, #43701, #48675, #53360 ),
 .UNSPECIFIED., .F., .F.,
 ( 4, 3, 3, 3, 3, 4 ),
 ( 2.194378057379452319E-17, 0.0002618515315864421394, 0.0003927756766341980454, 0.0005236998216950549626, 0.0007855159896329901156, 0.001047349442285927437 ),
 .UNSPECIFIED. ) ;
#18622 = ORIENTED_EDGE ( 'NONE', *, *, #22993, .T. ) ;
#18623 = VERTEX_POINT ( 'NONE', #3342 ) ;
#18624 = CARTESIAN_POINT ( 'NONE',  ( -6.063463321072276813, 17.85520303107520235, 7.211946838306062091 ) ) ;
#18625 = CARTESIAN_POINT ( 'NONE',  ( 4.833616638992205949, 8.578242093415124003, 45.44786513329600552 ) ) ;
#18626 = EDGE_CURVE ( 'NONE', #30942, #33762, #7855, .T. ) ;
#18627 = CARTESIAN_POINT ( 'NONE',  ( 0.8560838555295223751, -30.97734773434455491, -35.22466126774295248 ) ) ;
#18628 = DIRECTION ( 'NONE',  ( 0.09722883295013595717, 0.2288279796715356751, -0.9685991481322898666 ) ) ;
#18629 = CARTESIAN_POINT ( 'NONE',  ( 4.694002226626921015, -41.22189368134375087, 19.46895612944177500 ) ) ;
#18630 = ADVANCED_FACE ( 'NONE', ( #17169 ), #17666, .F. ) ;
#18631 = CARTESIAN_POINT ( 'NONE',  ( 1.227938101723748288, 15.63977281655842511, 39.96870412324341260 ) ) ;
#18632 = CARTESIAN_POINT ( 'NONE',  ( 0.1073791018717578927, 40.02496097243057704, -16.05399293000775529 ) ) ;
#18633 = CARTESIAN_POINT ( 'NONE',  ( 0.8744876279028306332, -14.81965677137948489, -46.80521149998148900 ) ) ;
#18634 = DIRECTION ( 'NONE',  ( 1.000000000000000000, 1.836909530733573776E-16, 0.000000000000000000 ) ) ;
#18635 = CARTESIAN_POINT ( 'NONE',  ( 5.901463166500145796, 3.359582080289229111, -19.83005493150324128 ) ) ;
#18636 = CARTESIAN_POINT ( 'NONE',  ( -6.072942160501519915, -4.299083787220544295, -18.77024349547649251 ) ) ;
#18637 = LINE ( 'NONE', #57734, #44886 ) ;
#18638 = ORIENTED_EDGE ( 'NONE', *, *, #4871, .T. ) ;
#18639 = CARTESIAN_POINT ( 'NONE',  ( 0.6064515330803588178, -46.73949274313381608, 3.841113660336747060 ) ) ;
#18640 = CARTESIAN_POINT ( 'NONE',  ( -6.079354080745853928, 0.6183512803180944983, 19.24605406160678456 ) ) ;
#18641 = CARTESIAN_POINT ( 'NONE',  ( 0.1155031312995260795, -35.26066340436319280, -26.52597309838059658 ) ) ;
#18642 = CARTESIAN_POINT ( 'NONE',  ( 0.6029443449137434907, -39.32931611637160785, -29.40653722902179368 ) ) ;
#18643 = EDGE_CURVE ( 'NONE', #35726, #7624, #19793, .T. ) ;
#18644 = B_SPLINE_CURVE_WITH_KNOTS ( 'NONE', 3,
 ( #56259, #22455, #41895, #14305, #47501, #42817 ),
 .UNSPECIFIED., .F., .F.,
 ( 4, 2, 4 ),
 ( 2.224174099750402954E-17, 0.0002293319059085117972, 0.0004586638118170013141 ),
 .UNSPECIFIED. ) ;
#18645 = CARTESIAN_POINT ( 'NONE',  ( 1.479689385636123067, -23.83924572570610323, -37.05771456116924867 ) ) ;
#18646 = CARTESIAN_POINT ( 'NONE',  ( -6.016104459813371719, -17.41090761020830868, -7.206059014950265684 ) ) ;
#18647 = FACE_OUTER_BOUND ( 'NONE', #56049, .T. ) ;
#18648 = CARTESIAN_POINT ( 'NONE',  ( 4.975610109902397937, 0.000000000000000000, 0.000000000000000000 ) ) ;
#18649 = CIRCLE ( 'NONE', #26639, 48.91267123290010943 ) ;
#18650 = CARTESIAN_POINT ( 'NONE',  ( 5.960721111146673579, 0.006321279846536711350, 20.52557019979492026 ) ) ;
#18652 = EDGE_LOOP ( 'NONE', ( #48864, #5788 ) ) ;
#18651 = CARTESIAN_POINT ( 'NONE',  ( 0.6031357023905875581, -46.45693331047449703, -12.49325238079521760 ) ) ;
#18653 = VERTEX_POINT ( 'NONE', #38144 ) ;
#18654 = AXIS2_PLACEMENT_3D ( 'NONE', #37182, #60954, #45970 ) ;
#18655 = CARTESIAN_POINT ( 'NONE',  ( 0.9730545539215883499, -42.90536227157002003, 0.5054011016611185125 ) ) ;
#18656 = CARTESIAN_POINT ( 'NONE',  ( 2.281351352603287808, 43.80196780981719940, 19.56575819747240885 ) ) ;
#18657 = VECTOR ( 'NONE', #57718, 1000.000000000000114 ) ;
#18658 = CARTESIAN_POINT ( 'NONE',  ( -6.001507490154111224, -14.95933060264881753, 11.45906331631425878 ) ) ;
#18659 = ORIENTED_EDGE ( 'NONE', *, *, #59898, .T. ) ;
#18660 = CARTESIAN_POINT ( 'NONE',  ( 0.5837799406558225046, 22.61724361227189917, 41.08167281112525870 ) ) ;
#18661 = CARTESIAN_POINT ( 'NONE',  ( 0.8560838555295158248, 3.785103201470073397, 46.75516899590838449 ) ) ;
#18663 = B_SPLINE_CURVE_WITH_KNOTS ( 'NONE', 3,
 ( #53508, #58511, #34745, #15640 ),
 .UNSPECIFIED., .F., .F.,
 ( 4, 4 ),
 ( 0.000000000000000000, 0.004445488388166995986 ),
 .UNSPECIFIED. ) ;
#18662 = DIRECTION ( 'NONE',  ( 0.000000000000000000, 0.000000000000000000, 1.000000000000000000 ) ) ;
#18664 = ORIENTED_EDGE ( 'NONE', *, *, #4601, .F. ) ;
#18665 = VERTEX_POINT ( 'NONE', #9925 ) ;
#18666 = CARTESIAN_POINT ( 'NONE',  ( 0.9772918015221170318, 24.52412876038616574, -33.98387800552902860 ) ) ;
#18667 = AXIS2_PLACEMENT_3D ( 'NONE', #28876, #6899, #40171 ) ;
#18668 = CARTESIAN_POINT ( 'NONE',  ( 0.6252788684277226228, -20.50349297004706983, -44.62119571684401365 ) ) ;
#18669 = CARTESIAN_POINT ( 'NONE',  ( 0.5817216825391117174, 46.89379108365920956, -0.4553130896244175219 ) ) ;
#18670 = ADVANCED_FACE ( 'NONE', ( #38444 ), #58437, .F. ) ;
#18671 = CARTESIAN_POINT ( 'NONE',  ( 1.227938101723747621, 30.94118573761354440, -29.74462687941193551 ) ) ;
#18672 = EDGE_CURVE ( 'NONE', #58253, #47464, #35805, .T. ) ;
#18673 = FACE_OUTER_BOUND ( 'NONE', #32170, .T. ) ;
#18674 = DIRECTION ( 'NONE',  ( 0.1024043820194936449, 0.3927886084231570485, 0.9139094329506647352 ) ) ;
#18675 = ORIENTED_EDGE ( 'NONE', *, *, #46081, .T. ) ;
#18676 = EDGE_CURVE ( 'NONE', #28479, #57072, #22066, .T. ) ;
#18677 = DIRECTION ( 'NONE',  ( 0.000000000000000000, 0.7071067811865500152, -0.7071067811865449082 ) ) ;
#18678 = CARTESIAN_POINT ( 'NONE',  ( -6.010958268070873523, 13.31406649671981413, -13.33459572764743584 ) ) ;
#18679 = ORIENTED_EDGE ( 'NONE', *, *, #29340, .F. ) ;
#18680 = CARTESIAN_POINT ( 'NONE',  ( 0.1158516988532803521, 41.86075703818062976, -13.95059780164302765 ) ) ;
#18681 = EDGE_CURVE ( 'NONE', #36654, #45591, #33741, .T. ) ;
#18682 = LINE ( 'NONE', #58094, #55643 ) ;
#18683 = DIRECTION ( 'NONE',  ( -1.000000000000000000, -1.836909530733573776E-16, 2.465190328815655050E-32 ) ) ;
#18684 = CARTESIAN_POINT ( 'NONE',  ( 1.227938101723748288, 15.63977281655842511, 39.96870412324341260 ) ) ;
#18685 = ORIENTED_EDGE ( 'NONE', *, *, #18407, .T. ) ;
#18686 = VERTEX_POINT ( 'NONE', #48136 ) ;
#18687 = CARTESIAN_POINT ( 'NONE',  ( 0.7044674535452954967, 37.93506595837585138, -31.18867572604804650 ) ) ;
#18688 = LINE ( 'NONE', #27770, #12182 ) ;
#18689 = EDGE_CURVE ( 'NONE', #56737, #47174, #37006, .T. ) ;
#18690 = ORIENTED_EDGE ( 'NONE', *, *, #45884, .F. ) ;
#18691 = CARTESIAN_POINT ( 'NONE',  ( 4.960156602257177916, 35.23783291257167605, 30.22163187094397685 ) ) ;
#18692 = CONICAL_SURFACE ( 'NONE', #38694, 42.92674063221959813, 1.485477209440487556 ) ;
#18693 = ORIENTED_EDGE ( 'NONE', *, *, #39177, .F. ) ;
#18694 = CARTESIAN_POINT ( 'NONE',  ( 2.879087469061463178, 43.48727737615701017, 6.705101281305238636 ) ) ;
#18695 = LINE ( 'NONE', #61575, #31438 ) ;
#18696 = EDGE_CURVE ( 'NONE', #9817, #31225, #46920, .T. ) ;
#18697 = VECTOR ( 'NONE', #58880, 1000.000000000000114 ) ;
#18698 = VERTEX_POINT ( 'NONE', #37521 ) ;
#18699 = CONICAL_SURFACE ( 'NONE', #10695, 42.08604991992415023, 1.569615340895231137 ) ;
#18700 = CARTESIAN_POINT ( 'NONE',  ( 4.291220156522059348, -3.725477031303138453, 46.96285572870254299 ) ) ;
#18701 = DIRECTION ( 'NONE',  ( 0.000000000000000000, 0.000000000000000000, -1.000000000000000000 ) ) ;
#18702 = ORIENTED_EDGE ( 'NONE', *, *, #34006, .F. ) ;
#18703 = CARTESIAN_POINT ( 'NONE',  ( 0.6028618097248862329, -29.42431480658704501, -38.05975027458327276 ) ) ;
#18704 = CARTESIAN_POINT ( 'NONE',  ( 0.1368894036331274322, -43.67490804582807584, 6.274052367632553917 ) ) ;
#18705 = CARTESIAN_POINT ( 'NONE',  ( 4.963659409799333844, -37.47512675766712675, 24.46566636552813634 ) ) ;
#18706 = CARTESIAN_POINT ( 'NONE',  ( 0.6031356755773454870, 47.69587413076373394, -6.279306815850331347 ) ) ;
#18707 =( BOUNDED_SURFACE ( )  B_SPLINE_SURFACE ( 3, 1, ( 
 ( #53703, #5782 ),
 ( #21454, #49036 ),
 ( #21147, #35879 ),
 ( #15533, #24934 ) ),
 .UNSPECIFIED., .F., .F., .F. ) 
 B_SPLINE_SURFACE_WITH_KNOTS ( ( 4, 4 ),
 ( 2, 2 ),
 ( 0.000000000000000000, 1.000000000000000000 ),
 ( 0.000000000000000000, 1.000000000000000000 ),
 .UNSPECIFIED. ) 
 GEOMETRIC_REPRESENTATION_ITEM ( )  RATIONAL_B_SPLINE_SURFACE ( (
 ( 1.000000000000000000, 1.000000000000000000),
 ( 0.9732289882329797637, 0.9999525324661233672),
 ( 0.9732289882329797637, 0.9999525324661233672),
 ( 1.000000000000000000, 1.000000000000000000) ) ) 
 REPRESENTATION_ITEM ( '' )  SURFACE ( )  );
#18708 = CARTESIAN_POINT ( 'NONE',  ( 0.1103878639767399278, 16.45816205842763935, -39.86034920885569477 ) ) ;
#18709 = ORIENTED_EDGE ( 'NONE', *, *, #12348, .F. ) ;
#18710 = CARTESIAN_POINT ( 'NONE',  ( 0.9780303403264766215, 41.57669851679587936, 5.264765316568995601 ) ) ;
#18711 = CARTESIAN_POINT ( 'NONE',  ( 0.3676999524040366896, -17.09834788623584600, 40.66444494744877858 ) ) ;
#18712 = VERTEX_POINT ( 'NONE', #19637 ) ;
#18713 = CARTESIAN_POINT ( 'NONE',  ( 1.227938101723756947, 37.58536632582779191, 20.72293514920763258 ) ) ;
#18714 = CARTESIAN_POINT ( 'NONE',  ( 0.5832367798473407916, 0.2724222379467150512, -47.89515946578894301 ) ) ;
#18715 = B_SPLINE_CURVE_WITH_KNOTS ( 'NONE', 3,
 ( #37184, #32164, #46895, #46577 ),
 .UNSPECIFIED., .F., .F.,
 ( 4, 4 ),
 ( 2.189128766608093472E-17, 0.004559932413162185935 ),
 .UNSPECIFIED. ) ;
#18716 = CARTESIAN_POINT ( 'NONE',  ( 5.981074661064941900, 5.303881226583402331, 19.82752479807529156 ) ) ;
#18717 = CARTESIAN_POINT ( 'NONE',  ( -6.016761891674564211, -14.95139917749696501, -11.46828378093574941 ) ) ;
#18718 = EDGE_CURVE ( 'NONE', #59625, #47413, #50390, .T. ) ;
#18719 = CARTESIAN_POINT ( 'NONE',  ( 0.6064782688330866423, -7.098623077535437531, -46.35670390377050154 ) ) ;
#18720 = CARTESIAN_POINT ( 'NONE',  ( 0.7954190325252781246, -41.21355377862716551, 24.79809930825913256 ) ) ;
#18721 = CONICAL_SURFACE ( 'NONE', #12739, 42.92674063221959813, 1.485477209440487556 ) ;
#18722 = CARTESIAN_POINT ( 'NONE',  ( 51.82989359177101107, 15.32891900549394038, 2.298613371999423727 ) ) ;
#18723 = CARTESIAN_POINT ( 'NONE',  ( 4.409518593371577921, 0.4834892475542106882, 0.7180814939294286603 ) ) ;
#18724 = CARTESIAN_POINT ( 'NONE',  ( 4.962356264823599261, -28.94323483023637777, 30.55363735178087126 ) ) ;
#18725 = ADVANCED_FACE ( 'NONE', ( #27788 ), #4882, .T. ) ;
#18726 = CARTESIAN_POINT ( 'NONE',  ( 0.5807400328401637335, 41.20655774453003062, -24.41979442053126448 ) ) ;
#18727 = CARTESIAN_POINT ( 'NONE',  ( 4.967162193818130511, -32.10009971360091896, 28.74031574030002645 ) ) ;
#18728 = DIRECTION ( 'NONE',  ( -1.626303258728256898E-16, 1.000000000000000000, 0.000000000000000000 ) ) ;
#18729 = ORIENTED_EDGE ( 'NONE', *, *, #330, .F. ) ;
#18730 = CARTESIAN_POINT ( 'NONE',  ( 4.962356264823608143, 0.000000000000000000, 0.000000000000000000 ) ) ;
#18731 = CARTESIAN_POINT ( 'NONE',  ( 4.553261556744875094, 1.633632119647590697, -43.89613664004262716 ) ) ;
#18732 = FACE_OUTER_BOUND ( 'NONE', #33645, .T. ) ;
#18733 = CARTESIAN_POINT ( 'NONE',  ( 0.6067099128993237445, -47.89177823194876282, 0.7089426894588903849 ) ) ;
#18734 = CARTESIAN_POINT ( 'NONE',  ( 2.706805983486679335, 32.41343978096548994, -29.76818830371574620 ) ) ;
#18735 = B_SPLINE_CURVE_WITH_KNOTS ( 'NONE', 3,
 ( #35359, #20626, #59125, #12168, #11538, #11229, #44763, #11865, #59434, #16236, #54415, #49740, #6797, #12470, #31255, #25939, #35668, #54107, #2730 ),
 .UNSPECIFIED., .F., .F.,
 ( 4, 3, 3, 3, 3, 3, 4 ),
 ( 1.161956753697875813E-16, 0.0002618519381806249952, 0.0003927759815485967884, 0.0005237000248299413701, 0.0006546240681324970662, 0.0007855481115631314081, 0.0009699050456655111587 ),
 .UNSPECIFIED. ) ;
#18736 = ORIENTED_EDGE ( 'NONE', *, *, #55214, .F. ) ;
#18737 = B_SPLINE_CURVE_WITH_KNOTS ( 'NONE', 3,
 ( #40783, #31660, #26643, #37931, #61371, #32910, #41698, #13182, #33215, #32593, #18487, #52286, #3434, #4045, #37611, #56678, #13803, #51987, #9078 ),
 .UNSPECIFIED., .F., .F.,
 ( 4, 3, 3, 3, 3, 3, 4 ),
 ( 1.250973872328959318E-17, 0.0002732106629380557099, 0.0004098138914053726673, 0.0005464171197651425697, 0.0006830203481512468755, 0.0008196235766963536583, 0.001011968216111134222 ),
 .UNSPECIFIED. ) ;
#18738 = VECTOR ( 'NONE', #20076, 1000.000000000000000 ) ;
#18739 = CARTESIAN_POINT ( 'NONE',  ( 4.956653778116999476, 43.37017594958085454, -20.77844580450516077 ) ) ;
#18740 =( GEOMETRIC_REPRESENTATION_CONTEXT ( 3 ) GLOBAL_UNCERTAINTY_ASSIGNED_CONTEXT ( ( #33001 ) ) GLOBAL_UNIT_ASSIGNED_CONTEXT ( ( #8438, #61362, #56362 ) ) REPRESENTATION_CONTEXT ( 'NONE', 'WORKASPACE' ) );
#18741 = CONICAL_SURFACE ( 'NONE', #5723, 42.08604991992415023, 1.569615340895231137 ) ;
#18742 = CARTESIAN_POINT ( 'NONE',  ( -17.97369999999976642, -7.719455939378112141, -2.099999999999997424 ) ) ;
#18743 = CIRCLE ( 'NONE', #55739, 42.92674063221959813 ) ;
#18744 = CARTESIAN_POINT ( 'NONE',  ( 5.901764892641307547, -4.659217859063449652, -48.74713485305021266 ) ) ;
#18745 = ORIENTED_EDGE ( 'NONE', *, *, #31403, .T. ) ;
#18746 = EDGE_CURVE ( 'NONE', #51963, #27614, #58580, .T. ) ;
#18747 = CARTESIAN_POINT ( 'NONE',  ( 5.880360259849752858, 15.37531919565172878, 45.44137230084887591 ) ) ;
#18748 = EDGE_CURVE ( 'NONE', #32528, #30513, #18808, .T. ) ;
#18749 = CARTESIAN_POINT ( 'NONE',  ( 0.5834584762367747146, 43.10339065662142843, 18.47521861618612604 ) ) ;
#18750 = ORIENTED_EDGE ( 'NONE', *, *, #33911, .T. ) ;
#18751 = DIRECTION ( 'NONE',  ( 0.000000000000000000, 0.000000000000000000, -1.000000000000000000 ) ) ;
#18752 = ORIENTED_EDGE ( 'NONE', *, *, #27779, .F. ) ;
#18753 = EDGE_CURVE ( 'NONE', #18771, #44393, #32809, .T. ) ;
#18754 = AXIS2_PLACEMENT_3D ( 'NONE', #35704, #30981, #45108 ) ;
#18755 = EDGE_CURVE ( 'NONE', #48168, #55855, #30266, .T. ) ;
#18756 = CARTESIAN_POINT ( 'NONE',  ( 0.3676999524040366896, 42.11837424242170158, 13.11461530118771179 ) ) ;
#18757 = DIRECTION ( 'NONE',  ( 0.09722883295013597105, -0.2904161885395503129, 0.9519479983052198113 ) ) ;
#18758 = EDGE_LOOP ( 'NONE', ( #25109, #27480, #27310, #11729 ) ) ;
#18759 = CARTESIAN_POINT ( 'NONE',  ( 2.526464513654347321, -22.53107770806397525, -36.59988118252427114 ) ) ;
#18760 = EDGE_CURVE ( 'NONE', #14535, #41116, #41496, .T. ) ;
#18761 = CARTESIAN_POINT ( 'NONE',  ( 0.5836750258453344831, -29.30109045202416596, 37.88760409476686419 ) ) ;
#18762 = CARTESIAN_POINT ( 'NONE',  ( 4.553261556744873317, -39.67390170502044100, -18.85526688551536623 ) ) ;
#18763 = CARTESIAN_POINT ( 'NONE',  ( 6.999999999999995559, 54.69470952478017267, -58.44237546506749936 ) ) ;
#18764 = CONICAL_SURFACE ( 'NONE', #39803, 42.92674063221959813, 1.485477209440487556 ) ;
#18765 = ORIENTED_EDGE ( 'NONE', *, *, #12724, .F. ) ;
#18766 = CARTESIAN_POINT ( 'NONE',  ( 0.8751705887134423323, 33.37254303619506857, 34.63284514348596588 ) ) ;
#18768 = ORIENTED_EDGE ( 'NONE', *, *, #1334, .F. ) ;
#18767 =( BOUNDED_SURFACE ( )  B_SPLINE_SURFACE ( 3, 1, ( 
 ( #25381, #26006 ),
 ( #54478, #34183 ),
 ( #54171, #39202 ),
 ( #20691, #30076 ) ),
 .UNSPECIFIED., .F., .F., .F. ) 
 B_SPLINE_SURFACE_WITH_KNOTS ( ( 4, 4 ),
 ( 2, 2 ),
 ( 0.000000000000000000, 1.000000000000000000 ),
 ( 0.000000000000000000, 1.000000000000000000 ),
 .UNSPECIFIED. ) 
 GEOMETRIC_REPRESENTATION_ITEM ( )  RATIONAL_B_SPLINE_SURFACE ( (
 ( 1.000000000000000000, 1.000000000000000000),
 ( 0.9953485035131437453, 0.8621029689291515030),
 ( 0.9953485035131437453, 0.8621029689291515030),
 ( 1.000000000000000000, 1.000000000000000000) ) ) 
 REPRESENTATION_ITEM ( '' )  SURFACE ( )  );
#18769 = CARTESIAN_POINT ( 'NONE',  ( 4.956445790444004018, -43.56224489968086999, -17.88487823385623443 ) ) ;
#18770 = EDGE_CURVE ( 'NONE', #351, #42525, #53121, .T. ) ;
#18771 = VERTEX_POINT ( 'NONE', #6405 ) ;
#18772 = VERTEX_POINT ( 'NONE', #25856 ) ;
#18773 = CARTESIAN_POINT ( 'NONE',  ( 4.691466044806102964, 43.66525414675629690, 9.025781474741620514 ) ) ;
#18774 = CARTESIAN_POINT ( 'NONE',  ( 0.8551540677456715978, 44.61036085020975861, -17.49081417858738519 ) ) ;
#18775 = CARTESIAN_POINT ( 'NONE',  ( 4.694002226626921015, -30.39302829899101965, -33.97864921186342713 ) ) ;
#18776 = CARTESIAN_POINT ( 'NONE',  ( 0.2940133293163011974, -43.64383948024472915, -6.438619805569689269 ) ) ;
#18777 = VERTEX_POINT ( 'NONE', #29321 ) ;
#18778 = CARTESIAN_POINT ( 'NONE',  ( -5.995132425357893702, 11.46484027925367499, 14.95525565067279139 ) ) ;
#18779 = CARTESIAN_POINT ( 'NONE',  ( 5.894904586330512508, -19.39861238634060925, 5.312555839344692998 ) ) ;
#18780 = CARTESIAN_POINT ( 'NONE',  ( 0.1129192098497447394, -38.20615368646970467, 22.07354996983974260 ) ) ;
#18781 = ORIENTED_EDGE ( 'NONE', *, *, #9901, .T. ) ;
#18782 = B_SPLINE_CURVE_WITH_KNOTS ( 'NONE', 3,
 ( #4967, #45846, #60210, #27638, #3812, #43227, #60512, #263, #12946, #19411, #2889, #22023, #31729, #41147, #41767, #32045 ),
 .UNSPECIFIED., .F., .F.,
 ( 4, 3, 3, 3, 3, 4 ),
 ( 1.127622383284612036E-17, 0.0002732102107931897827, 0.0004098135523333829976, 0.0005464168938825005517, 0.0008195847345945430100, 0.001092771384553107216 ),
 .UNSPECIFIED. ) ;
#18783 = ORIENTED_EDGE ( 'NONE', *, *, #61234, .T. ) ;
#18784 =( BOUNDED_SURFACE ( )  B_SPLINE_SURFACE ( 3, 1, ( 
 ( #6512, #35388 ),
 ( #25655, #44800 ),
 ( #1839, #20966 ),
 ( #40110, #59155 ) ),
 .UNSPECIFIED., .F., .F., .F. ) 
 B_SPLINE_SURFACE_WITH_KNOTS ( ( 4, 4 ),
 ( 2, 2 ),
 ( 0.000000000000000000, 1.000000000000000000 ),
 ( 0.000000000000000000, 1.000000000000000000 ),
 .UNSPECIFIED. ) 
 GEOMETRIC_REPRESENTATION_ITEM ( )  RATIONAL_B_SPLINE_SURFACE ( (
 ( 1.000000000000000000, 1.000000000000000000),
 ( 0.9729067724841187204, 0.9999501103223794596),
 ( 0.9729067724841187204, 0.9999501103223794596),
 ( 1.000000000000000000, 1.000000000000000000) ) ) 
 REPRESENTATION_ITEM ( '' )  SURFACE ( )  );
#18785 =( LENGTH_UNIT ( ) NAMED_UNIT ( * ) SI_UNIT ( .MILLI., .METRE. ) );
#18786 = CARTESIAN_POINT ( 'NONE',  ( 5.974727161628367256, -19.82959049719571709, -5.297264154380866508 ) ) ;
#18787 = CARTESIAN_POINT ( 'NONE',  ( 4.956445790443991584, 29.98832127573247774, 36.30755619981999871 ) ) ;
#18788 = CARTESIAN_POINT ( 'NONE',  ( 4.975610109902397937, 48.43414999183897862, -6.825138951392602849 ) ) ;
#18789 = CARTESIAN_POINT ( 'NONE',  ( -6.016104459813374383, -16.31603998697563540, -9.426230926598815785 ) ) ;
#18790 = EDGE_LOOP ( 'NONE', ( #54470, #54462, #58098, #59234 ) ) ;
#18791 = ORIENTED_EDGE ( 'NONE', *, *, #41212, .F. ) ;
#18792 = VECTOR ( 'NONE', #38514, 1000.000000000000114 ) ;
#18793 = VECTOR ( 'NONE', #50047, 1000.000000000000000 ) ;
#18794 = CARTESIAN_POINT ( 'NONE',  ( 4.553261556744875094, -41.75933753256810377, 13.62707946203756393 ) ) ;
#18795 = CARTESIAN_POINT ( 'NONE',  ( 48.20074816270739859, 15.44360797527890483, 1.328834602619866967 ) ) ;
#18796 = CARTESIAN_POINT ( 'NONE',  ( 2.879087469061463178, -39.15901799926898263, -20.06671338601083932 ) ) ;
#18797 = CARTESIAN_POINT ( 'NONE',  ( 0.8551540677456715978, 5.348818140991581593, -47.61725548905984340 ) ) ;
#18798 = SURFACE_STYLE_FILL_AREA ( #38226 ) ;
#18799 = CARTESIAN_POINT ( 'NONE',  ( 0.3622758884714730732, -42.62881903538215056, 6.444611261693867554 ) ) ;
#18800 = APPLICATION_CONTEXT ( 'automotive_design' ) ;
#18801 = ADVANCED_FACE ( 'NONE', ( #1113 ), #43772, .F. ) ;
#18802 = VERTEX_POINT ( 'NONE', #5798 ) ;
#18803 = CARTESIAN_POINT ( 'NONE',  ( 0.8744876279028263033, -31.30103973185235233, 37.82320666052117275 ) ) ;
#18804 = CARTESIAN_POINT ( 'NONE',  ( 5.838029081930955932, -16.99499549701727119, 44.07079743105724390 ) ) ;
#18805 = CARTESIAN_POINT ( 'NONE',  ( 0.8760168074886960365, 24.81951362746078260, -41.20610493656884898 ) ) ;
#18806 = CARTESIAN_POINT ( 'NONE',  ( 4.549368137175248350, 40.58005590356690817, -13.99871866169321599 ) ) ;
#18807 = CARTESIAN_POINT ( 'NONE',  ( 0.9784957157296355623, -34.41894368623801626, 23.90960837228307412 ) ) ;
#18808 = CIRCLE ( 'NONE', #22773, 5.633200000000004870 ) ;
#18809 = CARTESIAN_POINT ( 'NONE',  ( 0.5830081025819940921, 22.29738496909589074, -41.25601359707673055 ) ) ;
#18810 = B_SPLINE_CURVE_WITH_KNOTS ( 'NONE', 3,
 ( #38042, #57087, #5077, #53013, #33626, #33325 ),
 .UNSPECIFIED., .F., .F.,
 ( 4, 2, 4 ),
 ( 3.511543213478341086E-18, 0.0002450742804987349893, 0.0004901485609974664008 ),
 .UNSPECIFIED. ) ;
#18811 = B_SPLINE_CURVE_WITH_KNOTS ( 'NONE', 3,
 ( #44265, #14512, #24197, #38947 ),
 .UNSPECIFIED., .F., .F.,
 ( 4, 4 ),
 ( 0.000000000000000000, 0.004442905043737215703 ),
 .UNSPECIFIED. ) ;
#18812 = B_SPLINE_CURVE_WITH_KNOTS ( 'NONE', 3,
 ( #58065, #5131, #57135, #33069 ),
 .UNSPECIFIED., .F., .F.,
 ( 4, 4 ),
 ( 2.292215966409847280E-17, 0.004564976165746185977 ),
 .UNSPECIFIED. ) ;
#18813 = AXIS2_PLACEMENT_3D ( 'NONE', #48395, #5455, #10493 ) ;
#18814 = CARTESIAN_POINT ( 'NONE',  ( -6.001507490154111224, 14.95933060264889392, -11.45906331631416286 ) ) ;
#18815 = ORIENTED_EDGE ( 'NONE', *, *, #48095, .F. ) ;
#18816 = CARTESIAN_POINT ( 'NONE',  ( 1.088908134280555107, -39.93902428011476502, -15.69861202536792710 ) ) ;
#18817 = CARTESIAN_POINT ( 'NONE',  ( 2.879087469061462734, 23.73415476983658934, -37.05120206072701450 ) ) ;
#18818 = CARTESIAN_POINT ( 'NONE',  ( 0.8751705887134423323, -38.69254731947852832, 28.56654290188588163 ) ) ;
#18819 = CARTESIAN_POINT ( 'NONE',  ( 4.303969348037246512, 42.70173985163847874, -22.16169334783792877 ) ) ;
#18820 = ORIENTED_EDGE ( 'NONE', *, *, #47769, .T. ) ;
#18821 = CARTESIAN_POINT ( 'NONE',  ( 4.958415959904820092, -31.93886907500572647, -32.29725369179680428 ) ) ;
#18822 = LINE ( 'NONE', #43253, #30972 ) ;
#18823 = EDGE_CURVE ( 'NONE', #58899, #23453, #29790, .T. ) ;
#18824 = ORIENTED_EDGE ( 'NONE', *, *, #31047, .T. ) ;
#18825 = FACE_OUTER_BOUND ( 'NONE', #56732, .T. ) ;
#18826 = CARTESIAN_POINT ( 'NONE',  ( 0.5837800005270561421, -45.95629507620387955, -9.340995745136783768 ) ) ;
#18827 = EDGE_CURVE ( 'NONE', #5237, #44283, #11579, .T. ) ;
#18828 = CARTESIAN_POINT ( 'NONE',  ( 0.5980271706414734822, -45.78139539622846144, -17.77956912908339859 ) ) ;
#18829 = ORIENTED_EDGE ( 'NONE', *, *, #35231, .F. ) ;
#18830 = CONICAL_SURFACE ( 'NONE', #61803, 48.09070567114147110, 0.04450589592585947607 ) ;
#18831 = EDGE_CURVE ( 'NONE', #61591, #13981, #51780, .T. ) ;
#18832 = CARTESIAN_POINT ( 'NONE',  ( 0.6041374136657475802, -38.05989626241411372, -29.42442150067184059 ) ) ;
#18833 = VECTOR ( 'NONE', #55128, 1000.000000000000114 ) ;
#18834 = B_SPLINE_CURVE_WITH_KNOTS ( 'NONE', 3,
 ( #59728, #6459, #25603, #16842, #40056, #55021 ),
 .UNSPECIFIED., .F., .F.,
 ( 4, 2, 4 ),
 ( 9.913782460405889843E-18, 0.0002448709889506573193, 0.0004897419779013046639 ),
 .UNSPECIFIED. ) ;
#18835 = ORIENTED_EDGE ( 'NONE', *, *, #59487, .T. ) ;
#18836 = CARTESIAN_POINT ( 'NONE',  ( 0.5998501479064699549, 33.64490850298844293, -34.38546660123262200 ) ) ;
#18837 = EDGE_CURVE ( 'NONE', #39132, #43794, #45212, .T. ) ;
#18838 = ORIENTED_EDGE ( 'NONE', *, *, #14244, .T. ) ;
#18839 = CARTESIAN_POINT ( 'NONE',  ( 4.553261556744873317, -9.994631851593151595, -42.77437199977056537 ) ) ;
#18840 = CARTESIAN_POINT ( 'NONE',  ( -6.015611763856276717, 17.41126425312538117, 7.205255340944677123 ) ) ;
#18841 = ORIENTED_EDGE ( 'NONE', *, *, #19120, .T. ) ;
#18842 = CARTESIAN_POINT ( 'NONE',  ( 0.5786265663353153954, -47.89572889566446889, 0.7221568112304753706 ) ) ;
#18843 = ORIENTED_EDGE ( 'NONE', *, *, #39656, .T. ) ;
#18844 = CARTESIAN_POINT ( 'NONE',  ( 1.227938101723756947, -11.92353943227920610, -41.23019537246722876 ) ) ;
#18845 = CARTESIAN_POINT ( 'NONE',  ( 1.227938101723748288, 0.8460948827231143943, -42.91134962331486236 ) ) ;
#18846 = CARTESIAN_POINT ( 'NONE',  ( 5.960721111146673579, 16.28787783074210438, 12.49016043756476790 ) ) ;
#18847 = VERTEX_POINT ( 'NONE', #14944 ) ;
#18848 = CARTESIAN_POINT ( 'NONE',  ( 0.8554163680231720024, -46.74230100997663584, 4.045092014349757292 ) ) ;
#18849 = ADVANCED_FACE ( 'NONE', ( #35276, #15856 ), #5494, .F. ) ;
#18850 = CIRCLE ( 'NONE', #58777, 47.09074272231896430 ) ;
#18851 = CARTESIAN_POINT ( 'NONE',  ( 0.5807400328401637335, 34.25275203086282261, -33.48217046439074807 ) ) ;
#18852 = CARTESIAN_POINT ( 'NONE',  ( 14.84250595937556660, 5.000000000000015099, 10.00000000000000711 ) ) ;
#18853 = CARTESIAN_POINT ( 'NONE',  ( 0.1157506346131639274, -22.95291453873705478, -37.68427223630924061 ) ) ;
#18854 = ORIENTED_EDGE ( 'NONE', *, *, #46654, .T. ) ;
#18855 = CARTESIAN_POINT ( 'NONE',  ( 0.5786265663353153954, 13.09387673186335377, 46.07681357296491598 ) ) ;
#18856 = ADVANCED_FACE ( 'NONE', ( #19952 ), #35245, .F. ) ;
#18857 = CARTESIAN_POINT ( 'NONE',  ( 0.1156495703730067715, -31.79125611521524419, -30.59834943012220876 ) ) ;
#18858 = EDGE_LOOP ( 'NONE', ( #56236, #46298, #57189, #2389 ) ) ;
#18859 = CARTESIAN_POINT ( 'NONE',  ( 0.5824936645240106348, 43.31572343942117698, -17.97181910547413608 ) ) ;
#18860 = EDGE_LOOP ( 'NONE', ( #25081, #55789, #28891, #14271 ) ) ;
#18861 = CARTESIAN_POINT ( 'NONE',  ( 4.967162193818130511, 13.42934394584221280, -40.93989340068594629 ) ) ;
#18862 = CARTESIAN_POINT ( 'NONE',  ( 0.5837800005270562531, 10.87140793764657332, -45.61850225615763321 ) ) ;
#18863 = ORIENTED_EDGE ( 'NONE', *, *, #31089, .T. ) ;
#18864 = CARTESIAN_POINT ( 'NONE',  ( 0.5804410086790514622, 40.07081992599715647, 24.36902218624511818 ) ) ;
#18865 = CARTESIAN_POINT ( 'NONE',  ( 4.962356264823601926, -38.57439820587641321, 16.83007429920694875 ) ) ;
#18866 = DIRECTION ( 'NONE',  ( -1.000000000000000000, -0.000000000000000000, -0.000000000000000000 ) ) ;
#18867 = CARTESIAN_POINT ( 'NONE',  ( 4.975801465491695552, 0.000000000000000000, 0.000000000000000000 ) ) ;
#18868 = VECTOR ( 'NONE', #29174, 1000.000000000000114 ) ;
#18869 = ORIENTED_EDGE ( 'NONE', *, *, #24339, .T. ) ;
#18870 = CARTESIAN_POINT ( 'NONE',  ( 4.834790513006553603, -21.44535528597671004, -42.10327870347644108 ) ) ;
#18871 = CARTESIAN_POINT ( 'NONE',  ( 1.231276596079881935, -41.76121777166937221, -3.643825084341031584 ) ) ;
#18872 = CARTESIAN_POINT ( 'NONE',  ( 0.5980894510889448457, 48.10766805928368228, 0.7015180096006546906 ) ) ;
#18873 = CARTESIAN_POINT ( 'NONE',  ( 0.5806925824938511393, 42.95845041307772050, -18.80940989108128747 ) ) ;
#18874 = CARTESIAN_POINT ( 'NONE',  ( 0.6000166863083106206, -39.66797998683833271, -28.95297645272843923 ) ) ;
#18875 = ADVANCED_FACE ( 'NONE', ( #11460 ), #54051, .F. ) ;
#18876 = CARTESIAN_POINT ( 'NONE',  ( 0.6001305935487422083, -28.87057754790912156, -38.48510059944036499 ) ) ;
#18877 = AXIS2_PLACEMENT_3D ( 'NONE', #2073, #58164, #40044 ) ;
#18878 = DIRECTION ( 'NONE',  ( -0.1736481776669316357, 0.9848077530122079093, 4.662936703425656681E-15 ) ) ;
#18879 = VECTOR ( 'NONE', #30536, 1000.000000000000000 ) ;
#18880 = CARTESIAN_POINT ( 'NONE',  ( 0.5998501479064708430, -41.39809967730470674, -24.50586714782589937 ) ) ;
#18881 = DIRECTION ( 'NONE',  ( 0.1011922191286468153, -0.7235494112461594574, -0.6828150439710272135 ) ) ;
#18882 = EDGE_CURVE ( 'NONE', #17395, #18471, #19021, .T. ) ;
#18883 = CARTESIAN_POINT ( 'NONE',  ( 0.9757402383260941336, 30.40085236181992201, -30.28078671294493773 ) ) ;
#18884 = CARTESIAN_POINT ( 'NONE',  ( 0.5797568599927156452, 33.05098809540313454, -33.26946790359784245 ) ) ;
#18885 = CARTESIAN_POINT ( 'NONE',  ( -6.016761891674564211, -11.47373234755493243, -14.94721834528426463 ) ) ;
#18886 = CARTESIAN_POINT ( 'NONE',  ( 4.975610109902397937, 14.46773809681547718, 46.72401910687614190 ) ) ;
#18887 = DIRECTION ( 'NONE',  ( -1.000000000000000000, -0.000000000000000000, -0.000000000000000000 ) ) ;
#18888 = B_SPLINE_CURVE_WITH_KNOTS ( 'NONE', 3,
 ( #47493, #791, #52791, #23677, #38731, #48714 ),
 .UNSPECIFIED., .F., .F.,
 ( 4, 2, 4 ),
 ( 9.446879437911127976E-18, 0.0002448709889506566688, 0.0004897419779013039050 ),
 .UNSPECIFIED. ) ;
#18889 =( BOUNDED_SURFACE ( )  B_SPLINE_SURFACE ( 3, 1, ( 
 ( #53173, #43821 ),
 ( #58471, #34399 ),
 ( #24996, #9649 ),
 ( #4935, #15600 ) ),
 .UNSPECIFIED., .F., .F., .F. ) 
 B_SPLINE_SURFACE_WITH_KNOTS ( ( 4, 4 ),
 ( 2, 2 ),
 ( 0.000000000000000000, 1.000000000000000000 ),
 ( 0.000000000000000000, 1.000000000000000000 ),
 .UNSPECIFIED. ) 
 GEOMETRIC_REPRESENTATION_ITEM ( )  RATIONAL_B_SPLINE_SURFACE ( (
 ( 1.000000000000000000, 1.000000000000000000),
 ( 0.7282232189291694135, 0.9929344683865672927),
 ( 0.7282232189291694135, 0.9929344683865672927),
 ( 1.000000000000000000, 1.000000000000000000) ) ) 
 REPRESENTATION_ITEM ( '' )  SURFACE ( )  );
#18890 = CARTESIAN_POINT ( 'NONE',  ( 0.9757892942422827787, -37.18547544211197220, -21.40977514834421314 ) ) ;
#18891 = CARTESIAN_POINT ( 'NONE',  ( 0.5830081025819929819, 45.15677286343053254, -12.65297984439984980 ) ) ;
#18892 = DIRECTION ( 'NONE',  ( -1.000000000000000000, -0.000000000000000000, -0.000000000000000000 ) ) ;
#18893 = ORIENTED_EDGE ( 'NONE', *, *, #39281, .F. ) ;
#18894 = AXIS2_PLACEMENT_3D ( 'NONE', #38603, #28868, #47679 ) ;
#18895 = CARTESIAN_POINT ( 'NONE',  ( 0.5782707292762442330, 43.45719891954342273, -17.64109451748540280 ) ) ;
#18896 = CARTESIAN_POINT ( 'NONE',  ( 4.967162193818130511, 38.83676580803767564, 18.65818244221271627 ) ) ;
#18897 = CARTESIAN_POINT ( 'NONE',  ( 0.5807400328401574052, -46.40483864045135931, -11.87003418057292237 ) ) ;
#18898 = ORIENTED_EDGE ( 'NONE', *, *, #46659, .T. ) ;
#18899 = CARTESIAN_POINT ( 'NONE',  ( 0.5819845079324652559, -33.54497088780105685, 34.18710788661938693 ) ) ;
#18900 = CARTESIAN_POINT ( 'NONE',  ( 5.895881250540457863, -15.78739120953167330, -12.46137875218881952 ) ) ;
#18901 = PRODUCT_DEFINITION_FORMATION_WITH_SPECIFIED_SOURCE ( 'ANY', '', #34426, .NOT_KNOWN. ) ;
#18902 = ORIENTED_EDGE ( 'NONE', *, *, #19256, .T. ) ;
#18903 = VERTEX_POINT ( 'NONE', #30859 ) ;
#18904 = CARTESIAN_POINT ( 'NONE',  ( 0.9757892942422808913, -11.15510465568972265, -41.43309903783668346 ) ) ;
#18905 = EDGE_CURVE ( 'NONE', #51992, #20695, #49605, .T. ) ;
#18906 = VERTEX_POINT ( 'NONE', #22393 ) ;
#18907 = CARTESIAN_POINT ( 'NONE',  ( 4.975610109902397937, -23.13264022976583334, 43.09675583078141869 ) ) ;
#18908 = CARTESIAN_POINT ( 'NONE',  ( 1.091591847532194626, -41.86498133637820018, 2.020477334826483951 ) ) ;
#18909 = ORIENTED_EDGE ( 'NONE', *, *, #22713, .F. ) ;
#18910 = ADVANCED_FACE ( 'NONE', ( #40920 ), #57765, .T. ) ;
#18911 = EDGE_LOOP ( 'NONE', ( #32863, #44841 ) ) ;
#18912 = LINE ( 'NONE', #31524, #47708 ) ;
#18913 = ORIENTED_EDGE ( 'NONE', *, *, #33919, .F. ) ;
#18914 = DIRECTION ( 'NONE',  ( 0.000000000000000000, 0.000000000000000000, 1.000000000000000000 ) ) ;
#18915 = CARTESIAN_POINT ( 'NONE',  ( -6.072942160501519915, -8.919639966878049719, -17.06587780192662507 ) ) ;
#18916 = B_SPLINE_CURVE_WITH_KNOTS ( 'NONE', 3,
 ( #44708, #59073, #49378, #30268, #35617, #48763 ),
 .UNSPECIFIED., .F., .F.,
 ( 4, 2, 4 ),
 ( 5.421010862427522170E-19, 0.0002293801035737097786, 0.0004587602071474190151 ),
 .UNSPECIFIED. ) ;
#18917 = VERTEX_POINT ( 'NONE', #49976 ) ;
#18918 = DIRECTION ( 'NONE',  ( 1.000000000000000000, 0.000000000000000000, 0.000000000000000000 ) ) ;
#18919 = CARTESIAN_POINT ( 'NONE',  ( 0.9747592971366235703, -34.23774590565619746, -25.86343094887217475 ) ) ;
#18920 = ORIENTED_EDGE ( 'NONE', *, *, #34026, .T. ) ;
#18921 = VECTOR ( 'NONE', #25188, 1000.000000000000000 ) ;
#18922 = ORIENTED_EDGE ( 'NONE', *, *, #17818, .T. ) ;
#18923 = CARTESIAN_POINT ( 'NONE',  ( -6.078726893082806448, -16.13637198556892827, -10.50768958487384808 ) ) ;
#18924 = ORIENTED_EDGE ( 'NONE', *, *, #20227, .T. ) ;
#18925 = CARTESIAN_POINT ( 'NONE',  ( 0.6027444965799114707, 46.56435540091575831, 15.59805507057365936 ) ) ;
#18926 = LINE ( 'NONE', #13924, #52251 ) ;
#18927 = CARTESIAN_POINT ( 'NONE',  ( 3.238018933889920792, -3.704930136113386840, 12.87171259212121299 ) ) ;
#18928 = CARTESIAN_POINT ( 'NONE',  ( 0.1084644655670283925, 6.022910953206533691, 42.70194587816330767 ) ) ;
#18929 = EDGE_CURVE ( 'NONE', #32930, #10204, #31817, .T. ) ;
#18930 = ORIENTED_EDGE ( 'NONE', *, *, #49357, .F. ) ;
#18931 = LINE ( 'NONE', #47423, #32918 ) ;
#18932 = CARTESIAN_POINT ( 'NONE',  ( 4.962356264823608143, 0.000000000000000000, 0.000000000000000000 ) ) ;
#18933 = CARTESIAN_POINT ( 'NONE',  ( 0.5830082357119558134, 36.97260366664089304, -28.84889275254475649 ) ) ;
#18934 = B_SPLINE_CURVE_WITH_KNOTS ( 'NONE', 3,
 ( #3819, #22955, #12032, #59602 ),
 .UNSPECIFIED., .F., .F.,
 ( 4, 4 ),
 ( 2.168404344971008868E-19, 0.004048833967417087357 ),
 .UNSPECIFIED. ) ;
#18935 = CIRCLE ( 'NONE', #26926, 48.91267123290010943 ) ;
#18936 = ORIENTED_EDGE ( 'NONE', *, *, #46935, .T. ) ;
#18937 = CARTESIAN_POINT ( 'NONE',  ( 43.00000000000000000, 0.000000000000000000, 12.50000000000000000 ) ) ;
#18938 = CARTESIAN_POINT ( 'NONE',  ( 2.528190830796659405, 41.74865909485399129, -4.393586227066999861 ) ) ;
#18939 = CARTESIAN_POINT ( 'NONE',  ( 0.5988103564986357874, 38.53259703935791691, 28.80261217992934419 ) ) ;
#18940 = AXIS2_PLACEMENT_3D ( 'NONE', #37214, #32504, #40691 ) ;
#18941 = EDGE_LOOP ( 'NONE', ( #57424, #31775, #23832, #39439 ) ) ;
#18942 = EDGE_LOOP ( 'NONE', ( #15841, #27522, #35878, #14547 ) ) ;
#18943 = CARTESIAN_POINT ( 'NONE',  ( 1.227938101723748288, 17.20315230597897482, -39.32113113558949635 ) ) ;
#18944 = CARTESIAN_POINT ( 'NONE',  ( 0.5809828226811544205, 33.48000389720665027, -34.25055090842118233 ) ) ;
#18945 = CARTESIAN_POINT ( 'NONE',  ( 0.1073791018717483448, -39.65380858626227223, 16.95003405440244038 ) ) ;
#18946 = FACE_OUTER_BOUND ( 'NONE', #60846, .T. ) ;
#18947 = CARTESIAN_POINT ( 'NONE',  ( 0.6001305935487422083, 28.87057754790937381, -38.48510059944018735 ) ) ;
#18948 = CARTESIAN_POINT ( 'NONE',  ( -6.015611763856276717, -4.882992715191428523, 18.19956619163656697 ) ) ;
#18949 = CARTESIAN_POINT ( 'NONE',  ( 4.303969348037258058, -22.16169334783867484, 42.70173985163810215 ) ) ;
#18950 = FACE_OUTER_BOUND ( 'NONE', #36016, .T. ) ;
#18951 = CARTESIAN_POINT ( 'NONE',  ( 4.956653778116949738, 45.71126949320249366, 14.93973939759898606 ) ) ;
#18952 = EDGE_CURVE ( 'NONE', #44276, #28569, #53374, .T. ) ;
#18953 = CARTESIAN_POINT ( 'NONE',  ( 5.895881250540457863, 19.00150250643885386, 6.593222588848265175 ) ) ;
#18954 = CARTESIAN_POINT ( 'NONE',  ( -6.015611763856276717, 2.465697960551318069, -18.68122482568277221 ) ) ;
#18955 = CARTESIAN_POINT ( 'NONE',  ( 5.958863334805807099, -5.313608583996383139, -19.82594244347351520 ) ) ;
#18956 = ORIENTED_EDGE ( 'NONE', *, *, #1646, .T. ) ;
#18957 = B_SPLINE_CURVE_WITH_KNOTS ( 'NONE', 3,
 ( #40272, #60868, #50859, #60556, #31451, #60248, #51464, #56176, #36795, #17363, #8247, #21747, #55867, #41184, #32392, #13285, #36174, #55239, #22363 ),
 .UNSPECIFIED., .F., .F.,
 ( 4, 3, 3, 3, 3, 3, 4 ),
 ( 1.149162571898268292E-16, 0.0002618519381806292778, 0.0003927759815485966258, 0.0005237000248299431048, 0.0006546240681324950062, 0.0007855481115631322755, 0.0009699050456655125682 ),
 .UNSPECIFIED. ) ;
#18958 = LINE ( 'NONE', #9223, #59915 ) ;
#18959 = CARTESIAN_POINT ( 'NONE',  ( 4.553261556744873317, 17.98701270972406618, 40.07501640179154379 ) ) ;
#18960 = CARTESIAN_POINT ( 'NONE',  ( 0.8751705887134423323, -33.37254303619531726, -34.63284514348573850 ) ) ;
#18961 = CARTESIAN_POINT ( 'NONE',  ( 5.896782393890504181, -15.78060201202815094, -12.46991126736615385 ) ) ;
#18962 = CARTESIAN_POINT ( 'NONE',  ( 4.967162193818129623, -19.45289607368849616, 38.44485641567065670 ) ) ;
#18963 = CARTESIAN_POINT ( 'NONE',  ( 0.9722240750034567558, -39.41582016107710018, 16.95645446544471824 ) ) ;
#18964 = EDGE_CURVE ( 'NONE', #10097, #38122, #56375, .T. ) ;
#18965 = CONTEXT_DEPENDENT_SHAPE_REPRESENTATION ( #56364, #19349 ) ;
#18966 = DIRECTION ( 'NONE',  ( 0.000000000000000000, 0.000000000000000000, 1.000000000000000000 ) ) ;
#18967 =( BOUNDED_SURFACE ( )  B_SPLINE_SURFACE ( 3, 1, ( 
 ( #20021, #29390 ),
 ( #43209, #28776 ),
 ( #5257, #23773 ),
 ( #9994, #14389 ) ),
 .UNSPECIFIED., .F., .F., .F. ) 
 B_SPLINE_SURFACE_WITH_KNOTS ( ( 4, 4 ),
 ( 2, 2 ),
 ( 0.000000000000000000, 1.000000000000000000 ),
 ( 0.000000000000000000, 1.000000000000000000 ),
 .UNSPECIFIED. ) 
 GEOMETRIC_REPRESENTATION_ITEM ( )  RATIONAL_B_SPLINE_SURFACE ( (
 ( 1.000000000000000000, 1.000000000000000000),
 ( 0.9953390228620291325, 0.8624445117760984880),
 ( 0.9953390228620291325, 0.8624445117760984880),
 ( 1.000000000000000000, 1.000000000000000000) ) ) 
 REPRESENTATION_ITEM ( '' )  SURFACE ( )  );
#18968 = CIRCLE ( 'NONE', #20962, 9.500000000000000000 ) ;
#18969 = CARTESIAN_POINT ( 'NONE',  ( 0.6029443199889047422, 48.20182254088276608, -9.387328991339774831 ) ) ;
#18970 = B_SPLINE_CURVE_WITH_KNOTS ( 'NONE', 3,
 ( #36488, #8890, #31781, #60563 ),
 .UNSPECIFIED., .F., .F.,
 ( 4, 4 ),
 ( 0.002290414566844504660, 0.004042984057420971958 ),
 .UNSPECIFIED. ) ;
#18971 = CARTESIAN_POINT ( 'NONE',  ( 0.7056313189692693388, 10.05087499617880908, -45.81188225524841329 ) ) ;
#18972 = ADVANCED_FACE ( 'NONE', ( #41219 ), #9800, .T. ) ;
#18973 = CARTESIAN_POINT ( 'NONE',  ( 4.956653778116986153, -48.02038484091102077, 2.599733001514167086 ) ) ;
#18975 = ORIENTED_EDGE ( 'NONE', *, *, #51209, .T. ) ;
#18974 = CARTESIAN_POINT ( 'NONE',  ( 0.9730545539215883499, -36.90443313492345823, 21.89037132892422832 ) ) ;
#18976 = ORIENTED_EDGE ( 'NONE', *, *, #39855, .T. ) ;
#18977 = AXIS2_PLACEMENT_3D ( 'NONE', #11305, #44848, #27559 ) ;
#18978 = LINE ( 'NONE', #42174, #26867 ) ;
#18979 = CARTESIAN_POINT ( 'NONE',  ( 0.1129192098497447394, 14.78321943369649283, -41.57412910645673776 ) ) ;
#18980 = CARTESIAN_POINT ( 'NONE',  ( 0.8554163680231816613, -41.45413358837884488, 21.97180651536553952 ) ) ;
#18981 = ORIENTED_EDGE ( 'NONE', *, *, #20951, .F. ) ;
#18982 = DIRECTION ( 'NONE',  ( 0.000000000000000000, 0.000000000000000000, -1.000000000000000000 ) ) ;
#18983 = DIRECTION ( 'NONE',  ( 0.09835009131224552170, -0.2650256080583695550, -0.9592125346408710840 ) ) ;
#18984 = CARTESIAN_POINT ( 'NONE',  ( 0.8557997880470697982, 28.43566216845025352, -38.55640757422408882 ) ) ;
#18985 = ORIENTED_EDGE ( 'NONE', *, *, #15178, .F. ) ;
#18986 = ORIENTED_EDGE ( 'NONE', *, *, #59946, .T. ) ;
#18987 = CARTESIAN_POINT ( 'NONE',  ( 0.9754292589017242721, 33.24763086278803570, 25.51318304146031579 ) ) ;
#18988 = EDGE_CURVE ( 'NONE', #27840, #33545, #6726, .T. ) ;
#18989 = CONICAL_SURFACE ( 'NONE', #1909, 42.92674063221959813, 1.485477209440487556 ) ;
#18990 = CARTESIAN_POINT ( 'NONE',  ( 5.959547316686252039, 7.858107265727477753, 18.96183906913546480 ) ) ;
#18991 = CARTESIAN_POINT ( 'NONE',  ( 0.5830082357119539260, 17.10941071709084937, -43.66348703267112086 ) ) ;
#18992 = EDGE_CURVE ( 'NONE', #5228, #6983, #38436, .T. ) ;
#18993 = CARTESIAN_POINT ( 'NONE',  ( 5.896278296736517710, 14.91306641426024093, 13.49545959714773424 ) ) ;
#18994 = CARTESIAN_POINT ( 'NONE',  ( 1.231276596079887264, -6.136529359146732254, 41.46829847537028257 ) ) ;
#18995 = ADVANCED_FACE ( 'NONE', ( #38072 ), #14784, .T. ) ;
#18996 = CARTESIAN_POINT ( 'NONE',  ( 0.5827357941260199459, 37.77622264066054214, -29.44458568814473054 ) ) ;
#18997 = EDGE_LOOP ( 'NONE', ( #43022, #14999, #3230, #22512 ) ) ;
#18998 = CARTESIAN_POINT ( 'NONE',  ( -2.569797478183790229, -6.924386868080758539, -12.89088113963433457 ) ) ;
#18999 = CARTESIAN_POINT ( 'NONE',  ( 0.8560838555295223751, -44.60403252362528548, -14.52078223489045072 ) ) ;
#19000 = ORIENTED_EDGE ( 'NONE', *, *, #43902, .T. ) ;
#19001 = CARTESIAN_POINT ( 'NONE',  ( 0.1149546198390367924, 41.96184135302931395, -13.64369580745698762 ) ) ;
#19002 = CARTESIAN_POINT ( 'NONE',  ( 0.1129192098497447394, -35.06977877439262414, 26.77802092202325213 ) ) ;
#19003 = LINE ( 'NONE', #38119, #57732 ) ;
#19004 = CARTESIAN_POINT ( 'NONE',  ( 1.088313998177379283, 15.69908095455155639, 39.93881167962107526 ) ) ;
#19005 = EDGE_CURVE ( 'NONE', #23785, #33784, #52813, .T. ) ;
#19006 = ORIENTED_EDGE ( 'NONE', *, *, #43228, .T. ) ;
#19007 = ORIENTED_EDGE ( 'NONE', *, *, #40907, .F. ) ;
#19008 = CARTESIAN_POINT ( 'NONE',  ( 0.1129192098497447394, -44.12161472487018443, 0.4846667466135898827 ) ) ;
#19009 = CARTESIAN_POINT ( 'NONE',  ( 5.896782393890504181, 0.6657210432558627877, -20.10181341000305366 ) ) ;
#19010 = FACE_OUTER_BOUND ( 'NONE', #15378, .T. ) ;
#19011 = ORIENTED_EDGE ( 'NONE', *, *, #44249, .T. ) ;
#19012 = DIRECTION ( 'NONE',  ( 0.000000000000000000, 0.000000000000000000, 1.000000000000000000 ) ) ;
#19013 = VERTEX_POINT ( 'NONE', #33359 ) ;
#19014 = CARTESIAN_POINT ( 'NONE',  ( 4.553261556744873317, -14.95853073564509828, 41.30111286702087625 ) ) ;
#19015 = CARTESIAN_POINT ( 'NONE',  ( 0.6027444965799114707, -25.56852311693717894, 41.92599601090104500 ) ) ;
#19016 = VECTOR ( 'NONE', #49094, 999.9999999999998863 ) ;
#19017 = ORIENTED_EDGE ( 'NONE', *, *, #60703, .F. ) ;
#19018 = CARTESIAN_POINT ( 'NONE',  ( 0.5839879882012681822, -47.48621496524027208, -6.251648354650674477 ) ) ;
#19019 = CARTESIAN_POINT ( 'NONE',  ( 0.9754292580325135686, -30.68784781142436557, -28.54090859813089054 ) ) ;
#19020 = CARTESIAN_POINT ( 'NONE',  ( 4.975801465491694664, -26.14269827151650816, -40.15204426031524321 ) ) ;
#19021 = B_SPLINE_CURVE_WITH_KNOTS ( 'NONE', 3,
 ( #46524, #35590, #16785, #59357 ),
 .UNSPECIFIED., .F., .F.,
 ( 4, 4 ),
 ( 2.308109569601360422E-17, 0.004559932413162185935 ),
 .UNSPECIFIED. ) ;
#19022 = ORIENTED_EDGE ( 'NONE', *, *, #56510, .T. ) ;
#19023 = CARTESIAN_POINT ( 'NONE',  ( 0.6253024248130472085, -0.8873488924062337135, -49.09844029458358250 ) ) ;
#19024 = DIRECTION ( 'NONE',  ( -1.000000000000000000, -3.673819061467147552E-16, 1.925929944387235306E-32 ) ) ;
#19025 = CARTESIAN_POINT ( 'NONE',  ( 0.5980271706414711508, 22.09347986454737622, 43.86259671196521026 ) ) ;
#19026 = CARTESIAN_POINT ( 'NONE',  ( 0.6023143664670691511, 29.49326149840232247, -38.00627775314932677 ) ) ;
#19027 = B_SPLINE_CURVE_WITH_KNOTS ( 'NONE', 3,
 ( #42288, #13779, #3407, #36657, #60418, #56345, #32886, #51338, #60731, #56656, #41363, #46987, #27545, #51648, #41984, #3110 ),
 .UNSPECIFIED., .F., .F.,
 ( 4, 3, 3, 3, 3, 4 ),
 ( 5.057544569639795705E-18, 0.0005656085177311398569, 0.001131215744874500056, 0.001696821861372766350, 0.002262427090022499018, 0.002715792992282060631 ),
 .UNSPECIFIED. ) ;
#19028 = DIRECTION ( 'NONE',  ( -0.07836865515943411409, 0.007886984708657411927, 0.9968932487286223942 ) ) ;
#19029 = ORIENTED_EDGE ( 'NONE', *, *, #58638, .T. ) ;
#19030 = CARTESIAN_POINT ( 'NONE',  ( 0.7056759521545010738, -42.23392822606338370, 20.39715999134963198 ) ) ;
#19031 = EDGE_CURVE ( 'NONE', #2992, #54794, #39221, .T. ) ;
#19032 = CARTESIAN_POINT ( 'NONE',  ( 3.050102900204245682, -16.13753096457668335, 40.92682914110729087 ) ) ;
#19033 = VECTOR ( 'NONE', #24877, 1000.000000000000000 ) ;
#19034 = ORIENTED_EDGE ( 'NONE', *, *, #32303, .T. ) ;
#19035 = ADVANCED_FACE ( 'NONE', ( #9521 ), #47443, .T. ) ;
#19036 = CARTESIAN_POINT ( 'NONE',  ( 0.5806925824938499181, -34.41156632303712826, -31.86010774524751454 ) ) ;
#19037 = CARTESIAN_POINT ( 'NONE',  ( 0.1073791018717483448, -39.65380858626227223, 16.95003405440244038 ) ) ;
#19038 = CARTESIAN_POINT ( 'NONE',  ( 5.901463166500146684, 14.92627229327871596, 13.48051429907393306 ) ) ;
#19039 = CARTESIAN_POINT ( 'NONE',  ( 0.8751705887134423323, 47.79200036674280483, -5.393078191592203474 ) ) ;
#19040 = CARTESIAN_POINT ( 'NONE',  ( 1.000433927950264090, -6.320470408796723838, 41.43030691974620083 ) ) ;
#19041 = B_SPLINE_CURVE_WITH_KNOTS ( 'NONE', 3,
 ( #30255, #1427, #830, #6729 ),
 .UNSPECIFIED., .F., .F.,
 ( 4, 4 ),
 ( 0.000000000000000000, 0.005014147105413705591 ),
 .UNSPECIFIED. ) ;
#19042 = DIRECTION ( 'NONE',  ( 0.000000000000000000, 0.000000000000000000, 1.000000000000000000 ) ) ;
#19043 = CARTESIAN_POINT ( 'NONE',  ( 0.5839254288179533958, -47.89590036163259157, -0.09078831291274436222 ) ) ;
#19044 = ADVANCED_FACE ( 'NONE', ( #41839 ), #37762, .T. ) ;
#19045 = DIRECTION ( 'NONE',  ( 1.000000000000000000, -8.031849550658623177E-18, 6.323743061686233666E-22 ) ) ;
#19046 = CARTESIAN_POINT ( 'NONE',  ( 0.6028618097248862329, 47.71844004092979930, 6.106174977919211599 ) ) ;
#19047 = CARTESIAN_POINT ( 'NONE',  ( 0.8751705887134553219, 28.56654290188653178, -38.69254731947804515 ) ) ;
#19048 = EDGE_CURVE ( 'NONE', #32640, #44566, #61645, .T. ) ;
#19049 = DIRECTION ( 'NONE',  ( 0.07906939808003032866, -0.9208896734047763433, 0.3817201064965091151 ) ) ;
#19050 = ORIENTED_EDGE ( 'NONE', *, *, #48933, .T. ) ;
#19051 = EDGE_LOOP ( 'NONE', ( #52943, #17550, #37320, #4939 ) ) ;
#19052 = CARTESIAN_POINT ( 'NONE',  ( 4.303969348037258058, 22.16169334783896971, -42.70173985163793873 ) ) ;
#19053 = CARTESIAN_POINT ( 'NONE',  ( 48.19985924247141185, 15.44373933981895952, -1.327350711001176631 ) ) ;
#19054 = CARTESIAN_POINT ( 'NONE',  ( 0.5806925824938502512, 23.01490136172913026, 40.85996423950273737 ) ) ;
#19055 = CARTESIAN_POINT ( 'NONE',  ( 0.9740398440564312921, 42.48528956276145152, -6.011466167923673609 ) ) ;
#19056 = CARTESIAN_POINT ( 'NONE',  ( 0.6028618097248864549, -38.05975027458356408, 29.42431480658666132 ) ) ;
#19057 = B_SPLINE_CURVE_WITH_KNOTS ( 'NONE', 3,
 ( #22312, #36123, #51407, #56113 ),
 .UNSPECIFIED., .F., .F.,
 ( 4, 4 ),
 ( 1.387948177032400748E-17, 0.005004948556313828720 ),
 .UNSPECIFIED. ) ;
#19058 = ORIENTED_EDGE ( 'NONE', *, *, #38941, .F. ) ;
#19059 = B_SPLINE_CURVE_WITH_KNOTS ( 'NONE', 3,
 ( #9224, #23949, #48067, #24247, #9850, #5427, #19567, #28951, #52748, #42460, #24563, #743, #8923, #38378, #43385, #57740, #43074, #61520, #33365 ),
 .UNSPECIFIED., .F., .F.,
 ( 4, 3, 3, 3, 3, 3, 4 ),
 ( 1.138109825968292890E-16, 0.0002618519381806256457, 0.0003927759815485970594, 0.0005237000248299464658, 0.0006546240681324991262, 0.0007855481115631363954, 0.0009699050456655126766 ),
 .UNSPECIFIED. ) ;
#19060 = DIRECTION ( 'NONE',  ( -1.000000000000000000, -0.000000000000000000, -0.000000000000000000 ) ) ;
#19061 = EDGE_CURVE ( 'NONE', #50265, #10364, #37443, .T. ) ;
#19062 = FACE_OUTER_BOUND ( 'NONE', #26938, .T. ) ;
#19063 = CARTESIAN_POINT ( 'NONE',  ( -6.077587904424778920, 0.6110050725289616347, 19.24636833782608392 ) ) ;
#19064 = EDGE_CURVE ( 'NONE', #29464, #50394, #54884, .T. ) ;
#19065 = ORIENTED_EDGE ( 'NONE', *, *, #48344, .T. ) ;
#19066 = CARTESIAN_POINT ( 'NONE',  ( 1.088908134280554885, -30.89124834763367744, -29.78762923589999900 ) ) ;
#19067 = EDGE_CURVE ( 'NONE', #32330, #27931, #13758, .T. ) ;
#19068 = CARTESIAN_POINT ( 'NONE',  ( 0.5839254288179563934, 47.49799454719525471, -6.161657890844459473 ) ) ;
#19069 = EDGE_LOOP ( 'NONE', ( #54363, #10596 ) ) ;
#19070 = CARTESIAN_POINT ( 'NONE',  ( 0.5809828226811617480, -44.45562576850614533, 17.82437196699665094 ) ) ;
#19071 = ORIENTED_EDGE ( 'NONE', *, *, #9612, .T. ) ;
#19072 = CARTESIAN_POINT ( 'NONE',  ( -6.016104459813371719, -13.32794178584988209, -13.32039631884698494 ) ) ;
#19073 = AXIS2_PLACEMENT_3D ( 'NONE', #24849, #20768, #43990 ) ;
#19074 = FACE_OUTER_BOUND ( 'NONE', #27004, .T. ) ;
#19075 = ORIENTED_EDGE ( 'NONE', *, *, #48978, .F. ) ;
#19076 = DIRECTION ( 'NONE',  ( 0.000000000000000000, 0.000000000000000000, -1.000000000000000000 ) ) ;
#19077 = CARTESIAN_POINT ( 'NONE',  ( 0.9780303403264770656, 40.50400539199167582, 10.75942194546684760 ) ) ;
#19078 = CARTESIAN_POINT ( 'NONE',  ( 0.8560838555295158248, -29.58154842764465542, -36.40473632241614155 ) ) ;
#19079 = ADVANCED_FACE ( 'NONE', ( #33660 ), #5564, .F. ) ;
#19080 = VERTEX_POINT ( 'NONE', #28945 ) ;
#19081 = B_SPLINE_CURVE_WITH_KNOTS ( 'NONE', 3,
 ( #28152, #18457, #42284, #57250 ),
 .UNSPECIFIED., .F., .F.,
 ( 4, 4 ),
 ( 3.127317220692750759E-18, 0.004042984057420974560 ),
 .UNSPECIFIED. ) ;
#19082 = CARTESIAN_POINT ( 'NONE',  ( 0.6029443199889047422, -7.837561479521124141, -48.47793592872049118 ) ) ;
#19083 = ORIENTED_EDGE ( 'NONE', *, *, #19064, .T. ) ;
#19084 = CARTESIAN_POINT ( 'NONE',  ( 5.959547316686252039, 12.49803383497749820, -16.28190225198605745 ) ) ;
#19085 = EDGE_CURVE ( 'NONE', #44253, #5033, #10081, .T. ) ;
#19086 = EDGE_LOOP ( 'NONE', ( #14548, #1292, #16183, #39678 ) ) ;
#19087 = VERTEX_POINT ( 'NONE', #60905 ) ;
#19088 = CARTESIAN_POINT ( 'NONE',  ( -4.908599999999998964, 9.539392014169456147, 3.000000000000000000 ) ) ;
#19089 = CARTESIAN_POINT ( 'NONE',  ( 0.9780106845699467755, -37.54462564979032635, 18.62075001906600136 ) ) ;
#19090 = CARTESIAN_POINT ( 'NONE',  ( 0.6067099128993237445, 46.44339333106615442, 11.71051825714719463 ) ) ;
#19091 = CARTESIAN_POINT ( 'NONE',  ( 0.9268187852002115479, -28.25673427553589434, -33.84244821212526944 ) ) ;
#19092 = ORIENTED_EDGE ( 'NONE', *, *, #46640, .T. ) ;
#19093 = CARTESIAN_POINT ( 'NONE',  ( 0.9752570700956806338, 0.2306661201227225566, -42.90785210525867654 ) ) ;
#19094 = CARTESIAN_POINT ( 'NONE',  ( 5.838029081930955932, -22.68231883182838260, -41.43159990350605426 ) ) ;
#19095 = DIRECTION ( 'NONE',  ( -0.1011922191286467598, 0.4144321176143397900, -0.9044369268652812099 ) ) ;
#19096 = VERTEX_POINT ( 'NONE', #37138 ) ;
#19097 = ORIENTED_EDGE ( 'NONE', *, *, #16348, .F. ) ;
#19098 = CARTESIAN_POINT ( 'NONE',  ( 4.958415959904816539, 42.74072562871904779, -15.37642112304408037 ) ) ;
#19099 = CARTESIAN_POINT ( 'NONE',  ( -6.077587904424778920, -6.656176160390447905, -18.06907137391903717 ) ) ;
#19100 = CARTESIAN_POINT ( 'NONE',  ( 0.1097557419366048670, 30.65094619415025434, 30.33543403792248228 ) ) ;
#19101 = CARTESIAN_POINT ( 'NONE',  ( 0.1087620492084205165, -34.43219573047449700, 25.96440931622072767 ) ) ;
#19102 = B_SPLINE_CURVE_WITH_KNOTS ( 'NONE', 3,
 ( #33141, #13726, #9311, #28412, #47539, #23727 ),
 .UNSPECIFIED., .F., .F.,
 ( 4, 2, 4 ),
 ( 1.553373257785006303E-17, 0.0002293319059085063220, 0.0004586638118169971399 ),
 .UNSPECIFIED. ) ;
#19103 = CARTESIAN_POINT ( 'NONE',  ( 0.9784957157296367836, 38.67345032168838515, 16.14612328728703616 ) ) ;
#19104 = EDGE_LOOP ( 'NONE', ( #13273, #4772, #37632, #49374 ) ) ;
#19105 = B_SPLINE_CURVE_WITH_KNOTS ( 'NONE', 3,
 ( #54621, #25833, #58396, #10507 ),
 .UNSPECIFIED., .F., .F.,
 ( 4, 4 ),
 ( 0.000000000000000000, 0.004446090762761384201 ),
 .UNSPECIFIED. ) ;
#19106 = ORIENTED_EDGE ( 'NONE', *, *, #27858, .F. ) ;
#19107 = EDGE_CURVE ( 'NONE', #42620, #29913, #56205, .T. ) ;
#19108 = CARTESIAN_POINT ( 'NONE',  ( 4.962356264823608143, -19.84272732133934269, -37.11471096901227185 ) ) ;
#19109 = CARTESIAN_POINT ( 'NONE',  ( 0.8760168074886965917, 37.61398439004493355, 29.98565522133359806 ) ) ;
#19110 = CARTESIAN_POINT ( 'NONE',  ( 0.9268187852002115479, -38.89159468621753035, -20.76531231818109191 ) ) ;
#19111 = DIRECTION ( 'NONE',  ( 0.000000000000000000, 0.000000000000000000, 1.000000000000000000 ) ) ;
#19112 = CARTESIAN_POINT ( 'NONE',  ( 0.7057020205115001055, 7.085441699094293000, -47.37450661940661689 ) ) ;
#19113 = ADVANCED_FACE ( 'NONE', ( #56514 ), #39272, .F. ) ;
#19114 = SURFACE_SIDE_STYLE ('',( #57274 ) ) ;
#19115 = CARTESIAN_POINT ( 'NONE',  ( 0.6023142530420679819, 0.2618396477460823712, 48.10676733004997629 ) ) ;
#19116 = VECTOR ( 'NONE', #25165, 1000.000000000000000 ) ;
#19117 = ORIENTED_EDGE ( 'NONE', *, *, #55497, .T. ) ;
#19118 = CARTESIAN_POINT ( 'NONE',  ( 0.6039202388192953519, 49.01762936092966783, 2.972494690241990423 ) ) ;
#19119 = CARTESIAN_POINT ( 'NONE',  ( 50.15577769773999961, 12.80000000000000071, -3.000000000000000000 ) ) ;
#19120 = EDGE_CURVE ( 'NONE', #35558, #25685, #4054, .T. ) ;
#19121 = LINE ( 'NONE', #33832, #41884 ) ;
#19122 = EDGE_CURVE ( 'NONE', #1997, #9596, #20472, .T. ) ;
#19123 = CARTESIAN_POINT ( 'NONE',  ( 0.5807400328401574052, -41.20655774452986719, 24.41979442053154514 ) ) ;
#19124 = EDGE_CURVE ( 'NONE', #32260, #57388, #39958, .T. ) ;
#19125 = CARTESIAN_POINT ( 'NONE',  ( 0.9785694773339252972, -34.67671301199700906, 23.53425121813456045 ) ) ;
#19126 = CARTESIAN_POINT ( 'NONE',  ( 0.6845945791218034371, -6.946890923033673282, -46.39124084584735641 ) ) ;
#19127 = B_SPLINE_CURVE_WITH_KNOTS ( 'NONE', 3,
 ( #49184, #15069, #58877, #53555 ),
 .UNSPECIFIED., .F., .F.,
 ( 4, 4 ),
 ( 0.000000000000000000, 0.005013413432710141573 ),
 .UNSPECIFIED. ) ;
#19128 = ADVANCED_FACE ( 'NONE', ( #34896 ), #11640, .F. ) ;
#19129 = CARTESIAN_POINT ( 'NONE',  ( -6.072942160501519915, -12.95676005301696421, -14.24522836663435577 ) ) ;
#19130 = ORIENTED_EDGE ( 'NONE', *, *, #57338, .T. ) ;
#19131 = CARTESIAN_POINT ( 'NONE',  ( 0.5807400328401574052, 28.72484455891640920, 38.33001520688959829 ) ) ;
#19132 = CARTESIAN_POINT ( 'NONE',  ( 0.6067375320500714153, 47.38951440911015567, 6.954068056450886104 ) ) ;
#19133 = FACE_OUTER_BOUND ( 'NONE', #11360, .T. ) ;
#19134 = CARTESIAN_POINT ( 'NONE',  ( 2.624215991343608501, 42.26352390376127488, -22.77108897942091659 ) ) ;
#19135 = EDGE_LOOP ( 'NONE', ( #44574, #24461, #53840, #27934 ) ) ;
#19136 = CARTESIAN_POINT ( 'NONE',  ( 1.542467486220083783, -0.2257246335812510551, -44.06061125825107894 ) ) ;
#19137 = CARTESIAN_POINT ( 'NONE',  ( 0.5804410086790514622, 11.40290849443471899, 45.49168638029310330 ) ) ;
#19138 =( BOUNDED_SURFACE ( )  B_SPLINE_SURFACE ( 3, 1, ( 
 ( #182, #61589 ),
 ( #37523, #23712 ),
 ( #56592, #47839 ),
 ( #52508, #9597 ) ),
 .UNSPECIFIED., .F., .F., .F. ) 
 B_SPLINE_SURFACE_WITH_KNOTS ( ( 4, 4 ),
 ( 2, 2 ),
 ( 0.000000000000000000, 1.000000000000000000 ),
 ( 0.000000000000000000, 1.000000000000000000 ),
 .UNSPECIFIED. ) 
 GEOMETRIC_REPRESENTATION_ITEM ( )  RATIONAL_B_SPLINE_SURFACE ( (
 ( 1.000000000000000000, 1.000000000000000000),
 ( 0.7223157951917480446, 0.9931996967497186413),
 ( 0.7223157951917480446, 0.9931996967497186413),
 ( 1.000000000000000000, 1.000000000000000000) ) ) 
 REPRESENTATION_ITEM ( '' )  SURFACE ( )  );
#19139 = CARTESIAN_POINT ( 'NONE',  ( 4.956653778116961284, 40.28700667097682953, 26.26162724282386662 ) ) ;
#19140 = ORIENTED_EDGE ( 'NONE', *, *, #39638, .F. ) ;
#19141 = CARTESIAN_POINT ( 'NONE',  ( 0.6845945791218034371, -29.61886432665992430, -36.37484565895580602 ) ) ;
#19142 = CARTESIAN_POINT ( 'NONE',  ( 4.963659409799330291, -42.53037318520986076, -13.93274247732065696 ) ) ;
#19143 = ORIENTED_EDGE ( 'NONE', *, *, #53944, .T. ) ;
#19144 = CARTESIAN_POINT ( 'NONE',  ( 0.6252788684277206244, -31.15129425738415847, -37.96104842155354220 ) ) ;
#19145 = ORIENTED_EDGE ( 'NONE', *, *, #15207, .F. ) ;
#19146 = CARTESIAN_POINT ( 'NONE',  ( 0.8744876279028306332, -38.80702141274064587, 30.07266432244707843 ) ) ;
#19147 = VERTEX_POINT ( 'NONE', #48360 ) ;
#19148 = CARTESIAN_POINT ( 'NONE',  ( 5.895596859100789899, 8.462961974658767872, -18.24572437114973056 ) ) ;
#19149 = DIRECTION ( 'NONE',  ( 0.000000000000000000, -1.000000000000000000, 0.000000000000000000 ) ) ;
#19150 = ORIENTED_EDGE ( 'NONE', *, *, #38232, .T. ) ;
#19151 = CARTESIAN_POINT ( 'NONE',  ( 4.291220156522060236, 31.16808953869651333, -35.32618280841412428 ) ) ;
#19152 = ORIENTED_EDGE ( 'NONE', *, *, #6824, .T. ) ;
#19153 = CARTESIAN_POINT ( 'NONE',  ( 0.8551540677456739292, -38.56334384152450667, 28.44084013485104379 ) ) ;
#19154 =( BOUNDED_SURFACE ( )  B_SPLINE_SURFACE ( 3, 1, ( 
 ( #4386, #28842 ),
 ( #43589, #57028 ),
 ( #311, #18527 ),
 ( #9117, #61407 ) ),
 .UNSPECIFIED., .F., .F., .F. ) 
 B_SPLINE_SURFACE_WITH_KNOTS ( ( 4, 4 ),
 ( 2, 2 ),
 ( 0.000000000000000000, 1.000000000000000000 ),
 ( 0.000000000000000000, 1.000000000000000000 ),
 .UNSPECIFIED. ) 
 GEOMETRIC_REPRESENTATION_ITEM ( )  RATIONAL_B_SPLINE_SURFACE ( (
 ( 1.000000000000000000, 1.000000000000000000),
 ( 0.7269869731126821222, 0.9931720237060910339),
 ( 0.7269869731126821222, 0.9931720237060910339),
 ( 1.000000000000000000, 1.000000000000000000) ) ) 
 REPRESENTATION_ITEM ( '' )  SURFACE ( )  );
#19155 = VECTOR ( 'NONE', #46233, 1000.000000000000000 ) ;
#19156 = EDGE_CURVE ( 'NONE', #24678, #22536, #53960, .T. ) ;
#19157 = CARTESIAN_POINT ( 'NONE',  ( 0.6001305935487422083, 46.33281397023046821, 12.95698906763824709 ) ) ;
#19158 = VERTEX_POINT ( 'NONE', #58978 ) ;
#19159 = CARTESIAN_POINT ( 'NONE',  ( 4.956445790444040433, 46.94638516972321440, -3.684422564748698115 ) ) ;
#19160 = CARTESIAN_POINT ( 'NONE',  ( 1.227938101723748288, -42.65467462194921922, 4.762198645644287076 ) ) ;
#19161 = CARTESIAN_POINT ( 'NONE',  ( 0.1157991065609915715, -22.80398465254558360, -37.77460323423880340 ) ) ;
#19162 = ORIENTED_EDGE ( 'NONE', *, *, #6777, .T. ) ;
#19163 = CARTESIAN_POINT ( 'NONE',  ( 0.5848930533535030563, -1.749067435711754159, 46.86377967570361847 ) ) ;
#19164 = CARTESIAN_POINT ( 'NONE',  ( 0.8760168074886960365, -42.09738177923970426, 23.27577685234524907 ) ) ;
#19165 = B_SPLINE_CURVE_WITH_KNOTS ( 'NONE', 3,
 ( #45470, #17569, #41392, #3138, #27268, #60449 ),
 .UNSPECIFIED., .F., .F.,
 ( 4, 2, 4 ),
 ( 1.238878783205199297E-16, 0.0002448718616795882716, 0.0004897437233590527274 ),
 .UNSPECIFIED. ) ;
#19166 = VERTEX_POINT ( 'NONE', #57730 ) ;
#19167 = CARTESIAN_POINT ( 'NONE',  ( 5.960721111146673579, 7.848955554238515653, -18.96557324978279624 ) ) ;
#19168 = ORIENTED_EDGE ( 'NONE', *, *, #39411, .F. ) ;
#19169 = CARTESIAN_POINT ( 'NONE',  ( 0.9736507210033054083, 25.76216842460696199, 34.31386771842671379 ) ) ;
#19170 = CARTESIAN_POINT ( 'NONE',  ( -6.016761891674564211, 11.46828378093580980, -14.95139917749692415 ) ) ;
#19171 = ORIENTED_EDGE ( 'NONE', *, *, #43459, .T. ) ;
#19172 = CARTESIAN_POINT ( 'NONE',  ( 0.9791128995231609400, -34.55414444086503778, -23.71388909913344634 ) ) ;
#19173 = DIRECTION ( 'NONE',  ( -1.000000000000000000, -0.000000000000000000, -0.000000000000000000 ) ) ;
#19174 = CARTESIAN_POINT ( 'NONE',  ( 4.975610109902397937, 0.000000000000000000, 0.000000000000000000 ) ) ;
#19175 = CARTESIAN_POINT ( 'NONE',  ( 0.2224561200757577961, -40.12166550582823277, 15.79689521915794614 ) ) ;
#19176 = ORIENTED_EDGE ( 'NONE', *, *, #34562, .F. ) ;
#19177 = CARTESIAN_POINT ( 'NONE',  ( 0.1156495703730067437, -40.84808789472971569, 16.68462371692890756 ) ) ;
#19178 = LINE ( 'NONE', #9754, #37870 ) ;
#19179 = CARTESIAN_POINT ( 'NONE',  ( 5.960721111146673579, -10.25731071096570268, -17.77882586010663246 ) ) ;
#19180 = EDGE_CURVE ( 'NONE', #4359, #54823, #56322, .T. ) ;
#19181 = CARTESIAN_POINT ( 'NONE',  ( 3.407937589446178528, -13.10584870154469606, 3.987184287467740784 ) ) ;
#19182 = CARTESIAN_POINT ( 'NONE',  ( 0.5263152470540294336, 0.000000000000000000, 0.000000000000000000 ) ) ;
#19183 = CARTESIAN_POINT ( 'NONE',  ( 4.962356264823608143, 0.000000000000000000, 0.000000000000000000 ) ) ;
#19184 = EDGE_CURVE ( 'NONE', #11109, #5908, #34823, .T. ) ;
#19185 = CARTESIAN_POINT ( 'NONE',  ( -6.016104459813374383, -2.454244026260969047, -18.68271063303497215 ) ) ;
#19186 = EDGE_CURVE ( 'NONE', #16242, #27767, #14863, .T. ) ;
#19187 = ADVANCED_FACE ( 'NONE', ( #35204 ), #22818, .T. ) ;
#19188 = CARTESIAN_POINT ( 'NONE',  ( 0.5809828226811617480, -44.03860873105681151, -18.83114015454746237 ) ) ;
#19189 = CARTESIAN_POINT ( 'NONE',  ( 4.975610109902397937, -48.84566763821283786, -2.559328059280381318 ) ) ;
#19190 = CARTESIAN_POINT ( 'NONE',  ( 0.6027935024548037868, 48.10716172909472022, 0.1745403365873163526 ) ) ;
#19191 = CARTESIAN_POINT ( 'NONE',  ( 2.000000000000027089, 3.464101615137739731, -5.600000000000000533 ) ) ;
#19192 = CARTESIAN_POINT ( 'NONE',  ( 0.1152339509894530906, 39.85093012247246946, 18.94323253378521699 ) ) ;
#19193 = CIRCLE ( 'NONE', #57153, 12.50000000000000000 ) ;
#19194 = CARTESIAN_POINT ( 'NONE',  ( 1.088908134280555995, -41.64642044161486467, -10.35121946298456486 ) ) ;
#19195 = CARTESIAN_POINT ( 'NONE',  ( 0.3676999524040366896, -17.09834788623584600, 40.66444494744877858 ) ) ;
#19196 = AXIS2_PLACEMENT_3D ( 'NONE', #23052, #3600, #32143 ) ;
#19197 = LINE ( 'NONE', #38310, #1429 ) ;
#19198 = SURFACE_SIDE_STYLE ('',( #27962 ) ) ;
#19199 = CARTESIAN_POINT ( 'NONE',  ( -6.079354080745853928, 19.09774425860446811, -2.463558296672129888 ) ) ;
#19200 = ORIENTED_EDGE ( 'NONE', *, *, #21868, .T. ) ;
#19201 = EDGE_CURVE ( 'NONE', #19843, #20243, #15168, .T. ) ;
#19202 = CARTESIAN_POINT ( 'NONE',  ( 0.5837374860065662752, 29.01294733976413553, -38.10878877974113266 ) ) ;
#19203 = CARTESIAN_POINT ( 'NONE',  ( 0.5819845079324669213, 24.34013310064393920, 41.25022834067357280 ) ) ;
#19204 = CARTESIAN_POINT ( 'NONE',  ( 3.270143674763207553, -3.277085381513213047, 13.28976595685392681 ) ) ;
#19205 = ORIENTED_EDGE ( 'NONE', *, *, #51122, .F. ) ;
#19206 = EDGE_CURVE ( 'NONE', #36885, #47523, #23493, .T. ) ;
#19207 = CARTESIAN_POINT ( 'NONE',  ( 4.694002226626921015, -38.39382765324710789, 24.58045503197395476 ) ) ;
#19208 = CARTESIAN_POINT ( 'NONE',  ( 0.5980271706414711508, -39.77423938000287507, 28.81074668563609009 ) ) ;
#19209 = UNCERTAINTY_MEASURE_WITH_UNIT (LENGTH_MEASURE( 1.000000000000000082E-05 ), #60142, 'distance_accuracy_value', 'NONE');
#19210 = VERTEX_POINT ( 'NONE', #53048 ) ;
#19211 = ORIENTED_EDGE ( 'NONE', *, *, #42273, .F. ) ;
#19212 = CARTESIAN_POINT ( 'NONE',  ( 0.6027935024548038978, -38.05972402498757390, -29.42425667880423035 ) ) ;
#19213 = ORIENTED_EDGE ( 'NONE', *, *, #27355, .F. ) ;
#19214 = CARTESIAN_POINT ( 'NONE',  ( 0.5998501479064708430, -6.798102206414489146, 47.62484632993676570 ) ) ;
#19215 = ORIENTED_EDGE ( 'NONE', *, *, #33756, .F. ) ;
#19216 = ORIENTED_EDGE ( 'NONE', *, *, #49006, .F. ) ;
#19217 = LINE ( 'NONE', #23288, #59676 ) ;
#19218 = VERTEX_POINT ( 'NONE', #34274 ) ;
#19219 = CARTESIAN_POINT ( 'NONE',  ( 0.1064266379913942628, 15.98292486309336624, -40.05351204369889473 ) ) ;
#19220 = CARTESIAN_POINT ( 'NONE',  ( 4.549368137175248350, 0.000000000000000000, 0.000000000000000000 ) ) ;
#19221 = B_SPLINE_CURVE_WITH_KNOTS ( 'NONE', 3,
 ( #58840, #22500, #4285, #32844 ),
 .UNSPECIFIED., .F., .F.,
 ( 4, 4 ),
 ( 0.000000000000000000, 0.004445488388166993383 ),
 .UNSPECIFIED. ) ;
#19222 = FACE_OUTER_BOUND ( 'NONE', #18438, .T. ) ;
#19223 = ORIENTED_EDGE ( 'NONE', *, *, #51122, .T. ) ;
#19224 = CARTESIAN_POINT ( 'NONE',  ( 4.967162193818131399, 42.16965968614193372, 8.839793687085363061 ) ) ;
#19225 = EDGE_CURVE ( 'NONE', #24495, #38023, #31720, .T. ) ;
#19226 = CARTESIAN_POINT ( 'NONE',  ( 0.9788927965476029724, -39.54311573103250765, 13.88087212367969236 ) ) ;
#19227 = EDGE_LOOP ( 'NONE', ( #23087, #47498, #19022, #27535, #28345, #56112, #14577 ) ) ;
#19228 = VERTEX_POINT ( 'NONE', #53349 ) ;
#19229 = FACE_OUTER_BOUND ( 'NONE', #24322, .T. ) ;
#19230 = EDGE_LOOP ( 'NONE', ( #55552, #29522 ) ) ;
#19231 = CARTESIAN_POINT ( 'NONE',  ( 0.6008122571543325074, 46.74120789342043025, 15.06034644785334109 ) ) ;
#19232 = CARTESIAN_POINT ( 'NONE',  ( 4.303969348037258058, -8.413118729223747039, -47.36875205922780907 ) ) ;
#19233 = DIRECTION ( 'NONE',  ( -1.000000000000000000, -0.000000000000000000, -0.000000000000000000 ) ) ;
#19234 = ORIENTED_EDGE ( 'NONE', *, *, #51350, .F. ) ;
#19235 = FACE_OUTER_BOUND ( 'NONE', #21139, .T. ) ;
#19236 = VECTOR ( 'NONE', #8691, 1000.000000000000000 ) ;
#19237 = B_SPLINE_CURVE_WITH_KNOTS ( 'NONE', 3,
 ( #1692, #59022, #40576, #30831, #16752, #15518 ),
 .UNSPECIFIED., .F., .F.,
 ( 4, 2, 4 ),
 ( 1.870830531855975817E-17, 0.0002293755540694300988, 0.0004587511081388414950 ),
 .UNSPECIFIED. ) ;
#19238 = AXIS2_PLACEMENT_3D ( 'NONE', #8515, #60514, #52052 ) ;
#19239 = CARTESIAN_POINT ( 'NONE',  ( 4.956653778116994147, 35.79382859084161339, -32.11725092155005967 ) ) ;
#19240 = ORIENTED_EDGE ( 'NONE', *, *, #25179, .F. ) ;
#19241 = CARTESIAN_POINT ( 'NONE',  ( 0.9762797500689124330, -34.83496347773922963, -23.29914386174477059 ) ) ;
#19242 = CARTESIAN_POINT ( 'NONE',  ( -6.057079549204054558, 11.99988366729700573, 15.06101002825099400 ) ) ;
#19243 = CARTESIAN_POINT ( 'NONE',  ( 0.6008122571543322854, -35.57793373092638234, -33.84915334100880102 ) ) ;
#19244 = VERTEX_POINT ( 'NONE', #51664 ) ;
#19245 = ORIENTED_EDGE ( 'NONE', *, *, #47676, .F. ) ;
#19246 = DIRECTION ( 'NONE',  ( -0.5000000000000055511, -0.8660254037844354880, 0.000000000000000000 ) ) ;
#19247 = CARTESIAN_POINT ( 'NONE',  ( 1.154321713695929175, -20.73950268329797453, -37.57248787340957108 ) ) ;
#19248 = CARTESIAN_POINT ( 'NONE',  ( 1.830465331921977912, -32.48963746129035002, 29.74557973064752403 ) ) ;
#19249 = CARTESIAN_POINT ( 'NONE',  ( 5.895596859100789899, -11.93344155749905866, 16.19015613903219730 ) ) ;
#19250 = DIRECTION ( 'NONE',  ( -1.000000000000000000, -0.000000000000000000, -0.000000000000000000 ) ) ;
#19251 = DIRECTION ( 'NONE',  ( 1.000000000000000000, 0.000000000000000000, 0.000000000000000000 ) ) ;
#19252 = CARTESIAN_POINT ( 'NONE',  ( 0.6016117650947689910, -42.61630575986080771, 24.40085116602604387 ) ) ;
#19253 = CARTESIAN_POINT ( 'NONE',  ( 0.5809828226811617480, 0.5448590168539207967, -47.89273459658652854 ) ) ;
#19254 = CARTESIAN_POINT ( 'NONE',  ( 4.553261556744873317, 1.633632119646958980, 43.89613664004264848 ) ) ;
#19255 = CARTESIAN_POINT ( 'NONE',  ( 5.896278296736517710, 19.00178995741540788, 6.592340861078921144 ) ) ;
#19256 = EDGE_CURVE ( 'NONE', #13969, #8619, #34722, .T. ) ;
#19257 = CARTESIAN_POINT ( 'NONE',  ( 0.9785694773339239649, 41.90806447728379425, 0.2225701743215739437 ) ) ;
#19258 = CARTESIAN_POINT ( 'NONE',  ( 3.783198216974391404, -22.99723434398817545, 36.37893817280279052 ) ) ;
#19259 = VERTEX_POINT ( 'NONE', #22562 ) ;
#19260 = EDGE_CURVE ( 'NONE', #61948, #28137, #51354, .T. ) ;
#19261 = CARTESIAN_POINT ( 'NONE',  ( 0.000000000000000000, 0.000000000000000000, 0.000000000000000000 ) ) ;
#19262 = CARTESIAN_POINT ( 'NONE',  ( 0.6027444965799114707, 41.08494361130553330, 26.89918073739952931 ) ) ;
#19263 = CARTESIAN_POINT ( 'NONE',  ( 0.1129192098497455998, -35.64954734424960492, 26.00118385641814456 ) ) ;
#19264 = CARTESIAN_POINT ( 'NONE',  ( 0.1365634738349410515, -27.00966719914814362, -34.89040695398243486 ) ) ;
#19265 = FACE_OUTER_BOUND ( 'NONE', #4833, .T. ) ;
#19266 = DIRECTION ( 'NONE',  ( -1.000000000000000000, -0.000000000000000000, -0.000000000000000000 ) ) ;
#19267 = ITEM_DEFINED_TRANSFORMATION ( 'NONE', 'NONE', #36936,  #14677 ) ;
#19268 = CARTESIAN_POINT ( 'NONE',  ( 2.643462169533600914, -48.01657676222236404, -1.382267876918291893 ) ) ;
#19269 = CARTESIAN_POINT ( 'NONE',  ( 0.5997462898726536595, 48.09935696025637952, -9.899671214446758682 ) ) ;
#19270 = CARTESIAN_POINT ( 'NONE',  ( 1.231276596079887931, -7.805643096901414779, -41.18675402191659174 ) ) ;
#19272 = VERTEX_POINT ( 'NONE', #18477 ) ;
#19271 = CARTESIAN_POINT ( 'NONE',  ( 0.9722240741986373225, -6.177112427866152444, 42.46141200043699371 ) ) ;
#19273 = ORIENTED_EDGE ( 'NONE', *, *, #59634, .F. ) ;
#19274 = EDGE_CURVE ( 'NONE', #9802, #12689, #18302, .T. ) ;
#19275 = CARTESIAN_POINT ( 'NONE',  ( 4.553261556744873317, 42.54662847375970358, 10.92355122382355148 ) ) ;
#19276 = CARTESIAN_POINT ( 'NONE',  ( 0.3676999524040366896, 14.45783756353458216, -41.67639039443420756 ) ) ;
#19277 = CARTESIAN_POINT ( 'NONE',  ( 4.303969348037246512, 32.45857549159302380, 35.51084504003208764 ) ) ;
#19278 = EDGE_CURVE ( 'NONE', #14506, #6786, #37603, .T. ) ;
#19279 = ORIENTED_EDGE ( 'NONE', *, *, #50439, .F. ) ;
#19280 = CARTESIAN_POINT ( 'NONE',  ( -6.077587904424778920, -18.89978312007036720, 3.687033958106935128 ) ) ;
#19281 = CARTESIAN_POINT ( 'NONE',  ( 0.2885697896453102151, -29.91358794843040769, -31.05173034173360591 ) ) ;
#19282 = CARTESIAN_POINT ( 'NONE',  ( 0.5827359174754811466, -41.29633904010498924, -24.26188383263413684 ) ) ;
#19283 = MECHANICAL_DESIGN_GEOMETRIC_PRESENTATION_REPRESENTATION (  '', ( #61275 ), #16269 ) ;
#19284 = AXIS2_PLACEMENT_3D ( 'NONE', #53323, #23602, #43664 ) ;
#19285 = ORIENTED_EDGE ( 'NONE', *, *, #40054, .T. ) ;
#19286 = ORIENTED_EDGE ( 'NONE', *, *, #28188, .T. ) ;
#19287 = LINE ( 'NONE', #28978, #47303 ) ;
#19288 = CARTESIAN_POINT ( 'NONE',  ( 0.5987334308729318488, -20.42989745030504523, -44.65626716083365011 ) ) ;
#19289 = CARTESIAN_POINT ( 'NONE',  ( 0.5837799406558208393, 46.89600465499675863, -0.09108773643912386475 ) ) ;
#19290 = CARTESIAN_POINT ( 'NONE',  ( 0.5998501479064708430, 41.92175333043619645, -23.59887241503310307 ) ) ;
#19291 = CARTESIAN_POINT ( 'NONE',  ( 3.661921753702001237, -12.12682059594439821, 45.44855713955956134 ) ) ;
#19292 = EDGE_CURVE ( 'NONE', #48331, #61199, #45170, .T. ) ;
#19293 = CARTESIAN_POINT ( 'NONE',  ( 0.1135584504625007374, 33.31662552165888513, 28.93016619352194851 ) ) ;
#19294 = ORIENTED_EDGE ( 'NONE', *, *, #32618, .T. ) ;
#19295 = CARTESIAN_POINT ( 'NONE',  ( 4.833616638992208614, -46.11947910922911831, 3.476827473557080772 ) ) ;
#19296 = CARTESIAN_POINT ( 'NONE',  ( 4.956445790444004018, -45.27177431812773278, -12.96165499572285817 ) ) ;
#19297 = ORIENTED_EDGE ( 'NONE', *, *, #48428, .F. ) ;
#19298 = CARTESIAN_POINT ( 'NONE',  ( 0.9730545539215883499, -37.40983423658458662, -21.01499094264588763 ) ) ;
#19299 = CARTESIAN_POINT ( 'NONE',  ( 4.962356264823602814, 6.570263404307167932, -41.57002810511882274 ) ) ;
#19300 = CARTESIAN_POINT ( 'NONE',  ( 0.7948884756798508811, -39.86121518214929438, 28.66674325420559200 ) ) ;
#19301 = CARTESIAN_POINT ( 'NONE',  ( 0.1158516988532803521, -40.91787788753845234, -16.51270504833438935 ) ) ;
#19302 = VERTEX_POINT ( 'NONE', #4340 ) ;
#19303 = ORIENTED_EDGE ( 'NONE', *, *, #44117, .T. ) ;
#19304 = CARTESIAN_POINT ( 'NONE',  ( 0.9730545539215883499, 0.5054011016612682816, 42.90536227157002003 ) ) ;
#19305 = CARTESIAN_POINT ( 'NONE',  ( 0.9972139404380291339, 10.46878911444733973, -41.61281131482451201 ) ) ;
#19306 = FACE_OUTER_BOUND ( 'NONE', #54320, .T. ) ;
#19307 = CYLINDRICAL_SURFACE ( 'NONE', #3420, 15.43999999999999240 ) ;
#19308 = ORIENTED_EDGE ( 'NONE', *, *, #5343, .T. ) ;
#19309 = CARTESIAN_POINT ( 'NONE',  ( 4.553261556744873317, -20.11719049292697648, 39.04917684785332455 ) ) ;
#19310 = ORIENTED_EDGE ( 'NONE', *, *, #27576, .T. ) ;
#19311 = CARTESIAN_POINT ( 'NONE',  ( 2.528190830796658517, 39.10452951792409237, -15.26728225110188930 ) ) ;
#19312 = CARTESIAN_POINT ( 'NONE',  ( 0.6024113833632039894, -25.64285567226712814, 41.88061391708750847 ) ) ;
#19313 = VERTEX_POINT ( 'NONE', #48517 ) ;
#19314 = CARTESIAN_POINT ( 'NONE',  ( 5.896782393890504181, -17.30187591025968530, 10.25529994022543079 ) ) ;
#19315 = FACE_OUTER_BOUND ( 'NONE', #44558, .T. ) ;
#19316 = CARTESIAN_POINT ( 'NONE',  ( 0.8557997880470606944, -19.17299735372040459, 43.90420959842174398 ) ) ;
#19317 = TOROIDAL_SURFACE ( 'NONE', #1267, 6.866799999999992465, 0.02570000000000187065 ) ;
#19318 = ORIENTED_EDGE ( 'NONE', *, *, #35408, .T. ) ;
#19319 = CARTESIAN_POINT ( 'NONE',  ( 0.5819845901640493535, -17.90867915372020391, -44.42187107932964096 ) ) ;
#19320 =( BOUNDED_SURFACE ( )  B_SPLINE_SURFACE ( 3, 1, ( 
 ( #40941, #11803 ),
 ( #2677, #59070 ),
 ( #49998, #54984 ),
 ( #20877, #30881 ) ),
 .UNSPECIFIED., .F., .F., .F. ) 
 B_SPLINE_SURFACE_WITH_KNOTS ( ( 4, 4 ),
 ( 2, 2 ),
 ( 0.000000000000000000, 1.000000000000000000 ),
 ( 0.000000000000000000, 1.000000000000000000 ),
 .UNSPECIFIED. ) 
 GEOMETRIC_REPRESENTATION_ITEM ( )  RATIONAL_B_SPLINE_SURFACE ( (
 ( 1.000000000000000000, 1.000000000000000000),
 ( 0.7269869731126817891, 0.9931720237060910339),
 ( 0.7269869731126817891, 0.9931720237060910339),
 ( 1.000000000000000000, 1.000000000000000000) ) ) 
 REPRESENTATION_ITEM ( '' )  SURFACE ( )  );
#19321 = CARTESIAN_POINT ( 'NONE',  ( 4.833616638992205949, 20.86133030530291421, -41.27831852777620725 ) ) ;
#19322 = CARTESIAN_POINT ( 'NONE',  ( -6.078726893082806448, -8.909671472910670076, -17.07078778245227824 ) ) ;
#19323 = FACE_OUTER_BOUND ( 'NONE', #5076, .T. ) ;
#19324 = CARTESIAN_POINT ( 'NONE',  ( 0.1100247026804066219, 16.65964013375385733, -39.77655614012837759 ) ) ;
#19325 = EDGE_LOOP ( 'NONE', ( #30826, #23279, #48626, #24888 ) ) ;
#19326 = EDGE_CURVE ( 'NONE', #11136, #7783, #24280, .T. ) ;
#19327 = FACE_OUTER_BOUND ( 'NONE', #12929, .T. ) ;
#19328 = CARTESIAN_POINT ( 'NONE',  ( 10.00000000000000533, 1.836909530733574959E-15, -1.925929944387237167E-31 ) ) ;
#19329 = VERTEX_POINT ( 'NONE', #14104 ) ;
#19330 = ADVANCED_FACE ( 'NONE', ( #5578 ), #38854, .F. ) ;
#19331 = CARTESIAN_POINT ( 'NONE',  ( 0.6845945791218034371, -24.50629722878996830, -39.99809891542528106 ) ) ;
#19332 = CARTESIAN_POINT ( 'NONE',  ( 4.553261556744873317, 38.38432632180467863, 21.35844232721216684 ) ) ;
#19333 = CARTESIAN_POINT ( 'NONE',  ( -6.016104459813371719, -7.215917642688938649, -17.40682403289256541 ) ) ;
#19334 = B_SPLINE_CURVE_WITH_KNOTS ( 'NONE', 3,
 ( #48071, #12805, #60998, #22490, #32208, #60681 ),
 .UNSPECIFIED., .F., .F.,
 ( 4, 2, 4 ),
 ( 0.000000000000000000, 0.0002291459268755696927, 0.0004582918537511393854 ),
 .UNSPECIFIED. ) ;
#19335 = AXIS2_PLACEMENT_3D ( 'NONE', #43574, #11276, #58238 ) ;
#19336 = CARTESIAN_POINT ( 'NONE',  ( -6.077587904424778920, 5.484810954822209261, 18.45840919970604688 ) ) ;
#19337 = CARTESIAN_POINT ( 'NONE',  ( 0.6845945791218034371, 33.22744374803217227, -33.11107824709581138 ) ) ;
#19338 = LINE ( 'NONE', #13719, #39507 ) ;
#19339 = EDGE_CURVE ( 'NONE', #13969, #31069, #30811, .T. ) ;
#19340 = DIRECTION ( 'NONE',  ( 1.000000000000000000, 0.000000000000000000, 0.000000000000000000 ) ) ;
#19341 = B_SPLINE_CURVE_WITH_KNOTS ( 'NONE', 3,
 ( #3436, #56376, #26965, #51060 ),
 .UNSPECIFIED., .F., .F.,
 ( 4, 4 ),
 ( 0.000000000000000000, 0.005004741218457183817 ),
 .UNSPECIFIED. ) ;
#19342 = CARTESIAN_POINT ( 'NONE',  ( 4.975610109902397937, 42.89797504594955058, -23.49921581872176191 ) ) ;
#19343 = CARTESIAN_POINT ( 'NONE',  ( 1.231276596079881047, -11.60895935156387537, -40.28037777618035875 ) ) ;
#19345 = VERTEX_POINT ( 'NONE', #23793 ) ;
#19344 = DIRECTION ( 'NONE',  ( -0.000000000000000000, -1.000000000000000000, -0.000000000000000000 ) ) ;
#19346 = ORIENTED_EDGE ( 'NONE', *, *, #29135, .T. ) ;
#19347 = CARTESIAN_POINT ( 'NONE',  ( 0.5809828226811617480, -24.41822904836953612, 41.20389530892298779 ) ) ;
#19348 = EDGE_CURVE ( 'NONE', #21932, #16132, #6260, .T. ) ;
#19349 = PRODUCT_DEFINITION_SHAPE ( 'NONE', 'NONE',  #61988 ) ;
#19350 = DIRECTION ( 'NONE',  ( 0.09722883295013595717, 0.9469132758617077039, -0.3064340092744340383 ) ) ;
#19351 = CARTESIAN_POINT ( 'NONE',  ( 0.9745511491811736926, 42.58443036172455720, -5.262846425219182223 ) ) ;
#19353 = CARTESIAN_POINT ( 'NONE',  ( 4.322998006666165516, -47.80838462754068274, 4.155494336617899798 ) ) ;
#19352 = B_SPLINE_CURVE_WITH_KNOTS ( 'NONE', 3,
 ( #38123, #9575, #38420, #37187 ),
 .UNSPECIFIED., .F., .F.,
 ( 4, 4 ),
 ( 2.343940034265377226E-17, 0.004564976165746189446 ),
 .UNSPECIFIED. ) ;
#19354 = B_SPLINE_CURVE_WITH_KNOTS ( 'NONE', 3,
 ( #5466, #21132, #54307, #6374, #11129, #6687 ),
 .UNSPECIFIED., .F., .F.,
 ( 4, 2, 4 ),
 ( 1.260375116100749216E-16, 0.0002450741128632348900, 0.0004901482257263436873 ),
 .UNSPECIFIED. ) ;
#19355 = VERTEX_POINT ( 'NONE', #33206 ) ;
#19356 = CARTESIAN_POINT ( 'NONE',  ( 4.553261556744875094, 0.000000000000000000, 0.000000000000000000 ) ) ;
#19357 = CARTESIAN_POINT ( 'NONE',  ( -19.25636039734503413, -7.824477911287009313, 1.668439766839475480 ) ) ;
#19358 = CARTESIAN_POINT ( 'NONE',  ( 4.335381028904216727, -3.692956800736317824, -48.84791620665349399 ) ) ;
#19359 = EDGE_LOOP ( 'NONE', ( #41075, #24376, #1598, #43121 ) ) ;
#19360 = B_SPLINE_CURVE_WITH_KNOTS ( 'NONE', 3,
 ( #15735, #20422, #38317, #58605 ),
 .UNSPECIFIED., .F., .F.,
 ( 4, 4 ),
 ( 8.673617379884035472E-19, 0.004048833967417083887 ),
 .UNSPECIFIED. ) ;
#19361 = CARTESIAN_POINT ( 'NONE',  ( 5.965394784446460541, -12.48356622107665714, -16.29267539192338887 ) ) ;
#19362 = CARTESIAN_POINT ( 'NONE',  ( 0.5834872094924180574, 47.51530820063773319, -6.026535573893641029 ) ) ;
#19363 = ORIENTED_EDGE ( 'NONE', *, *, #12836, .T. ) ;
#19364 = CARTESIAN_POINT ( 'NONE',  ( 0.7044674535453004927, 23.45856740197648449, 43.14508475200662474 ) ) ;
#19365 = ORIENTED_EDGE ( 'NONE', *, *, #21599, .F. ) ;
#19366 = CARTESIAN_POINT ( 'NONE',  ( 0.6001305935487422083, -44.64600790884068005, 17.92615948558462691 ) ) ;
#19367 = CARTESIAN_POINT ( 'NONE',  ( 0.000000000000000000, 0.000000000000000000, -5.599999999999999645 ) ) ;
#19368 = B_SPLINE_CURVE_WITH_KNOTS ( 'NONE', 3,
 ( #30318, #39138, #1489, #15932 ),
 .UNSPECIFIED., .F., .F.,
 ( 4, 4 ),
 ( 1.962615573354719267E-17, 0.005004741218457437087 ),
 .UNSPECIFIED. ) ;
#19369 = ORIENTED_EDGE ( 'NONE', *, *, #18393, .T. ) ;
#19370 = FACE_BOUND ( 'NONE', #25814, .T. ) ;
#19371 = CARTESIAN_POINT ( 'NONE',  ( 4.975801465491694664, -40.15204426031552032, 26.14269827151608894 ) ) ;
#19372 = CARTESIAN_POINT ( 'NONE',  ( 2.500000000000002220, 0.000000000000000000, -25.03750572909317285 ) ) ;
#19373 = CARTESIAN_POINT ( 'NONE',  ( 0.1129192098497455998, 39.96249028893973332, -18.70698152272436587 ) ) ;
#19374 = ADVANCED_FACE ( 'NONE', ( #57577 ), #27697, .F. ) ;
#19375 = VECTOR ( 'NONE', #13141, 1000.000000000000227 ) ;
#19376 = ORIENTED_EDGE ( 'NONE', *, *, #48974, .T. ) ;
#19377 = ADVANCED_FACE ( 'NONE', ( #34134 ), #15669, .F. ) ;
#19378 = CARTESIAN_POINT ( 'NONE',  ( 0.6028777368367060907, -7.751577361373165331, -48.49178154823474785 ) ) ;
#19379 = ORIENTED_EDGE ( 'NONE', *, *, #13420, .T. ) ;
#19380 = FACE_BOUND ( 'NONE', #53090, .T. ) ;
#19381 = ORIENTED_EDGE ( 'NONE', *, *, #14704, .T. ) ;
#19382 = EDGE_CURVE ( 'NONE', #9472, #14392, #11525, .T. ) ;
#19383 = ORIENTED_EDGE ( 'NONE', *, *, #58603, .T. ) ;
#19384 = CARTESIAN_POINT ( 'NONE',  ( 5.917102823773431552, 8.458006992051032569, -18.24696785151324008 ) ) ;
#19385 = CARTESIAN_POINT ( 'NONE',  ( 5.959547316686252039, -20.34955788964378698, 2.682663672454569159 ) ) ;
#19386 = CARTESIAN_POINT ( 'NONE',  ( 3.238018933889920792, -11.82813123897611796, 6.285125596295605632 ) ) ;
#19387 = FACE_OUTER_BOUND ( 'NONE', #29116, .T. ) ;
#19388 = ORIENTED_EDGE ( 'NONE', *, *, #8724, .F. ) ;
#19389 = CARTESIAN_POINT ( 'NONE',  ( 0.6067375320500703051, -46.07640252006471115, -13.08014790719075293 ) ) ;
#19390 = CARTESIAN_POINT ( 'NONE',  ( 43.00000000000000000, 5.682605120120046040E-15, -2.995852231480065614E-16 ) ) ;
#19391 = CARTESIAN_POINT ( 'NONE',  ( 0.2940133293163021966, -28.13058116957257582, 33.98398082391366870 ) ) ;
#19392 = VERTEX_POINT ( 'NONE', #37923 ) ;
#19393 = B_SPLINE_CURVE_WITH_KNOTS ( 'NONE', 3,
 ( #13396, #53120, #29320, #19951 ),
 .UNSPECIFIED., .F., .F.,
 ( 4, 4 ),
 ( 0.000000000000000000, 0.004446090762761387670 ),
 .UNSPECIFIED. ) ;
#19394 = ORIENTED_EDGE ( 'NONE', *, *, #18882, .F. ) ;
#19395 = PRESENTATION_STYLE_ASSIGNMENT (( #4956 ) ) ;
#19396 = CARTESIAN_POINT ( 'NONE',  ( -6.078726893082806448, -18.90156862012333860, 3.677600436084480062 ) ) ;
#19397 = DIRECTION ( 'NONE',  ( 0.000000000000000000, 0.000000000000000000, 1.000000000000000000 ) ) ;
#19398 = CARTESIAN_POINT ( 'NONE',  ( 2.648799415243696664, 43.56092747588109404, 22.51584021818029768 ) ) ;
#19399 = B_SPLINE_CURVE_WITH_KNOTS ( 'NONE', 3,
 ( #29112, #44481, #5284, #24412 ),
 .UNSPECIFIED., .F., .F.,
 ( 4, 4 ),
 ( 0.000000000000000000, 0.004444103432399267029 ),
 .UNSPECIFIED. ) ;
#19400 = CARTESIAN_POINT ( 'NONE',  ( -6.016761891674565099, -16.31696541414265766, -9.424569481870424426 ) ) ;
#19401 = EDGE_LOOP ( 'NONE', ( #24342, #48250 ) ) ;
#19402 = EDGE_CURVE ( 'NONE', #57645, #53012, #56979, .T. ) ;
#19403 =( BOUNDED_SURFACE ( )  B_SPLINE_SURFACE ( 3, 1, ( 
 ( #40575, #61102 ),
 ( #18522, #16751 ),
 ( #32316, #37647 ),
 ( #51710, #51392 ) ),
 .UNSPECIFIED., .F., .F., .F. ) 
 B_SPLINE_SURFACE_WITH_KNOTS ( ( 4, 4 ),
 ( 2, 2 ),
 ( 0.000000000000000000, 1.000000000000000000 ),
 ( 0.000000000000000000, 1.000000000000000000 ),
 .UNSPECIFIED. ) 
 GEOMETRIC_REPRESENTATION_ITEM ( )  RATIONAL_B_SPLINE_SURFACE ( (
 ( 1.000000000000000000, 1.000000000000000000),
 ( 0.9754377213608244057, 0.9999580625633939235),
 ( 0.9754377213608244057, 0.9999580625633939235),
 ( 1.000000000000000000, 1.000000000000000000) ) ) 
 REPRESENTATION_ITEM ( '' )  SURFACE ( )  );
#19404 = B_SPLINE_CURVE_WITH_KNOTS ( 'NONE', 3,
 ( #3584, #56831, #23339, #13959 ),
 .UNSPECIFIED., .F., .F.,
 ( 4, 4 ),
 ( 0.000000000000000000, 0.005004741218457404127 ),
 .UNSPECIFIED. ) ;
#19405 = VERTEX_POINT ( 'NONE', #14406 ) ;
#19406 = CARTESIAN_POINT ( 'NONE',  ( 4.549368137175248350, -42.14271863032827525, -8.166781970325585505 ) ) ;
#19407 = CARTESIAN_POINT ( 'NONE',  ( 0.9762797500689124330, -41.16654106227479559, 7.851158013551082782 ) ) ;
#19408 = CARTESIAN_POINT ( 'NONE',  ( -5.571549742892843327, -9.254395351074540699, 0.000000000000000000 ) ) ;
#19409 = AXIS2_PLACEMENT_3D ( 'NONE', #36142, #50823, #12952 ) ;
#19410 = CARTESIAN_POINT ( 'NONE',  ( 0.9736507210033075177, -21.84312502845817150, 36.93248879681202368 ) ) ;
#19411 = CARTESIAN_POINT ( 'NONE',  ( 0.5837800005270546988, 4.694056397113588019, -46.66048749405113227 ) ) ;
#19412 = EDGE_CURVE ( 'NONE', #8164, #694, #17514, .T. ) ;
#19413 = CARTESIAN_POINT ( 'NONE',  ( 4.956653778116971942, 35.79382859084115864, 32.11725092155054995 ) ) ;
#19414 = VERTEX_POINT ( 'NONE', #33514 ) ;
#19415 = CARTESIAN_POINT ( 'NONE',  ( 0.8753041380234471980, 48.93739466471249955, 4.033575498629939027 ) ) ;
#19416 = CARTESIAN_POINT ( 'NONE',  ( 2.648799415243696664, -24.22471848649487214, -42.63426412569674540 ) ) ;
#19417 = CARTESIAN_POINT ( 'NONE',  ( -6.078726893082806448, 3.069885851706565916, -19.00973019603939917 ) ) ;
#19418 = CARTESIAN_POINT ( 'NONE',  ( 3.680974057930775700, 22.36814223828908865, 42.44218549341218250 ) ) ;
#19419 = CARTESIAN_POINT ( 'NONE',  ( -2.569797478183783568, 9.259773107242914136, 11.33042594333551278 ) ) ;
#19420 = EDGE_CURVE ( 'NONE', #56419, #28932, #42735, .T. ) ;
#19421 = LINE ( 'NONE', #23804, #15116 ) ;
#19422 = PRESENTATION_LAYER_ASSIGNMENT (  '', '', ( #56416 ) ) ;
#19423 = CARTESIAN_POINT ( 'NONE',  ( 0.5807400328401574052, -47.41494605191439149, -6.791881299636076008 ) ) ;
#19424 = ORIENTED_EDGE ( 'NONE', *, *, #10617, .T. ) ;
#19425 = CARTESIAN_POINT ( 'NONE',  ( 1.231276596079881935, -39.31472542100197387, -14.54747868495734053 ) ) ;
#19426 = CARTESIAN_POINT ( 'NONE',  ( 0.1073791018717483448, 37.58707531572176919, 21.14095454447572564 ) ) ;
#19427 = CARTESIAN_POINT ( 'NONE',  ( 0.8753041380234524160, 33.66554281472423327, 35.74590263041275762 ) ) ;
#19428 = CARTESIAN_POINT ( 'NONE',  ( 0.9762797500689124330, 4.697980241569248427, -41.64437257103928403 ) ) ;
#19429 = CARTESIAN_POINT ( 'NONE',  ( 4.962356264823608143, 0.000000000000000000, 0.000000000000000000 ) ) ;
#19430 = ORIENTED_EDGE ( 'NONE', *, *, #18472, .F. ) ;
#19431 = DIRECTION ( 'NONE',  ( 0.09835009131224567436, 0.9632152266566422760, -0.2500873580884609981 ) ) ;
#19432 = CARTESIAN_POINT ( 'NONE',  ( 1.227938101723756947, 17.20315230597844192, 39.32113113558972373 ) ) ;
#19433 = B_SPLINE_CURVE_WITH_KNOTS ( 'NONE', 3,
 ( #9227, #47453, #3273, #4504 ),
 .UNSPECIFIED., .F., .F.,
 ( 4, 4 ),
 ( 1.250926888277100334E-16, 0.005004948556313948416 ),
 .UNSPECIFIED. ) ;
#19434 = CARTESIAN_POINT ( 'NONE',  ( 5.838029081930955932, -22.71741985886587045, 41.41236401256183086 ) ) ;
#19435 = ORIENTED_EDGE ( 'NONE', *, *, #286, .T. ) ;
#19436 = CARTESIAN_POINT ( 'NONE',  ( 4.000000000000000000, 0.000000000000000000, 0.000000000000000000 ) ) ;
#19437 = FACE_OUTER_BOUND ( 'NONE', #7833, .T. ) ;
#19438 = ORIENTED_EDGE ( 'NONE', *, *, #38573, .T. ) ;
#19439 = CARTESIAN_POINT ( 'NONE',  ( -6.077587904424778920, -6.656176160390709917, 18.06907137391894125 ) ) ;
#19440 = VERTEX_POINT ( 'NONE', #54742 ) ;
#19441 = ORIENTED_EDGE ( 'NONE', *, *, #10565, .T. ) ;
#19442 = CARTESIAN_POINT ( 'NONE',  ( 4.967162193818130511, 38.83676580803792433, -18.65818244221215849 ) ) ;
#19443 = CARTESIAN_POINT ( 'NONE',  ( 0.6000166863083090663, -14.47337940799722134, 46.92914627628139357 ) ) ;
#19444 = ADVANCED_FACE ( 'NONE', ( #25951 ), #28450, .F. ) ;
#19445 = VERTEX_POINT ( 'NONE', #15639 ) ;
#19446 = CARTESIAN_POINT ( 'NONE',  ( 4.967162193818131399, -19.45289607368795259, -38.44485641567092671 ) ) ;
#19447 = AXIS2_PLACEMENT_3D ( 'NONE', #47162, #23042, #50595 ) ;
#19448 = VERTEX_POINT ( 'NONE', #34744 ) ;
#19449 = EDGE_CURVE ( 'NONE', #3592, #34476, #16740, .T. ) ;
#19450 = CARTESIAN_POINT ( 'NONE',  ( -2.601141883200665639, 9.698805021789150160, 11.34586306187000382 ) ) ;
#19451 = CARTESIAN_POINT ( 'NONE',  ( 0.8557997880470697982, -47.37054680076710866, 7.156447707085535903 ) ) ;
#19452 = VECTOR ( 'NONE', #40903, 1000.000000000000114 ) ;
#19453 = ADVANCED_FACE ( 'NONE', ( #29713 ), #26435, .F. ) ;
#19454 = ORIENTED_EDGE ( 'NONE', *, *, #15753, .F. ) ;
#19455 = EDGE_CURVE ( 'NONE', #5939, #33472, #2516, .T. ) ;
#19456 = CARTESIAN_POINT ( 'NONE',  ( 0.5997462898726536595, -1.051648045107538954, 49.09628974305014992 ) ) ;
#19457 = CARTESIAN_POINT ( 'NONE',  ( 1.088908134280558881, 36.76788378223859155, -22.12904883058516603 ) ) ;
#19458 = CARTESIAN_POINT ( 'NONE',  ( 0.5835226383429290564, 17.02466281517259716, 43.69671990636877013 ) ) ;
#19460 = ADVANCED_FACE ( 'NONE', ( #30634 ), #56437, .F. ) ;
#19459 = ORIENTED_EDGE ( 'NONE', *, *, #22530, .T. ) ;
#19461 = CARTESIAN_POINT ( 'NONE',  ( 0.5832366564991509073, 44.35361744978938958, 18.07697797533105089 ) ) ;
#19462 = CARTESIAN_POINT ( 'NONE',  ( 5.880360259849739535, -43.00389496650629440, 21.25991003419878211 ) ) ;
#19463 = AXIS2_PLACEMENT_3D ( 'NONE', #58865, #10976, #50401 ) ;
#19464 = ORIENTED_EDGE ( 'NONE', *, *, #5152, .F. ) ;
#19465 = CARTESIAN_POINT ( 'NONE',  ( 5.981074661064941900, -16.27808421740034817, 12.50143471347253765 ) ) ;
#19466 = B_SPLINE_CURVE_WITH_KNOTS ( 'NONE', 3,
 ( #28520, #4380, #61705, #18844 ),
 .UNSPECIFIED., .F., .F.,
 ( 4, 4 ),
 ( 4.670885906470169154E-18, 0.004050076154993004218 ),
 .UNSPECIFIED. ) ;
#19467 = B_SPLINE_CURVE_WITH_KNOTS ( 'NONE', 3,
 ( #20066, #44813, #1850, #20364, #45119, #39809 ),
 .UNSPECIFIED., .F., .F.,
 ( 4, 2, 4 ),
 ( 3.471140604459641645E-18, 0.0002291459268755725658, 0.0004582918537511416622 ),
 .UNSPECIFIED. ) ;
#19468 = ORIENTED_EDGE ( 'NONE', *, *, #38884, .F. ) ;
#19469 = CARTESIAN_POINT ( 'NONE',  ( 4.956445790443998689, -22.15545010017797622, 41.55326799420426198 ) ) ;
#19470 = ADVANCED_FACE ( 'NONE', ( #35683 ), #3199, .F. ) ;
#19471 = CARTESIAN_POINT ( 'NONE',  ( 0.1145239942831223490, 24.97564404501438062, 36.37530323229500340 ) ) ;
#19472 = ORIENTED_EDGE ( 'NONE', *, *, #53770, .T. ) ;
#19473 = CARTESIAN_POINT ( 'NONE',  ( 0.8560838555295158248, 27.08392101972004440, 38.29926965725714894 ) ) ;
#19474 = CARTESIAN_POINT ( 'NONE',  ( 3.782625744892851749, 37.01847680236511451, 19.92160835193178414 ) ) ;
#19475 = CARTESIAN_POINT ( 'NONE',  ( 0.5998501479064699549, 38.48283596221989455, 28.86886762351138103 ) ) ;
#19476 = CARTESIAN_POINT ( 'NONE',  ( 0.9789889208857696090, -22.63130747653287855, -35.27263556845443304 ) ) ;
#19477 = EDGE_CURVE ( 'NONE', #42440, #61394, #6495, .T. ) ;
#19478 = ORIENTED_EDGE ( 'NONE', *, *, #15802, .F. ) ;
#19479 = CARTESIAN_POINT ( 'NONE',  ( 0.6017667736363750963, 18.73201910948661819, -44.31084570541182188 ) ) ;
#19480 = LINE ( 'NONE', #38596, #42825 ) ;
#19481 = CARTESIAN_POINT ( 'NONE',  ( 5.895881250540457863, 10.81854556178491222, -16.95543433639743114 ) ) ;
#19482 = B_SPLINE_CURVE_WITH_KNOTS ( 'NONE', 3,
 ( #19906, #14895, #39019, #20500 ),
 .UNSPECIFIED., .F., .F.,
 ( 4, 4 ),
 ( 8.673617379884035472E-19, 0.004042984057420975427 ),
 .UNSPECIFIED. ) ;
#19483 = CARTESIAN_POINT ( 'NONE',  ( 4.956653778116990594, 2.599733001515011743, -48.02038484091096393 ) ) ;
#19484 = CARTESIAN_POINT ( 'NONE',  ( 4.975801465491695552, 20.67815041659141784, -43.22084481528199973 ) ) ;
#19485 = AXIS2_PLACEMENT_3D ( 'NONE', #4202, #13964, #6346 ) ;
#19486 = CARTESIAN_POINT ( 'NONE',  ( 4.956445790443994248, 24.88142650099509723, 39.98065363916922621 ) ) ;
#19487 = FACE_OUTER_BOUND ( 'NONE', #29462, .T. ) ;
#19488 = CARTESIAN_POINT ( 'NONE',  ( -17.29438283698436862, -7.748258867160539687, 1.991845353126138862 ) ) ;
#19489 = FACE_OUTER_BOUND ( 'NONE', #21134, .T. ) ;
#19490 = CARTESIAN_POINT ( 'NONE',  ( 0.1129192098497455998, 33.91039995638899995, -28.23183597612607798 ) ) ;
#19491 = EDGE_CURVE ( 'NONE', #51084, #52796, #20334, .T. ) ;
#19492 = CARTESIAN_POINT ( 'NONE',  ( 0.7764146366350277439, 33.24270218630520191, 33.09022854290649462 ) ) ;
#19493 = CARTESIAN_POINT ( 'NONE',  ( 0.1140933569871965536, 39.58854792274839696, 19.48581082357515015 ) ) ;
#19494 = CARTESIAN_POINT ( 'NONE',  ( 4.960386119450149955, 1.932332837766998379, -43.71158375621306647 ) ) ;
#19495 = CARTESIAN_POINT ( 'NONE',  ( 0.5839880159502333079, -23.90868446765450628, -41.50181427378129229 ) ) ;
#19496 =( BOUNDED_SURFACE ( )  B_SPLINE_SURFACE ( 3, 1, ( 
 ( #37839, #56890 ),
 ( #61887, #51891 ),
 ( #42834, #33121 ),
 ( #14321, #38441 ) ),
 .UNSPECIFIED., .F., .F., .F. ) 
 B_SPLINE_SURFACE_WITH_KNOTS ( ( 4, 4 ),
 ( 2, 2 ),
 ( 0.000000000000000000, 1.000000000000000000 ),
 ( 0.000000000000000000, 1.000000000000000000 ),
 .UNSPECIFIED. ) 
 GEOMETRIC_REPRESENTATION_ITEM ( )  RATIONAL_B_SPLINE_SURFACE ( (
 ( 1.000000000000000000, 1.000000000000000000),
 ( 0.7282232189291694135, 0.9929344683865672927),
 ( 0.7282232189291694135, 0.9929344683865672927),
 ( 1.000000000000000000, 1.000000000000000000) ) ) 
 REPRESENTATION_ITEM ( '' )  SURFACE ( )  );
#19497 = EDGE_CURVE ( 'NONE', #23542, #6995, #28718, .T. ) ;
#19498 = AXIS2_PLACEMENT_3D ( 'NONE', #27785, #33738, #28707 ) ;
#19499 = CARTESIAN_POINT ( 'NONE',  ( -4.473699999999999122, 5.863696293535578419E-15, 47.67072199303260049 ) ) ;
#19500 = CARTESIAN_POINT ( 'NONE',  ( 3.376099380956838925, 13.04318434631702139, -3.095759315589272642 ) ) ;
#19501 = VERTEX_POINT ( 'NONE', #22483 ) ;
#19502 = CARTESIAN_POINT ( 'NONE',  ( 0.5819845079324666992, 28.79567599618816232, -38.27312975753780933 ) ) ;
#19503 = AXIS2_PLACEMENT_3D ( 'NONE', #40323, #25571, #21185 ) ;
#19504 = CARTESIAN_POINT ( 'NONE',  ( 1.112077966505211846, 19.45195591732835538, -39.55567893639127419 ) ) ;
#19505 = DIRECTION ( 'NONE',  ( 0.07836865515943411409, 0.9893941468723566057, -0.1223011693452815268 ) ) ;
#19506 = ORIENTED_EDGE ( 'NONE', *, *, #53686, .T. ) ;
#19507 = CARTESIAN_POINT ( 'NONE',  ( 0.9736507210033050752, 5.153758453069551493, 42.59776535855981194 ) ) ;
#19508 = AXIS2_PLACEMENT_3D ( 'NONE', #36813, #22077, #12083 ) ;
#19509 = CARTESIAN_POINT ( 'NONE',  ( 3.559346040607745287, 26.81358697290394488, 34.84912961880832682 ) ) ;
#19510 =( BOUNDED_SURFACE ( )  B_SPLINE_SURFACE ( 3, 1, ( 
 ( #61043, #24302 ),
 ( #39048, #56340 ),
 ( #43437, #58104 ),
 ( #57795, #477 ) ),
 .UNSPECIFIED., .F., .F., .F. ) 
 B_SPLINE_SURFACE_WITH_KNOTS ( ( 4, 4 ),
 ( 2, 2 ),
 ( 0.000000000000000000, 1.000000000000000000 ),
 ( 0.000000000000000000, 1.000000000000000000 ),
 .UNSPECIFIED. ) 
 GEOMETRIC_REPRESENTATION_ITEM ( )  RATIONAL_B_SPLINE_SURFACE ( (
 ( 1.000000000000000000, 1.000000000000000000),
 ( 0.9952954269826590483, 0.8620686068821339365),
 ( 0.9952954269826590483, 0.8620686068821339365),
 ( 1.000000000000000000, 1.000000000000000000) ) ) 
 REPRESENTATION_ITEM ( '' )  SURFACE ( )  );
#19511 = ORIENTED_EDGE ( 'NONE', *, *, #28160, .F. ) ;
#19512 = VERTEX_POINT ( 'NONE', #8677 ) ;
#19513 = CARTESIAN_POINT ( 'NONE',  ( 0.9749527285493309048, -10.82939760924474193, -41.51939261707894957 ) ) ;
#19514 = ORIENTED_EDGE ( 'NONE', *, *, #22477, .T. ) ;
#19515 = CARTESIAN_POINT ( 'NONE',  ( 5.960221823109900008, -12.49951306783078131, -16.28072933292543922 ) ) ;
#19516 = ORIENTED_EDGE ( 'NONE', *, *, #46483, .T. ) ;
#19517 = VERTEX_POINT ( 'NONE', #3661 ) ;
#19518 = DIRECTION ( 'NONE',  ( 0.07500201931887538753, -0.4910262002617780674, 0.8679101150203120119 ) ) ;
#19519 = EDGE_CURVE ( 'NONE', #59488, #34766, #35992, .T. ) ;
#19520 = ORIENTED_EDGE ( 'NONE', *, *, #34303, .T. ) ;
#19521 = CARTESIAN_POINT ( 'NONE',  ( 3.783198216974390959, 31.62918462580879719, -29.18723368117329997 ) ) ;
#19522 = LINE ( 'NONE', #5383, #33106 ) ;
#19523 = FACE_OUTER_BOUND ( 'NONE', #27402, .T. ) ;
#19524 = ORIENTED_EDGE ( 'NONE', *, *, #48923, .F. ) ;
#19525 = ADVANCED_FACE ( 'NONE', ( #22791 ), #24802, .F. ) ;
#19526 = CARTESIAN_POINT ( 'NONE',  ( 0.3676999524040366896, -7.853951980431815194, -43.40813312746713848 ) ) ;
#19527 = AXIS2_PLACEMENT_3D ( 'NONE', #4909, #28118, #59076 ) ;
#19528 = CARTESIAN_POINT ( 'NONE',  ( 0.6028618097248863439, -48.10721794025128162, 0.1745704727164173742 ) ) ;
#19529 = VERTEX_POINT ( 'NONE', #3969 ) ;
#19530 = VERTEX_POINT ( 'NONE', #8365 ) ;
#19531 = EDGE_CURVE ( 'NONE', #9388, #18069, #3054, .T. ) ;
#19532 = CARTESIAN_POINT ( 'NONE',  ( 0.6039202388192953519, 41.25132197622554742, 26.64380130654712175 ) ) ;
#19533 = ORIENTED_EDGE ( 'NONE', *, *, #6397, .F. ) ;
#19534 = CARTESIAN_POINT ( 'NONE',  ( 0.8760168074886960365, -44.77533136581894269, 17.58183840866320935 ) ) ;
#19535 = CARTESIAN_POINT ( 'NONE',  ( -6.078075953587585900, -14.66587681219991524, -12.47827037599814481 ) ) ;
#19536 = DIRECTION ( 'NONE',  ( 0.000000000000000000, 0.000000000000000000, 1.000000000000000000 ) ) ;
#19537 = ADVANCED_FACE ( 'NONE', ( #12180 ), #24428, .F. ) ;
#19538 = CARTESIAN_POINT ( 'NONE',  ( 0.1102144999581332746, 5.503895401229410567, 42.77179372778545030 ) ) ;
#19539 = B_SPLINE_CURVE_WITH_KNOTS ( 'NONE', 3,
 ( #8040, #2712, #21840, #60041, #12770, #17149 ),
 .UNSPECIFIED., .F., .F.,
 ( 4, 2, 4 ),
 ( 8.554130121340520410E-17, 0.0002293366620881447950, 0.0004586733241762040465 ),
 .UNSPECIFIED. ) ;
#19540 = ORIENTED_EDGE ( 'NONE', *, *, #48237, .F. ) ;
#19541 = DIRECTION ( 'NONE',  ( 1.000000000000000000, 0.000000000000000000, 0.000000000000000000 ) ) ;
#19542 = CARTESIAN_POINT ( 'NONE',  ( 4.553261556744875094, 0.000000000000000000, 0.000000000000000000 ) ) ;
#19543 = CARTESIAN_POINT ( 'NONE',  ( 5.917102823773431552, 10.82912387347610128, 16.94756012482775986 ) ) ;
#19544 = FACE_OUTER_BOUND ( 'NONE', #29650, .T. ) ;
#19545 = CIRCLE ( 'NONE', #47577, 6.728125000000023448 ) ;
#19546 = VERTEX_POINT ( 'NONE', #46308 ) ;
#19547 = CARTESIAN_POINT ( 'NONE',  ( 5.901463166500146684, -19.93509711719964272, -2.666415809369400591 ) ) ;
#19548 = CARTESIAN_POINT ( 'NONE',  ( 4.975801465491695552, 39.51822597168496287, -27.09127437476339395 ) ) ;
#19549 = CARTESIAN_POINT ( 'NONE',  ( 0.9762797500689124330, -11.93232144563776487, -40.17392798947692256 ) ) ;
#19550 = DIRECTION ( 'NONE',  ( 0.000000000000000000, 0.000000000000000000, 1.000000000000000000 ) ) ;
#19552 = ORIENTED_EDGE ( 'NONE', *, *, #22881, .T. ) ;
#19551 = VECTOR ( 'NONE', #57769, 1000.000000000000114 ) ;
#19553 = VERTEX_POINT ( 'NONE', #45692 ) ;
#19554 = DIRECTION ( 'NONE',  ( 0.000000000000000000, 0.000000000000000000, 1.000000000000000000 ) ) ;
#19555 = CARTESIAN_POINT ( 'NONE',  ( 4.694002226626921015, 36.32786722402781265, 27.54216466437490496 ) ) ;
#19556 = AXIS2_PLACEMENT_3D ( 'NONE', #50500, #7572, #27624 ) ;
#19557 = CARTESIAN_POINT ( 'NONE',  ( 5.895596859100789899, 18.99884588797230478, 6.600911917119146821 ) ) ;
#19558 = CARTESIAN_POINT ( 'NONE',  ( 4.553261556744875094, 12.28162544311214432, 42.17465165592641796 ) ) ;
#19559 = PRESENTATION_STYLE_ASSIGNMENT (( #23025 ) ) ;
#19560 = CARTESIAN_POINT ( 'NONE',  ( 0.1064266379913940130, -17.02047542254822687, -39.62374453032489896 ) ) ;
#19561 = CARTESIAN_POINT ( 'NONE',  ( 2.301430502907647391, 28.20897229937352435, 38.87758534782515341 ) ) ;
#19562 = CARTESIAN_POINT ( 'NONE',  ( 5.894904586330512508, 12.98452142685960631, 15.36006560458211467 ) ) ;
#19563 = CARTESIAN_POINT ( 'NONE',  ( 0.5998501479064708430, -47.76154736470761719, 5.759754759339972274 ) ) ;
#19564 = FACE_OUTER_BOUND ( 'NONE', #6275, .T. ) ;
#19565 = VERTEX_POINT ( 'NONE', #2741 ) ;
#19566 = CARTESIAN_POINT ( 'NONE',  ( 5.959828726073459926, -10.26672511661768006, 17.77343634131824146 ) ) ;
#19567 = CARTESIAN_POINT ( 'NONE',  ( 0.1102847568649952675, -34.26895182984680588, -26.17930421801138863 ) ) ;
#19568 = CARTESIAN_POINT ( 'NONE',  ( -6.057079549204054558, 16.77479338118040886, 9.457142175014846330 ) ) ;
#19569 = CARTESIAN_POINT ( 'NONE',  ( 0.6001305935487315502, -0.5236757026892772116, 48.10757715638247589 ) ) ;
#19570 = CARTESIAN_POINT ( 'NONE',  ( 5.960721111146673579, 20.34914600876571456, 2.685391721746106963 ) ) ;
#19571 = CARTESIAN_POINT ( 'NONE',  ( 0.6030672727741701600, -46.49075153683480721, 12.36682345648100423 ) ) ;
#19572 = CARTESIAN_POINT ( 'NONE',  ( 0.8560838555295158248, 45.47430759461114747, -11.50913475776619599 ) ) ;
#19573 = CONTEXT_DEPENDENT_SHAPE_REPRESENTATION ( #41216, #41319 ) ;
#19574 = CARTESIAN_POINT ( 'NONE',  ( 0.9757892942422831117, -26.08029006934560101, 34.07281211842312985 ) ) ;
#19575 = CARTESIAN_POINT ( 'NONE',  ( 0.6021447746440204973, 22.48211463121051068, -43.65885546825062846 ) ) ;
#19576 = EDGE_CURVE ( 'NONE', #23785, #10647, #49683, .T. ) ;
#19577 = CARTESIAN_POINT ( 'NONE',  ( 3.660087539127334200, 32.61167949558434742, -35.27260502801098596 ) ) ;
#19578 = CARTESIAN_POINT ( 'NONE',  ( 4.834790513006555379, -39.84947630189435586, -25.38914294317831022 ) ) ;
#19579 = DIRECTION ( 'NONE',  ( -1.000000000000000000, -0.000000000000000000, -0.000000000000000000 ) ) ;
#19581 = VERTEX_POINT ( 'NONE', #17791 ) ;
#19580 = DIRECTION ( 'NONE',  ( -1.000000000000000000, -0.000000000000000000, -0.000000000000000000 ) ) ;
#19582 = ORIENTED_EDGE ( 'NONE', *, *, #50750, .F. ) ;
#19583 = CARTESIAN_POINT ( 'NONE',  ( 4.956653778116966613, 0.000000000000000000, 0.000000000000000000 ) ) ;
#19584 = FACE_OUTER_BOUND ( 'NONE', #7168, .T. ) ;
#19585 = CYLINDRICAL_SURFACE ( 'NONE', #21802, 9.500000000000005329 ) ;
#19586 = EDGE_LOOP ( 'NONE', ( #3939, #2556, #37213, #15391 ) ) ;
#19587 = FACE_OUTER_BOUND ( 'NONE', #49492, .T. ) ;
#19588 = CARTESIAN_POINT ( 'NONE',  ( 0.7762783648524398394, 37.45705264446620220, -29.86325223096974923 ) ) ;
#19589 = B_SPLINE_CURVE_WITH_KNOTS ( 'NONE', 3,
 ( #34813, #21319, #10687, #20395, #16307, #11618 ),
 .UNSPECIFIED., .F., .F.,
 ( 4, 2, 4 ),
 ( 1.426045310262811165E-18, 0.0002450742804987333088, 0.0004901485609974652081 ),
 .UNSPECIFIED. ) ;
#19590 = B_SPLINE_CURVE_WITH_KNOTS ( 'NONE', 3,
 ( #53386, #39324, #13747, #27824, #58385, #34615 ),
 .UNSPECIFIED., .F., .F.,
 ( 4, 2, 4 ),
 ( 0.000000000000000000, 0.0002450742804987331462, 0.0004901485609974662924 ),
 .UNSPECIFIED. ) ;
#19591 = ORIENTED_EDGE ( 'NONE', *, *, #37617, .T. ) ;
#19592 = ORIENTED_EDGE ( 'NONE', *, *, #4294, .T. ) ;
#19593 = VECTOR ( 'NONE', #43042, 1000.000000000000114 ) ;
#19594 = CARTESIAN_POINT ( 'NONE',  ( 0.1073791018717578927, 30.14884492832347718, 30.83464511437148659 ) ) ;
#19595 = CARTESIAN_POINT ( 'NONE',  ( 4.963659409799331179, -43.98510776953404644, -8.262218268420943090 ) ) ;
#19596 = CARTESIAN_POINT ( 'NONE',  ( 4.553261556744875094, -39.67390170502071811, 18.85526688551479424 ) ) ;
#19597 = VECTOR ( 'NONE', #43191, 1000.000000000000114 ) ;
#19598 = CARTESIAN_POINT ( 'NONE',  ( 3.407937589446178528, 10.00592723328961142, 9.356405769959087237 ) ) ;
#19600 = CARTESIAN_POINT ( 'NONE',  ( 0.7954190325252783467, -17.60078418395023547, 44.76287681188600942 ) ) ;
#19599 = CIRCLE ( 'NONE', #564, 43.08621763946400307 ) ;
#19601 = ADVANCED_FACE ( 'NONE', ( #21873 ), #7213, .F. ) ;
#19602 = CARTESIAN_POINT ( 'NONE',  ( 0.5809828226811617480, 38.32755012159184815, -28.72298383114449294 ) ) ;
#19603 = ADVANCED_FACE ( 'NONE', ( #8072 ), #60826, .F. ) ;
#19604 = VERTEX_POINT ( 'NONE', #51281 ) ;
#19605 = VERTEX_POINT ( 'NONE', #56601 ) ;
#19606 = CARTESIAN_POINT ( 'NONE',  ( 0.7762783648524405056, -11.53708172997851911, 46.49451980369975246 ) ) ;
#19607 = CARTESIAN_POINT ( 'NONE',  ( 1.088313998177382613, 42.43756598879024722, 6.373602917100332554 ) ) ;
#19608 = ORIENTED_EDGE ( 'NONE', *, *, #61071, .T. ) ;
#19609 = CARTESIAN_POINT ( 'NONE',  ( 0.1152809850208375703, 41.94550343259623304, -13.69379510127901867 ) ) ;
#19610 = CARTESIAN_POINT ( 'NONE',  ( 0.2230388203127617042, 37.71673103297339935, 20.89822698305281534 ) ) ;
#19611 = EDGE_CURVE ( 'NONE', #10729, #33488, #48143, .T. ) ;
#19612 = CARTESIAN_POINT ( 'NONE',  ( 0.6253024248130470975, -39.76151138891634673, 28.81781462024348173 ) ) ;
#19613 = CARTESIAN_POINT ( 'NONE',  ( 5.896278296736517710, 3.339955767731461300, 19.83359965018909676 ) ) ;
#19614 = ORIENTED_EDGE ( 'NONE', *, *, #5838, .T. ) ;
#19615 = ORIENTED_EDGE ( 'NONE', *, *, #29709, .T. ) ;
#19616 = CARTESIAN_POINT ( 'NONE',  ( 5.200000000000002842, 0.000000000000000000, 0.000000000000000000 ) ) ;
#19617 = CARTESIAN_POINT ( 'NONE',  ( 5.896278296736517710, 0.6665948613555030544, -20.10180665774094422 ) ) ;
#19618 = CARTESIAN_POINT ( 'NONE',  ( 4.960386119450153508, -15.28553149072512340, -40.99742664751524046 ) ) ;
#19619 = SHAPE_REPRESENTATION ( 'socket head cap screw_iso_ISO 4762 M5 x 16 - 16N', ( #14677 ), #38903 ) ;
#19620 = FACE_OUTER_BOUND ( 'NONE', #57860, .T. ) ;
#19621 = ORIENTED_EDGE ( 'NONE', *, *, #11262, .F. ) ;
#19622 = CARTESIAN_POINT ( 'NONE',  ( 4.975610109902397937, 2.142807115709095100, 48.86571174967821918 ) ) ;
#19623 = VERTEX_POINT ( 'NONE', #42847 ) ;
#19624 = CARTESIAN_POINT ( 'NONE',  ( 0.6254087463353913412, 48.10157520235527073, -0.6881259009462784570 ) ) ;
#19625 = CARTESIAN_POINT ( 'NONE',  ( 4.553261556744873317, 40.80044851610476542, 16.27461110774448372 ) ) ;
#19626 = ADVANCED_FACE ( 'NONE', ( #32827 ), #33440, .F. ) ;
#19627 = VERTEX_POINT ( 'NONE', #51906 ) ;
#19628 = DIRECTION ( 'NONE',  ( 0.07439287786467667363, 0.7144194931003065019, -0.6957517427943048505 ) ) ;
#19629 = CARTESIAN_POINT ( 'NONE',  ( 0.6025881611877911270, -47.72390913208169394, 6.062907795288557722 ) ) ;
#19630 = ADVANCED_FACE ( 'NONE', ( #189 ), #37264, .F. ) ;
#19631 = DIRECTION ( 'NONE',  ( 0.000000000000000000, 0.000000000000000000, 1.000000000000000000 ) ) ;
#19632 = ORIENTED_EDGE ( 'NONE', *, *, #36032, .T. ) ;
#19633 = FACE_OUTER_BOUND ( 'NONE', #5849, .T. ) ;
#19634 = DIRECTION ( 'NONE',  ( 0.000000000000000000, 0.000000000000000000, 1.000000000000000000 ) ) ;
#19635 = CARTESIAN_POINT ( 'NONE',  ( 0.2224561200757608492, 10.42482236669245665, 41.84032767736803748 ) ) ;
#19636 = CARTESIAN_POINT ( 'NONE',  ( 4.000000000000003553, -0.3902508023145564442, -1.995609623731131599E-15 ) ) ;
#19637 = CARTESIAN_POINT ( 'NONE',  ( 0.5806925824938499181, 40.62497527030964051, -23.42720099863178973 ) ) ;
#19638 = EDGE_LOOP ( 'NONE', ( #17131, #44444, #9100 ) ) ;
#19639 = CARTESIAN_POINT ( 'NONE',  ( 0.5839879327111919816, -23.86931774877327683, 41.52454255611500855 ) ) ;
#19640 = CARTESIAN_POINT ( 'NONE',  ( 1.231276596079881047, -39.86997064245551314, 12.94844438485960580 ) ) ;
#19641 = CARTESIAN_POINT ( 'NONE',  ( 0.5804410086790514622, 37.14246315962257938, -28.63489623329332545 ) ) ;
#19642 = VERTEX_POINT ( 'NONE', #43154 ) ;
#19643 = CIRCLE ( 'NONE', #54608, 48.09070567114147110 ) ;
#19644 = CARTESIAN_POINT ( 'NONE',  ( 0.5782707292762442330, -24.62356639979741502, -39.91761931105593675 ) ) ;
#19645 = CARTESIAN_POINT ( 'NONE',  ( 0.5834872094924189456, 0.2270145249679870747, -47.89542889285417004 ) ) ;
#19646 = CARTESIAN_POINT ( 'NONE',  ( 0.9730545539215883499, -26.52009130076794108, 33.73144377768549163 ) ) ;
#19647 = CARTESIAN_POINT ( 'NONE',  ( 0.5782707292762442330, -45.81184706829294129, -10.05042396612988931 ) ) ;
#19648 = CARTESIAN_POINT ( 'NONE',  ( 1.227938101723756947, 36.73927144310543014, -22.18841447410681411 ) ) ;
#19649 = CARTESIAN_POINT ( 'NONE',  ( 4.975610109902397937, -48.77192499014908833, -3.707929326867496655 ) ) ;
#19650 = SURFACE_SIDE_STYLE ('',( #9304 ) ) ;
#19651 = ADVANCED_FACE ( 'NONE', ( #23408 ), #34874, .F. ) ;
#19652 = CARTESIAN_POINT ( 'NONE',  ( 0.9784957157296367836, -6.740996248989422845, 41.36293058480602269 ) ) ;
#19653 = CIRCLE ( 'NONE', #52621, 0.02570000000000870199 ) ;
#19654 = CARTESIAN_POINT ( 'NONE',  ( 1.091591847532196624, -11.67058309673969774, -40.25613594395188244 ) ) ;
#19656 = ORIENTED_EDGE ( 'NONE', *, *, #22929, .T. ) ;
#19655 = CARTESIAN_POINT ( 'NONE',  ( 0.8760168074886960365, 19.22870327415304104, -44.09317760313732748 ) ) ;
#19657 = ORIENTED_EDGE ( 'NONE', *, *, #20252, .F. ) ;
#19658 = CARTESIAN_POINT ( 'NONE',  ( -6.078457390727109555, 18.62514245781370548, -4.888617336594570872 ) ) ;
#19659 = FACE_OUTER_BOUND ( 'NONE', #14917, .T. ) ;
#19660 = CARTESIAN_POINT ( 'NONE',  ( 47.85000000000000853, 15.50000000000000711, 1.598617397282144235E-15 ) ) ;
#19661 = CARTESIAN_POINT ( 'NONE',  ( 0.1156867017252034835, -22.98040861868942386, 37.66754076115470440 ) ) ;
#19662 = CARTESIAN_POINT ( 'NONE',  ( 0.9758171775293909000, 42.54062484958064516, -5.606549717953765111 ) ) ;
#19663 = CARTESIAN_POINT ( 'NONE',  ( 0.1152809850208375564, 10.03408747456458627, -42.96815531347071726 ) ) ;
#19664 = ORIENTED_EDGE ( 'NONE', *, *, #20519, .T. ) ;
#19665 = CARTESIAN_POINT ( 'NONE',  ( 4.540110984502055302, 10.44709687487745065, 3.997669511110601399E-16 ) ) ;
#19666 = CARTESIAN_POINT ( 'NONE',  ( -6.001507490154111224, 11.48377994779722755, -14.94036486426001353 ) ) ;
#19667 = DIRECTION ( 'NONE',  ( -1.000000000000000000, -0.000000000000000000, -0.000000000000000000 ) ) ;
#19668 = ORIENTED_EDGE ( 'NONE', *, *, #47053, .T. ) ;
#19669 = DIRECTION ( 'NONE',  ( 0.000000000000000000, 0.000000000000000000, 1.000000000000000000 ) ) ;
#19670 = CARTESIAN_POINT ( 'NONE',  ( 2.528190830796656741, -18.76089685257605311, 37.55373330895358208 ) ) ;
#19671 = EDGE_LOOP ( 'NONE', ( #12735, #45150, #51168, #14695 ) ) ;
#19672 = CARTESIAN_POINT ( 'NONE',  ( 0.7762777257811890319, 28.45155622761428660, 38.54028505510729730 ) ) ;
#19673 = EDGE_CURVE ( 'NONE', #46030, #53909, #33941, .T. ) ;
#19674 = AXIS2_PLACEMENT_3D ( 'NONE', #49054, #39070, #30548 ) ;
#19675 = VERTEX_POINT ( 'NONE', #47847 ) ;
#19676 = CARTESIAN_POINT ( 'NONE',  ( 0.5980894510889448457, 33.52121017007780068, 34.51330645350414272 ) ) ;
#19677 = CARTESIAN_POINT ( 'NONE',  ( 0.6030672727741701600, 33.95535904584739484, 34.07876014368871864 ) ) ;
#19678 = VERTEX_POINT ( 'NONE', #37850 ) ;
#19679 = VECTOR ( 'NONE', #11523, 1000.000000000000000 ) ;
#19680 = CARTESIAN_POINT ( 'NONE',  ( 4.322998006666179727, 40.45864630878519108, -25.80712523194233299 ) ) ;
#19681 = CARTESIAN_POINT ( 'NONE',  ( 0.8751705887134553219, -41.19904111682524928, 24.81530984069135570 ) ) ;
#19682 = EDGE_CURVE ( 'NONE', #5752, #57645, #40732, .T. ) ;
#19683 = DIRECTION ( 'NONE',  ( 1.000000000000000000, 1.836909530733573776E-16, -1.925929944387235853E-32 ) ) ;
#19684 = CARTESIAN_POINT ( 'NONE',  ( 3.270143674763207553, -11.71453292426884296, 7.080034332678216913 ) ) ;
#19685 = ORIENTED_EDGE ( 'NONE', *, *, #45653, .F. ) ;
#19686 = CARTESIAN_POINT ( 'NONE',  ( 4.834790513006553603, 47.24803566211424055, 0.4609414235700721174 ) ) ;
#19687 = VERTEX_POINT ( 'NONE', #9936 ) ;
#19688 = CARTESIAN_POINT ( 'NONE',  ( 3.238931869106855377, -36.28407486357536982, 23.06038324659503758 ) ) ;
#19689 =( BOUNDED_SURFACE ( )  B_SPLINE_SURFACE ( 3, 1, ( 
 ( #3755, #42329 ),
 ( #4059, #31992 ),
 ( #46404, #3450 ),
 ( #22588, #23198 ) ),
 .UNSPECIFIED., .F., .F., .F. ) 
 B_SPLINE_SURFACE_WITH_KNOTS ( ( 4, 4 ),
 ( 2, 2 ),
 ( 0.000000000000000000, 1.000000000000000000 ),
 ( 0.000000000000000000, 1.000000000000000000 ),
 .UNSPECIFIED. ) 
 GEOMETRIC_REPRESENTATION_ITEM ( )  RATIONAL_B_SPLINE_SURFACE ( (
 ( 1.000000000000000000, 1.000000000000000000),
 ( 0.7223157951917480446, 0.9931996967497186413),
 ( 0.7223157951917480446, 0.9931996967497186413),
 ( 1.000000000000000000, 1.000000000000000000) ) ) 
 REPRESENTATION_ITEM ( '' )  SURFACE ( )  );
#19690 = ORIENTED_EDGE ( 'NONE', *, *, #9540, .F. ) ;
#19691 = ORIENTED_EDGE ( 'NONE', *, *, #32636, .F. ) ;
#19692 = CARTESIAN_POINT ( 'NONE',  ( 5.901463166500145796, 0.6865185226679980657, -20.10090949829560714 ) ) ;
#19694 = AXIS2_PLACEMENT_3D ( 'NONE', #58058, #14878, #48371 ) ;
#19693 = CARTESIAN_POINT ( 'NONE',  ( 4.924595438175360940, 0.7801755544698492084, -2.999999999999945821 ) ) ;
#19695 = CARTESIAN_POINT ( 'NONE',  ( 0.1365634738349405242, 10.43816654247781806, -42.87082106578719021 ) ) ;
#19696 = ORIENTED_EDGE ( 'NONE', *, *, #9385, .F. ) ;
#19697 = CARTESIAN_POINT ( 'NONE',  ( 5.880360259849752858, -31.59460303415958293, -36.09847387447848632 ) ) ;
#19698 = CARTESIAN_POINT ( 'NONE',  ( 5.880360259849752858, -45.41096578730637390, -15.46489389606739984 ) ) ;
#19699 = EDGE_CURVE ( 'NONE', #61648, #14372, #39168, .T. ) ;
#19700 = ORIENTED_EDGE ( 'NONE', *, *, #29798, .F. ) ;
#19701 = AXIS2_PLACEMENT_3D ( 'NONE', #29102, #38842, #5272 ) ;
#19702 = B_SPLINE_CURVE_WITH_KNOTS ( 'NONE', 3,
 ( #37838, #60978, #52193, #18086 ),
 .UNSPECIFIED., .F., .F.,
 ( 4, 4 ),
 ( 0.000000000000000000, 0.005004741218457439689 ),
 .UNSPECIFIED. ) ;
#19703 = EDGE_LOOP ( 'NONE', ( #58647, #34157, #55336, #33415 ) ) ;
#19704 = CARTESIAN_POINT ( 'NONE',  ( 4.549368137175248350, -8.582197505784725067, 42.06008734272381133 ) ) ;
#19705 = CARTESIAN_POINT ( 'NONE',  ( 0.3676999524040366896, 25.91024933382758277, 35.70167450949220722 ) ) ;
#19706 = LINE ( 'NONE', #29093, #52935 ) ;
#19707 = CARTESIAN_POINT ( 'NONE',  ( 0.9769922540276050338, -26.71843606007641725, -32.28709850063540188 ) ) ;
#19708 = CARTESIAN_POINT ( 'NONE',  ( 0.6846871229502932144, -29.84551600520658354, 37.47592888575237424 ) ) ;
#19709 = EDGE_LOOP ( 'NONE', ( #32074, #55233, #50193, #41287, #31629 ) ) ;
#19710 = CARTESIAN_POINT ( 'NONE',  ( 0.9785694773339250752, -41.82934473077335724, 2.577076853490416486 ) ) ;
#19711 = ORIENTED_EDGE ( 'NONE', *, *, #42155, .F. ) ;
#19712 = CARTESIAN_POINT ( 'NONE',  ( 0.1365634738349406074, -42.83729192637484573, 10.57492506062288307 ) ) ;
#19713 = CARTESIAN_POINT ( 'NONE',  ( 0.8554163680231708922, -0.6539261334248972490, -46.91244881397519606 ) ) ;
#19714 = FACE_OUTER_BOUND ( 'NONE', #10183, .T. ) ;
#19715 = CARTESIAN_POINT ( 'NONE',  ( 0.2940133293163009753, -32.24540449752910831, 30.10771393461770984 ) ) ;
#19716 = CARTESIAN_POINT ( 'NONE',  ( 0.8751705887134423323, -19.22545746485690188, 44.08562551107050353 ) ) ;
#19717 = FILL_AREA_STYLE ('',( #583 ) ) ;
#19718 = CARTESIAN_POINT ( 'NONE',  ( 4.303969348037246512, -45.22910199346984683, 16.39840148505076911 ) ) ;
#19719 = ORIENTED_EDGE ( 'NONE', *, *, #9474, .F. ) ;
#19720 = CARTESIAN_POINT ( 'NONE',  ( -6.016761891674564211, 2.456125503350979677, -18.68243340030200272 ) ) ;
#19721 = CARTESIAN_POINT ( 'NONE',  ( 4.549368137175248350, 2.596185425821331272, 42.84816078363931524 ) ) ;
#19722 = VECTOR ( 'NONE', #865, 1000.000000000000114 ) ;
#19723 = CARTESIAN_POINT ( 'NONE',  ( 0.1156867017252034557, 29.57210022659650051, 32.74803345948146927 ) ) ;
#19724 = CARTESIAN_POINT ( 'NONE',  ( 4.834790513006553603, -4.995710817785154134, 46.98544683568995595 ) ) ;
#19725 = PRESENTATION_LAYER_ASSIGNMENT (  '', '', ( #11723 ) ) ;
#19726 = AXIS2_PLACEMENT_3D ( 'NONE', #5834, #38796, #58462 ) ;
#19727 = CARTESIAN_POINT ( 'NONE',  ( 3.270143674763207553, 13.68510027222513337, -0.2742231296309999844 ) ) ;
#19728 = EDGE_CURVE ( 'NONE', #60297, #36895, #57876, .T. ) ;
#19729 = DIRECTION ( 'NONE',  ( -2.341930812374879235E-31, 1.110223024625156540E-16, 1.000000000000000000 ) ) ;
#19730 = CARTESIAN_POINT ( 'NONE',  ( 0.5850706913938533704, -47.46255051844948980, -6.431767090163312162 ) ) ;
#19731 = EDGE_CURVE ( 'NONE', #19405, #46003, #10746, .T. ) ;
#19732 = B_SPLINE_CURVE_WITH_KNOTS ( 'NONE', 3,
 ( #20285, #43176, #39400, #6753 ),
 .UNSPECIFIED., .F., .F.,
 ( 4, 4 ),
 ( 0.000000000000000000, 0.005013413432710141573 ),
 .UNSPECIFIED. ) ;
#19733 = EDGE_LOOP ( 'NONE', ( #17345, #61636, #11985, #18702 ) ) ;
#19734 = EDGE_CURVE ( 'NONE', #59493, #25828, #55542, .T. ) ;
#19735 = FILL_AREA_STYLE ('',( #34761 ) ) ;
#19736 = VECTOR ( 'NONE', #22971, 1000.000000000000114 ) ;
#19737 = CARTESIAN_POINT ( 'NONE',  ( 1.227938101723756947, -30.94118573761292623, -29.74462687941258210 ) ) ;
#19738 = CARTESIAN_POINT ( 'NONE',  ( 1.112077966505211846, 24.35052357902559450, -36.74346644719130239 ) ) ;
#19739 = CARTESIAN_POINT ( 'NONE',  ( 4.553261556744875094, 40.63093864075490558, 16.69330377710913993 ) ) ;
#19740 = CARTESIAN_POINT ( 'NONE',  ( 4.956445790444027999, 19.33052208089617352, -42.94029536716791995 ) ) ;
#19741 = VERTEX_POINT ( 'NONE', #8148 ) ;
#19742 = CARTESIAN_POINT ( 'NONE',  ( 0.8744876279028263033, 32.34273794994744833, 36.93639603806145288 ) ) ;
#19743 = DIRECTION ( 'NONE',  ( -1.000000000000000000, -0.000000000000000000, -0.000000000000000000 ) ) ;
#19744 = B_SPLINE_CURVE_WITH_KNOTS ( 'NONE', 3,
 ( #54421, #48286, #7115, #6488 ),
 .UNSPECIFIED., .F., .F.,
 ( 4, 4 ),
 ( 0.000000000000000000, 0.004446090762761341700 ),
 .UNSPECIFIED. ) ;
#19745 = CARTESIAN_POINT ( 'NONE',  ( 0.8751705887134553219, 33.37254303619554463, -34.63284514348550402 ) ) ;
#19746 = ORIENTED_EDGE ( 'NONE', *, *, #11200, .T. ) ;
#19747 = CARTESIAN_POINT ( 'NONE',  ( 0.5782707292762442330, -29.72436028066389824, -36.27945368404695614 ) ) ;
#19748 = CARTESIAN_POINT ( 'NONE',  ( 0.9730545539215883499, -41.31259007387222226, -11.59290486963550393 ) ) ;
#19749 = EDGE_CURVE ( 'NONE', #59488, #4551, #9173, .T. ) ;
#19750 = VECTOR ( 'NONE', #47687, 1000.000000000000227 ) ;
#19751 = ORIENTED_EDGE ( 'NONE', *, *, #15232, .T. ) ;
#19752 = CARTESIAN_POINT ( 'NONE',  ( 0.6041374136657476912, -38.27243465845322135, -29.14743607025070204 ) ) ;
#19753 = ORIENTED_EDGE ( 'NONE', *, *, #20975, .T. ) ;
#19754 = CARTESIAN_POINT ( 'NONE',  ( 1.500000000000001332, 0.000000000000000000, 0.000000000000000000 ) ) ;
#19756 = ORIENTED_EDGE ( 'NONE', *, *, #38988, .F. ) ;
#19755 = EDGE_CURVE ( 'NONE', #52026, #15046, #56060, .T. ) ;
#19757 = CARTESIAN_POINT ( 'NONE',  ( 0.1129192098497447394, 29.30421273086510681, -32.98810246148386227 ) ) ;
#19758 = CARTESIAN_POINT ( 'NONE',  ( 2.299746137290199943, -49.01654327427706193, 1.288341230832333428 ) ) ;
#19759 = ORIENTED_EDGE ( 'NONE', *, *, #56632, .F. ) ;
#19760 = CARTESIAN_POINT ( 'NONE',  ( 4.956653778116991482, -21.75875759808677046, -42.88673967249153662 ) ) ;
#19761 = ORIENTED_EDGE ( 'NONE', *, *, #20374, .T. ) ;
#19762 = CARTESIAN_POINT ( 'NONE',  ( 0.5804410086790514622, 45.08525424748427213, 12.91664435118883958 ) ) ;
#19763 = EDGE_CURVE ( 'NONE', #27747, #18385, #32381, .T. ) ;
#19764 = CARTESIAN_POINT ( 'NONE',  ( 4.694002226626921015, 45.58690636503205695, -0.3445860007819027127 ) ) ;
#19765 = CARTESIAN_POINT ( 'NONE',  ( 0.5832655196449142432, 40.23291104114027661, 24.09456478397196477 ) ) ;
#19766 = AXIS2_PLACEMENT_3D ( 'NONE', #19930, #10202, #14298 ) ;
#19767 =( BOUNDED_SURFACE ( )  B_SPLINE_SURFACE ( 3, 1, ( 
 ( #3083, #51622 ),
 ( #17825, #61324 ),
 ( #41639, #32545 ),
 ( #22214, #22521 ) ),
 .UNSPECIFIED., .F., .F., .F. ) 
 B_SPLINE_SURFACE_WITH_KNOTS ( ( 4, 4 ),
 ( 2, 2 ),
 ( 0.000000000000000000, 1.000000000000000000 ),
 ( 0.000000000000000000, 1.000000000000000000 ),
 .UNSPECIFIED. ) 
 GEOMETRIC_REPRESENTATION_ITEM ( )  RATIONAL_B_SPLINE_SURFACE ( (
 ( 1.000000000000000000, 1.000000000000000000),
 ( 0.7211978278499970862, 0.9934217856018976445),
 ( 0.7211978278499970862, 0.9934217856018976445),
 ( 1.000000000000000000, 1.000000000000000000) ) ) 
 REPRESENTATION_ITEM ( '' )  SURFACE ( )  );
#19768 = ORIENTED_EDGE ( 'NONE', *, *, #6607, .F. ) ;
#19769 = CARTESIAN_POINT ( 'NONE',  ( 0.8760168074887090262, -7.161346975773370538, -47.56749362999710939 ) ) ;
#19770 = CARTESIAN_POINT ( 'NONE',  ( 0.5837374860065644988, 33.73893264285595706, -33.99581326751397370 ) ) ;
#19771 = VECTOR ( 'NONE', #55251, 1000.000000000000114 ) ;
#19772 = CARTESIAN_POINT ( 'NONE',  ( 4.962356264823608143, 17.31942680647409460, 38.35717733303029320 ) ) ;
#19773 = CIRCLE ( 'NONE', #11771, 6.728125000000023448 ) ;
#19774 = CARTESIAN_POINT ( 'NONE',  ( 5.959547316686252039, -7.858107265727618085, -18.96183906913540795 ) ) ;
#19775 = ORIENTED_EDGE ( 'NONE', *, *, #31764, .F. ) ;
#19776 = CARTESIAN_POINT ( 'NONE',  ( 0.5998501479064699549, 6.798102206413494386, 47.62484632993690781 ) ) ;
#19777 = ADVANCED_FACE ( 'NONE', ( #26637 ), #41652, .F. ) ;
#19778 = CARTESIAN_POINT ( 'NONE',  ( 0.3622758884714600280, -39.50828911766986096, -17.25816669464980890 ) ) ;
#19779 = ORIENTED_EDGE ( 'NONE', *, *, #51726, .T. ) ;
#19780 = CARTESIAN_POINT ( 'NONE',  ( 0.6846871229502932144, -19.12907057981236036, 43.92355552798031937 ) ) ;
#19781 = ORIENTED_EDGE ( 'NONE', *, *, #55935, .T. ) ;
#19782 = B_SPLINE_CURVE_WITH_KNOTS ( 'NONE', 3,
 ( #15294, #48790, #29676, #10277 ),
 .UNSPECIFIED., .F., .F.,
 ( 4, 4 ),
 ( 2.122407100861210668E-17, 0.004444306975806114161 ),
 .UNSPECIFIED. ) ;
#19783 = LINE ( 'NONE', #4394, #20516 ) ;
#19784 = DIRECTION ( 'NONE',  ( 0.000000000000000000, 0.000000000000000000, 1.000000000000000000 ) ) ;
#19785 = VERTEX_POINT ( 'NONE', #50745 ) ;
#19786 = CARTESIAN_POINT ( 'NONE',  ( 2.281351352603291804, -44.80774876812572671, 17.13758816714735644 ) ) ;
#19787 = CARTESIAN_POINT ( 'NONE',  ( 0.1140933569871965259, 25.55436557308794931, -35.97115997908439766 ) ) ;
#19788 = CARTESIAN_POINT ( 'NONE',  ( 1.827119703190780653, 15.32887915442596594, -40.22835835992449205 ) ) ;
#19789 = CARTESIAN_POINT ( 'NONE',  ( 0.8560838555295158248, -39.18289055412748922, 25.78902716088759206 ) ) ;
#19790 = ORIENTED_EDGE ( 'NONE', *, *, #47376, .T. ) ;
#19791 = CARTESIAN_POINT ( 'NONE',  ( 0.1129192098497447394, -42.80154921430116843, -10.72283417016740259 ) ) ;
#19792 = CARTESIAN_POINT ( 'NONE',  ( 4.291220156522060236, -16.00047830133216564, -44.30997282141229476 ) ) ;
#19793 = B_SPLINE_CURVE_WITH_KNOTS ( 'NONE', 3,
 ( #50656, #45379, #55046, #12170, #31257, #56590 ),
 .UNSPECIFIED., .F., .F.,
 ( 4, 2, 4 ),
 ( 8.546004838552221719E-17, 0.0002293366620881438192, 0.0004586733241762021491 ),
 .UNSPECIFIED. ) ;
#19794 = CARTESIAN_POINT ( 'NONE',  ( 0.9772918015221170318, 41.47740498993091052, -5.996810073025064192 ) ) ;
#19795 = LINE ( 'NONE', #19181, #37958 ) ;
#19796 = CARTESIAN_POINT ( 'NONE',  ( -6.078726893082806448, 15.43407385306362301, 11.51448676958282391 ) ) ;
#19797 = CARTESIAN_POINT ( 'NONE',  ( -1.200000000000006617, 0.000000000000000000, 0.000000000000000000 ) ) ;
#19798 = AXIS2_PLACEMENT_3D ( 'NONE', #43167, #33144, #5217 ) ;
#19799 = CARTESIAN_POINT ( 'NONE',  ( 0.6064782688330865312, 43.44828147745647584, -17.65166516435432342 ) ) ;
#19800 = EDGE_CURVE ( 'NONE', #46169, #55636, #30677, .T. ) ;
#19801 = B_SPLINE_CURVE_WITH_KNOTS ( 'NONE', 3,
 ( #10978, #34165, #15679, #43573 ),
 .UNSPECIFIED., .F., .F.,
 ( 4, 4 ),
 ( 0.000000000000000000, 0.004444103432399267029 ),
 .UNSPECIFIED. ) ;
#19802 = CARTESIAN_POINT ( 'NONE',  ( -2.708315649062910779, 14.63219292706382646, 0.2635547933244035690 ) ) ;
#19803 = CARTESIAN_POINT ( 'NONE',  ( 0.9757954354143122400, -4.033171854401937560E-17, -42.90846090505964128 ) ) ;
#19804 = EDGE_CURVE ( 'NONE', #41909, #32930, #36678, .T. ) ;
#19805 = CARTESIAN_POINT ( 'NONE',  ( 0.9730545539215883499, 29.98130006528905156, -30.69604515769618658 ) ) ;
#19806 = DIRECTION ( 'NONE',  ( 0.000000000000000000, 0.000000000000000000, -1.000000000000000000 ) ) ;
#19807 = DIRECTION ( 'NONE',  ( 1.000000000000000000, 1.836909530733573776E-16, 0.000000000000000000 ) ) ;
#19808 = CARTESIAN_POINT ( 'NONE',  ( 0.8760168074886965917, -11.58706983520293221, -46.68716261866173056 ) ) ;
#19809 = EDGE_CURVE ( 'NONE', #1366, #3780, #1726, .T. ) ;
#19810 = EDGE_CURVE ( 'NONE', #16670, #147, #54764, .T. ) ;
#19811 = CARTESIAN_POINT ( 'NONE',  ( 0.5980271706414711508, -45.25597162979951804, -19.07737599054031463 ) ) ;
#19812 = LINE ( 'NONE', #19500, #61193 ) ;
#19813 = EDGE_CURVE ( 'NONE', #26300, #36881, #45820, .T. ) ;
#19814 = EDGE_LOOP ( 'NONE', ( #59870, #54816, #33378, #54021 ) ) ;
#19815 = AXIS2_PLACEMENT_3D ( 'NONE', #22245, #28781, #61657 ) ;
#19816 = DIRECTION ( 'NONE',  ( 0.000000000000000000, 0.7071067811865421326, 0.7071067811865527908 ) ) ;
#19817 = CARTESIAN_POINT ( 'NONE',  ( 0.9791128995231621612, -1.395278494606673636, 41.88544654374177156 ) ) ;
#19818 = CARTESIAN_POINT ( 'NONE',  ( 0.9762797500689124330, -30.73989051779348003, 28.48480149377514437 ) ) ;
#19819 = ORIENTED_EDGE ( 'NONE', *, *, #55504, .T. ) ;
#19820 = CARTESIAN_POINT ( 'NONE',  ( 0.5786265663353153954, 47.39171391660402577, -6.967625775955234246 ) ) ;
#19821 = FACE_OUTER_BOUND ( 'NONE', #11648, .T. ) ;
#19822 = B_SPLINE_CURVE_WITH_KNOTS ( 'NONE', 3,
 ( #21960, #36687, #60759, #37005 ),
 .UNSPECIFIED., .F., .F.,
 ( 4, 4 ),
 ( 0.000000000000000000, 0.004041751736740985604 ),
 .UNSPECIFIED. ) ;
#19823 = ORIENTED_EDGE ( 'NONE', *, *, #2524, .F. ) ;
#19824 = VERTEX_POINT ( 'NONE', #8763 ) ;
#19825 = CARTESIAN_POINT ( 'NONE',  ( 0.7948878604505658085, 37.94263140573792015, 31.16176133190687736 ) ) ;
#19826 = EDGE_CURVE ( 'NONE', #38104, #9098, #9969, .T. ) ;
#19827 = VERTEX_POINT ( 'NONE', #37293 ) ;
#19828 = CARTESIAN_POINT ( 'NONE',  ( 5.960721111146673579, -12.50019045452726907, -16.28018152803688778 ) ) ;
#19829 = CIRCLE ( 'NONE', #24823, 43.08621763946400307 ) ;
#19831 = VERTEX_POINT ( 'NONE', #9072 ) ;
#19830 = ADVANCED_FACE ( 'NONE', ( #23180 ), #41290, .F. ) ;
#19832 = EDGE_LOOP ( 'NONE', ( #17621, #4692, #34098, #55093 ) ) ;
#19833 = CARTESIAN_POINT ( 'NONE',  ( 0.9722240741986377666, 25.65687427836904888, 34.39263045016065234 ) ) ;
#19834 = ORIENTED_EDGE ( 'NONE', *, *, #57794, .T. ) ;
#19835 = CARTESIAN_POINT ( 'NONE',  ( 0.6023142530420679819, -29.07781306567130386, 38.32506243004142021 ) ) ;
#19836 = CARTESIAN_POINT ( 'NONE',  ( 3.376099380956842921, -1.774645281739918090, 13.28755123249070635 ) ) ;
#19837 = CARTESIAN_POINT ( 'NONE',  ( 3.407937589446174087, -12.08659953757613259, 6.447869442558121555 ) ) ;
#19838 = VERTEX_POINT ( 'NONE', #14716 ) ;
#19839 = CARTESIAN_POINT ( 'NONE',  ( 1.231276596079881047, -13.22565419922034557, 39.77887431816932917 ) ) ;
#19840 = EDGE_CURVE ( 'NONE', #5480, #3927, #57939, .T. ) ;
#19841 = CARTESIAN_POINT ( 'NONE',  ( 0.9758171775293910111, -34.04519363167618451, -26.11633498242663975 ) ) ;
#19842 = ORIENTED_EDGE ( 'NONE', *, *, #19826, .F. ) ;
#19843 = VERTEX_POINT ( 'NONE', #18481 ) ;
#19844 = CARTESIAN_POINT ( 'NONE',  ( 4.956653778116988818, -45.35992544608517818, -15.97476558431931082 ) ) ;
#19845 = CARTESIAN_POINT ( 'NONE',  ( 1.000110580585050535, -37.10379152213305787, -19.48656299746027543 ) ) ;
#19846 = LINE ( 'NONE', #28917, #230 ) ;
#19847 = CARTESIAN_POINT ( 'NONE',  ( 4.834790513006555379, 29.81904690970609551, 36.65260948856339951 ) ) ;
#19848 = DIRECTION ( 'NONE',  ( 0.000000000000000000, -0.7071067811865435759, -0.7071067811865514585 ) ) ;
#19849 = ADVANCED_FACE ( 'NONE', ( #37607 ), #31726, .F. ) ;
#19850 = VERTEX_POINT ( 'NONE', #5277 ) ;
#19851 = CARTESIAN_POINT ( 'NONE',  ( 4.975801465491695552, -46.87746200127462970, 9.906103548667402947 ) ) ;
#19852 = CARTESIAN_POINT ( 'NONE',  ( 4.549368137175248350, 0.000000000000000000, 0.000000000000000000 ) ) ;
#19853 = ADVANCED_FACE ( 'NONE', ( #61066 ), #9613, .F. ) ;
#19854 = FACE_OUTER_BOUND ( 'NONE', #17968, .T. ) ;
#19855 = CARTESIAN_POINT ( 'NONE',  ( 0.6000166863083106206, -25.01014854877413995, -42.26483113981061024 ) ) ;
#19856 = ORIENTED_EDGE ( 'NONE', *, *, #47323, .F. ) ;
#19857 = CARTESIAN_POINT ( 'NONE',  ( 4.303969348037246512, 40.54345935592778716, 25.89994482339384163 ) ) ;
#19858 = CARTESIAN_POINT ( 'NONE',  ( 2.282803330402958242, 46.36091562948769251, 7.560582613298351795 ) ) ;
#19859 = FACE_OUTER_BOUND ( 'NONE', #24275, .T. ) ;
#19860 = VECTOR ( 'NONE', #57023, 1000.000000000000114 ) ;
#19861 = AXIS2_PLACEMENT_3D ( 'NONE', #25866, #59991, #49986 ) ;
#19862 = ORIENTED_EDGE ( 'NONE', *, *, #27256, .T. ) ;
#19863 = ORIENTED_EDGE ( 'NONE', *, *, #38632, .F. ) ;
#19864 = CARTESIAN_POINT ( 'NONE',  ( 1.154321485836934169, 39.32643515542059731, -17.18284940416407736 ) ) ;
#19865 = DIRECTION ( 'NONE',  ( 0.1024043820194936311, 0.1428674944015942416, 0.9844298967354739860 ) ) ;
#19866 = CARTESIAN_POINT ( 'NONE',  ( 0.1101816497532063233, -39.78963561881077737, 16.62841624476607194 ) ) ;
#19867 = FACE_OUTER_BOUND ( 'NONE', #559, .T. ) ;
#19868 = CARTESIAN_POINT ( 'NONE',  ( 0.7764146366350237471, -20.54893576326343307, -42.16374879759197825 ) ) ;
#19869 = CARTESIAN_POINT ( 'NONE',  ( 0.1158816050234199174, -31.69261404977700280, 30.70049276472673228 ) ) ;
#19870 =( BOUNDED_SURFACE ( )  B_SPLINE_SURFACE ( 3, 1, ( 
 ( #48078, #43086 ),
 ( #39010, #29264 ),
 ( #24260, #52141 ),
 ( #28342, #757 ) ),
 .UNSPECIFIED., .F., .F., .F. ) 
 B_SPLINE_SURFACE_WITH_KNOTS ( ( 4, 4 ),
 ( 2, 2 ),
 ( 0.000000000000000000, 1.000000000000000000 ),
 ( 0.000000000000000000, 1.000000000000000000 ),
 .UNSPECIFIED. ) 
 GEOMETRIC_REPRESENTATION_ITEM ( )  RATIONAL_B_SPLINE_SURFACE ( (
 ( 1.000000000000000000, 1.000000000000000000),
 ( 0.9953485035131437453, 0.8621029689291523912),
 ( 0.9953485035131437453, 0.8621029689291523912),
 ( 1.000000000000000000, 1.000000000000000000) ) ) 
 REPRESENTATION_ITEM ( '' )  SURFACE ( )  );
#19871 = CARTESIAN_POINT ( 'NONE',  ( 2.618530812446111078, -29.26021975733388203, -36.79084572214571125 ) ) ;
#19872 = CARTESIAN_POINT ( 'NONE',  ( 4.549368137175248350, 32.13400537129925283, -28.46244473166639111 ) ) ;
#19873 = CARTESIAN_POINT ( 'NONE',  ( 0.7954196712028458460, 19.20650004025001678, -44.09776749253662587 ) ) ;
#19874 = CARTESIAN_POINT ( 'NONE',  ( 0.6029303876144825880, -18.28892193312832859, -44.49541906039121386 ) ) ;
#19875 = B_SPLINE_CURVE_WITH_KNOTS ( 'NONE', 3,
 ( #7156, #49169, #20366, #11273 ),
 .UNSPECIFIED., .F., .F.,
 ( 4, 4 ),
 ( 2.165753205240583906E-17, 0.004559932413162187670 ),
 .UNSPECIFIED. ) ;
#19876 = ORIENTED_EDGE ( 'NONE', *, *, #51828, .F. ) ;
#19877 = CIRCLE ( 'NONE', #57848, 2.649999999999992806 ) ;
#19878 = CARTESIAN_POINT ( 'NONE',  ( 5.000000000000007994, -58.44237546506844438, 54.69470952477915660 ) ) ;
#19879 = CARTESIAN_POINT ( 'NONE',  ( 4.967162193818130511, 0.000000000000000000, 0.000000000000000000 ) ) ;
#19880 = ADVANCED_FACE ( 'NONE', ( #13799 ), #60452, .F. ) ;
#19881 = CARTESIAN_POINT ( 'NONE',  ( 0.5807400328401574052, 28.72484455891697053, -38.33001520688919328 ) ) ;
#19882 = CARTESIAN_POINT ( 'NONE',  ( 3.238018933889920792, 1.614035038994356519, -13.29670572963662423 ) ) ;
#19883 = CARTESIAN_POINT ( 'NONE',  ( 0.6039202388192952409, -20.03711874569821205, 44.83388880322316794 ) ) ;
#19884 = CARTESIAN_POINT ( 'NONE',  ( 0.5832367798473397924, -41.61463593465321509, 23.71165515427700043 ) ) ;
#19885 = DIRECTION ( 'NONE',  ( 0.000000000000000000, 0.000000000000000000, 1.000000000000000000 ) ) ;
#19886 = CONTEXT_DEPENDENT_SHAPE_REPRESENTATION ( #3938, #10355 ) ;
#19888 = EDGE_CURVE ( 'NONE', #56636, #59488, #12985, .T. ) ;
#19887 = CARTESIAN_POINT ( 'NONE',  ( 3.660176727303411148, 20.10773453922346832, -43.62748706623501960 ) ) ;
#19889 = AXIS2_PLACEMENT_3D ( 'NONE', #29336, #42850, #37533 ) ;
#19890 =( BOUNDED_SURFACE ( )  B_SPLINE_SURFACE ( 3, 1, ( 
 ( #3558, #32407 ),
 ( #56190, #60887 ),
 ( #23312, #36191 ),
 ( #51481, #55255 ) ),
 .UNSPECIFIED., .F., .F., .F. ) 
 B_SPLINE_SURFACE_WITH_KNOTS ( ( 4, 4 ),
 ( 2, 2 ),
 ( 0.000000000000000000, 1.000000000000000000 ),
 ( 0.000000000000000000, 1.000000000000000000 ),
 .UNSPECIFIED. ) 
 GEOMETRIC_REPRESENTATION_ITEM ( )  RATIONAL_B_SPLINE_SURFACE ( (
 ( 1.000000000000000000, 1.000000000000000000),
 ( 0.9953040768229005630, 0.8617119497784937465),
 ( 0.9953040768229005630, 0.8617119497784937465),
 ( 1.000000000000000000, 1.000000000000000000) ) ) 
 REPRESENTATION_ITEM ( '' )  SURFACE ( )  );
#19891 = CARTESIAN_POINT ( 'NONE',  ( 0.5997462898726536595, 22.24958391914565681, -43.77793560195825506 ) ) ;
#19892 = CARTESIAN_POINT ( 'NONE',  ( 0.6026112563231247332, -30.75395997435152751, 38.28491792860723564 ) ) ;
#19893 = EDGE_CURVE ( 'NONE', #31073, #49600, #36836, .T. ) ;
#19894 = CARTESIAN_POINT ( 'NONE',  ( -6.016761891674564211, 4.873659902332621918, -18.20201388312090529 ) ) ;
#19895 = CARTESIAN_POINT ( 'NONE',  ( 0.9762797500689124330, -37.17323042682988188, 19.35137526946117958 ) ) ;
#19896 = ADVANCED_FACE ( 'NONE', ( #49444 ), #20337, .F. ) ;
#19898 = ORIENTED_EDGE ( 'NONE', *, *, #26446, .T. ) ;
#19897 = CARTESIAN_POINT ( 'NONE',  ( -2.739355103387248747, -9.511660422586917463, -11.50547187021943429 ) ) ;
#19899 = ORIENTED_EDGE ( 'NONE', *, *, #55256, .T. ) ;
#19900 = CARTESIAN_POINT ( 'NONE',  ( 4.975801465491694664, 36.39623109580467997, -31.15993731089085017 ) ) ;
#19901 = FACE_OUTER_BOUND ( 'NONE', #27081, .T. ) ;
#19902 = CIRCLE ( 'NONE', #32770, 48.09070567114147110 ) ;
#19903 = EDGE_CURVE ( 'NONE', #55806, #8492, #31595, .T. ) ;
#19904 = CARTESIAN_POINT ( 'NONE',  ( 0.1157506346131639274, 41.90541932839798278, 13.81580582933776036 ) ) ;
#19905 = VERTEX_POINT ( 'NONE', #15950 ) ;
#19906 = CARTESIAN_POINT ( 'NONE',  ( 4.962356264823609919, 39.89814050050791394, -13.39305724859256763 ) ) ;
#19907 = CARTESIAN_POINT ( 'NONE',  ( 0.5806925824938511393, -45.84420715090610798, 9.875780123533177246 ) ) ;
#19908 = CARTESIAN_POINT ( 'NONE',  ( 5.895881250540457863, -19.39704354167987077, 5.318118412603870304 ) ) ;
#19909 = B_SPLINE_CURVE_WITH_KNOTS ( 'NONE', 3,
 ( #60121, #11930, #41658, #31941 ),
 .UNSPECIFIED., .F., .F.,
 ( 4, 4 ),
 ( 0.000000000000000000, 0.004447772540403785099 ),
 .UNSPECIFIED. ) ;
#19910 = B_SPLINE_CURVE_WITH_KNOTS ( 'NONE', 3,
 ( #37480, #8629, #56555, #22744, #46885, #23061, #41878, #13671, #41562, #45640, #2692, #55937, #17739, #12748, #56243, #46566 ),
 .UNSPECIFIED., .F., .F.,
 ( 4, 3, 3, 3, 3, 4 ),
 ( 2.081781105835003771E-17, 0.0002612764279487743012, 0.0003919131003184794619, 0.0005225497727000646053, 0.0007837925190632457880, 0.001045051706266715216 ),
 .UNSPECIFIED. ) ;
#19911 = ORIENTED_EDGE ( 'NONE', *, *, #7489, .F. ) ;
#19912 = ORIENTED_EDGE ( 'NONE', *, *, #58107, .T. ) ;
#19913 = ADVANCED_FACE ( 'NONE', ( #43541 ), #32873, .F. ) ;
#19914 = CARTESIAN_POINT ( 'NONE',  ( 0.6023143664670691511, -23.82663958122407522, -41.79259346737314473 ) ) ;
#19915 = CIRCLE ( 'NONE', #27890, 12.50000000000000000 ) ;
#19916 = CARTESIAN_POINT ( 'NONE',  ( 0.9722240741986376555, -39.41582013185135480, -16.95645453362505961 ) ) ;
#19917 = CARTESIAN_POINT ( 'NONE',  ( 4.322998006666179727, 14.45630056002876174, 45.75942687572302958 ) ) ;
#19918 = CARTESIAN_POINT ( 'NONE',  ( 0.2279481005628791745, 14.52238209920514933, 41.66057975157808357 ) ) ;
#19919 = CARTESIAN_POINT ( 'NONE',  ( 0.3622758884714730732, -41.42293301073634382, 11.95365414648425428 ) ) ;
#19920 = DIRECTION ( 'NONE',  ( 0.000000000000000000, 0.000000000000000000, 1.000000000000000000 ) ) ;
#19921 = PRODUCT_DEFINITION_SHAPE ( 'NONE', 'NONE',  #43635 ) ;
#19922 = CARTESIAN_POINT ( 'NONE',  ( 0.5839879882012675161, 37.99840755997087172, -29.15724166963611452 ) ) ;
#19923 = ORIENTED_EDGE ( 'NONE', *, *, #14585, .T. ) ;
#19924 = ORIENTED_EDGE ( 'NONE', *, *, #51418, .F. ) ;
#19925 = CARTESIAN_POINT ( 'NONE',  ( 3.782625744892850861, 34.03288848122618049, 24.67793763099795967 ) ) ;
#19926 = CARTESIAN_POINT ( 'NONE',  ( 3.559346040607745287, 43.96414470145123943, 0.7643704676690852295 ) ) ;
#19927 = AXIS2_PLACEMENT_3D ( 'NONE', #3269, #22714, #45930 ) ;
#19928 = ORIENTED_EDGE ( 'NONE', *, *, #36445, .F. ) ;
#19929 = CARTESIAN_POINT ( 'NONE',  ( 4.967162193818132288, 19.45289607368876617, -38.44485641567052880 ) ) ;
#19930 = CARTESIAN_POINT ( 'NONE',  ( 4.967162193818130511, 0.000000000000000000, 0.000000000000000000 ) ) ;
#19931 = CARTESIAN_POINT ( 'NONE',  ( -2.601141883200665639, 14.91765895884289428, -0.5088011959921571181 ) ) ;
#19932 = ORIENTED_EDGE ( 'NONE', *, *, #33530, .T. ) ;
#19933 = CARTESIAN_POINT ( 'NONE',  ( 50.15577769773999961, 0.000000000000000000, 0.000000000000000000 ) ) ;
#19934 = CARTESIAN_POINT ( 'NONE',  ( 4.553261556744875094, 0.000000000000000000, 0.000000000000000000 ) ) ;
#19935 = CARTESIAN_POINT ( 'NONE',  ( 0.1098349054025746646, -37.23978094195836519, -21.74670956129746813 ) ) ;
#19936 = PRODUCT_DEFINITION_FORMATION_WITH_SPECIFIED_SOURCE ( 'ANY', '', #36825, .NOT_KNOWN. ) ;
#19937 = EDGE_CURVE ( 'NONE', #36320, #43985, #29717, .T. ) ;
#19938 = ORIENTED_EDGE ( 'NONE', *, *, #8512, .T. ) ;
#19939 = CARTESIAN_POINT ( 'NONE',  ( 0.6026777506516367566, 4.542038867869873542, -48.89699656993237653 ) ) ;
#19940 = ORIENTED_EDGE ( 'NONE', *, *, #26723, .T. ) ;
#19941 = CARTESIAN_POINT ( 'NONE',  ( 0.6064782688330857541, -44.06397689832020603, -16.05304912853237553 ) ) ;
#19942 = CARTESIAN_POINT ( 'NONE',  ( 4.956445790444011124, -16.41925925744418180, -44.13554095710700409 ) ) ;
#19943 = ORIENTED_EDGE ( 'NONE', *, *, #16602, .F. ) ;
#19944 = CARTESIAN_POINT ( 'NONE',  ( 5.000000000000007994, -58.44237546506844438, 54.69470952477916370 ) ) ;
#19945 = CARTESIAN_POINT ( 'NONE',  ( 0.1073791018717483448, -6.109314776652422729, -42.68962945260951614 ) ) ;
#19946 = PRODUCT_RELATED_PRODUCT_CATEGORY ( 'part', '', ( #31800 ) ) ;
#19947 = CARTESIAN_POINT ( 'NONE',  ( 0.5804410086790514622, -34.41390132670950663, -31.86225427258558440 ) ) ;
#19948 = DIRECTION ( 'NONE',  ( -1.000000000000000000, -0.000000000000000000, -0.000000000000000000 ) ) ;
#19949 = CARTESIAN_POINT ( 'NONE',  ( 0.1145239942831223490, 33.80898014942432894, -28.35310109953591251 ) ) ;
#19950 = CARTESIAN_POINT ( 'NONE',  ( 0.2230388203127631752, 26.84831060237797118, 33.74101226470672543 ) ) ;
#19951 = CARTESIAN_POINT ( 'NONE',  ( 0.8557997880470599172, 46.50333260518575429, -11.51622788066409697 ) ) ;
#19952 = FACE_OUTER_BOUND ( 'NONE', #18286, .T. ) ;
#19953 = VERTEX_POINT ( 'NONE', #48832 ) ;
#19954 = CARTESIAN_POINT ( 'NONE',  ( 0.9787464366903548818, 41.51074110666462502, 5.761281599256292907 ) ) ;
#19955 = CARTESIAN_POINT ( 'NONE',  ( 3.894904216938897878, -15.73571937194873804, 41.04280044445649622 ) ) ;
#19956 = ORIENTED_EDGE ( 'NONE', *, *, #36382, .F. ) ;
#19957 = VECTOR ( 'NONE', #58458, 1000.000000000000000 ) ;
#19958 = CARTESIAN_POINT ( 'NONE',  ( 5.960721111146673579, 2.685391721746036353, -20.34914600876572521 ) ) ;
#19959 = CARTESIAN_POINT ( 'NONE',  ( 4.975610109902397937, 42.89797504594920241, 23.49921581872238718 ) ) ;
#19960 = EDGE_CURVE ( 'NONE', #26927, #38058, #23388, .T. ) ;
#19961 = CARTESIAN_POINT ( 'NONE',  ( 2.624215991343620935, -13.78323291683751606, -45.98641578154045817 ) ) ;
#19962 = CARTESIAN_POINT ( 'NONE',  ( 0.5980894510889448457, 17.76188940524884075, 44.71414919659913068 ) ) ;
#19963 = CARTESIAN_POINT ( 'NONE',  ( 0.6026112563231247332, -20.03700257410760699, 44.83368736507640762 ) ) ;
#19964 = DIRECTION ( 'NONE',  ( 0.000000000000000000, 0.000000000000000000, -1.000000000000000000 ) ) ;
#19966 = EDGE_CURVE ( 'NONE', #6350, #36253, #25032, .T. ) ;
#19965 = CARTESIAN_POINT ( 'NONE',  ( 0.7954196712028472893, 17.60078400783960006, 44.76287685048092868 ) ) ;
#19967 = FACE_OUTER_BOUND ( 'NONE', #6869, .T. ) ;
#19968 = EDGE_CURVE ( 'NONE', #8227, #8570, #52550, .T. ) ;
#19969 = CARTESIAN_POINT ( 'NONE',  ( 2.526552050251863246, 37.81244156771019505, -20.43086833796918356 ) ) ;
#19970 = ADVANCED_FACE ( 'NONE', ( #32207 ), #39644, .F. ) ;
#19972 = ORIENTED_EDGE ( 'NONE', *, *, #50439, .T. ) ;
#19971 = CARTESIAN_POINT ( 'NONE',  ( 4.833616638992208614, -38.20222678111956327, 26.07076047129070773 ) ) ;
#19973 = ORIENTED_EDGE ( 'NONE', *, *, #51257, .F. ) ;
#19975 = CONICAL_SURFACE ( 'NONE', #43000, 43.08621763946400307, 1.568696531533066763 ) ;
#19974 = CARTESIAN_POINT ( 'NONE',  ( 0.8557997880470690211, -28.43566216844996930, 38.55640757422429488 ) ) ;
#19976 = DIRECTION ( 'NONE',  ( 0.07439287786467665975, 0.9971416435352942198, 0.01320009283087282027 ) ) ;
#19977 = EDGE_CURVE ( 'NONE', #61565, #17051, #8077, .T. ) ;
#19978 = CARTESIAN_POINT ( 'NONE',  ( 2.299746137290199943, -26.51152743748404816, -41.24827572902495376 ) ) ;
#19979 = CARTESIAN_POINT ( 'NONE',  ( 0.8760168074886965917, 42.09738177923954794, -23.27577685234553684 ) ) ;
#19980 = CARTESIAN_POINT ( 'NONE',  ( 5.958863334805807099, -20.35021240744033122, -2.677925489610565979 ) ) ;
#19981 = VERTEX_POINT ( 'NONE', #16558 ) ;
#19982 = CARTESIAN_POINT ( 'NONE',  ( 0.3676999524040323597, -22.15802448779959377, -38.14410221935904843 ) ) ;
#19983 = ADVANCED_FACE ( 'NONE', ( #60078 ), #13661, .F. ) ;
#19984 = FACE_OUTER_BOUND ( 'NONE', #39897, .T. ) ;
#19985 = CARTESIAN_POINT ( 'NONE',  ( 2.648799415243708655, -2.956030660111293784, -48.94669903094671781 ) ) ;
#19986 = ORIENTED_EDGE ( 'NONE', *, *, #27947, .T. ) ;
#19987 = ADVANCED_FACE ( 'NONE', ( #22489 ), #4832, .F. ) ;
#19988 = B_SPLINE_CURVE_WITH_KNOTS ( 'NONE', 3,
 ( #49164, #608, #5302, #38555, #33855, #57606 ),
 .UNSPECIFIED., .F., .F.,
 ( 4, 2, 4 ),
 ( 1.253517773560139088E-16, 0.0002450741128632347274, 0.0004901482257263441210 ),
 .UNSPECIFIED. ) ;
#19989 = CARTESIAN_POINT ( 'NONE',  ( 4.691466044806103852, 24.49380602310813870, -37.25818859570281916 ) ) ;
#19990 = CARTESIAN_POINT ( 'NONE',  ( 1.088908134280558437, -20.77739698351960129, 37.54826033999255230 ) ) ;
#19991 = ORIENTED_EDGE ( 'NONE', *, *, #50593, .T. ) ;
#19992 =( REPRESENTATION_RELATIONSHIP ('NONE','NONE', #44881, #40484 ) REPRESENTATION_RELATIONSHIP_WITH_TRANSFORMATION ( #52753 )SHAPE_REPRESENTATION_RELATIONSHIP( ) );
#19993 =( BOUNDED_SURFACE ( )  B_SPLINE_SURFACE ( 3, 1, ( 
 ( #2765, #44799 ),
 ( #36013, #26580 ),
 ( #1518, #17198 ),
 ( #15967, #35079 ) ),
 .UNSPECIFIED., .F., .F., .F. ) 
 B_SPLINE_SURFACE_WITH_KNOTS ( ( 4, 4 ),
 ( 2, 2 ),
 ( 0.000000000000000000, 1.000000000000000000 ),
 ( 0.000000000000000000, 1.000000000000000000 ),
 .UNSPECIFIED. ) 
 GEOMETRIC_REPRESENTATION_ITEM ( )  RATIONAL_B_SPLINE_SURFACE ( (
 ( 1.000000000000000000, 1.000000000000000000),
 ( 0.7269869731126817891, 0.9931720237060910339),
 ( 0.7269869731126817891, 0.9931720237060910339),
 ( 1.000000000000000000, 1.000000000000000000) ) ) 
 REPRESENTATION_ITEM ( '' )  SURFACE ( )  );
#19994 = CARTESIAN_POINT ( 'NONE',  ( -6.078075953587585900, -8.901949479772877538, -17.07484903906055962 ) ) ;
#19995 = ORIENTED_EDGE ( 'NONE', *, *, #1325, .F. ) ;
#19996 = DIRECTION ( 'NONE',  ( -0.1024043820194934507, 0.9573600124648741216, 0.2701391291102821501 ) ) ;
#19998 = CARTESIAN_POINT ( 'NONE',  ( 4.549368137175248350, -40.71620287708334018, -13.59764261105737404 ) ) ;
#19997 = AXIS2_PLACEMENT_3D ( 'NONE', #36482, #22061, #12366 ) ;
#19999 = ORIENTED_EDGE ( 'NONE', *, *, #30418, .T. ) ;
#20000 = CARTESIAN_POINT ( 'NONE',  ( 0.5998501479064699549, -38.48283596222010061, -28.86886762351111457 ) ) ;
#20001 = DIRECTION ( 'NONE',  ( 0.09722883295013597105, 0.8382159563662602286, -0.5366009360187049548 ) ) ;
#20002 = CARTESIAN_POINT ( 'NONE',  ( 0.9791128995231607179, 40.42097734080745397, 11.06715975578630839 ) ) ;
#20003 = DIRECTION ( 'NONE',  ( 1.000000000000000000, 0.000000000000000000, 0.000000000000000000 ) ) ;
#20004 = B_SPLINE_CURVE_WITH_KNOTS ( 'NONE', 3,
 ( #31357, #54834, #21963, #59851 ),
 .UNSPECIFIED., .F., .F.,
 ( 4, 4 ),
 ( 0.000000000000000000, 0.004446090762761376394 ),
 .UNSPECIFIED. ) ;
#20005 = EDGE_LOOP ( 'NONE', ( #31215, #28501, #43640, #29163 ) ) ;
#20006 = DIRECTION ( 'NONE',  ( 0.07906939808003035641, 0.4122784474075788519, 0.9076202466287637272 ) ) ;
#20007 = CARTESIAN_POINT ( 'NONE',  ( 5.974727161628367256, 16.29297756969631195, 12.48248968439934536 ) ) ;
#20008 = VERTEX_POINT ( 'NONE', #7127 ) ;
#20009 = DIRECTION ( 'NONE',  ( 0.07906939808003032866, 0.9784699099467771832, -0.1906427696399925209 ) ) ;
#20010 = EDGE_CURVE ( 'NONE', #20493, #31086, #21258, .T. ) ;
#20011 = VERTEX_POINT ( 'NONE', #26254 ) ;
#20012 = CARTESIAN_POINT ( 'NONE',  ( -6.077587904424778920, -11.01164173315302008, 15.79682777441765751 ) ) ;
#20013 = ORIENTED_EDGE ( 'NONE', *, *, #55771, .T. ) ;
#20014 = CARTESIAN_POINT ( 'NONE',  ( 3.678834586032788234, 12.69316164127655000, -47.30217772129290665 ) ) ;
#20015 = DIRECTION ( 'NONE',  ( -1.000000000000000000, 0.000000000000000000, -0.000000000000000000 ) ) ;
#20016 = AXIS2_PLACEMENT_3D ( 'NONE', #11083, #36673, #50443 ) ;
#20017 = FACE_OUTER_BOUND ( 'NONE', #3384, .T. ) ;
#20018 = VERTEX_POINT ( 'NONE', #21880 ) ;
#20019 = CARTESIAN_POINT ( 'NONE',  ( 4.975610109902397937, -48.84566763821283786, -2.559328059280381318 ) ) ;
#20020 = CARTESIAN_POINT ( 'NONE',  ( 0.5839880159502364165, -6.296669079378488298, 47.48028790449881598 ) ) ;
#20021 = CARTESIAN_POINT ( 'NONE',  ( 5.960721111146673579, 16.28018152803675633, 12.50019045452743782 ) ) ;
#20022 = ORIENTED_EDGE ( 'NONE', *, *, #52376, .T. ) ;
#20023 = B_SPLINE_CURVE_WITH_KNOTS ( 'NONE', 3,
 ( #23088, #168, #43444, #48128, #23390, #3948, #56268, #61879, #33114, #19018, #47509, #4555, #52187, #61272, #18390, #23696 ),
 .UNSPECIFIED., .F., .F.,
 ( 4, 3, 3, 3, 3, 4 ),
 ( 1.127622383284612036E-17, 0.0002724568934985558181, 0.0004086836638483798759, 0.0005449104342063616335, 0.0008173270854453682996, 0.001089761613562687925 ),
 .UNSPECIFIED. ) ;
#20024 = ORIENTED_EDGE ( 'NONE', *, *, #5224, .F. ) ;
#20025 = CARTESIAN_POINT ( 'NONE',  ( 0.5809828226811617480, 17.82437196699680726, 44.45562576850608139 ) ) ;
#20026 = B_SPLINE_CURVE_WITH_KNOTS ( 'NONE', 3,
 ( #6278, #57671, #24183, #43323, #1286, #48307, #58601, #20420, #39547, #5970, #353, #15415, #10095, #24808, #33916, #34840, #49225, #25413, #10718, #34527, #19504, #53907, #38936, #44560, #52992 ),
 .UNSPECIFIED., .F., .F.,
 ( 4, 3, 3, 3, 3, 3, 3, 3, 4 ),
 ( 6.254634441385501517E-18, 0.0005656085177311400737, 0.001131215744874499189, 0.001696821861372766133, 0.002262427090022496850, 0.002828031679238745058, 0.003393635864401603995, 0.003977030878808130755, 0.004561030005651158133 ),
 .UNSPECIFIED. ) ;
#20027 = CARTESIAN_POINT ( 'NONE',  ( 0.6000166863083090663, -19.40010892967620038, -45.11606427011504650 ) ) ;
#20028 = CARTESIAN_POINT ( 'NONE',  ( 0.1084644655670281704, 30.77359411724684435, 30.21121552071008054 ) ) ;
#20029 = CARTESIAN_POINT ( 'NONE',  ( 4.956653778116966613, 0.000000000000000000, 0.000000000000000000 ) ) ;
#20030 = CARTESIAN_POINT ( 'NONE',  ( -6.016761891674564211, 14.94721834528430371, -11.47373234755488092 ) ) ;
#20031 = ORIENTED_EDGE ( 'NONE', *, *, #33478, .F. ) ;
#20032 = CARTESIAN_POINT ( 'NONE',  ( 1.231276596079881935, -40.90292846002442673, -9.177538581351248226 ) ) ;
#20033 = ORIENTED_EDGE ( 'NONE', *, *, #3223, .F. ) ;
#20034 = CARTESIAN_POINT ( 'NONE',  ( 0.1119899015040011631, -42.82020505619818351, 10.64853732386031915 ) ) ;
#20035 = CARTESIAN_POINT ( 'NONE',  ( 0.6026112563231247332, -19.71849761537919932, -44.97468006219157388 ) ) ;
#20036 = FACE_OUTER_BOUND ( 'NONE', #22458, .T. ) ;
#20037 = CARTESIAN_POINT ( 'NONE',  ( 5.960221823109900008, -2.684531185214569238, 20.34928172836725935 ) ) ;
#20038 = CARTESIAN_POINT ( 'NONE',  ( -6.078075953587585900, 19.09862890096249544, 2.457142313838565961 ) ) ;
#20039 = CARTESIAN_POINT ( 'NONE',  ( 0.6029443199889047422, 37.39262245022165132, -31.83283569130437130 ) ) ;
#20040 = CARTESIAN_POINT ( 'NONE',  ( 0.3622758884714730732, 22.26738722580116558, 36.91764744403329246 ) ) ;
#20041 = EDGE_CURVE ( 'NONE', #8823, #3829, #29367, .T. ) ;
#20042 = CARTESIAN_POINT ( 'NONE',  ( 4.335381028904201628, -5.712845112847932505, -48.65306001045518514 ) ) ;
#20043 = CARTESIAN_POINT ( 'NONE',  ( 0.5980894510889457338, 46.28687279963691736, -13.12879507229240161 ) ) ;
#20044 = CARTESIAN_POINT ( 'NONE',  ( 0.8744876279028306332, 3.827863332835647281, -48.94586308039347955 ) ) ;
#20045 = ADVANCED_FACE ( 'NONE', ( #50370 ), #16031, .F. ) ;
#20046 = CARTESIAN_POINT ( 'NONE',  ( 0.9783242366443545279, -34.70225378719274545, 23.49655447710985001 ) ) ;
#20047 = CARTESIAN_POINT ( 'NONE',  ( 0.5807400328401637335, -47.89582301953902999, -0.5448834511095090871 ) ) ;
#20048 = ORIENTED_EDGE ( 'NONE', *, *, #55087, .T. ) ;
#20049 = CARTESIAN_POINT ( 'NONE',  ( 4.975610109902397937, 0.000000000000000000, 0.000000000000000000 ) ) ;
#20050 = AXIS2_PLACEMENT_3D ( 'NONE', #44408, #5215, #23186 ) ;
#20051 = CARTESIAN_POINT ( 'NONE',  ( 4.553261556744873317, -39.67390170502044100, -18.85526688551536623 ) ) ;
#20052 = CARTESIAN_POINT ( 'NONE',  ( 0.5800708057587374844, 47.40012370174866874, 6.873290064481538231 ) ) ;
#20053 = CARTESIAN_POINT ( 'NONE',  ( 4.956445790444001354, -28.36659270909979114, 37.58822246682706947 ) ) ;
#20054 = ORIENTED_EDGE ( 'NONE', *, *, #24473, .T. ) ;
#20055 = EDGE_CURVE ( 'NONE', #61884, #42948, #45733, .T. ) ;
#20056 = CARTESIAN_POINT ( 'NONE',  ( 4.975801465491695552, 0.000000000000000000, 0.000000000000000000 ) ) ;
#20057 = DIRECTION ( 'NONE',  ( 1.000000000000000000, 1.836909530733573776E-16, -1.925929944387235853E-32 ) ) ;
#20058 = B_SPLINE_CURVE_WITH_KNOTS ( 'NONE', 3,
 ( #4801, #61815, #52737, #14861, #19560, #38676 ),
 .UNSPECIFIED., .F., .F.,
 ( 4, 2, 4 ),
 ( 8.471125239557413953E-17, 0.0002293366620881436566, 0.0004586733241762026370 ),
 .UNSPECIFIED. ) ;
#20059 = CARTESIAN_POINT ( 'NONE',  ( 1.157644175074338699, 38.26069983002199137, 17.12078047275106485 ) ) ;
#20060 =( BOUNDED_SURFACE ( )  B_SPLINE_SURFACE ( 3, 1, ( 
 ( #42583, #37902 ),
 ( #56959, #23455 ),
 ( #9046, #38504 ),
 ( #57557, #52884 ) ),
 .UNSPECIFIED., .F., .F., .F. ) 
 B_SPLINE_SURFACE_WITH_KNOTS ( ( 4, 4 ),
 ( 2, 2 ),
 ( 0.000000000000000000, 1.000000000000000000 ),
 ( 0.000000000000000000, 1.000000000000000000 ),
 .UNSPECIFIED. ) 
 GEOMETRIC_REPRESENTATION_ITEM ( )  RATIONAL_B_SPLINE_SURFACE ( (
 ( 1.000000000000000000, 1.000000000000000000),
 ( 0.9952954269826590483, 0.8620686068821307169),
 ( 0.9952954269826590483, 0.8620686068821307169),
 ( 1.000000000000000000, 1.000000000000000000) ) ) 
 REPRESENTATION_ITEM ( '' )  SURFACE ( )  );
#20061 = VERTEX_POINT ( 'NONE', #19047 ) ;
#20062 = CARTESIAN_POINT ( 'NONE',  ( -2.601141883200662974, -14.31801740503249931, 4.217796232462521111 ) ) ;
#20063 = FACE_OUTER_BOUND ( 'NONE', #61938, .T. ) ;
#20064 = VERTEX_POINT ( 'NONE', #56607 ) ;
#20065 = B_SPLINE_CURVE_WITH_KNOTS ( 'NONE', 3,
 ( #25806, #59001, #48382, #14892, #33998, #53982, #39016, #25489, #11107, #30190, #58677, #53071, #6052, #762, #15495, #24581, #44627, #39943, #20807, #1359, #44329, #11406, #16111, #29578, #49602 ),
 .UNSPECIFIED., .F., .F.,
 ( 4, 3, 3, 3, 3, 3, 3, 3, 4 ),
 ( 5.057544569639794935E-18, 0.0005656085177311390979, 0.001131215744874498972, 0.001696821861372765482, 0.002262427090022497284, 0.002828031679238745058, 0.003393635864401603561, 0.003977030878808130755, 0.004561030005651157265 ),
 .UNSPECIFIED. ) ;
#20066 = CARTESIAN_POINT ( 'NONE',  ( 0.9762797500689124330, -26.66896101499549587, -32.32787193067855469 ) ) ;
#20067 = EDGE_LOOP ( 'NONE', ( #31536, #42599, #8054, #8633 ) ) ;
#20068 = CARTESIAN_POINT ( 'NONE',  ( 0.5806925824938502512, -25.69265091979982429, -39.23149310256842170 ) ) ;
#20069 = ORIENTED_EDGE ( 'NONE', *, *, #41420, .F. ) ;
#20070 = CARTESIAN_POINT ( 'NONE',  ( 0.1129192098497447394, -13.01845098534572820, -42.16007260106777466 ) ) ;
#20071 = CARTESIAN_POINT ( 'NONE',  ( 0.7954196712028462901, -28.58653687859139225, -38.68220069891160051 ) ) ;
#20072 = ORIENTED_EDGE ( 'NONE', *, *, #52661, .F. ) ;
#20073 = CARTESIAN_POINT ( 'NONE',  ( 4.956445790444004018, -47.08764048036452721, -0.5405220916603282744 ) ) ;
#20074 = ORIENTED_EDGE ( 'NONE', *, *, #52156, .F. ) ;
#20075 = FACE_OUTER_BOUND ( 'NONE', #57600, .T. ) ;
#20076 = DIRECTION ( 'NONE',  ( -0.1024043820194934507, -0.9139094329506576297, -0.3927886084231733688 ) ) ;
#20077 = LINE ( 'NONE', #28837, #19860 ) ;
#20078 = ADVANCED_FACE ( 'NONE', ( #38158 ), #22424, .F. ) ;
#20079 = ORIENTED_EDGE ( 'NONE', *, *, #54314, .T. ) ;
#20080 = FACE_OUTER_BOUND ( 'NONE', #30366, .T. ) ;
#20081 = CARTESIAN_POINT ( 'NONE',  ( 0.5839879327111923146, 33.80333292213305896, -33.93179405280454120 ) ) ;
#20082 = CARTESIAN_POINT ( 'NONE',  ( 3.661921753702006566, -39.81514960208500042, -25.04765430130383308 ) ) ;
#20083 = CARTESIAN_POINT ( 'NONE',  ( 4.975801465491694664, -47.76942479135482955, -3.702618843597289544 ) ) ;
#20084 = ORIENTED_EDGE ( 'NONE', *, *, #20858, .T. ) ;
#20085 = FACE_OUTER_BOUND ( 'NONE', #21367, .T. ) ;
#20086 = CARTESIAN_POINT ( 'NONE',  ( 0.5998501479064708430, -12.95623334615534716, 46.33007877220716608 ) ) ;
#20087 = ORIENTED_EDGE ( 'NONE', *, *, #19749, .F. ) ;
#20088 = CARTESIAN_POINT ( 'NONE',  ( 0.5830082357119563685, -46.77220610048276939, -3.404815917535003233 ) ) ;
#20089 = EDGE_CURVE ( 'NONE', #33107, #26859, #38392, .T. ) ;
#20090 = EDGE_LOOP ( 'NONE', ( #32598, #5072, #36358, #49264 ) ) ;
#20091 = VECTOR ( 'NONE', #27800, 1000.000000000000000 ) ;
#20092 = DIRECTION ( 'NONE',  ( 0.000000000000000000, 0.000000000000000000, -1.000000000000000000 ) ) ;
#20093 = CARTESIAN_POINT ( 'NONE',  ( 0.9790724872846782167, 40.43026749430960365, -11.03307211614352745 ) ) ;
#20094 = ORIENTED_EDGE ( 'NONE', *, *, #26212, .T. ) ;
#20095 = LINE ( 'NONE', #53269, #39597 ) ;
#20096 = CARTESIAN_POINT ( 'NONE',  ( 0.6254087463353935616, 37.74264085326059615, -29.82831063981293340 ) ) ;
#20097 = EDGE_CURVE ( 'NONE', #47245, #30566, #24703, .T. ) ;
#20098 = CARTESIAN_POINT ( 'NONE',  ( 0.8560838555295223751, 39.88643293834682879, -24.68694597426934223 ) ) ;
#20099 = CARTESIAN_POINT ( 'NONE',  ( 0.5806925824938499181, -38.96949031362449745, 26.08833430941674436 ) ) ;
#20100 = ORIENTED_EDGE ( 'NONE', *, *, #36442, .T. ) ;
#20101 = CARTESIAN_POINT ( 'NONE',  ( 0.5998501479064708430, 18.89267974119668025, -44.24259072156067418 ) ) ;
#20102 = CARTESIAN_POINT ( 'NONE',  ( 0.5809828226811553087, -44.45562576850588243, -17.82437196699728332 ) ) ;
#20103 = FACE_OUTER_BOUND ( 'NONE', #26777, .T. ) ;
#20104 = CARTESIAN_POINT ( 'NONE',  ( 1.231276596079887264, 20.88402890667827450, 36.34740854095507245 ) ) ;
#20105 = CARTESIAN_POINT ( 'NONE',  ( 4.553261556744875094, -9.554252317234240621, -42.87488575474295516 ) ) ;
#20106 = EDGE_CURVE ( 'NONE', #12273, #61654, #14700, .T. ) ;
#20107 = DIRECTION ( 'NONE',  ( -1.000000000000000000, -0.000000000000000000, -0.000000000000000000 ) ) ;
#20108 = CARTESIAN_POINT ( 'NONE',  ( -15.87375730239583937, -7.999984958122236200, 0.1385333841346340356 ) ) ;
#20109 = ADVANCED_FACE ( 'NONE', ( #57205 ), #18049, .F. ) ;
#20110 = DIRECTION ( 'NONE',  ( 0.000000000000000000, 0.000000000000000000, 1.000000000000000000 ) ) ;
#20111 = CARTESIAN_POINT ( 'NONE',  ( 0.7044674535452954967, 32.38853019898860452, 36.91592927667010571 ) ) ;
#20112 = B_SPLINE_CURVE_WITH_KNOTS ( 'NONE', 3,
 ( #28179, #27567, #32590, #31654, #42005, #46691 ),
 .UNSPECIFIED., .F., .F.,
 ( 4, 2, 4 ),
 ( 8.559238840292261462E-17, 0.0002293366620881445782, 0.0004586733241762035586 ),
 .UNSPECIFIED. ) ;
#20113 = CARTESIAN_POINT ( 'NONE',  ( 0.5806925824938499181, -19.24316026636448029, -42.76591101925195204 ) ) ;
#20114 = FACE_OUTER_BOUND ( 'NONE', #51023, .T. ) ;
#20115 = CARTESIAN_POINT ( 'NONE',  ( 0.5824936645240087474, -1.931019941530967454, 46.85626255929636841 ) ) ;
#20116 = ADVANCED_FACE ( 'NONE', ( #33448 ), #18721, .F. ) ;
#20117 = CARTESIAN_POINT ( 'NONE',  ( 0.5839879882012681822, 33.86758487442402554, 33.86754218494311175 ) ) ;
#20118 = CARTESIAN_POINT ( 'NONE',  ( 0.9762797500689124330, -37.62962005162893320, -18.44821075215020656 ) ) ;
#20119 = ORIENTED_EDGE ( 'NONE', *, *, #43840, .F. ) ;
#20120 = DIRECTION ( 'NONE',  ( 0.000000000000000000, 0.000000000000000000, 1.000000000000000000 ) ) ;
#20121 = CARTESIAN_POINT ( 'NONE',  ( 0.9775691876210974574, -1.777855953716244608, 41.87090800541382407 ) ) ;
#20122 = FACE_OUTER_BOUND ( 'NONE', #20811, .T. ) ;
#20123 = ORIENTED_EDGE ( 'NONE', *, *, #34798, .T. ) ;
#20124 = EDGE_CURVE ( 'NONE', #41574, #25523, #33164, .T. ) ;
#20125 = LINE ( 'NONE', #15113, #1281 ) ;
#20126 = CARTESIAN_POINT ( 'NONE',  ( 1.479689385636123067, 26.16456136252788767, 35.45418979435581974 ) ) ;
#20127 = B_SPLINE_CURVE_WITH_KNOTS ( 'NONE', 3,
 ( #54944, #12078, #30840, #50260 ),
 .UNSPECIFIED., .F., .F.,
 ( 4, 4 ),
 ( 0.000000000000000000, 0.004447772540403824131 ),
 .UNSPECIFIED. ) ;
#20129 = ORIENTED_EDGE ( 'NONE', *, *, #18124, .F. ) ;
#20128 = AXIS2_PLACEMENT_3D ( 'NONE', #20411, #7210, #20720 ) ;
#20130 = ORIENTED_EDGE ( 'NONE', *, *, #56551, .T. ) ;
#20131 = CARTESIAN_POINT ( 'NONE',  ( 0.5807400328401637335, -38.33001520688971198, 28.72484455891626709 ) ) ;
#20133 = VERTEX_POINT ( 'NONE', #195 ) ;
#20132 =( BOUNDED_SURFACE ( )  B_SPLINE_SURFACE ( 3, 1, ( 
 ( #40304, #31483 ),
 ( #35591, #11159 ),
 ( #54651, #2969 ),
 ( #49977, #25547 ) ),
 .UNSPECIFIED., .F., .F., .F. ) 
 B_SPLINE_SURFACE_WITH_KNOTS ( ( 4, 4 ),
 ( 2, 2 ),
 ( 0.000000000000000000, 1.000000000000000000 ),
 ( 0.000000000000000000, 1.000000000000000000 ),
 .UNSPECIFIED. ) 
 GEOMETRIC_REPRESENTATION_ITEM ( )  RATIONAL_B_SPLINE_SURFACE ( (
 ( 1.000000000000000000, 1.000000000000000000),
 ( 0.9953485035131437453, 0.8621029689291515030),
 ( 0.9953485035131437453, 0.8621029689291515030),
 ( 1.000000000000000000, 1.000000000000000000) ) ) 
 REPRESENTATION_ITEM ( '' )  SURFACE ( )  );
#20134 = CARTESIAN_POINT ( 'NONE',  ( 5.959547316686252039, -12.49803383497738807, -16.28190225198614627 ) ) ;
#20135 = ORIENTED_EDGE ( 'NONE', *, *, #34172, .T. ) ;
#20136 = ORIENTED_EDGE ( 'NONE', *, *, #25688, .F. ) ;
#20137 = FACE_OUTER_BOUND ( 'NONE', #18511, .T. ) ;
#20138 = ORIENTED_EDGE ( 'NONE', *, *, #49010, .T. ) ;
#20139 = CARTESIAN_POINT ( 'NONE',  ( 0.5848930533535030563, -46.77916419324616015, -3.314042813373960339 ) ) ;
#20140 = DIRECTION ( 'NONE',  ( 0.000000000000000000, 0.000000000000000000, -1.000000000000000000 ) ) ;
#20141 = CARTESIAN_POINT ( 'NONE',  ( -6.016761891674564211, 16.32039929810256851, 9.418621820384554866 ) ) ;
#20142 = ORIENTED_EDGE ( 'NONE', *, *, #45446, .F. ) ;
#20143 = CARTESIAN_POINT ( 'NONE',  ( 3.270143674763207553, -0.2742231296308566546, -13.68510027222513692 ) ) ;
#20144 = PLANE ( 'NONE',  #36011 ) ;
#20145 = ORIENTED_EDGE ( 'NONE', *, *, #22957, .T. ) ;
#20146 = EDGE_LOOP ( 'NONE', ( #5183, #34473, #44969, #59811 ) ) ;
#20147 =( BOUNDED_SURFACE ( )  B_SPLINE_SURFACE ( 3, 1, ( 
 ( #1550, #25686 ),
 ( #20992, #6861 ),
 ( #49802, #53254 ),
 ( #29453, #5618 ) ),
 .UNSPECIFIED., .F., .F., .F. ) 
 B_SPLINE_SURFACE_WITH_KNOTS ( ( 4, 4 ),
 ( 2, 2 ),
 ( 0.000000000000000000, 1.000000000000000000 ),
 ( 0.000000000000000000, 1.000000000000000000 ),
 .UNSPECIFIED. ) 
 GEOMETRIC_REPRESENTATION_ITEM ( )  RATIONAL_B_SPLINE_SURFACE ( (
 ( 1.000000000000000000, 1.000000000000000000),
 ( 0.9729067724841187204, 0.9999501103223794596),
 ( 0.9729067724841187204, 0.9999501103223794596),
 ( 1.000000000000000000, 1.000000000000000000) ) ) 
 REPRESENTATION_ITEM ( '' )  SURFACE ( )  );
#20148 = CARTESIAN_POINT ( 'NONE',  ( 0.1156495703730067437, 43.28422450877429384, -8.568480723272513089 ) ) ;
#20149 = CARTESIAN_POINT ( 'NONE',  ( 48.39340508532479390, 12.39581920280924088, 1.616942749076695662 ) ) ;
#20150 = CARTESIAN_POINT ( 'NONE',  ( 0.1087620492084205581, -30.74858804150707670, 30.23658359364767989 ) ) ;
#20151 = CARTESIAN_POINT ( 'NONE',  ( 5.960721111146673579, -16.28787783074218964, -12.49016043756465422 ) ) ;
#20152 = EDGE_CURVE ( 'NONE', #27210, #14390, #50999, .T. ) ;
#20153 =( BOUNDED_SURFACE ( )  B_SPLINE_SURFACE ( 3, 1, ( 
 ( #4951, #56962 ),
 ( #33496, #9049 ),
 ( #43518, #52572 ),
 ( #9665, #24385 ) ),
 .UNSPECIFIED., .F., .F., .F. ) 
 B_SPLINE_SURFACE_WITH_KNOTS ( ( 4, 4 ),
 ( 2, 2 ),
 ( 0.000000000000000000, 1.000000000000000000 ),
 ( 0.000000000000000000, 1.000000000000000000 ),
 .UNSPECIFIED. ) 
 GEOMETRIC_REPRESENTATION_ITEM ( )  RATIONAL_B_SPLINE_SURFACE ( (
 ( 1.000000000000000000, 1.000000000000000000),
 ( 0.9952954269826590483, 0.8620686068821307169),
 ( 0.9952954269826590483, 0.8620686068821307169),
 ( 1.000000000000000000, 1.000000000000000000) ) ) 
 REPRESENTATION_ITEM ( '' )  SURFACE ( )  );
#20154 = ORIENTED_EDGE ( 'NONE', *, *, #58457, .F. ) ;
#20155 = CARTESIAN_POINT ( 'NONE',  ( 4.553261556744875094, 0.000000000000000000, 0.000000000000000000 ) ) ;
#20156 = CARTESIAN_POINT ( 'NONE',  ( 0.6064782688330868643, 46.56801696588680528, -5.545650753847469971 ) ) ;
#20157 = ADVANCED_FACE ( 'NONE', ( #33757 ), #50051, .F. ) ;
#20158 = CARTESIAN_POINT ( 'NONE',  ( -6.079354080745853928, -6.649248899792496559, 18.07153685541909027 ) ) ;
#20159 = FACE_OUTER_BOUND ( 'NONE', #50724, .T. ) ;
#20160 = ORIENTED_EDGE ( 'NONE', *, *, #22290, .T. ) ;
#20161 = FACE_OUTER_BOUND ( 'NONE', #30710, .T. ) ;
#20162 = DIRECTION ( 'NONE',  ( -1.000000000000000000, -0.000000000000000000, -0.000000000000000000 ) ) ;
#20163 = EDGE_CURVE ( 'NONE', #21722, #54914, #11700, .T. ) ;
#20164 = CARTESIAN_POINT ( 'NONE',  ( -6.078726893082806448, 9.985094725776445301, -16.46486940689149137 ) ) ;
#20165 = CARTESIAN_POINT ( 'NONE',  ( 1.000433927950263646, 41.90447303099593057, -0.6586483488038954448 ) ) ;
#20166 = ORIENTED_EDGE ( 'NONE', *, *, #22301, .F. ) ;
#20167 = VERTEX_POINT ( 'NONE', #58137 ) ;
#20168 = CARTESIAN_POINT ( 'NONE',  ( 2.624215991343620935, -38.92973006074493725, -28.09277600149258447 ) ) ;
#20169 = FACE_OUTER_BOUND ( 'NONE', #8875, .T. ) ;
#20170 = CARTESIAN_POINT ( 'NONE',  ( 4.549368137175248350, -38.40568845698290801, 19.17571786012255686 ) ) ;
#20171 = CARTESIAN_POINT ( 'NONE',  ( 4.956445790444035104, 35.28522167764516837, -31.18479086508480691 ) ) ;
#20172 = B_SPLINE_CURVE_WITH_KNOTS ( 'NONE', 3,
 ( #13318, #50578, #17390, #51813, #37137, #22703 ),
 .UNSPECIFIED., .F., .F.,
 ( 4, 2, 4 ),
 ( 8.510565793060200234E-17, 0.0002293366620881444426, 0.0004586733241762037754 ),
 .UNSPECIFIED. ) ;
#20173 = VECTOR ( 'NONE', #18451, 999.9999999999998863 ) ;
#20174 = CARTESIAN_POINT ( 'NONE',  ( 0.1129192098497447394, 15.69290830752478882, 41.23935519181615206 ) ) ;
#20175 = CARTESIAN_POINT ( 'NONE',  ( 4.967162193818130511, 0.000000000000000000, 0.000000000000000000 ) ) ;
#20176 = CARTESIAN_POINT ( 'NONE',  ( 0.8744876279028306332, -19.05609938969034545, 45.24616145519679122 ) ) ;
#20177 = CARTESIAN_POINT ( 'NONE',  ( 0.9730545539215883499, 37.40983423658502716, -21.01499094264509893 ) ) ;
#20178 = CARTESIAN_POINT ( 'NONE',  ( 0.5807400328401574052, -37.66660715020886840, 29.58941477093001993 ) ) ;
#20179 = EDGE_CURVE ( 'NONE', #51998, #57230, #39696, .T. ) ;
#20180 = CARTESIAN_POINT ( 'NONE',  ( 0.6031356755773454870, -18.40994522247727971, -44.44547243635314970 ) ) ;
#20181 = B_SPLINE_CURVE_WITH_KNOTS ( 'NONE', 3,
 ( #48753, #16175, #1732, #44399, #57824, #1425 ),
 .UNSPECIFIED., .F., .F.,
 ( 4, 2, 4 ),
 ( 9.745765416140531346E-18, 0.0002291978881530162685, 0.0004583957763060227792 ),
 .UNSPECIFIED. ) ;
#20182 = CARTESIAN_POINT ( 'NONE',  ( 2.500000000000000000, 2.357898499370431722, -2.818925648462311528E-15 ) ) ;
#20183 = ORIENTED_EDGE ( 'NONE', *, *, #46704, .F. ) ;
#20184 = ADVANCED_FACE ( 'NONE', ( #58438 ), #53684, .F. ) ;
#20185 = CARTESIAN_POINT ( 'NONE',  ( 0.3676999524040323597, -42.87209381266892194, 10.38913641457044434 ) ) ;
#20186 = CARTESIAN_POINT ( 'NONE',  ( 0.6000166863083090663, 23.17738933882538177, -43.29702189694987879 ) ) ;
#20187 = CARTESIAN_POINT ( 'NONE',  ( 5.895596859100789899, -15.78235929336518950, -12.46777118604672197 ) ) ;
#20188 = CARTESIAN_POINT ( 'NONE',  ( 0.6027935024548037868, -24.20473723001725830, 41.57475399306878217 ) ) ;
#20189 = CARTESIAN_POINT ( 'NONE',  ( 0.5838002273316419410, -41.54704836736068074, 23.82993264414549373 ) ) ;
#20190 = LINE ( 'NONE', #30176, #44700 ) ;
#20191 = ITEM_DEFINED_TRANSFORMATION ( 'NONE', 'NONE', #42923,  #14677 ) ;
#20192 = CARTESIAN_POINT ( 'NONE',  ( 4.553261556744875094, -15.38244134641827898, 41.14510984366961566 ) ) ;
#20193 = ADVANCED_FACE ( 'NONE', ( #19967 ), #47733, .F. ) ;
#20194 = CARTESIAN_POINT ( 'NONE',  ( 4.962356264823608143, -15.53171314616189846, 39.11523340857994668 ) ) ;
#20195 = FACE_OUTER_BOUND ( 'NONE', #57817, .T. ) ;
#20196 = CARTESIAN_POINT ( 'NONE',  ( 1.000110580585050979, -27.55712950893854440, 31.57565669941787689 ) ) ;
#20198 = ORIENTED_EDGE ( 'NONE', *, *, #14134, .F. ) ;
#20197 = CARTESIAN_POINT ( 'NONE',  ( 0.9730545539215883499, 10.61654491617563423, 41.57420493492389113 ) ) ;
#20199 = ORIENTED_EDGE ( 'NONE', *, *, #29909, .F. ) ;
#20200 = CARTESIAN_POINT ( 'NONE',  ( 0.8554163680231738898, -46.15020320557310640, 8.447734441619829227 ) ) ;
#20201 = CARTESIAN_POINT ( 'NONE',  ( 0.1119898979215350615, -43.83035652836955620, -5.085386401035962400 ) ) ;
#20202 = CARTESIAN_POINT ( 'NONE',  ( 1.231276596079887264, -34.07446381689716475, 24.41736444846234733 ) ) ;
#20203 = EDGE_CURVE ( 'NONE', #38470, #17692, #25595, .T. ) ;
#20204 = EDGE_LOOP ( 'NONE', ( #45252, #10661, #41242, #22769 ) ) ;
#20205 = CARTESIAN_POINT ( 'NONE',  ( 4.967162193818130511, 23.56777426397228936, -36.06913038482774425 ) ) ;
#20206 = CARTESIAN_POINT ( 'NONE',  ( 1.827119703190778877, -15.32887915442621818, 40.22835835992437836 ) ) ;
#20207 = CARTESIAN_POINT ( 'NONE',  ( 5.974727161628367256, 7.868887636447348122, 18.95664195401520402 ) ) ;
#20208 = B_SPLINE_CURVE_WITH_KNOTS ( 'NONE', 3,
 ( #50332, #35960, #50945, #45659, #36570, #3022 ),
 .UNSPECIFIED., .F., .F.,
 ( 4, 2, 4 ),
 ( 1.097135458930219133E-17, 0.0002291978881530148590, 0.0004583957763060187134 ),
 .UNSPECIFIED. ) ;
#20209 = EDGE_LOOP ( 'NONE', ( #23883, #26729, #30987, #4315 ) ) ;
#20210 = ORIENTED_EDGE ( 'NONE', *, *, #33178, .T. ) ;
#20211 = CARTESIAN_POINT ( 'NONE',  ( 5.895881250540457863, 18.99851645375302311, -6.601822033709823678 ) ) ;
#20212 = FACE_OUTER_BOUND ( 'NONE', #60814, .T. ) ;
#20213 = CARTESIAN_POINT ( 'NONE',  ( 4.833616638992205949, -15.29495699393755359, 43.64812679991092637 ) ) ;
#20214 = CARTESIAN_POINT ( 'NONE',  ( 0.5824935313925946323, 16.51437437898027838, -43.89206780187871715 ) ) ;
#20215 = CARTESIAN_POINT ( 'NONE',  ( 0.9780303403264777318, -41.13220516101565494, -8.030025652960466331 ) ) ;
#20216 = CIRCLE ( 'NONE', #45267, 9.500000000000000000 ) ;
#20217 = CARTESIAN_POINT ( 'NONE',  ( 5.901463166500146684, 18.99503018386013053, -6.611104193315902045 ) ) ;
#20218 = CARTESIAN_POINT ( 'NONE',  ( 0.9756354156337463390, 42.52418499698895005, 5.729847988735494724 ) ) ;
#20219 = VERTEX_POINT ( 'NONE', #5812 ) ;
#20220 = VERTEX_POINT ( 'NONE', #20269 ) ;
#20221 = CARTESIAN_POINT ( 'NONE',  ( 4.549368137175248350, 42.14271863032833920, -8.166781970325278195 ) ) ;
#20222 = CARTESIAN_POINT ( 'NONE',  ( 2.643462169533613793, -22.81120928486525301, 42.27470921730900244 ) ) ;
#20223 = ORIENTED_EDGE ( 'NONE', *, *, #36242, .T. ) ;
#20224 = CARTESIAN_POINT ( 'NONE',  ( -5.272380000000000067, 0.000000000000000000, 0.000000000000000000 ) ) ;
#20225 = CARTESIAN_POINT ( 'NONE',  ( 0.7245667037590763915, 44.74806999162964871, 17.64710816761277812 ) ) ;
#20226 = CARTESIAN_POINT ( 'NONE',  ( 0.1149546198390367369, -40.79590554332651209, -16.81192005462792949 ) ) ;
#20227 = EDGE_CURVE ( 'NONE', #31789, #5687, #26373, .T. ) ;
#20228 = ORIENTED_EDGE ( 'NONE', *, *, #60760, .F. ) ;
#20229 = CARTESIAN_POINT ( 'NONE',  ( 0.8744876279028306332, 48.92939099258504143, -4.032957658373305776 ) ) ;
#20230 = CARTESIAN_POINT ( 'NONE',  ( 0.6001305935487422083, -44.24520387813817024, -18.89378601236048283 ) ) ;
#20231 = EDGE_CURVE ( 'NONE', #26754, #57580, #34070, .T. ) ;
#20232 = DIRECTION ( 'NONE',  ( 0.07500201931887538753, 0.4319596767211368871, -0.8987688995426253991 ) ) ;
#20233 =( BOUNDED_SURFACE ( )  B_SPLINE_SURFACE ( 3, 1, ( 
 ( #2198, #12569 ),
 ( #46092, #22265 ),
 ( #54831, #60448 ),
 ( #31042, #7841 ) ),
 .UNSPECIFIED., .F., .F., .F. ) 
 B_SPLINE_SURFACE_WITH_KNOTS ( ( 4, 4 ),
 ( 2, 2 ),
 ( 0.000000000000000000, 1.000000000000000000 ),
 ( 0.000000000000000000, 1.000000000000000000 ),
 .UNSPECIFIED. ) 
 GEOMETRIC_REPRESENTATION_ITEM ( )  RATIONAL_B_SPLINE_SURFACE ( (
 ( 1.000000000000000000, 1.000000000000000000),
 ( 0.9729067724841187204, 0.9999501103223794596),
 ( 0.9729067724841187204, 0.9999501103223794596),
 ( 1.000000000000000000, 1.000000000000000000) ) ) 
 REPRESENTATION_ITEM ( '' )  SURFACE ( )  );
#20234 = CARTESIAN_POINT ( 'NONE',  ( -5.440000000000003055, 15.43999999999999950, 0.000000000000000000 ) ) ;
#20235 = ORIENTED_EDGE ( 'NONE', *, *, #8999, .F. ) ;
#20236 = CARTESIAN_POINT ( 'NONE',  ( 0.7762777257811899201, -46.49451973287609263, 11.53708189756924618 ) ) ;
#20238 = ORIENTED_EDGE ( 'NONE', *, *, #54998, .T. ) ;
#20237 = EDGE_CURVE ( 'NONE', #49382, #9581, #59065, .T. ) ;
#20239 = CARTESIAN_POINT ( 'NONE',  ( -5.995132425357893702, 9.429450169547955340, 16.31525984181036293 ) ) ;
#20240 = CARTESIAN_POINT ( 'NONE',  ( 0.5839880159502340851, 23.98728323041108013, -41.45643525694580944 ) ) ;
#20241 = EDGE_CURVE ( 'NONE', #22663, #3284, #166, .T. ) ;
#20242 =( BOUNDED_SURFACE ( )  B_SPLINE_SURFACE ( 3, 1, ( 
 ( #46649, #41044 ),
 ( #3693, #60107 ),
 ( #37254, #17213 ),
 ( #36334, #31611 ) ),
 .UNSPECIFIED., .F., .F., .F. ) 
 B_SPLINE_SURFACE_WITH_KNOTS ( ( 4, 4 ),
 ( 2, 2 ),
 ( 0.000000000000000000, 1.000000000000000000 ),
 ( 0.000000000000000000, 1.000000000000000000 ),
 .UNSPECIFIED. ) 
 GEOMETRIC_REPRESENTATION_ITEM ( )  RATIONAL_B_SPLINE_SURFACE ( (
 ( 1.000000000000000000, 1.000000000000000000),
 ( 0.9953390228620291325, 0.8624445117760984880),
 ( 0.9953390228620291325, 0.8624445117760984880),
 ( 1.000000000000000000, 1.000000000000000000) ) ) 
 REPRESENTATION_ITEM ( '' )  SURFACE ( )  );
#20243 = VERTEX_POINT ( 'NONE', #1132 ) ;
#20244 = CARTESIAN_POINT ( 'NONE',  ( 0.5998501479064699549, -5.759754759341138453, 47.76154736470748219 ) ) ;
#20245 = EDGE_CURVE ( 'NONE', #35307, #35477, #9712, .T. ) ;
#20246 = CARTESIAN_POINT ( 'NONE',  ( 0.8760168074886965917, -42.09738177923971136, 23.27577685234524196 ) ) ;
#20247 = CARTESIAN_POINT ( 'NONE',  ( 0.2230388203127610935, -22.21453373073364546, -36.95676097786368786 ) ) ;
#20248 = B_SPLINE_CURVE_WITH_KNOTS ( 'NONE', 3,
 ( #12604, #41730, #31694, #22297 ),
 .UNSPECIFIED., .F., .F.,
 ( 4, 4 ),
 ( 0.002122961284640939757, 0.004442905043737215703 ),
 .UNSPECIFIED. ) ;
#20249 = CARTESIAN_POINT ( 'NONE',  ( -6.010958268070873523, 18.84344976839986785, 0.01451635840169903692 ) ) ;
#20250 = DIRECTION ( 'NONE',  ( 1.000000000000000000, 0.000000000000000000, 0.000000000000000000 ) ) ;
#20251 = CARTESIAN_POINT ( 'NONE',  ( 0.8560838555295223751, 45.47430759461099115, 11.50913475776684791 ) ) ;
#20252 = EDGE_CURVE ( 'NONE', #38956, #25747, #38497, .T. ) ;
#20253 = CARTESIAN_POINT ( 'NONE',  ( 0.1073791018717483448, -21.14095454447585709, 37.58707531572169813 ) ) ;
#20254 = CARTESIAN_POINT ( 'NONE',  ( 5.000000000000007994, -56.56854249492331377, -56.56854249492430142 ) ) ;
#20255 = ORIENTED_EDGE ( 'NONE', *, *, #46945, .T. ) ;
#20256 = CARTESIAN_POINT ( 'NONE',  ( 50.15577769773999961, 0.000000000000000000, 0.000000000000000000 ) ) ;
#20257 = EDGE_CURVE ( 'NONE', #44894, #3092, #17466, .T. ) ;
#20258 = CARTESIAN_POINT ( 'NONE',  ( 4.549368137175248350, -32.13400537129945178, 28.46244473166616729 ) ) ;
#20259 = CARTESIAN_POINT ( 'NONE',  ( 0.9780303403264755113, 15.36406718167910945, 38.99083293585732690 ) ) ;
#20260 = VERTEX_POINT ( 'NONE', #20564 ) ;
#20261 = CARTESIAN_POINT ( 'NONE',  ( 0.5786265663353153954, -5.535668456754276434, 47.58023467411537410 ) ) ;
#20262 = CARTESIAN_POINT ( 'NONE',  ( 4.956445790444006683, -32.34643101787064978, -34.22347806032829709 ) ) ;
#20263 = CARTESIAN_POINT ( 'NONE',  ( 0.6026777506516368677, 22.86838944615219305, 43.45783191527546307 ) ) ;
#20264 = CARTESIAN_POINT ( 'NONE',  ( 0.8554163680231708922, -45.78608427674268455, -10.23913862172187628 ) ) ;
#20265 = CARTESIAN_POINT ( 'NONE',  ( 0.6029443199889047422, -19.87783894042105715, 44.90444477903142229 ) ) ;
#20266 = DIRECTION ( 'NONE',  ( 0.07836865515943411409, -0.9240274869783839939, 0.3742079063794805371 ) ) ;
#20267 = DIRECTION ( 'NONE',  ( 1.468930164684295977E-18, -0.003998373736177452710, -0.9999920064717846557 ) ) ;
#20268 = CARTESIAN_POINT ( 'NONE',  ( 5.896782393890504181, -11.92541098582113612, -16.19600752337651883 ) ) ;
#20269 = CARTESIAN_POINT ( 'NONE',  ( 1.231276596079881047, -27.70544295162376258, 31.45926257674180704 ) ) ;
#20270 = CARTESIAN_POINT ( 'NONE',  ( 45.00000000000001421, 9.184850993605151889E-15, -75.00000000000001421 ) ) ;
#20272 = ORIENTED_EDGE ( 'NONE', *, *, #56624, .F. ) ;
#20271 = CARTESIAN_POINT ( 'NONE',  ( -2.739355103387248747, -3.994689410813206276, 14.38367211327322615 ) ) ;
#20273 = VERTEX_POINT ( 'NONE', #5209 ) ;
#20274 = CARTESIAN_POINT ( 'NONE',  ( 0.5998501479064708430, 28.86886762351073088, 38.48283596222038483 ) ) ;
#20275 = CARTESIAN_POINT ( 'NONE',  ( 5.981074661064941900, 20.34795181394745001, 2.687517936920068351 ) ) ;
#20276 = FACE_OUTER_BOUND ( 'NONE', #45618, .T. ) ;
#20277 = EDGE_CURVE ( 'NONE', #33488, #26084, #21957, .T. ) ;
#20278 = CARTESIAN_POINT ( 'NONE',  ( 4.958415959904816539, 43.07243048339532265, 14.42115411732758012 ) ) ;
#20279 = CARTESIAN_POINT ( 'NONE',  ( 0.5827359174754822568, -47.53228759166452733, 5.891371786504793207 ) ) ;
#20280 = CARTESIAN_POINT ( 'NONE',  ( 0.9722240741986364343, 30.74950262511642052, -29.92651525529343814 ) ) ;
#20282 = EDGE_CURVE ( 'NONE', #35884, #31400, #7359, .T. ) ;
#20281 = ORIENTED_EDGE ( 'NONE', *, *, #23880, .F. ) ;
#20283 = ORIENTED_EDGE ( 'NONE', *, *, #37597, .F. ) ;
#20284 = LINE ( 'NONE', #44716, #5286 ) ;
#20285 = CARTESIAN_POINT ( 'NONE',  ( 4.975610109902397937, 30.94437158899635776, -37.88001153774755636 ) ) ;
#20286 = CYLINDRICAL_SURFACE ( 'NONE', #53892, 8.000000000000000000 ) ;
#20287 = ORIENTED_EDGE ( 'NONE', *, *, #18367, .T. ) ;
#20288 = CARTESIAN_POINT ( 'NONE',  ( 0.1098349054025746369, -0.2133124578267739657, 43.12395110775227636 ) ) ;
#20289 = DIRECTION ( 'NONE',  ( -1.000000000000000000, -0.000000000000000000, -0.000000000000000000 ) ) ;
#20290 = VERTEX_POINT ( 'NONE', #17106 ) ;
#20291 = CARTESIAN_POINT ( 'NONE',  ( -6.078457390727109555, -8.902764005229702349, -17.07440494145240351 ) ) ;
#20292 = ORIENTED_EDGE ( 'NONE', *, *, #26465, .F. ) ;
#20293 = CARTESIAN_POINT ( 'NONE',  ( 0.6017666602106489515, 34.26316403931513577, 33.76944145963986443 ) ) ;
#20294 = ORIENTED_EDGE ( 'NONE', *, *, #9063, .T. ) ;
#20295 = CARTESIAN_POINT ( 'NONE',  ( 4.960386119450153508, -42.07286811692932105, -12.01291942401236668 ) ) ;
#20296 = CARTESIAN_POINT ( 'NONE',  ( 5.896278296736517710, 18.99819559441548833, 6.602692160832260626 ) ) ;
#20297 = CARTESIAN_POINT ( 'NONE',  ( 0.7948884756798507700, -48.57723108478376162, -7.138015461994420718 ) ) ;
#20298 = CARTESIAN_POINT ( 'NONE',  ( 4.962356264823608143, 0.000000000000000000, 0.000000000000000000 ) ) ;
#20299 = CIRCLE ( 'NONE', #16314, 42.92674063221959813 ) ;
#20300 = EDGE_LOOP ( 'NONE', ( #33621, #39981, #33812, #29193 ) ) ;
#20301 = CARTESIAN_POINT ( 'NONE',  ( -6.077587904424778920, 9.976910903713122281, -16.46988980574249695 ) ) ;
#20302 = CARTESIAN_POINT ( 'NONE',  ( 0.5998501479064699549, -0.5236536531311584142, -48.10473956285919428 ) ) ;
#20303 = EDGE_CURVE ( 'NONE', #21575, #37980, #26485, .T. ) ;
#20304 = ORIENTED_EDGE ( 'NONE', *, *, #49627, .T. ) ;
#20305 = CARTESIAN_POINT ( 'NONE',  ( 0.1073791018717483448, 21.14095454447559419, -37.58707531572184735 ) ) ;
#20307 = EDGE_CURVE ( 'NONE', #6110, #4631, #49555, .T. ) ;
#20306 = ORIENTED_EDGE ( 'NONE', *, *, #35991, .T. ) ;
#20308 = CARTESIAN_POINT ( 'NONE',  ( 5.960221823109900008, -5.307149561568222929, 19.82761049839333012 ) ) ;
#20309 = ORIENTED_EDGE ( 'NONE', *, *, #30346, .F. ) ;
#20310 = CARTESIAN_POINT ( 'NONE',  ( 0.9754292589017187209, -31.46929217701820036, -27.67690583813050864 ) ) ;
#20311 = CARTESIAN_POINT ( 'NONE',  ( 0.6008123274975391004, -30.27644390292597265, -38.66382670858426707 ) ) ;
#20312 = EDGE_CURVE ( 'NONE', #497, #42276, #60629, .T. ) ;
#20313 = CARTESIAN_POINT ( 'NONE',  ( 0.7057020205115085432, 41.05685587925835023, 24.67553336431198829 ) ) ;
#20314 = ORIENTED_EDGE ( 'NONE', *, *, #6617, .T. ) ;
#20315 = CARTESIAN_POINT ( 'NONE',  ( -6.016761891674564211, 7.207804629151548070, -17.41015286184795130 ) ) ;
#20316 = ADVANCED_FACE ( 'NONE', ( #7050 ), #11264, .F. ) ;
#20317 = CARTESIAN_POINT ( 'NONE',  ( 0.8557997880470599172, 11.51622788066458369, 46.50333260518563350 ) ) ;
#20318 = CARTESIAN_POINT ( 'NONE',  ( -1.200000000000006617, 0.000000000000000000, 0.000000000000000000 ) ) ;
#20319 = EDGE_LOOP ( 'NONE', ( #26975, #21118, #58563, #50856 ) ) ;
#20320 = ORIENTED_EDGE ( 'NONE', *, *, #17734, .T. ) ;
#20321 = CARTESIAN_POINT ( 'NONE',  ( 0.9787284016396604613, -31.20693553390243480, -27.97254320779017078 ) ) ;
#20322 = LINE ( 'NONE', #6794, #5151 ) ;
#20323 = CARTESIAN_POINT ( 'NONE',  ( -6.077587904424778920, 7.800189710370596607, 17.60548385805284255 ) ) ;
#20324 = CARTESIAN_POINT ( 'NONE',  ( 4.975801465491695552, -42.71626295676279028, 21.70134120755125906 ) ) ;
#20325 = AXIS2_PLACEMENT_3D ( 'NONE', #15810, #58374, #44036 ) ;
#20326 = CARTESIAN_POINT ( 'NONE',  ( 0.9784957157296365615, -27.23471787112080733, -31.85283660010242812 ) ) ;
#20327 = CARTESIAN_POINT ( 'NONE',  ( -6.078075953587585900, -16.14115596471642178, 10.50039324834243359 ) ) ;
#20328 = ORIENTED_EDGE ( 'NONE', *, *, #20397, .F. ) ;
#20329 = CARTESIAN_POINT ( 'NONE',  ( 5.895881250540457863, -11.92688455204484121, -16.19497164216397422 ) ) ;
#20330 = ORIENTED_EDGE ( 'NONE', *, *, #24526, .F. ) ;
#20331 = CARTESIAN_POINT ( 'NONE',  ( 0.6028618097248862329, 12.61968633793851247, 46.42282207635408042 ) ) ;
#20332 = CARTESIAN_POINT ( 'NONE',  ( 2.526552050251864134, 42.96196914573631886, 1.212569781798080726 ) ) ;
#20333 = CARTESIAN_POINT ( 'NONE',  ( -6.015611763856276717, -17.41126425312532433, -7.205255340944797027 ) ) ;
#20334 = LINE ( 'NONE', #39454, #9669 ) ;
#20335 = CARTESIAN_POINT ( 'NONE',  ( 2.185380717157383135, 11.19526193201791919, 42.58504330561036255 ) ) ;
#20336 = CARTESIAN_POINT ( 'NONE',  ( 3.238931869106855377, -18.12707634097797538, -38.98364358950738051 ) ) ;
#20337 = CYLINDRICAL_SURFACE ( 'NONE', #16702, 5.000000000000000888 ) ;
#20338 = CARTESIAN_POINT ( 'NONE',  ( 0.5809828226811556418, 44.03860873105722362, -18.83114015454650314 ) ) ;
#20339 = CARTESIAN_POINT ( 'NONE',  ( 0.1157506346131639274, 29.73331724943256305, 32.60169482016893028 ) ) ;
#20340 = CARTESIAN_POINT ( 'NONE',  ( 4.549368137175248350, -42.06008734272390370, -8.582197505784284530 ) ) ;
#20341 = B_SPLINE_CURVE_WITH_KNOTS ( 'NONE', 3,
 ( #14180, #33285, #52356, #15407, #53282, #24795 ),
 .UNSPECIFIED., .F., .F.,
 ( 4, 2, 4 ),
 ( 2.168404344971008868E-19, 0.0002445244328975376192, 0.0004890488657950750216 ),
 .UNSPECIFIED. ) ;
#20342 = DIRECTION ( 'NONE',  ( -0.07836865515943411409, 0.9968932487286223942, -0.007886984708660891782 ) ) ;
#20343 = CARTESIAN_POINT ( 'NONE',  ( 2.706805983486680223, -19.31528737462589973, -39.54359350078559743 ) ) ;
#20344 = CARTESIAN_POINT ( 'NONE',  ( 0.8751705887134423323, 11.58504748649134974, 46.67919521768892110 ) ) ;
#20345 = CARTESIAN_POINT ( 'NONE',  ( 5.959547316686252039, 20.34955788964373014, 2.682663672454983050 ) ) ;
#20346 = APPLICATION_CONTEXT ( 'automotive_design' ) ;
#20347 =( BOUNDED_SURFACE ( )  B_SPLINE_SURFACE ( 3, 1, ( 
 ( #17587, #30739 ),
 ( #12284, #36708 ),
 ( #12900, #32000 ),
 ( #51077, #8171 ) ),
 .UNSPECIFIED., .F., .F., .F. ) 
 B_SPLINE_SURFACE_WITH_KNOTS ( ( 4, 4 ),
 ( 2, 2 ),
 ( 0.000000000000000000, 1.000000000000000000 ),
 ( 0.000000000000000000, 1.000000000000000000 ),
 .UNSPECIFIED. ) 
 GEOMETRIC_REPRESENTATION_ITEM ( )  RATIONAL_B_SPLINE_SURFACE ( (
 ( 1.000000000000000000, 1.000000000000000000),
 ( 0.7282232189291694135, 0.9929344683865672927),
 ( 0.7282232189291694135, 0.9929344683865672927),
 ( 1.000000000000000000, 1.000000000000000000) ) ) 
 REPRESENTATION_ITEM ( '' )  SURFACE ( )  );
#20348 = ADVANCED_FACE ( 'NONE', ( #55912 ), #32131, .F. ) ;
#20349 = ORIENTED_EDGE ( 'NONE', *, *, #58371, .F. ) ;
#20350 = CARTESIAN_POINT ( 'NONE',  ( 1.830465331921978800, -41.27772401688780946, 15.37938736959416453 ) ) ;
#20351 = CARTESIAN_POINT ( 'NONE',  ( 0.5850706913938533704, 29.01314519953797699, 38.10903744847151842 ) ) ;
#20352 = CARTESIAN_POINT ( 'NONE',  ( 0.5832366564991506852, 18.07697797533149853, -44.35361744978919774 ) ) ;
#20353 = CARTESIAN_POINT ( 'NONE',  ( 0.8554163680231816613, -30.98316862405899741, -35.23136010892773839 ) ) ;
#20354 = DIRECTION ( 'NONE',  ( 0.000000000000000000, 0.000000000000000000, -1.000000000000000000 ) ) ;
#20355 = EDGE_LOOP ( 'NONE', ( #51081, #11195, #52489, #61943 ) ) ;
#20356 = CARTESIAN_POINT ( 'NONE',  ( 0.9730545539215883499, -21.89037132892409687, -36.90443313492354349 ) ) ;
#20357 = CARTESIAN_POINT ( 'NONE',  ( 0.6008123274975389894, 28.45128422543073299, -40.02597877731679432 ) ) ;
#20358 = AXIS2_PLACEMENT_3D ( 'NONE', #39813, #6225, #25675 ) ;
#20359 = B_SPLINE_CURVE_WITH_KNOTS ( 'NONE', 3,
 ( #55568, #47132, #41206, #60576, #33037, #60892, #46832, #27704, #61201, #32103, #52109, #32411, #51486, #12695, #36815, #23016, #28313, #42145, #13935 ),
 .UNSPECIFIED., .F., .F.,
 ( 4, 3, 3, 3, 3, 3, 4 ),
 ( 0.000000000000000000, 0.0002724573126191823149, 0.0004086839781548524345, 0.0005449106435901870157, 0.0006811373090491508074, 0.0008459866663933821680, 0.001010840725717217052 ),
 .UNSPECIFIED. ) ;
#20360 = CARTESIAN_POINT ( 'NONE',  ( -2.700785417809989042, -13.56184546075576769, -3.000000000000003997 ) ) ;
#20361 = ORIENTED_EDGE ( 'NONE', *, *, #24185, .T. ) ;
#20362 = CARTESIAN_POINT ( 'NONE',  ( 0.8560838555295158248, 5.603718208094640829, -46.57221463840858888 ) ) ;
#20363 = ORIENTED_EDGE ( 'NONE', *, *, #52475, .T. ) ;
#20364 = CARTESIAN_POINT ( 'NONE',  ( 1.091591847532196846, -26.46008473750376311, -32.50573651895864202 ) ) ;
#20365 = ORIENTED_EDGE ( 'NONE', *, *, #10691, .F. ) ;
#20366 = CARTESIAN_POINT ( 'NONE',  ( 3.240649175237396484, -28.83388502998269587, 33.22456909390083979 ) ) ;
#20367 = ORIENTED_EDGE ( 'NONE', *, *, #36070, .T. ) ;
#20368 = CARTESIAN_POINT ( 'NONE',  ( 0.1135584504625007513, 29.98315275015343673, -32.37225051330565861 ) ) ;
#20369 = CARTESIAN_POINT ( 'NONE',  ( 0.1154773475650540948, 20.56842169694548872, 39.03695248021728759 ) ) ;
#20370 = EDGE_LOOP ( 'NONE', ( #57926, #18135, #50097, #28376 ) ) ;
#20371 = CARTESIAN_POINT ( 'NONE',  ( 0.6845945791218023269, -18.95641467630792931, 42.90758514917615685 ) ) ;
#20372 = ORIENTED_EDGE ( 'NONE', *, *, #26576, .T. ) ;
#20373 = CARTESIAN_POINT ( 'NONE',  ( 0.5804410086790514622, -38.35366574781981797, -26.99103880105228370 ) ) ;
#20374 = EDGE_CURVE ( 'NONE', #52874, #47700, #24047, .T. ) ;
#20375 = LINE ( 'NONE', #53250, #8698 ) ;
#20376 = EDGE_CURVE ( 'NONE', #59796, #61948, #44498, .T. ) ;
#20377 = ORIENTED_EDGE ( 'NONE', *, *, #54399, .F. ) ;
#20378 = CARTESIAN_POINT ( 'NONE',  ( 3.270143674763207553, -8.548517033725183012, -10.69018354892896205 ) ) ;
#20379 = CARTESIAN_POINT ( 'NONE',  ( 4.553261556744875094, -36.69060082144763868, -24.15241969627107110 ) ) ;
#20380 = CARTESIAN_POINT ( 'NONE',  ( 0.5998501479064699549, 47.76154736470750350, 5.759754759340949271 ) ) ;
#20381 = CARTESIAN_POINT ( 'NONE',  ( 0.2279481005628790080, -6.290797834582413373, -43.66840218827940845 ) ) ;
#20382 = ORIENTED_EDGE ( 'NONE', *, *, #480, .T. ) ;
#20383 = EDGE_CURVE ( 'NONE', #46057, #41641, #27043, .T. ) ;
#20384 = DIRECTION ( 'NONE',  ( 1.000000000000000000, 0.000000000000000000, 0.000000000000000000 ) ) ;
#20385 = FACE_OUTER_BOUND ( 'NONE', #15915, .T. ) ;
#20386 = ORIENTED_EDGE ( 'NONE', *, *, #17284, .F. ) ;
#20387 = AXIS2_PLACEMENT_3D ( 'NONE', #16312, #2189, #21324 ) ;
#20388 = CARTESIAN_POINT ( 'NONE',  ( 4.962356264823608143, -41.76635909427997717, 5.177532797578748180 ) ) ;
#20389 = ORIENTED_EDGE ( 'NONE', *, *, #33627, .T. ) ;
#20390 = CARTESIAN_POINT ( 'NONE',  ( 4.963659409799330291, -39.92545197189564732, 20.22157859941717462 ) ) ;
#20391 = CARTESIAN_POINT ( 'NONE',  ( 0.9772918015221170318, 40.30802579601094493, -11.47170049202803987 ) ) ;
#20392 = ORIENTED_EDGE ( 'NONE', *, *, #12076, .T. ) ;
#20393 = CARTESIAN_POINT ( 'NONE',  ( 2.301529144917015213, 4.990866136406635789, -47.77346141661145396 ) ) ;
#20394 = CARTESIAN_POINT ( 'NONE',  ( 0.5980271706414734822, -14.64360625457663545, -46.87871626551421400 ) ) ;
#20395 = CARTESIAN_POINT ( 'NONE',  ( 0.7245667037590756143, -0.8205429720401278271, -48.09508190954919371 ) ) ;
#20396 = CARTESIAN_POINT ( 'NONE',  ( -6.077587904424778920, 15.43577113102541887, -11.51229738082424348 ) ) ;
#20397 = EDGE_CURVE ( 'NONE', #27345, #15368, #51210, .T. ) ;
#20398 = EDGE_LOOP ( 'NONE', ( #14211, #27358 ) ) ;
#20399 = CARTESIAN_POINT ( 'NONE',  ( 0.6023142530420679819, 18.16775455049945265, -44.54505940664467545 ) ) ;
#20400 = EDGE_CURVE ( 'NONE', #8721, #8500, #31497, .T. ) ;
#20401 = CARTESIAN_POINT ( 'NONE',  ( -69.95594261585600293, 1.530808498934191521E-15, 12.50000000000000000 ) ) ;
#20402 = VECTOR ( 'NONE', #32094, 1000.000000000000000 ) ;
#20404 = CARTESIAN_POINT ( 'NONE',  ( -6.016761891674564211, 0.003433883959783673098, 18.84319130225482297 ) ) ;
#20403 =( BOUNDED_SURFACE ( )  B_SPLINE_SURFACE ( 3, 1, ( 
 ( #31001, #50109 ),
 ( #31307, #26294 ),
 ( #45428, #2476 ),
 ( #59808, #52875 ) ),
 .UNSPECIFIED., .F., .F., .F. ) 
 B_SPLINE_SURFACE_WITH_KNOTS ( ( 4, 4 ),
 ( 2, 2 ),
 ( 0.000000000000000000, 1.000000000000000000 ),
 ( 0.000000000000000000, 1.000000000000000000 ),
 .UNSPECIFIED. ) 
 GEOMETRIC_REPRESENTATION_ITEM ( )  RATIONAL_B_SPLINE_SURFACE ( (
 ( 1.000000000000000000, 1.000000000000000000),
 ( 0.7282232189291694135, 0.9929344683865672927),
 ( 0.7282232189291694135, 0.9929344683865672927),
 ( 1.000000000000000000, 1.000000000000000000) ) ) 
 REPRESENTATION_ITEM ( '' )  SURFACE ( )  );
#20405 = LINE ( 'NONE', #58582, #29833 ) ;
#20406 = CARTESIAN_POINT ( 'NONE',  ( 2.879087469061463178, -8.726460098500798068, -43.12714424736063989 ) ) ;
#20407 = CARTESIAN_POINT ( 'NONE',  ( 0.7056759521544990754, 43.50199477485651300, -17.53069535772447551 ) ) ;
#20408 = CARTESIAN_POINT ( 'NONE',  ( 2.299746137290199943, 18.13766869742548238, 45.55552998164515088 ) ) ;
#20409 = CARTESIAN_POINT ( 'NONE',  ( 0.8554163680231738898, 40.82560365045097228, -23.11872746688500868 ) ) ;
#20410 = CARTESIAN_POINT ( 'NONE',  ( -6.077587904424778920, -12.95044751835525609, -14.25068175450762809 ) ) ;
#20411 = CARTESIAN_POINT ( 'NONE',  ( 0.000000000000000000, 0.000000000000000000, -1.199999999999999956 ) ) ;
#20412 = DIRECTION ( 'NONE',  ( -1.718001593797181987E-16, 1.000000000000000000, 0.000000000000000000 ) ) ;
#20413 = CARTESIAN_POINT ( 'NONE',  ( 0.6067099128993242996, 44.51753430581941018, 17.67241243535499251 ) ) ;
#20414 =( BOUNDED_SURFACE ( )  B_SPLINE_SURFACE ( 3, 1, ( 
 ( #61914, #56922 ),
 ( #33146, #14657 ),
 ( #33767, #47238 ),
 ( #14046, #24039 ) ),
 .UNSPECIFIED., .F., .F., .F. ) 
 B_SPLINE_SURFACE_WITH_KNOTS ( ( 4, 4 ),
 ( 2, 2 ),
 ( 0.000000000000000000, 1.000000000000000000 ),
 ( 0.000000000000000000, 1.000000000000000000 ),
 .UNSPECIFIED. ) 
 GEOMETRIC_REPRESENTATION_ITEM ( )  RATIONAL_B_SPLINE_SURFACE ( (
 ( 1.000000000000000000, 1.000000000000000000),
 ( 0.7211978278499968642, 0.9934217856018975334),
 ( 0.7211978278499968642, 0.9934217856018975334),
 ( 1.000000000000000000, 1.000000000000000000) ) ) 
 REPRESENTATION_ITEM ( '' )  SURFACE ( )  );
#20415 = EDGE_CURVE ( 'NONE', #56211, #13708, #13634, .T. ) ;
#20416 = DIRECTION ( 'NONE',  ( -1.000000000000000000, -0.000000000000000000, -0.000000000000000000 ) ) ;
#20417 = CARTESIAN_POINT ( 'NONE',  ( 3.678834586032788234, 15.16700106520579716, 46.56795516571884264 ) ) ;
#20418 = ORIENTED_EDGE ( 'NONE', *, *, #21095, .F. ) ;
#20419 = CARTESIAN_POINT ( 'NONE',  ( 4.226256110419179812, -3.807882442703405257, -43.77587556279986813 ) ) ;
#20420 = CARTESIAN_POINT ( 'NONE',  ( 3.390910168358336474, 18.57460499532419007, -39.86328117204245558 ) ) ;
#20421 = ORIENTED_EDGE ( 'NONE', *, *, #3250, .T. ) ;
#20422 = CARTESIAN_POINT ( 'NONE',  ( 2.526552050251863246, 9.948123361606842963, 41.81191169914599470 ) ) ;
#20423 = CARTESIAN_POINT ( 'NONE',  ( 0.1154773475650540671, 4.415934506188623487, 43.90265541494242996 ) ) ;
#20424 = VECTOR ( 'NONE', #20479, 1000.000000000000000 ) ;
#20425 = B_SPLINE_CURVE_WITH_KNOTS ( 'NONE', 3,
 ( #44435, #39731, #40049, #49713 ),
 .UNSPECIFIED., .F., .F.,
 ( 4, 4 ),
 ( 0.000000000000000000, 0.004447772540403797242 ),
 .UNSPECIFIED. ) ;
#20426 = ORIENTED_EDGE ( 'NONE', *, *, #52383, .F. ) ;
#20427 = ORIENTED_EDGE ( 'NONE', *, *, #34394, .F. ) ;
#20428 = CARTESIAN_POINT ( 'NONE',  ( 0.5806925824938511393, 32.99217760300656010, 33.32774488853447536 ) ) ;
#20429 = VERTEX_POINT ( 'NONE', #22724 ) ;
#20430 = CARTESIAN_POINT ( 'NONE',  ( 0.6027444965799114707, 10.80005187744475492, 47.90508736378573218 ) ) ;
#20431 = ORIENTED_EDGE ( 'NONE', *, *, #31371, .T. ) ;
#20432 = ORIENTED_EDGE ( 'NONE', *, *, #7555, .F. ) ;
#20433 = CARTESIAN_POINT ( 'NONE',  ( 0.8744876279028263033, -48.79802643035343834, 5.394688766001209501 ) ) ;
#20434 = ORIENTED_EDGE ( 'NONE', *, *, #34496, .F. ) ;
#20435 = CARTESIAN_POINT ( 'NONE',  ( 4.553261556744873317, 27.21079963941887314, -34.48350256002191117 ) ) ;
#20436 = CIRCLE ( 'NONE', #55436, 2.649999999999999467 ) ;
#20437 = CARTESIAN_POINT ( 'NONE',  ( 0.9790850452238872847, -17.68673899395511739, -37.99363886261624401 ) ) ;
#20438 = ORIENTED_EDGE ( 'NONE', *, *, #45215, .F. ) ;
#20439 = LINE ( 'NONE', #40499, #57738 ) ;
#20440 = CARTESIAN_POINT ( 'NONE',  ( 1.499999999999998668, 7.400000000000022560, 0.000000000000000000 ) ) ;
#20441 = ORIENTED_EDGE ( 'NONE', *, *, #38642, .T. ) ;
#20442 = ADVANCED_FACE ( 'NONE', ( #13644 ), #52050, .F. ) ;
#20443 = VERTEX_POINT ( 'NONE', #42469 ) ;
#20444 = CARTESIAN_POINT ( 'NONE',  ( 3.240649175237395596, 30.90334817137453172, -31.30891229660418773 ) ) ;
#20445 = B_SPLINE_CURVE_WITH_KNOTS ( 'NONE', 3,
 ( #26524, #45651, #2706, #36256 ),
 .UNSPECIFIED., .F., .F.,
 ( 4, 4 ),
 ( 8.673617379884035472E-19, 0.004050076154993002484 ),
 .UNSPECIFIED. ) ;
#20446 = CARTESIAN_POINT ( 'NONE',  ( 1.157644175074337145, 14.29172630907547692, 39.40493414010056483 ) ) ;
#20447 = DIRECTION ( 'NONE',  ( -1.000000000000000000, 0.000000000000000000, 0.000000000000000000 ) ) ;
#20448 = CARTESIAN_POINT ( 'NONE',  ( -5.720000000000000639, 3.469446951953614189E-15, 0.000000000000000000 ) ) ;
#20449 = EDGE_CURVE ( 'NONE', #55166, #7311, #50229, .T. ) ;
#20450 = ORIENTED_EDGE ( 'NONE', *, *, #17377, .T. ) ;
#20451 = CARTESIAN_POINT ( 'NONE',  ( -6.079354080745853928, 7.795569227098915199, 17.60744318956248833 ) ) ;
#20452 = CARTESIAN_POINT ( 'NONE',  ( -5.440000000000000391, 4.832908975360033023E-15, 0.000000000000000000 ) ) ;
#20453 = EDGE_CURVE ( 'NONE', #1908, #45184, #29479, .T. ) ;
#20454 = FACE_OUTER_BOUND ( 'NONE', #30394, .T. ) ;
#20455 = AXIS2_PLACEMENT_3D ( 'NONE', #14491, #48002, #35072 ) ;
#20456 = DIRECTION ( 'NONE',  ( 0.09722883295013594329, 0.8299705264940797633, -0.5492681305103133127 ) ) ;
#20457 = VERTEX_POINT ( 'NONE', #58063 ) ;
#20458 = CARTESIAN_POINT ( 'NONE',  ( 5.960721111146673579, -17.77882586010660049, -10.25731071096576486 ) ) ;
#20459 = CARTESIAN_POINT ( 'NONE',  ( 4.956445790444022670, -4.175462451061590308, -46.90526157542895191 ) ) ;
#20460 = CARTESIAN_POINT ( 'NONE',  ( 0.6029443199889047422, -35.27629250736205080, -34.16315015904468311 ) ) ;
#20461 = ORIENTED_EDGE ( 'NONE', *, *, #2524, .T. ) ;
#20462 = ORIENTED_EDGE ( 'NONE', *, *, #47612, .F. ) ;
#20463 = CARTESIAN_POINT ( 'NONE',  ( 0.9972139404380295780, 39.38665787682688091, -17.02682566833142630 ) ) ;
#20464 = CARTESIAN_POINT ( 'NONE',  ( 45.00000000000001421, 0.000000000000000000, 0.000000000000000000 ) ) ;
#20465 = CARTESIAN_POINT ( 'NONE',  ( 0.1100247026804066219, -39.90641708963723744, 16.34612806822689635 ) ) ;
#20466 = EDGE_CURVE ( 'NONE', #10980, #25968, #12087, .T. ) ;
#20467 = CARTESIAN_POINT ( 'NONE',  ( 0.9972139404380309102, -33.63772329383400006, 26.64066783422323681 ) ) ;
#20468 = CARTESIAN_POINT ( 'NONE',  ( 3.660087539127328871, -30.71416465583032007, -36.93668088065476951 ) ) ;
#20469 = CARTESIAN_POINT ( 'NONE',  ( 4.553261556744875094, 17.57396821678876364, 40.25785894628445760 ) ) ;
#20470 = CARTESIAN_POINT ( 'NONE',  ( 0.5807400328401637335, -41.75144119563903189, 23.47602859900699457 ) ) ;
#20471 = B_SPLINE_CURVE_WITH_KNOTS ( 'NONE', 3,
 ( #37144, #8596, #32430, #37451 ),
 .UNSPECIFIED., .F., .F.,
 ( 4, 4 ),
 ( 7.757919228897728493E-18, 0.005004741218457447495 ),
 .UNSPECIFIED. ) ;
#20472 = LINE ( 'NONE', #11382, #48793 ) ;
#20473 = CARTESIAN_POINT ( 'NONE',  ( -6.016761891674565099, -14.95139917749712488, 11.46828378093553980 ) ) ;
#20474 = VECTOR ( 'NONE', #16686, 1000.000000000000114 ) ;
#20475 = CARTESIAN_POINT ( 'NONE',  ( 3.782542959838394392, -10.79733161176426570, -40.62825966568303215 ) ) ;
#20476 = CARTESIAN_POINT ( 'NONE',  ( 5.958863334805807099, -14.51296551801793200, -14.51469124124474597 ) ) ;
#20477 = CIRCLE ( 'NONE', #17627, 42.08604991992415023 ) ;
#20478 = CARTESIAN_POINT ( 'NONE',  ( 0.1140933569871964842, -6.667546420828093900, -43.61758561417639157 ) ) ;
#20479 = DIRECTION ( 'NONE',  ( 1.000000000000000000, 1.836970198721027962E-16, -2.033782021272921061E-31 ) ) ;
#20480 = CARTESIAN_POINT ( 'NONE',  ( 5.895881250540457863, 14.91980774178274061, 13.48803241976162504 ) ) ;
#20481 = CIRCLE ( 'NONE', #55477, 7.400000000000022560 ) ;
#20482 = CARTESIAN_POINT ( 'NONE',  ( 4.553261556744873317, 40.63093864075514006, -16.69330377710856084 ) ) ;
#20483 = CARTESIAN_POINT ( 'NONE',  ( 0.5997462898726536595, 32.62638226927734308, -36.70246327105708417 ) ) ;
#20484 = CARTESIAN_POINT ( 'NONE',  ( 0.5998501479064708430, -44.24259072156073813, -18.89267974119652749 ) ) ;
#20485 = CONTEXT_DEPENDENT_SHAPE_REPRESENTATION ( #60377, #57310 ) ;
#20486 = CARTESIAN_POINT ( 'NONE',  ( 0.1368894036331285147, 44.06884517012258584, 2.190481977807497760 ) ) ;
#20487 = CARTESIAN_POINT ( 'NONE',  ( 0.5997462898726536595, -30.20781297212619165, 38.71743361310707598 ) ) ;
#20489 =( BOUNDED_SURFACE ( )  B_SPLINE_SURFACE ( 3, 1, ( 
 ( #17178, #8073 ),
 ( #36601, #55669 ),
 ( #59447, #46309 ),
 ( #22484, #30635 ) ),
 .UNSPECIFIED., .F., .F., .F. ) 
 B_SPLINE_SURFACE_WITH_KNOTS ( ( 4, 4 ),
 ( 2, 2 ),
 ( 0.000000000000000000, 1.000000000000000000 ),
 ( 0.000000000000000000, 1.000000000000000000 ),
 .UNSPECIFIED. ) 
 GEOMETRIC_REPRESENTATION_ITEM ( )  RATIONAL_B_SPLINE_SURFACE ( (
 ( 1.000000000000000000, 1.000000000000000000),
 ( 0.7282232189291694135, 0.9929344683865672927),
 ( 0.7282232189291694135, 0.9929344683865672927),
 ( 1.000000000000000000, 1.000000000000000000) ) ) 
 REPRESENTATION_ITEM ( '' )  SURFACE ( )  );
#20488 = CARTESIAN_POINT ( 'NONE',  ( 0.5998501479064708430, -47.62484632993683675, -6.798102206413969562 ) ) ;
#20490 = CARTESIAN_POINT ( 'NONE',  ( 1.231276596079881047, -27.70544295162376258, 31.45926257674180704 ) ) ;
#20492 = ORIENTED_EDGE ( 'NONE', *, *, #19449, .T. ) ;
#20491 = DIRECTION ( 'NONE',  ( 0.000000000000000000, 0.000000000000000000, 1.000000000000000000 ) ) ;
#20493 = VERTEX_POINT ( 'NONE', #19270 ) ;
#20494 = CARTESIAN_POINT ( 'NONE',  ( 0.1102144999581333162, -43.12427761225339395, -0.1260305566210554729 ) ) ;
#20495 = CARTESIAN_POINT ( 'NONE',  ( 4.962356264823608143, 0.000000000000000000, 0.000000000000000000 ) ) ;
#20496 = CARTESIAN_POINT ( 'NONE',  ( 1.827326673878743701, 15.32882202537219563, 40.22837085190317907 ) ) ;
#20497 = ADVANCED_FACE ( 'NONE', ( #5735 ), #45515, .F. ) ;
#20498 = ORIENTED_EDGE ( 'NONE', *, *, #23563, .F. ) ;
#20499 = ORIENTED_EDGE ( 'NONE', *, *, #21648, .F. ) ;
#20500 = CARTESIAN_POINT ( 'NONE',  ( 1.231276596079887264, 40.19859528295904738, -11.88905834349085922 ) ) ;
#20501 = CARTESIAN_POINT ( 'NONE',  ( 0.3622758884714600280, 0.8252992914328071139, -43.10531414739104861 ) ) ;
#20502 = CARTESIAN_POINT ( 'NONE',  ( 0.6017667736363748743, 5.933018439714683900, 47.74032759880257260 ) ) ;
#20503 = EDGE_CURVE ( 'NONE', #1834, #26558, #40490, .T. ) ;
#20504 = VERTEX_POINT ( 'NONE', #39615 ) ;
#20505 = VECTOR ( 'NONE', #48454, 1000.000000000000227 ) ;
#20506 = ORIENTED_EDGE ( 'NONE', *, *, #2997, .T. ) ;
#20507 = CARTESIAN_POINT ( 'NONE',  ( 4.999999999999984901, 72.00000000000002842, -4.333342374871278042E-31 ) ) ;
#20508 = EDGE_CURVE ( 'NONE', #18314, #58067, #48669, .T. ) ;
#20509 =( BOUNDED_SURFACE ( )  B_SPLINE_SURFACE ( 3, 1, ( 
 ( #37528, #32824 ),
 ( #32197, #14331 ),
 ( #28404, #8362 ),
 ( #51904, #51279 ) ),
 .UNSPECIFIED., .F., .F., .F. ) 
 B_SPLINE_SURFACE_WITH_KNOTS ( ( 4, 4 ),
 ( 2, 2 ),
 ( 0.000000000000000000, 1.000000000000000000 ),
 ( 0.000000000000000000, 1.000000000000000000 ),
 .UNSPECIFIED. ) 
 GEOMETRIC_REPRESENTATION_ITEM ( )  RATIONAL_B_SPLINE_SURFACE ( (
 ( 1.000000000000000000, 1.000000000000000000),
 ( 0.7269869731126821222, 0.9931720237060910339),
 ( 0.7269869731126821222, 0.9931720237060910339),
 ( 1.000000000000000000, 1.000000000000000000) ) ) 
 REPRESENTATION_ITEM ( '' )  SURFACE ( )  );
#20510 = CARTESIAN_POINT ( 'NONE',  ( -6.078726893082806448, -17.35055002122446410, -8.351793533709264139 ) ) ;
#20511 = CARTESIAN_POINT ( 'NONE',  ( 0.6000166863083106206, 32.62822748873757916, -36.70452632376071023 ) ) ;
#20512 = CARTESIAN_POINT ( 'NONE',  ( 4.553261556744875094, 0.000000000000000000, 0.000000000000000000 ) ) ;
#20513 =( BOUNDED_SURFACE ( )  B_SPLINE_SURFACE ( 3, 1, ( 
 ( #10816, #25210 ),
 ( #58698, #21437 ),
 ( #1377, #35557 ),
 ( #35247, #6070 ) ),
 .UNSPECIFIED., .F., .F., .F. ) 
 B_SPLINE_SURFACE_WITH_KNOTS ( ( 4, 4 ),
 ( 2, 2 ),
 ( 0.000000000000000000, 1.000000000000000000 ),
 ( 0.000000000000000000, 1.000000000000000000 ),
 .UNSPECIFIED. ) 
 GEOMETRIC_REPRESENTATION_ITEM ( )  RATIONAL_B_SPLINE_SURFACE ( (
 ( 1.000000000000000000, 1.000000000000000000),
 ( 0.9953040768229013402, 0.8617119497784988535),
 ( 0.9953040768229013402, 0.8617119497784988535),
 ( 1.000000000000000000, 1.000000000000000000) ) ) 
 REPRESENTATION_ITEM ( '' )  SURFACE ( )  );
#20514 = CARTESIAN_POINT ( 'NONE',  ( -2.708315649062916552, 0.2635547933241593199, 14.63219292706383179 ) ) ;
#20515 = CARTESIAN_POINT ( 'NONE',  ( -6.078075953587585900, 5.483964907265256095, 18.45863762965780808 ) ) ;
#20516 = VECTOR ( 'NONE', #24148, 1000.000000000000000 ) ;
#20517 = CARTESIAN_POINT ( 'NONE',  ( 0.1152339509894530906, 15.02909110027396800, -41.48576998387410697 ) ) ;
#20518 = VERTEX_POINT ( 'NONE', #25180 ) ;
#20519 = EDGE_CURVE ( 'NONE', #55413, #28131, #57627, .T. ) ;
#20520 = VERTEX_POINT ( 'NONE', #53064 ) ;
#20521 = DIRECTION ( 'NONE',  ( 0.000000000000000000, 0.000000000000000000, 1.000000000000000000 ) ) ;
#20522 = VECTOR ( 'NONE', #8299, 1000.000000000000114 ) ;
#20523 = ORIENTED_EDGE ( 'NONE', *, *, #29968, .T. ) ;
#20524 = CARTESIAN_POINT ( 'NONE',  ( 4.956653778116990594, -32.11725092155016625, -35.79382859084151391 ) ) ;
#20525 = CARTESIAN_POINT ( 'NONE',  ( 0.5998501479064699549, 44.64337787626223530, 17.92509395669123862 ) ) ;
#20526 = CARTESIAN_POINT ( 'NONE',  ( 0.8744876279028306332, -47.25615711918273121, 13.31186180466906954 ) ) ;
#20527 = DIRECTION ( 'NONE',  ( -1.000000000000000000, -0.000000000000000000, -0.000000000000000000 ) ) ;
#20528 = ADVANCED_FACE ( 'NONE', ( #15797 ), #2832, .F. ) ;
#20529 = CONICAL_SURFACE ( 'NONE', #61506, 42.92674063221959813, 1.485477209440487556 ) ;
#20530 = ORIENTED_EDGE ( 'NONE', *, *, #40427, .F. ) ;
#20531 = CARTESIAN_POINT ( 'NONE',  ( 0.5832655196449136881, -14.11139715999958888, 44.72251841260825245 ) ) ;
#20532 = CARTESIAN_POINT ( 'NONE',  ( 0.9762797500689124330, 32.57381952463229169, 26.36799322592426975 ) ) ;
#20533 = ADVANCED_FACE ( 'NONE', ( #34594 ), #56802, .F. ) ;
#20534 = DIRECTION ( 'NONE',  ( -1.000000000000000000, -1.836909530733580185E-16, 1.836909530733574022E-16 ) ) ;
#20535 = VERTEX_POINT ( 'NONE', #7598 ) ;
#20536 = CARTESIAN_POINT ( 'NONE',  ( -2.569797478183790229, -12.89088113963440740, 6.924386868080623536 ) ) ;
#20537 = FACE_OUTER_BOUND ( 'NONE', #14328, .T. ) ;
#20538 = ORIENTED_EDGE ( 'NONE', *, *, #23994, .T. ) ;
#20539 = PLANE ( 'NONE',  #10646 ) ;
#20540 = CARTESIAN_POINT ( 'NONE',  ( 5.965394784446458765, 18.96850062921623703, 7.841344330025009413 ) ) ;
#20541 = ORIENTED_EDGE ( 'NONE', *, *, #40918, .T. ) ;
#20542 = CARTESIAN_POINT ( 'NONE',  ( 4.553261556744873317, 35.33793455049254106, 26.09156851415302825 ) ) ;
#20543 = CARTESIAN_POINT ( 'NONE',  ( 4.956653778116966613, 0.000000000000000000, 0.000000000000000000 ) ) ;
#20544 = CARTESIAN_POINT ( 'NONE',  ( 3.238931869106854489, 1.828840280768788240, 42.95312220797018199 ) ) ;
#20545 = EDGE_CURVE ( 'NONE', #5168, #21617, #26258, .T. ) ;
#20546 = CARTESIAN_POINT ( 'NONE',  ( 0.6067099128993209689, -18.98236771638427101, -43.97493306231482535 ) ) ;
#20547 = FACE_OUTER_BOUND ( 'NONE', #61343, .T. ) ;
#20548 = DIRECTION ( 'NONE',  ( -1.000000000000000000, -0.000000000000000000, -0.000000000000000000 ) ) ;
#20549 = CARTESIAN_POINT ( 'NONE',  ( 2.643462169533613793, -46.73820883660198433, -11.09243630552516890 ) ) ;
#20550 = CARTESIAN_POINT ( 'NONE',  ( 0.9968887458511633826, 34.43855515351805963, -25.59699785741752365 ) ) ;
#20551 = VERTEX_POINT ( 'NONE', #11398 ) ;
#20552 = CARTESIAN_POINT ( 'NONE',  ( 4.549368137175248350, -38.40568845698290801, 19.17571786012255686 ) ) ;
#20553 = CARTESIAN_POINT ( 'NONE',  ( 0.9762797500689124330, -30.73989051779308568, -28.48480149377557424 ) ) ;
#20554 = CARTESIAN_POINT ( 'NONE',  ( 0.8560838555295223751, 44.99141268455589682, -13.27198623905683128 ) ) ;
#20555 = EDGE_LOOP ( 'NONE', ( #50050, #52325, #57448, #27477 ) ) ;
#20556 = CARTESIAN_POINT ( 'NONE',  ( 0.8751705887134423323, -0.8911681664091769539, 48.08707113907594533 ) ) ;
#20557 = CARTESIAN_POINT ( 'NONE',  ( 1.088313998177381503, -17.14007796983261755, 39.34193117255247785 ) ) ;
#20558 = CARTESIAN_POINT ( 'NONE',  ( 0.6252788684277198472, 48.95677309978731273, -3.831279007016552995 ) ) ;
#20559 = CARTESIAN_POINT ( 'NONE',  ( 0.1157991065609915993, 44.03865309785810922, -2.745796580996492597 ) ) ;
#20560 = DIRECTION ( 'NONE',  ( -0.8831157194574164038, 5.745494457772962184E-17, -0.4691552259617384202 ) ) ;
#20561 = CARTESIAN_POINT ( 'NONE',  ( 3.270143674763207553, 12.74832469035459681, -4.983712007628090745 ) ) ;
#20562 = DIRECTION ( 'NONE',  ( -1.000000000000000000, 1.577721810442030617E-30, -7.888609052210097910E-31 ) ) ;
#20563 = CARTESIAN_POINT ( 'NONE',  ( 5.838029081930955932, 30.48039787783015342, 36.08338126287622316 ) ) ;
#20564 = CARTESIAN_POINT ( 'NONE',  ( 4.962356264823608143, -40.47344704301786322, -11.53844366967987334 ) ) ;
#20565 = CIRCLE ( 'NONE', #30506, 5.612499999999999822 ) ;
#20566 = CARTESIAN_POINT ( 'NONE',  ( 0.3676999524040323597, -43.63756228305270213, -6.458617600968101335 ) ) ;
#20568 = VERTEX_POINT ( 'NONE', #26721 ) ;
#20567 = DIRECTION ( 'NONE',  ( -1.000000000000000000, -0.000000000000000000, -0.000000000000000000 ) ) ;
#20569 = ORIENTED_EDGE ( 'NONE', *, *, #32189, .T. ) ;
#20570 = CARTESIAN_POINT ( 'NONE',  ( 0.5839254288179567265, -12.48406597209070945, 46.24038938821428246 ) ) ;
#20571 = VECTOR ( 'NONE', #10727, 1000.000000000000227 ) ;
#20572 = CARTESIAN_POINT ( 'NONE',  ( 5.960721111146673579, -14.51823969584109619, 14.50930005614991813 ) ) ;
#20573 = DIRECTION ( 'NONE',  ( 0.09722883295013594329, 0.08804304236305897369, -0.9913601649928300841 ) ) ;
#20574 = ADVANCED_FACE ( 'NONE', ( #21716 ), #31205, .F. ) ;
#20575 = CIRCLE ( 'NONE', #10560, 15.99999999999999645 ) ;
#20576 = CARTESIAN_POINT ( 'NONE',  ( 0.7048096507298579061, 42.08020459959980997, -23.32077812596837418 ) ) ;
#20577 = CARTESIAN_POINT ( 'NONE',  ( 0.5988103564986356764, 0.6065102550366653356, 48.10388392110854028 ) ) ;
#20578 = CARTESIAN_POINT ( 'NONE',  ( 5.880360259849739535, -47.86623372148051914, 3.184717612777128171 ) ) ;
#20579 = EDGE_CURVE ( 'NONE', #40440, #39188, #21480, .T. ) ;
#20580 = VERTEX_POINT ( 'NONE', #6652 ) ;
#20581 = ORIENTED_EDGE ( 'NONE', *, *, #45221, .F. ) ;
#20582 = FACE_OUTER_BOUND ( 'NONE', #29977, .T. ) ;
#20583 = EDGE_CURVE ( 'NONE', #32701, #1858, #12040, .T. ) ;
#20584 = EDGE_CURVE ( 'NONE', #42039, #3844, #36059, .T. ) ;
#20585 = CARTESIAN_POINT ( 'NONE',  ( 0.1101816497532063233, -39.89358705406974082, -16.37745527993575578 ) ) ;
#20586 = CARTESIAN_POINT ( 'NONE',  ( 0.1073791018717578927, -21.98088480513690968, 37.10214135362851096 ) ) ;
#20587 = ORIENTED_EDGE ( 'NONE', *, *, #6824, .F. ) ;
#20588 = CARTESIAN_POINT ( 'NONE',  ( 5.965394784446460541, -20.52536205633085231, -0.01447339372445936509 ) ) ;
#20589 =( BOUNDED_SURFACE ( )  B_SPLINE_SURFACE ( 3, 1, ( 
 ( #32905, #51984 ),
 ( #4345, #9075 ),
 ( #28180, #23800 ),
 ( #23481, #61673 ) ),
 .UNSPECIFIED., .F., .F., .F. ) 
 B_SPLINE_SURFACE_WITH_KNOTS ( ( 4, 4 ),
 ( 2, 2 ),
 ( 0.000000000000000000, 1.000000000000000000 ),
 ( 0.000000000000000000, 1.000000000000000000 ),
 .UNSPECIFIED. ) 
 GEOMETRIC_REPRESENTATION_ITEM ( )  RATIONAL_B_SPLINE_SURFACE ( (
 ( 1.000000000000000000, 1.000000000000000000),
 ( 0.7269869731126821222, 0.9931720237060910339),
 ( 0.7269869731126821222, 0.9931720237060910339),
 ( 1.000000000000000000, 1.000000000000000000) ) ) 
 REPRESENTATION_ITEM ( '' )  SURFACE ( )  );
#20590 = ORIENTED_EDGE ( 'NONE', *, *, #56949, .F. ) ;
#20591 = EDGE_CURVE ( 'NONE', #1466, #15676, #52460, .T. ) ;
#20592 = B_SPLINE_CURVE_WITH_KNOTS ( 'NONE', 3,
 ( #34741, #53806, #10939, #7118 ),
 .UNSPECIFIED., .F., .F.,
 ( 4, 4 ),
 ( 0.000000000000000000, 0.005004741218457408464 ),
 .UNSPECIFIED. ) ;
#20593 = DIRECTION ( 'NONE',  ( -1.000000000000000000, -0.000000000000000000, -0.000000000000000000 ) ) ;
#20594 = VERTEX_POINT ( 'NONE', #54587 ) ;
#20595 = EDGE_CURVE ( 'NONE', #21146, #31192, #2280, .T. ) ;
#20596 = CARTESIAN_POINT ( 'NONE',  ( 1.227938101723748288, -33.52879263017845091, -26.79402671879361364 ) ) ;
#20597 = CARTESIAN_POINT ( 'NONE',  ( 0.2285344041767085332, -6.290293047543402238, 43.66844837719201422 ) ) ;
#20598 = ORIENTED_EDGE ( 'NONE', *, *, #56272, .F. ) ;
#20599 = CARTESIAN_POINT ( 'NONE',  ( 4.958415959904820092, -43.67231206503760177, -12.48731807541597050 ) ) ;
#20600 = CARTESIAN_POINT ( 'NONE',  ( 0.7764139734771249302, 46.89611479102006797, 0.8915651486764878397 ) ) ;
#20601 = CARTESIAN_POINT ( 'NONE',  ( 3.782542959838390839, 5.920274717261695407, -41.61956511868813635 ) ) ;
#20602 = DIRECTION ( 'NONE',  ( 0.000000000000000000, -1.000000000000000000, 1.287488025362403787E-15 ) ) ;
#20603 = EDGE_LOOP ( 'NONE', ( #26928, #44220, #9553, #30821 ) ) ;
#20604 = CARTESIAN_POINT ( 'NONE',  ( -6.057079549204054558, 9.975405573751451982, -16.47187040802916513 ) ) ;
#20605 = CARTESIAN_POINT ( 'NONE',  ( 5.974727161628367256, -18.95664195401523244, 7.868887636447281508 ) ) ;
#20606 = ORIENTED_EDGE ( 'NONE', *, *, #60165, .T. ) ;
#20607 = LINE ( 'NONE', #6462, #143 ) ;
#20608 = ORIENTED_EDGE ( 'NONE', *, *, #57586, .T. ) ;
#20609 = CARTESIAN_POINT ( 'NONE',  ( 5.960721111146673579, -5.306302591836717930, 19.82781442290488627 ) ) ;
#20610 = ORIENTED_EDGE ( 'NONE', *, *, #49674, .T. ) ;
#20611 = CARTESIAN_POINT ( 'NONE',  ( 0.3622758884714730732, 37.74294673546557988, 20.83792692158985460 ) ) ;
#20612 = CARTESIAN_POINT ( 'NONE',  ( 0.6029443449137436017, -30.58394248115737923, -38.42085371634249924 ) ) ;
#20613 = CIRCLE ( 'NONE', #10600, 2.649999999999985700 ) ;
#20614 = CARTESIAN_POINT ( 'NONE',  ( 4.967162193818130511, -42.16965968614200477, 8.839793687085075291 ) ) ;
#20615 = ORIENTED_EDGE ( 'NONE', *, *, #4718, .F. ) ;
#20616 = CARTESIAN_POINT ( 'NONE',  ( 0.8751705887134423323, 38.69254731947834358, -28.56654290188613032 ) ) ;
#20617 = CARTESIAN_POINT ( 'NONE',  ( 0.5827357941260216112, -5.891356987507951004, 47.53228940613937681 ) ) ;
#20618 = DIRECTION ( 'NONE',  ( -1.000000000000000000, -1.836909530733573776E-16, 1.925929944387235853E-32 ) ) ;
#20620 = ORIENTED_EDGE ( 'NONE', *, *, #31114, .T. ) ;
#20619 = EDGE_CURVE ( 'NONE', #16005, #40440, #34509, .T. ) ;
#20621 = ORIENTED_EDGE ( 'NONE', *, *, #13447, .F. ) ;
#20622 = CARTESIAN_POINT ( 'NONE',  ( 0.1129192098497447394, -23.28677643606880565, -37.47903188453118162 ) ) ;
#20623 = CARTESIAN_POINT ( 'NONE',  ( -4.473699999999997345, 0.000000000000000000, -12.50000000000000000 ) ) ;
#20625 = EDGE_CURVE ( 'NONE', #35006, #14741, #31426, .T. ) ;
#20624 = CARTESIAN_POINT ( 'NONE',  ( 3.376099380956838925, -1.774645281739724023, -13.28755123249073478 ) ) ;
#20626 = CARTESIAN_POINT ( 'NONE',  ( 0.1084644655670282121, -6.022910953206811691, -42.70194587816327214 ) ) ;
#20627 = CARTESIAN_POINT ( 'NONE',  ( 0.9789889208857702751, -27.13076157042887004, -31.94145699010782735 ) ) ;
#20628 = CARTESIAN_POINT ( 'NONE',  ( -6.017396004339687465, 14.95000090562897022, -11.47005965438123631 ) ) ;
#20629 = EDGE_LOOP ( 'NONE', ( #38145, #59185, #41592, #41985 ) ) ;
#20630 = AXIS2_PLACEMENT_3D ( 'NONE', #6107, #25243, #38921 ) ;
#20631 = CARTESIAN_POINT ( 'NONE',  ( 0.8557997880470690211, 7.156447707085701104, 47.37054680076709445 ) ) ;
#20632 = ORIENTED_EDGE ( 'NONE', *, *, #3143, .F. ) ;
#20633 = CARTESIAN_POINT ( 'NONE',  ( 0.1073791018717483448, -21.98088480513640874, -37.10214135362880228 ) ) ;
#20634 = CARTESIAN_POINT ( 'NONE',  ( 4.322998006666165516, 43.48102276965671820, 20.30542865297664079 ) ) ;
#20635 = CARTESIAN_POINT ( 'NONE',  ( -6.078726893082806448, 18.62710865126535253, -4.881072071038842886 ) ) ;
#20636 = CARTESIAN_POINT ( 'NONE',  ( 1.112077966505211624, 10.82950106662251244, 42.72882202654990635 ) ) ;
#20637 = DIRECTION ( 'NONE',  ( 0.000000000000000000, 0.000000000000000000, 1.000000000000000000 ) ) ;
#20638 = CARTESIAN_POINT ( 'NONE',  ( -90.00000000000000000, 0.000000000000000000, 0.000000000000000000 ) ) ;
#20639 = CARTESIAN_POINT ( 'NONE',  ( 2.526552050251864578, -9.948123361606551640, -41.81191169914605865 ) ) ;
#20640 = B_SPLINE_CURVE_WITH_KNOTS ( 'NONE', 3,
 ( #35285, #54662, #11471, #11788 ),
 .UNSPECIFIED., .F., .F.,
 ( 4, 4 ),
 ( 0.000000000000000000, 0.005014147105413705591 ),
 .UNSPECIFIED. ) ;
#20641 = CARTESIAN_POINT ( 'NONE',  ( 0.1158816050234199174, 29.66892107124847655, 32.66033012345694431 ) ) ;
#20642 = CARTESIAN_POINT ( 'NONE',  ( 4.956445790444002242, -37.28933980949966553, 28.75835855384135087 ) ) ;
#20643 = CARTESIAN_POINT ( 'NONE',  ( 1.157644175074338033, -41.75974213338677998, -3.623011514227223007 ) ) ;
#20644 = CARTESIAN_POINT ( 'NONE',  ( 5.331200000000000827, 0.000000000000000000, 0.000000000000000000 ) ) ;
#20645 = EDGE_CURVE ( 'NONE', #5544, #60819, #21830, .T. ) ;
#20646 = B_SPLINE_CURVE_WITH_KNOTS ( 'NONE', 3,
 ( #50381, #1832, #7444, #45401, #21574, #12500 ),
 .UNSPECIFIED., .F., .F.,
 ( 4, 2, 4 ),
 ( 6.314488766312914258E-18, 0.0002291472222819940197, 0.0004582944445639816969 ),
 .UNSPECIFIED. ) ;
#20647 = CARTESIAN_POINT ( 'NONE',  ( 1.157644175074338033, 3.373327072561506323, 41.78065269883544630 ) ) ;
#20648 = DIRECTION ( 'NONE',  ( 0.09722883295013598492, -0.9880289017988314049, 0.1197724645039495717 ) ) ;
#20649 = EDGE_CURVE ( 'NONE', #3284, #16197, #15070, .T. ) ;
#20650 = ORIENTED_EDGE ( 'NONE', *, *, #21584, .F. ) ;
#20651 = CIRCLE ( 'NONE', #9641, 47.91270532121795611 ) ;
#20652 = CARTESIAN_POINT ( 'NONE',  ( 0.9754292580325131246, 24.38796667030967669, 34.08158665015274380 ) ) ;
#20653 = ADVANCED_FACE ( 'NONE', ( #12960 ), #37631, .F. ) ;
#20654 = ADVANCED_FACE ( 'NONE', ( #46783 ), #50411, .F. ) ;
#20655 = CARTESIAN_POINT ( 'NONE',  ( 0.5806925824938499181, -24.77160101449041463, -39.81946942793766198 ) ) ;
#20656 = CIRCLE ( 'NONE', #15660, 47.09074272231896430 ) ;
#20657 = CARTESIAN_POINT ( 'NONE',  ( 0.1156867017252034419, -38.38474613842218730, -21.76129755239952601 ) ) ;
#20658 = CARTESIAN_POINT ( 'NONE',  ( 2.618530812446115519, -31.41152511854568274, -34.97202995145080706 ) ) ;
#20659 = CARTESIAN_POINT ( 'NONE',  ( 0.1073791018717483448, -41.52698815987176317, 11.62916352156079824 ) ) ;
#20660 = AXIS2_PLACEMENT_3D ( 'NONE', #54472, #35414, #17225 ) ;
#20661 = EDGE_CURVE ( 'NONE', #36980, #27845, #54456, .T. ) ;
#20662 = ORIENTED_EDGE ( 'NONE', *, *, #11739, .T. ) ;
#20663 = CARTESIAN_POINT ( 'NONE',  ( 2.624215991343620935, -37.21129343241625520, 30.33228621715021944 ) ) ;
#20664 = CARTESIAN_POINT ( 'NONE',  ( 0.9730545539215883499, 16.88610103448612065, -39.44597740938043273 ) ) ;
#20665 = B_SPLINE_CURVE_WITH_KNOTS ( 'NONE', 3,
 ( #58315, #35178, #34552, #48952, #53321, #11356 ),
 .UNSPECIFIED., .F., .F.,
 ( 4, 2, 4 ),
 ( 5.421010862427522170E-19, 0.0002293801035737084233, 0.0004587602071474163046 ),
 .UNSPECIFIED. ) ;
#20666 = DIRECTION ( 'NONE',  ( -1.000000000000000000, -0.000000000000000000, -0.000000000000000000 ) ) ;
#20667 = ORIENTED_EDGE ( 'NONE', *, *, #41082, .T. ) ;
#20669 = CARTESIAN_POINT ( 'NONE',  ( -2.601141883200665639, 13.63649176842545607, -6.069721552019776922 ) ) ;
#20668 = B_SPLINE_CURVE_WITH_KNOTS ( 'NONE', 3,
 ( #12209, #50393, #45721, #2771, #35087, #54454 ),
 .UNSPECIFIED., .F., .F.,
 ( 4, 2, 4 ),
 ( 1.867239236438689166E-17, 0.0002293755540694308577, 0.0004587511081388430129 ),
 .UNSPECIFIED. ) ;
#20670 = EDGE_CURVE ( 'NONE', #36860, #11517, #6818, .T. ) ;
#20671 = LINE ( 'NONE', #41038, #16997 ) ;
#20672 = ORIENTED_EDGE ( 'NONE', *, *, #329, .T. ) ;
#20673 = AXIS2_PLACEMENT_3D ( 'NONE', #56139, #38005, #14187 ) ;
#20674 = CARTESIAN_POINT ( 'NONE',  ( 3.270143674763207553, -13.14781761974172092, 3.806843787665870060 ) ) ;
#20675 = ORIENTED_EDGE ( 'NONE', *, *, #55562, .T. ) ;
#20676 = CARTESIAN_POINT ( 'NONE',  ( 5.974727161628367256, -12.50710176109996574, -16.27409205901371791 ) ) ;
#20677 = VERTEX_POINT ( 'NONE', #8851 ) ;
#20678 = CARTESIAN_POINT ( 'NONE',  ( 0.1152809850208375703, 29.82811608494973399, -32.51505456419408091 ) ) ;
#20679 = DIRECTION ( 'NONE',  ( 0.000000000000000000, -0.7071067811865449082, -0.7071067811865500152 ) ) ;
#20680 = ORIENTED_EDGE ( 'NONE', *, *, #35608, .F. ) ;
#20681 = EDGE_LOOP ( 'NONE', ( #57308, #24674, #33811, #20087 ) ) ;
#20682 = CARTESIAN_POINT ( 'NONE',  ( 0.9783242366443554161, 20.37523131597068371, -36.62218506625746528 ) ) ;
#20683 = CARTESIAN_POINT ( 'NONE',  ( 0.6039202388192953519, -45.45307514328658272, 18.58982713388518704 ) ) ;
#20684 = VERTEX_POINT ( 'NONE', #22648 ) ;
#20685 = ORIENTED_EDGE ( 'NONE', *, *, #26487, .T. ) ;
#20686 = LINE ( 'NONE', #1243, #12405 ) ;
#20687 = CARTESIAN_POINT ( 'NONE',  ( 0.5832367798473377940, 34.05962365606865916, -33.67436043247226962 ) ) ;
#20688 = CARTESIAN_POINT ( 'NONE',  ( 0.5830082357119558134, 32.79753409158529820, -33.51945394020668800 ) ) ;
#20689 = CARTESIAN_POINT ( 'NONE',  ( 0.7048096507298579061, 34.61049487267059277, -33.41730025321717079 ) ) ;
#20690 = ORIENTED_EDGE ( 'NONE', *, *, #39942, .T. ) ;
#20691 = CARTESIAN_POINT ( 'NONE',  ( -6.078726893082806448, -11.01948708261742738, 15.79129335123464983 ) ) ;
#20692 = PLANE ( 'NONE',  #32932 ) ;
#20693 = ORIENTED_EDGE ( 'NONE', *, *, #16934, .T. ) ;
#20694 = FACE_OUTER_BOUND ( 'NONE', #27835, .T. ) ;
#20695 = VERTEX_POINT ( 'NONE', #27650 ) ;
#20696 = CARTESIAN_POINT ( 'NONE',  ( 0.9752132459055852243, 33.89922943039213266, -26.30543738863311276 ) ) ;
#20697 = EDGE_CURVE ( 'NONE', #23596, #28479, #41779, .T. ) ;
#20698 = CARTESIAN_POINT ( 'NONE',  ( 0.1158816050234199035, 25.24882932350766396, 36.18616668144803583 ) ) ;
#20699 = ORIENTED_EDGE ( 'NONE', *, *, #32821, .T. ) ;
#20700 = CARTESIAN_POINT ( 'NONE',  ( -6.077587904424778920, -14.66646125808257395, 12.47761738310216550 ) ) ;
#20701 = CARTESIAN_POINT ( 'NONE',  ( 50.50000000000000000, 12.21587082446438011, -2.649999999999992806 ) ) ;
#20702 = CARTESIAN_POINT ( 'NONE',  ( -17.97369999999976642, -12.32233744059949210, 2.099999999999994760 ) ) ;
#20703 = AXIS2_PLACEMENT_3D ( 'NONE', #5573, #30019, #15939 ) ;
#20704 = CIRCLE ( 'NONE', #26683, 15.43999999999999240 ) ;
#20705 = ORIENTED_EDGE ( 'NONE', *, *, #27870, .F. ) ;
#20706 = DIRECTION ( 'NONE',  ( 0.000000000000000000, 0.000000000000000000, 1.000000000000000000 ) ) ;
#20707 = CIRCLE ( 'NONE', #689, 12.50000000000000000 ) ;
#20708 = CARTESIAN_POINT ( 'NONE',  ( 0.8560838555295223751, 40.81790744942443183, 23.11430867518979326 ) ) ;
#20709 = CARTESIAN_POINT ( 'NONE',  ( 0.9769922540276048117, 41.59126474070951218, -5.147645321342566582 ) ) ;
#20710 =( LENGTH_UNIT ( ) NAMED_UNIT ( * ) SI_UNIT ( .MILLI., .METRE. ) );
#20711 = CARTESIAN_POINT ( 'NONE',  ( 1.157643937452370153, 20.86452789596350854, 36.35483118202194674 ) ) ;
#20712 =( BOUNDED_SURFACE ( )  B_SPLINE_SURFACE ( 3, 1, ( 
 ( #28222, #57027 ),
 ( #61106, #47339 ),
 ( #47049, #27611 ),
 ( #8810, #4385 ) ),
 .UNSPECIFIED., .F., .F., .F. ) 
 B_SPLINE_SURFACE_WITH_KNOTS ( ( 4, 4 ),
 ( 2, 2 ),
 ( 0.000000000000000000, 1.000000000000000000 ),
 ( 0.000000000000000000, 1.000000000000000000 ),
 .UNSPECIFIED. ) 
 GEOMETRIC_REPRESENTATION_ITEM ( )  RATIONAL_B_SPLINE_SURFACE ( (
 ( 1.000000000000000000, 1.000000000000000000),
 ( 0.7282232189291693025, 0.9929344683865674037),
 ( 0.7282232189291693025, 0.9929344683865674037),
 ( 1.000000000000000000, 1.000000000000000000) ) ) 
 REPRESENTATION_ITEM ( '' )  SURFACE ( )  );
#20713 = B_SPLINE_CURVE_WITH_KNOTS ( 'NONE', 3,
 ( #44044, #19595, #5754, #57150 ),
 .UNSPECIFIED., .F., .F.,
 ( 4, 4 ),
 ( 0.000000000000000000, 0.005004741218457414535 ),
 .UNSPECIFIED. ) ;
#20714 = CARTESIAN_POINT ( 'NONE',  ( 4.691466044806103852, 42.11359095667489782, -14.64802401911184759 ) ) ;
#20715 = AXIS2_PLACEMENT_3D ( 'NONE', #27583, #60773, #47313 ) ;
#20716 = CARTESIAN_POINT ( 'NONE',  ( 0.1064266379913945265, 6.185137063632448751, 42.67882137217593197 ) ) ;
#20717 = CARTESIAN_POINT ( 'NONE',  ( -17.97369999999976642, -7.719455939378113030, 2.099999999999994760 ) ) ;
#20718 = CARTESIAN_POINT ( 'NONE',  ( 0.7954196712028454019, -42.08256091708719993, 23.29293472883116678 ) ) ;
#20719 = CARTESIAN_POINT ( 'NONE',  ( 0.3676999524040366896, -26.85386693986640338, 34.99743438737744583 ) ) ;
#20720 = DIRECTION ( 'NONE',  ( 1.000000000000000000, 0.000000000000000000, 0.000000000000000000 ) ) ;
#20721 = CARTESIAN_POINT ( 'NONE',  ( 0.5786265663353196143, -28.58414684753461188, -38.43785771743232260 ) ) ;
#20722 = EDGE_CURVE ( 'NONE', #27605, #47270, #31450, .T. ) ;
#20723 = ADVANCED_FACE ( 'NONE', ( #17959 ), #1186, .F. ) ;
#20724 = CARTESIAN_POINT ( 'NONE',  ( -6.078075953587585900, 17.85074021576659931, 7.221235905047625359 ) ) ;
#20725 = CARTESIAN_POINT ( 'NONE',  ( -2.708315649062916552, 13.41752550814510414, -5.842990691604468267 ) ) ;
#20726 = ORIENTED_EDGE ( 'NONE', *, *, #1824, .F. ) ;
#20727 = ADVANCED_FACE ( 'NONE', ( #33600 ), #7585, .F. ) ;
#20728 = CARTESIAN_POINT ( 'NONE',  ( 0.8560838555295158248, -46.14148336882297485, 8.446084690930096173 ) ) ;
#20729 = CARTESIAN_POINT ( 'NONE',  ( 0.9762797500689124330, -0.8945891712305065191, 41.89897964629235361 ) ) ;
#20730 = CARTESIAN_POINT ( 'NONE',  ( 4.967162193818130511, 0.000000000000000000, 0.000000000000000000 ) ) ;
#20731 = EDGE_CURVE ( 'NONE', #30005, #58891, #33835, .T. ) ;
#20732 = EDGE_LOOP ( 'NONE', ( #35633, #2224, #7467, #16815 ) ) ;
#20733 = FACE_OUTER_BOUND ( 'NONE', #13543, .T. ) ;
#20734 = CARTESIAN_POINT ( 'NONE',  ( 4.975801465491694664, 14.85979367497109571, 45.55012473237758996 ) ) ;
#20735 = B_SPLINE_CURVE_WITH_KNOTS ( 'NONE', 3,
 ( #16382, #35506, #54565, #11695, #30777, #49897 ),
 .UNSPECIFIED., .F., .F.,
 ( 4, 2, 4 ),
 ( 0.000000000000000000, 0.0002450742804987342304, 0.0004901485609974684608 ),
 .UNSPECIFIED. ) ;
#20736 = CARTESIAN_POINT ( 'NONE',  ( 3.238018933889920792, -0.1726436309640175248, -13.39319553147569408 ) ) ;
#20737 = EDGE_LOOP ( 'NONE', ( #41817, #45342, #28826, #12521 ) ) ;
#20738 = VERTEX_POINT ( 'NONE', #54128 ) ;
#20739 = CARTESIAN_POINT ( 'NONE',  ( 5.960721111146673579, 5.306302591836580262, -19.82781442290492890 ) ) ;
#20740 = CIRCLE ( 'NONE', #6701, 11.40403086437694569 ) ;
#20741 = ORIENTED_EDGE ( 'NONE', *, *, #55727, .T. ) ;
#20742 = EDGE_CURVE ( 'NONE', #42579, #17351, #5377, .T. ) ;
#20743 = CARTESIAN_POINT ( 'NONE',  ( 0.5997462898726536595, 11.43624519451647714, 47.75734421002918140 ) ) ;
#20744 = CONICAL_SURFACE ( 'NONE', #23739, 43.92652462719577500, 1.486293639869522343 ) ;
#20745 = AXIS2_PLACEMENT_3D ( 'NONE', #7399, #40660, #16841 ) ;
#20746 = ORIENTED_EDGE ( 'NONE', *, *, #14867, .F. ) ;
#20747 = ORIENTED_EDGE ( 'NONE', *, *, #22412, .F. ) ;
#20748 = CARTESIAN_POINT ( 'NONE',  ( 0.1101816497532062816, 11.29256821151155954, 41.61967362528560699 ) ) ;
#20750 = EDGE_LOOP ( 'NONE', ( #10171, #41478, #25304, #37034 ) ) ;
#20749 = ADVANCED_FACE ( 'NONE', ( #10952 ), #49765, .F. ) ;
#20751 = LINE ( 'NONE', #54227, #44126 ) ;
#20752 = CARTESIAN_POINT ( 'NONE',  ( 0.6253024248130496510, 41.52618082144132217, -26.21107654795206088 ) ) ;
#20753 = ORIENTED_EDGE ( 'NONE', *, *, #2112, .T. ) ;
#20754 = CARTESIAN_POINT ( 'NONE',  ( 0.1119899015040011075, 37.28332007608033649, -23.59905405513218213 ) ) ;
#20755 = CARTESIAN_POINT ( 'NONE',  ( 4.553261556744875094, -29.69864478935419072, 32.36556910513705532 ) ) ;
#20756 = EDGE_LOOP ( 'NONE', ( #60700, #39624, #22985, #16143 ) ) ;
#20757 = CARTESIAN_POINT ( 'NONE',  ( 1.830465331921977246, 34.32868985341965384, -27.60284602764924600 ) ) ;
#20758 = CARTESIAN_POINT ( 'NONE',  ( 1.091591847532194404, 14.33333461224457750, 39.38673012385353189 ) ) ;
#20759 = FACE_OUTER_BOUND ( 'NONE', #26295, .T. ) ;
#20760 = CARTESIAN_POINT ( 'NONE',  ( 0.3622758884714730732, 11.95365414648439462, 41.42293301073630118 ) ) ;
#20761 = ORIENTED_EDGE ( 'NONE', *, *, #10604, .T. ) ;
#20762 = ORIENTED_EDGE ( 'NONE', *, *, #38598, .T. ) ;
#20763 = AXIS2_PLACEMENT_3D ( 'NONE', #39840, #5944, #53568 ) ;
#20764 = CARTESIAN_POINT ( 'NONE',  ( 0.1095718737110178975, 41.58781525899394182, 11.40943879390663263 ) ) ;
#20765 =( BOUNDED_SURFACE ( )  B_SPLINE_SURFACE ( 3, 1, ( 
 ( #22071, #13000 ),
 ( #22685, #7962 ),
 ( #42133, #18000 ),
 ( #55247, #36806 ) ),
 .UNSPECIFIED., .F., .F., .F. ) 
 B_SPLINE_SURFACE_WITH_KNOTS ( ( 4, 4 ),
 ( 2, 2 ),
 ( 0.000000000000000000, 1.000000000000000000 ),
 ( 0.000000000000000000, 1.000000000000000000 ),
 .UNSPECIFIED. ) 
 GEOMETRIC_REPRESENTATION_ITEM ( )  RATIONAL_B_SPLINE_SURFACE ( (
 ( 1.000000000000000000, 1.000000000000000000),
 ( 0.9953485035131437453, 0.8621029689291515030),
 ( 0.9953485035131437453, 0.8621029689291515030),
 ( 1.000000000000000000, 1.000000000000000000) ) ) 
 REPRESENTATION_ITEM ( '' )  SURFACE ( )  );
#20766 = FACE_OUTER_BOUND ( 'NONE', #25312, .T. ) ;
#20767 = EDGE_CURVE ( 'NONE', #51225, #34606, #15959, .T. ) ;
#20768 = DIRECTION ( 'NONE',  ( -1.000000000000000000, -0.000000000000000000, -0.000000000000000000 ) ) ;
#20769 = ORIENTED_EDGE ( 'NONE', *, *, #39159, .T. ) ;
#20770 = CARTESIAN_POINT ( 'NONE',  ( 1.227938101723756947, 42.65467462194918369, 4.762198645644581951 ) ) ;
#20771 = CARTESIAN_POINT ( 'NONE',  ( 0.8560838555295223751, -2.480523550130904642, -46.84250032821665854 ) ) ;
#20772 = CARTESIAN_POINT ( 'NONE',  ( 5.895596859100789899, -20.11288567981415909, -0.003583743010673907416 ) ) ;
#20773 = FILL_AREA_STYLE_COLOUR ( '', #37453 ) ;
#20774 = VERTEX_POINT ( 'NONE', #11568 ) ;
#20775 = ORIENTED_EDGE ( 'NONE', *, *, #9631, .F. ) ;
#20776 = LINE ( 'NONE', #34887, #51901 ) ;
#20777 = CARTESIAN_POINT ( 'NONE',  ( 3.894904216938897878, 42.36413768828274584, 11.72195249966583752 ) ) ;
#20778 = CARTESIAN_POINT ( 'NONE',  ( -2.000000000000009770, 3.464101615137749057, -5.600000000000000533 ) ) ;
#20779 = CARTESIAN_POINT ( 'NONE',  ( 0.9730545539215883499, -33.73144377768576874, 26.52009130076758225 ) ) ;
#20780 = B_SPLINE_CURVE_WITH_KNOTS ( 'NONE', 3,
 ( #57252, #46985, #42286, #28459, #33808, #28154, #9356, #19093, #32884, #38204, #4625, #57559, #14386 ),
 .UNSPECIFIED., .F., .F.,
 ( 4, 3, 3, 3, 4 ),
 ( 0.0005054209210070093961, 0.0005449106435901839799, 0.0006811373090491489642, 0.0008459866663933690491, 0.001010840725717212715 ),
 .UNSPECIFIED. ) ;
#20781 = CARTESIAN_POINT ( 'NONE',  ( 0.3622758884714730732, -43.10531414739105571, 0.8252992914326598983 ) ) ;
#20782 = B_SPLINE_CURVE_WITH_KNOTS ( 'NONE', 3,
 ( #61937, #5537, #24676, #4932 ),
 .UNSPECIFIED., .F., .F.,
 ( 4, 4 ),
 ( 0.000000000000000000, 0.004444103432399267029 ),
 .UNSPECIFIED. ) ;
#20783 =( BOUNDED_SURFACE ( )  B_SPLINE_SURFACE ( 3, 1, ( 
 ( #3607, #55933 ),
 ( #60619, #46561 ),
 ( #47177, #41874 ),
 ( #60311, #22741 ) ),
 .UNSPECIFIED., .F., .F., .F. ) 
 B_SPLINE_SURFACE_WITH_KNOTS ( ( 4, 4 ),
 ( 2, 2 ),
 ( 0.000000000000000000, 1.000000000000000000 ),
 ( 0.000000000000000000, 1.000000000000000000 ),
 .UNSPECIFIED. ) 
 GEOMETRIC_REPRESENTATION_ITEM ( )  RATIONAL_B_SPLINE_SURFACE ( (
 ( 1.000000000000000000, 1.000000000000000000),
 ( 0.9953040768229013402, 0.8617119497784988535),
 ( 0.9953040768229013402, 0.8617119497784988535),
 ( 1.000000000000000000, 1.000000000000000000) ) ) 
 REPRESENTATION_ITEM ( '' )  SURFACE ( )  );
#20784 = CARTESIAN_POINT ( 'NONE',  ( -6.077587904424778920, -6.656176160390447905, -18.06907137391903717 ) ) ;
#20785 = CARTESIAN_POINT ( 'NONE',  ( 0.5850706913938533704, -38.10903744847161789, 29.01314519953784554 ) ) ;
#20786 = CARTESIAN_POINT ( 'NONE',  ( 5.896782393890504181, 12.98055409426324580, -15.36331026452040049 ) ) ;
#20787 = FACE_OUTER_BOUND ( 'NONE', #47470, .T. ) ;
#20788 = FACE_OUTER_BOUND ( 'NONE', #56018, .T. ) ;
#20789 = CIRCLE ( 'NONE', #19815, 5.000000000000000000 ) ;
#20790 = VECTOR ( 'NONE', #52333, 1000.000000000000114 ) ;
#20791 = CARTESIAN_POINT ( 'NONE',  ( 1.157644175074336479, 15.83273920285144243, -38.81142415338135976 ) ) ;
#20792 = CARTESIAN_POINT ( 'NONE',  ( 4.553261556744875094, 0.000000000000000000, 0.000000000000000000 ) ) ;
#20793 = CARTESIAN_POINT ( 'NONE',  ( 0.7954190325252784577, 5.415566973723242583, -47.79303692714236007 ) ) ;
#20794 = CARTESIAN_POINT ( 'NONE',  ( 0.8751705887134553219, 33.37254303619554463, -34.63284514348550402 ) ) ;
#20795 = CARTESIAN_POINT ( 'NONE',  ( 0.5839879882012690704, -41.47910964649813081, 23.94800997596668779 ) ) ;
#20796 = CARTESIAN_POINT ( 'NONE',  ( 0.6846871229502932144, 47.37786444808393327, 7.109010606687553135 ) ) ;
#20797 = CARTESIAN_POINT ( 'NONE',  ( 0.9757402383260943557, -26.18833306844175723, 33.98983788393810102 ) ) ;
#20798 = CARTESIAN_POINT ( 'NONE',  ( 0.1103573494271549854, -0.06145187104197965405, -43.12440049163654976 ) ) ;
#20799 = ADVANCED_FACE ( 'NONE', ( #30037 ), #14480, .T. ) ;
#20800 = CARTESIAN_POINT ( 'NONE',  ( 0.3622758884714730732, -22.26738722580142138, -36.91764744403313614 ) ) ;
#20801 = CARTESIAN_POINT ( 'NONE',  ( 0.6024113833632039894, 49.02002248349460700, -2.929038207082721001 ) ) ;
#20803 = ORIENTED_EDGE ( 'NONE', *, *, #9358, .F. ) ;
#20802 = CARTESIAN_POINT ( 'NONE',  ( 4.956445790443988031, 0.000000000000000000, 0.000000000000000000 ) ) ;
#20804 = VERTEX_POINT ( 'NONE', #6200 ) ;
#20805 = AXIS2_PLACEMENT_3D ( 'NONE', #61285, #36285, #42529 ) ;
#20806 = CARTESIAN_POINT ( 'NONE',  ( 0.9762797500689124330, 36.31338395866826829, -20.92039508843077300 ) ) ;
#20807 = CARTESIAN_POINT ( 'NONE',  ( 1.479689385636123067, 43.88190798430054684, -3.995246791510194129 ) ) ;
#20808 = CARTESIAN_POINT ( 'NONE',  ( 4.549368137175248350, 13.99871866169305434, 40.58005590356696501 ) ) ;
#20809 = EDGE_CURVE ( 'NONE', #58899, #39657, #55451, .T. ) ;
#20810 = EDGE_LOOP ( 'NONE', ( #43365, #42573, #41957, #30774 ) ) ;
#20811 = EDGE_LOOP ( 'NONE', ( #46805, #28144, #48327, #15918 ) ) ;
#20812 = CARTESIAN_POINT ( 'NONE',  ( 0.1095718737110178698, -11.40943879390677651, 41.58781525899390630 ) ) ;
#20813 = DIRECTION ( 'NONE',  ( 0.000000000000000000, 0.000000000000000000, 1.000000000000000000 ) ) ;
#20814 = CARTESIAN_POINT ( 'NONE',  ( 0.8753041380234524160, 48.36002538446245325, 8.511537621788880514 ) ) ;
#20815 = ORIENTED_EDGE ( 'NONE', *, *, #4899, .F. ) ;
#20816 = EDGE_LOOP ( 'NONE', ( #6315, #32160, #59791, #42642 ) ) ;
#20817 = CARTESIAN_POINT ( 'NONE',  ( 0.7413678028165008316, 28.94854816926588015, -33.26360850331690244 ) ) ;
#20818 = CARTESIAN_POINT ( 'NONE',  ( 0.5549461598389363592, -40.54382484153107669, 17.36133527946660848 ) ) ;
#20819 = CARTESIAN_POINT ( 'NONE',  ( -6.078075953587585900, -18.27338415406089212, 6.072775790793892625 ) ) ;
#20820 = FACE_OUTER_BOUND ( 'NONE', #45362, .T. ) ;
#20821 = VERTEX_POINT ( 'NONE', #25344 ) ;
#20822 = EDGE_CURVE ( 'NONE', #21575, #41654, #33057, .T. ) ;
#20823 = CARTESIAN_POINT ( 'NONE',  ( 0.1365634738349413013, -2.050550585729402631, 44.07559258726546858 ) ) ;
#20824 = DIRECTION ( 'NONE',  ( 1.000000000000000000, 0.000000000000000000, 0.000000000000000000 ) ) ;
#20825 = CARTESIAN_POINT ( 'NONE',  ( 0.9749527285493297946, 42.50314808877163131, 5.883724875809256183 ) ) ;
#20826 = ORIENTED_EDGE ( 'NONE', *, *, #8687, .T. ) ;
#20827 = AXIS2_PLACEMENT_3D ( 'NONE', #23122, #36935, #8381 ) ;
#20828 = ORIENTED_EDGE ( 'NONE', *, *, #38205, .T. ) ;
#20829 = CARTESIAN_POINT ( 'NONE',  ( 0.1368894036331288200, 34.00722248154819738, 28.11352245830850549 ) ) ;
#20830 = LINE ( 'NONE', #35867, #7523 ) ;
#20831 = AXIS2_PLACEMENT_3D ( 'NONE', #50899, #7995, #31180 ) ;
#20832 = EDGE_LOOP ( 'NONE', ( #23823, #26150, #26266, #16668 ) ) ;
#20833 = CARTESIAN_POINT ( 'NONE',  ( 4.833616638992208614, 20.86133030530232801, 41.27831852777651278 ) ) ;
#20834 = CARTESIAN_POINT ( 'NONE',  ( 0.6028777368367060907, -7.923479829246307560, 48.46398969035256954 ) ) ;
#20835 = CARTESIAN_POINT ( 'NONE',  ( -6.078726893082806448, 15.43407385306378998, -11.51448676958260187 ) ) ;
#20836 = DIRECTION ( 'NONE',  ( -1.626303258728256898E-16, 1.000000000000000000, 0.000000000000000000 ) ) ;
#20837 = ORIENTED_EDGE ( 'NONE', *, *, #16685, .F. ) ;
#20838 = CARTESIAN_POINT ( 'NONE',  ( 0.5835871038041837711, -14.02451996763116426, 44.74983008435918919 ) ) ;
#20839 = CARTESIAN_POINT ( 'NONE',  ( 4.967162193818130511, 0.000000000000000000, 0.000000000000000000 ) ) ;
#20840 = CARTESIAN_POINT ( 'NONE',  ( 4.958415959904820980, -27.34909152584742031, 36.26611568025254684 ) ) ;
#20841 = EDGE_CURVE ( 'NONE', #45571, #45978, #59458, .T. ) ;
#20842 = ORIENTED_EDGE ( 'NONE', *, *, #27426, .F. ) ;
#20843 = CARTESIAN_POINT ( 'NONE',  ( 5.959547316686252039, -10.25972575517542396, 17.77749189599199653 ) ) ;
#20844 = CARTESIAN_POINT ( 'NONE',  ( 5.910764540655178756, 10.80896614705666359, -16.96076322872724162 ) ) ;
#20845 = EDGE_LOOP ( 'NONE', ( #57459, #27518, #51147, #53293 ) ) ;
#20846 = DIRECTION ( 'NONE',  ( 0.000000000000000000, 0.000000000000000000, 1.000000000000000000 ) ) ;
#20847 = CARTESIAN_POINT ( 'NONE',  ( 0.1158516988532803799, 9.866537107317912003, 43.00690182218099977 ) ) ;
#20848 = AXIS2_PLACEMENT_3D ( 'NONE', #56747, #5350, #47077 ) ;
#20849 = ORIENTED_EDGE ( 'NONE', *, *, #37047, .F. ) ;
#20850 = CARTESIAN_POINT ( 'NONE',  ( 0.6041374136657475802, 12.61972904329599210, -46.42299778158143653 ) ) ;
#20851 = CARTESIAN_POINT ( 'NONE',  ( 4.963659409799330291, -40.34793212403957341, -19.36487359954742971 ) ) ;
#20852 = DIRECTION ( 'NONE',  ( -0.07906939808003034253, -0.9951496949144243986, -0.05852448204802653681 ) ) ;
#20853 = ADVANCED_FACE ( 'NONE', ( #1513 ), #14037, .F. ) ;
#20854 = CARTESIAN_POINT ( 'NONE',  ( 0.6025881611877910160, -41.77096849334466810, 23.86454577211492278 ) ) ;
#20855 = CARTESIAN_POINT ( 'NONE',  ( 3.240649175237396040, -36.31843312004634328, 24.82410790144071910 ) ) ;
#20856 = CARTESIAN_POINT ( 'NONE',  ( 0.5834872094924180574, 46.32218741137614160, -12.17696997821474625 ) ) ;
#20857 = CARTESIAN_POINT ( 'NONE',  ( -5.995132425357893702, -2.451215106828474877, 18.68405145320023308 ) ) ;
#20858 = EDGE_CURVE ( 'NONE', #41370, #3302, #19197, .T. ) ;
#20859 = CYLINDRICAL_SURFACE ( 'NONE', #3606, 10.00000000000000000 ) ;
#20860 = CARTESIAN_POINT ( 'NONE',  ( 1.157643937452367711, 14.29172636799923701, -39.40493410750726611 ) ) ;
#20861 =( BOUNDED_SURFACE ( )  B_SPLINE_SURFACE ( 3, 1, ( 
 ( #30558, #40312 ),
 ( #2043, #45610 ),
 ( #59368, #2664 ),
 ( #59682, #21173 ) ),
 .UNSPECIFIED., .F., .F., .F. ) 
 B_SPLINE_SURFACE_WITH_KNOTS ( ( 4, 4 ),
 ( 2, 2 ),
 ( 0.000000000000000000, 1.000000000000000000 ),
 ( 0.000000000000000000, 1.000000000000000000 ),
 .UNSPECIFIED. ) 
 GEOMETRIC_REPRESENTATION_ITEM ( )  RATIONAL_B_SPLINE_SURFACE ( (
 ( 1.000000000000000000, 1.000000000000000000),
 ( 0.9754377213608244057, 0.9999580625633939235),
 ( 0.9754377213608244057, 0.9999580625633939235),
 ( 1.000000000000000000, 1.000000000000000000) ) ) 
 REPRESENTATION_ITEM ( '' )  SURFACE ( )  );
#20862 = CARTESIAN_POINT ( 'NONE',  ( 0.9787284016396593511, 15.23687772655018868, 39.04066541537156354 ) ) ;
#20863 = ORIENTED_EDGE ( 'NONE', *, *, #19813, .F. ) ;
#20864 = CARTESIAN_POINT ( 'NONE',  ( 4.303969348037246512, 35.51084504003240738, -32.45857549159264721 ) ) ;
#20865 = CARTESIAN_POINT ( 'NONE',  ( 2.282803330402972453, 23.71786253601074890, -40.54577541717364397 ) ) ;
#20866 = CARTESIAN_POINT ( 'NONE',  ( -6.063463321072276813, -14.67303933398442695, -12.47086080360196014 ) ) ;
#20867 = CARTESIAN_POINT ( 'NONE',  ( 2.526552050251864134, -4.405466163647019151, -42.75269566045970748 ) ) ;
#20868 = FACE_OUTER_BOUND ( 'NONE', #38724, .T. ) ;
#20869 = CARTESIAN_POINT ( 'NONE',  ( 0.2885700199627512785, -0.8047882683535816373, -43.10898996868493072 ) ) ;
#20870 = CARTESIAN_POINT ( 'NONE',  ( -1.599999999999961231, 56.56854249492372588, 56.56854249492390352 ) ) ;
#20871 = CARTESIAN_POINT ( 'NONE',  ( 0.7954190325252793459, 46.67728753507125816, 11.60747917225601000 ) ) ;
#20872 = EDGE_CURVE ( 'NONE', #52483, #2209, #53216, .T. ) ;
#20873 = LINE ( 'NONE', #6732, #35464 ) ;
#20875 = ORIENTED_EDGE ( 'NONE', *, *, #22373, .T. ) ;
#20874 = CARTESIAN_POINT ( 'NONE',  ( 0.5997462898726536595, -25.90236585764290922, 41.72072714036901431 ) ) ;
#20876 = ORIENTED_EDGE ( 'NONE', *, *, #38831, .F. ) ;
#20877 = CARTESIAN_POINT ( 'NONE',  ( 5.960721111146673579, 17.77882586010667154, -10.25731071096564051 ) ) ;
#20878 = VECTOR ( 'NONE', #35571, 1000.000000000000000 ) ;
#20879 = CARTESIAN_POINT ( 'NONE',  ( 4.975610109902397937, -4.123593823332411645, 48.73854102369035957 ) ) ;
#20880 = CARTESIAN_POINT ( 'NONE',  ( 5.958863334805807099, -16.28483817244731213, -12.49425770716481487 ) ) ;
#20881 = EDGE_CURVE ( 'NONE', #51998, #56250, #1604, .T. ) ;
#20882 =( BOUNDED_SURFACE ( )  B_SPLINE_SURFACE ( 3, 1, ( 
 ( #61396, #32935 ),
 ( #17912, #7 ),
 ( #37324, #57305 ),
 ( #19148, #32620 ) ),
 .UNSPECIFIED., .F., .F., .F. ) 
 B_SPLINE_SURFACE_WITH_KNOTS ( ( 4, 4 ),
 ( 2, 2 ),
 ( 0.000000000000000000, 1.000000000000000000 ),
 ( 0.000000000000000000, 1.000000000000000000 ),
 .UNSPECIFIED. ) 
 GEOMETRIC_REPRESENTATION_ITEM ( )  RATIONAL_B_SPLINE_SURFACE ( (
 ( 1.000000000000000000, 1.000000000000000000),
 ( 0.9729067724841187204, 0.9999501103223794596),
 ( 0.9729067724841187204, 0.9999501103223794596),
 ( 1.000000000000000000, 1.000000000000000000) ) ) 
 REPRESENTATION_ITEM ( '' )  SURFACE ( )  );
#20883 = VERTEX_POINT ( 'NONE', #55069 ) ;
#20884 = CARTESIAN_POINT ( 'NONE',  ( 0.5980894510889448457, 42.01322166096920085, -23.44630161211543395 ) ) ;
#20885 = CARTESIAN_POINT ( 'NONE',  ( 0.5797568599927167554, 32.14649101875688331, 34.14422972995566141 ) ) ;
#20886 = EDGE_CURVE ( 'NONE', #1157, #54460, #2392, .T. ) ;
#20887 = ORIENTED_EDGE ( 'NONE', *, *, #18067, .T. ) ;
#20888 = ORIENTED_EDGE ( 'NONE', *, *, #4638, .T. ) ;
#20889 = DIRECTION ( 'NONE',  ( -0.000000000000000000, 0.000000000000000000, -1.000000000000000000 ) ) ;
#20890 = CARTESIAN_POINT ( 'NONE',  ( 0.1102144999581333440, -11.03964818279745153, -41.68747259405346028 ) ) ;
#20891 = CARTESIAN_POINT ( 'NONE',  ( 4.549368137175248350, 8.582197505784431968, -42.06008734272388239 ) ) ;
#20892 = ORIENTED_EDGE ( 'NONE', *, *, #53087, .F. ) ;
#20893 = EDGE_CURVE ( 'NONE', #60938, #34351, #17806, .T. ) ;
#20894 = DIRECTION ( 'NONE',  ( -0.07500201931887527651, 0.6023261099427817955, 0.7947187894968175126 ) ) ;
#20895 = DIRECTION ( 'NONE',  ( 0.1011922191286468431, 0.6592733245820293631, -0.7450629626295874885 ) ) ;
#20896 = ORIENTED_EDGE ( 'NONE', *, *, #13784, .F. ) ;
#20897 = CARTESIAN_POINT ( 'NONE',  ( 0.9758171775293918992, 41.44488232057081945, -11.11125068417950601 ) ) ;
#20898 = ORIENTED_EDGE ( 'NONE', *, *, #41027, .F. ) ;
#20899 = CARTESIAN_POINT ( 'NONE',  ( 0.3622758884714600280, -36.91764744403305087, -22.26738722580154217 ) ) ;
#20900 = CARTESIAN_POINT ( 'NONE',  ( 5.965394784446460541, 19.82972329408686107, -5.298374383010430400 ) ) ;
#20901 = EDGE_LOOP ( 'NONE', ( #31015, #21898, #38197, #40876 ) ) ;
#20902 = CARTESIAN_POINT ( 'NONE',  ( 0.7954196712028460681, 23.29293472883130889, 42.08256091708710755 ) ) ;
#20903 = CARTESIAN_POINT ( 'NONE',  ( -6.078726893082806448, -18.27610589745688330, -6.064486333867170842 ) ) ;
#20904 = CARTESIAN_POINT ( 'NONE',  ( 0.5839254288179566155, 41.52446060675855222, -23.86932519546686038 ) ) ;
#20905 = CARTESIAN_POINT ( 'NONE',  ( 3.783278058412225864, 33.06594414781534397, -27.54892951149511049 ) ) ;
#20906 = ORIENTED_EDGE ( 'NONE', *, *, #34798, .F. ) ;
#20907 = DIRECTION ( 'NONE',  ( -1.000000000000000000, -0.000000000000000000, -0.000000000000000000 ) ) ;
#20908 = DIRECTION ( 'NONE',  ( -1.000000000000000000, -0.000000000000000000, -0.000000000000000000 ) ) ;
#20909 = VERTEX_POINT ( 'NONE', #50676 ) ;
#20910 = CARTESIAN_POINT ( 'NONE',  ( 5.895596859100789899, 8.469463536102802337, 18.24270732712424348 ) ) ;
#20911 = VERTEX_POINT ( 'NONE', #8379 ) ;
#20912 = CARTESIAN_POINT ( 'NONE',  ( 0.1129192098497455998, 44.06201484046248140, -2.343210614524073421 ) ) ;
#20913 = VERTEX_POINT ( 'NONE', #60086 ) ;
#20914 = CARTESIAN_POINT ( 'NONE',  ( 1.231276596079881935, -40.90292846002442673, -9.177538581351248226 ) ) ;
#20915 = CARTESIAN_POINT ( 'NONE',  ( 0.6016117650947689910, -30.88963369689275851, -38.17566743773167559 ) ) ;
#20916 = EDGE_CURVE ( 'NONE', #14826, #988, #51463, .T. ) ;
#20917 = CONICAL_SURFACE ( 'NONE', #55917, 42.08604991992415023, 1.569615340895231137 ) ;
#20918 = B_SPLINE_CURVE_WITH_KNOTS ( 'NONE', 3,
 ( #25156, #58976, #16384, #20171 ),
 .UNSPECIFIED., .F., .F.,
 ( 4, 4 ),
 ( 4.336808689942017736E-19, 0.004446298630425097112 ),
 .UNSPECIFIED. ) ;
#20919 = CARTESIAN_POINT ( 'NONE',  ( 0.7044674535452954967, -42.37103341363646791, -24.82938280085530636 ) ) ;
#20920 = ORIENTED_EDGE ( 'NONE', *, *, #47258, .T. ) ;
#20921 = CARTESIAN_POINT ( 'NONE',  ( 0.5832367798473389042, 5.981481162905716076, 47.52096797443089571 ) ) ;
#20922 = EDGE_CURVE ( 'NONE', #57497, #24606, #60375, .T. ) ;
#20923 = CARTESIAN_POINT ( 'NONE',  ( 0.5997462898726536595, 40.86908001809362645, -27.22627276398607421 ) ) ;
#20924 = CARTESIAN_POINT ( 'NONE',  ( 5.895596859100789899, -7.232071727009982354, -18.76766692340500242 ) ) ;
#20925 = ORIENTED_EDGE ( 'NONE', *, *, #25688, .T. ) ;
#20926 = EDGE_CURVE ( 'NONE', #4535, #13345, #13117, .T. ) ;
#20927 = ORIENTED_EDGE ( 'NONE', *, *, #24714, .F. ) ;
#20928 = CYLINDRICAL_SURFACE ( 'NONE', #52523, 13.50000000000000178 ) ;
#20929 = CARTESIAN_POINT ( 'NONE',  ( 0.8753041380234524160, 48.01981714478404939, -10.25843502950054287 ) ) ;
#20930 = CARTESIAN_POINT ( 'NONE',  ( 0.7764146366350259676, 27.10005286464496521, -38.28351614471450404 ) ) ;
#20931 = CARTESIAN_POINT ( 'NONE',  ( 4.549368137175248350, -42.06008734272390370, -8.582197505784284530 ) ) ;
#20932 = CARTESIAN_POINT ( 'NONE',  ( 0.5830082357119567016, -30.06822118592455695, -35.98797173574322983 ) ) ;
#20933 = AXIS2_PLACEMENT_3D ( 'NONE', #59427, #25933, #45070 ) ;
#20934 = CARTESIAN_POINT ( 'NONE',  ( -6.078457390727109555, -16.14063570603411080, 10.50116136637299391 ) ) ;
#20935 = ORIENTED_EDGE ( 'NONE', *, *, #12752, .T. ) ;
#20936 = EDGE_CURVE ( 'NONE', #36860, #36466, #55679, .T. ) ;
#20937 = DIRECTION ( 'NONE',  ( 1.000000000000000000, 0.000000000000000000, 0.000000000000000000 ) ) ;
#20938 = DIRECTION ( 'NONE',  ( 1.000000000000000000, 0.000000000000000000, 0.000000000000000000 ) ) ;
#20939 = AXIS2_PLACEMENT_3D ( 'NONE', #42112, #37712, #42410 ) ;
#20940 = VERTEX_POINT ( 'NONE', #7766 ) ;
#20941 = FACE_OUTER_BOUND ( 'NONE', #19733, .T. ) ;
#20942 = CARTESIAN_POINT ( 'NONE',  ( 0.6029442701453591180, -19.95751149647216138, -44.86917605691526489 ) ) ;
#20943 = CARTESIAN_POINT ( 'NONE',  ( 0.1365634738349411625, -38.12893165387313843, -22.20466596365546508 ) ) ;
#20944 = CARTESIAN_POINT ( 'NONE',  ( -6.057079549204054558, -4.276794256740572564, -18.77605554916285868 ) ) ;
#20945 = CARTESIAN_POINT ( 'NONE',  ( -6.078726893082806448, 19.09835798914749816, 2.459016752095430025 ) ) ;
#20946 = FILL_AREA_STYLE ('',( #1818 ) ) ;
#20947 = CARTESIAN_POINT ( 'NONE',  ( 5.965394784446458765, -19.82223131420057882, 5.326334832595306601 ) ) ;
#20948 = ORIENTED_EDGE ( 'NONE', *, *, #7265, .T. ) ;
#20949 = CARTESIAN_POINT ( 'NONE',  ( 0.1158516988532803521, 20.36546015188544700, -39.14320109079942966 ) ) ;
#20950 = FACE_OUTER_BOUND ( 'NONE', #34153, .T. ) ;
#20951 = EDGE_CURVE ( 'NONE', #5687, #37326, #18061, .T. ) ;
#20952 = CARTESIAN_POINT ( 'NONE',  ( 0.1140933569871964842, 29.38290660318237002, 32.91800038933968153 ) ) ;
#20953 = DIRECTION ( 'NONE',  ( 0.000000000000000000, -0.4999999999999989453, 0.8660254037844391517 ) ) ;
#20954 = EDGE_CURVE ( 'NONE', #49864, #4461, #45701, .T. ) ;
#20955 = DIRECTION ( 'NONE',  ( 0.000000000000000000, 0.000000000000000000, -1.000000000000000000 ) ) ;
#20956 = CARTESIAN_POINT ( 'NONE',  ( 0.9791128995231621612, 9.720239283517752682, 40.76584823743178987 ) ) ;
#20957 = CARTESIAN_POINT ( 'NONE',  ( 0.1147471544378676211, -6.735538612062173414, 43.60716349498859046 ) ) ;
#20958 = CARTESIAN_POINT ( 'NONE',  ( 0.8760168074886965917, 47.80016357497249402, -5.394043284319003817 ) ) ;
#20959 = DIRECTION ( 'NONE',  ( -0.000000000000000000, 1.000000000000000000, -0.000000000000000000 ) ) ;
#20960 = EDGE_CURVE ( 'NONE', #60741, #42039, #7443, .T. ) ;
#20961 =( BOUNDED_SURFACE ( )  B_SPLINE_SURFACE ( 3, 1, ( 
 ( #8273, #46518 ),
 ( #41833, #3258 ),
 ( #2648, #7978 ),
 ( #45594, #46837 ) ),
 .UNSPECIFIED., .F., .F., .F. ) 
 B_SPLINE_SURFACE_WITH_KNOTS ( ( 4, 4 ),
 ( 2, 2 ),
 ( 0.000000000000000000, 1.000000000000000000 ),
 ( 0.000000000000000000, 1.000000000000000000 ),
 .UNSPECIFIED. ) 
 GEOMETRIC_REPRESENTATION_ITEM ( )  RATIONAL_B_SPLINE_SURFACE ( (
 ( 1.000000000000000000, 1.000000000000000000),
 ( 0.9953485035131437453, 0.8621029689291523912),
 ( 0.9953485035131437453, 0.8621029689291523912),
 ( 1.000000000000000000, 1.000000000000000000) ) ) 
 REPRESENTATION_ITEM ( '' )  SURFACE ( )  );
#20962 = AXIS2_PLACEMENT_3D ( 'NONE', #17661, #51456, #27058 ) ;
#20963 = ORIENTED_EDGE ( 'NONE', *, *, #52684, .F. ) ;
#20964 = CARTESIAN_POINT ( 'NONE',  ( 0.1073791018717483448, -25.86618856530736466, 34.50606437925502945 ) ) ;
#20965 = CARTESIAN_POINT ( 'NONE',  ( 0.1158403557922069033, -38.42759882943639838, -21.68547798384251379 ) ) ;
#20966 = CARTESIAN_POINT ( 'NONE',  ( 0.5848930533535030563, 32.73270734968706819, -33.58337314724803946 ) ) ;
#20967 = CARTESIAN_POINT ( 'NONE',  ( 0.1073791018717578927, -5.147744207006579309, -42.81622261970993293 ) ) ;
#20968 = ORIENTED_EDGE ( 'NONE', *, *, #30480, .F. ) ;
#20969 = CARTESIAN_POINT ( 'NONE',  ( 4.694002226626921015, -15.42074131724369934, -42.90088004543483891 ) ) ;
#20970 = CARTESIAN_POINT ( 'NONE',  ( 5.974727161628367256, 10.27590650342012779, 17.76736931401863373 ) ) ;
#20971 = EDGE_CURVE ( 'NONE', #24192, #11621, #2463, .T. ) ;
#20972 = DIRECTION ( 'NONE',  ( 0.000000000000000000, 0.000000000000000000, -1.000000000000000000 ) ) ;
#20973 = ORIENTED_EDGE ( 'NONE', *, *, #38930, .T. ) ;
#20974 = CARTESIAN_POINT ( 'NONE',  ( 5.959547316686252039, -20.34955788964374790, -2.682663672454841386 ) ) ;
#20975 = EDGE_CURVE ( 'NONE', #36033, #24949, #47475, .T. ) ;
#20976 = CARTESIAN_POINT ( 'NONE',  ( 4.975610109902397937, -11.44439439467595143, 47.55497076097179843 ) ) ;
#20977 = VERTEX_POINT ( 'NONE', #50080 ) ;
#20978 = CARTESIAN_POINT ( 'NONE',  ( 2.526464513654345545, -40.15570173027679601, -15.32058692775033570 ) ) ;
#20979 = ORIENTED_EDGE ( 'NONE', *, *, #55583, .F. ) ;
#20980 = DIRECTION ( 'NONE',  ( 0.07906939808003035641, -0.8617947135858070595, 0.5010567851280115503 ) ) ;
#20981 = VERTEX_POINT ( 'NONE', #17190 ) ;
#20982 = CARTESIAN_POINT ( 'NONE',  ( 7.000000000000006217, 8.392413579938656024E-13, -80.00000000000001421 ) ) ;
#20983 = CARTESIAN_POINT ( 'NONE',  ( 0.5988103622719989083, -28.80261254780011271, -38.53259676306911530 ) ) ;
#20984 = ORIENTED_EDGE ( 'NONE', *, *, #15510, .T. ) ;
#20985 = B_SPLINE_CURVE_WITH_KNOTS ( 'NONE', 3,
 ( #5922, #15062, #48261, #20073 ),
 .UNSPECIFIED., .F., .F.,
 ( 4, 4 ),
 ( 4.336808689942017736E-19, 0.004446298630425057213 ),
 .UNSPECIFIED. ) ;
#20986 = ORIENTED_EDGE ( 'NONE', *, *, #61650, .T. ) ;
#20987 = DIRECTION ( 'NONE',  ( -1.000000000000000000, -0.000000000000000000, -0.000000000000000000 ) ) ;
#20988 = CARTESIAN_POINT ( 'NONE',  ( 0.5807400328401574052, -12.92266817606047269, 46.12278621143493496 ) ) ;
#20989 = ORIENTED_EDGE ( 'NONE', *, *, #18831, .F. ) ;
#20990 = ORIENTED_EDGE ( 'NONE', *, *, #235, .T. ) ;
#20991 = CARTESIAN_POINT ( 'NONE',  ( 0.9757954354143110187, -0.03224588977114339200, -42.90846090505964838 ) ) ;
#20992 = CARTESIAN_POINT ( 'NONE',  ( 5.894904586330512508, 3.344157678208356188, 19.83295291894080847 ) ) ;
#20993 = CARTESIAN_POINT ( 'NONE',  ( 0.5832366564991509073, 33.67434452455960070, -34.05963937630765770 ) ) ;
#20994 = CARTESIAN_POINT ( 'NONE',  ( 0.3676999524040366896, -32.25712563511761743, -30.09033780274121739 ) ) ;
#20995 = CARTESIAN_POINT ( 'NONE',  ( -6.016104459813371719, -13.32039631884693875, 13.32794178584992828 ) ) ;
#20996 = ORIENTED_EDGE ( 'NONE', *, *, #28778, .T. ) ;
#20997 = EDGE_CURVE ( 'NONE', #31990, #44428, #34484, .T. ) ;
#20998 = CARTESIAN_POINT ( 'NONE',  ( 9.999999999999991118, 80.00000000000001421, -1.319262011905257654E-31 ) ) ;
#20999 = CARTESIAN_POINT ( 'NONE',  ( 2.648799415243708655, -42.02883204265824446, 25.26053721557843446 ) ) ;
#21001 = VERTEX_POINT ( 'NONE', #21889 ) ;
#21000 = B_SPLINE_CURVE_WITH_KNOTS ( 'NONE', 3,
 ( #763, #20496, #15192, #20808 ),
 .UNSPECIFIED., .F., .F.,
 ( 4, 4 ),
 ( 2.343940034265377226E-17, 0.004564976165746188579 ),
 .UNSPECIFIED. ) ;
#21002 = DIRECTION ( 'NONE',  ( 0.1011922191286468292, -0.9882612224441065241, -0.1144547552577001859 ) ) ;
#21003 = EDGE_CURVE ( 'NONE', #20493, #50622, #9061, .T. ) ;
#21004 = B_SPLINE_CURVE_WITH_KNOTS ( 'NONE', 3,
 ( #59667, #7343, #54036, #49353, #6406, #22117 ),
 .UNSPECIFIED., .F., .F.,
 ( 4, 2, 4 ),
 ( 4.770489558936219510E-18, 0.0002291472222819944263, 0.0004582944445639840821 ),
 .UNSPECIFIED. ) ;
#21005 = VERTEX_POINT ( 'NONE', #52849 ) ;
#21006 = CARTESIAN_POINT ( 'NONE',  ( 4.975610109902397937, 38.85236532789244279, 29.71435874397685595 ) ) ;
#21007 = CARTESIAN_POINT ( 'NONE',  ( 0.9769922540276045897, 40.53405221617700960, -10.64528844242186700 ) ) ;
#21008 = ORIENTED_EDGE ( 'NONE', *, *, #35046, .T. ) ;
#21009 = CARTESIAN_POINT ( 'NONE',  ( 0.9787464366903556590, -12.24730775580737330, -40.07913978149986178 ) ) ;
#21010 = CARTESIAN_POINT ( 'NONE',  ( 4.694002226626920127, -34.48859517587359846, 29.81311077765690598 ) ) ;
#21011 = LINE ( 'NONE', #40155, #52695 ) ;
#21012 = CARTESIAN_POINT ( 'NONE',  ( -19.79687759653248946, -12.45625484602615529, 1.051131599843221132 ) ) ;
#21013 = EDGE_CURVE ( 'NONE', #8559, #34089, #24478, .T. ) ;
#21014 = EDGE_CURVE ( 'NONE', #12545, #25700, #49304, .T. ) ;
#21015 = CIRCLE ( 'NONE', #45045, 2.041999999999999815 ) ;
#21016 = ORIENTED_EDGE ( 'NONE', *, *, #3513, .T. ) ;
#21017 = DIRECTION ( 'NONE',  ( -0.07906939808003035641, -0.9940710100007921213, 0.07463817631257134433 ) ) ;
#21018 = ORIENTED_EDGE ( 'NONE', *, *, #22675, .F. ) ;
#21019 = EDGE_CURVE ( 'NONE', #11417, #19272, #4284, .T. ) ;
#21020 = CARTESIAN_POINT ( 'NONE',  ( 4.549368137175248350, 32.13400537129885493, 28.46244473166684941 ) ) ;
#21021 = CARTESIAN_POINT ( 'NONE',  ( 2.678494666091051801, 3.072372537026355044, -5.565789719053469753 ) ) ;
#21022 = VECTOR ( 'NONE', #56389, 1000.000000000000000 ) ;
#21023 = ADVANCED_FACE ( 'NONE', ( #18732 ), #20414, .F. ) ;
#21024 = CARTESIAN_POINT ( 'NONE',  ( 0.2230388203127582347, -25.64246103889320594, 34.66629317821121958 ) ) ;
#21025 = CARTESIAN_POINT ( 'NONE',  ( 4.963659409799330291, -3.403493583737023265, -44.62477100936220609 ) ) ;
#21026 = CIRCLE ( 'NONE', #41092, 42.08604991992415023 ) ;
#21027 = CARTESIAN_POINT ( 'NONE',  ( 4.975610109902397937, -48.84566763821283786, -2.559328059280381318 ) ) ;
#21028 = CARTESIAN_POINT ( 'NONE',  ( 4.956653778117001252, 45.71126949320271393, -14.93973939759840519 ) ) ;
#21029 = CARTESIAN_POINT ( 'NONE',  ( 0.5988103564986357874, 47.61318305157295327, -6.880138274944463284 ) ) ;
#21030 = CARTESIAN_POINT ( 'NONE',  ( 0.1129192098497455998, -43.69739906996312584, -6.122834499277253428 ) ) ;
#21031 = CARTESIAN_POINT ( 'NONE',  ( 4.956653778116970166, 36.51451553856417576, 31.29546495791861460 ) ) ;
#21032 = CARTESIAN_POINT ( 'NONE',  ( 0.5839879327111922036, 33.93179405280490357, 33.80333292213272500 ) ) ;
#21033 = CARTESIAN_POINT ( 'NONE',  ( 0.6021447746440204973, -45.41982514268575954, 18.67031395280587347 ) ) ;
#21034 = VERTEX_POINT ( 'NONE', #42549 ) ;
#21035 = CARTESIAN_POINT ( 'NONE',  ( 0.3676999524040366896, -2.238562284875889041, -44.05609404179596567 ) ) ;
#21036 = B_SPLINE_CURVE_WITH_KNOTS ( 'NONE', 3,
 ( #23380, #56571, #31861, #55952, #46901, #42507, #8038, #36884, #27150, #51553, #46277, #60639, #3935, #60333, #36568, #37188 ),
 .UNSPECIFIED., .F., .F.,
 ( 4, 3, 3, 3, 3, 4 ),
 ( 1.250973872328959318E-17, 0.0002724568934985507223, 0.0004086836638483677328, 0.0005449104342063536104, 0.0008173270854453667817, 0.001089761613562691177 ),
 .UNSPECIFIED. ) ;
#21037 = CARTESIAN_POINT ( 'NONE',  ( 0.5980894510889457338, -47.60453381548698104, 6.974827154143293129 ) ) ;
#21038 = CARTESIAN_POINT ( 'NONE',  ( 2.533389852662419894, -42.14803637618723542, 12.68832382015906113 ) ) ;
#21039 = VERTEX_POINT ( 'NONE', #61308 ) ;
#21040 = LINE ( 'NONE', #21974, #28310 ) ;
#21041 = CARTESIAN_POINT ( 'NONE',  ( 0.9972139404380286898, -4.947665363829067076, 42.62325912566431896 ) ) ;
#21042 = EDGE_CURVE ( 'NONE', #49963, #49511, #26905, .T. ) ;
#21043 = CARTESIAN_POINT ( 'NONE',  ( 0.6023142530420679819, -12.70386526143740369, -46.39979989577476260 ) ) ;
#21044 = ORIENTED_EDGE ( 'NONE', *, *, #27430, .T. ) ;
#21045 = CARTESIAN_POINT ( 'NONE',  ( 4.956445790443988031, 0.000000000000000000, 0.000000000000000000 ) ) ;
#21046 = EDGE_CURVE ( 'NONE', #49073, #19517, #35907, .T. ) ;
#21047 = CARTESIAN_POINT ( 'NONE',  ( 0.5809828226811617480, -41.20389530892290253, -24.41822904836968178 ) ) ;
#21048 = EDGE_LOOP ( 'NONE', ( #11116, #20598, #1549, #46569 ) ) ;
#21049 = CONICAL_SURFACE ( 'NONE', #49931, 43.08621763946400307, 1.568696531533066763 ) ;
#21050 = CARTESIAN_POINT ( 'NONE',  ( -6.015611763856276717, 14.94556629257441038, -11.47596948473795919 ) ) ;
#21051 = VERTEX_POINT ( 'NONE', #8693 ) ;
#21052 = ORIENTED_EDGE ( 'NONE', *, *, #6981, .T. ) ;
#21053 = CARTESIAN_POINT ( 'NONE',  ( 0.9758171775293916772, -5.594812732687391765, 42.54217005300509413 ) ) ;
#21054 = ORIENTED_EDGE ( 'NONE', *, *, #37491, .F. ) ;
#21055 = CARTESIAN_POINT ( 'NONE',  ( 3.270143674763207553, -7.080034332678346587, 11.71453292426876835 ) ) ;
#21056 = CARTESIAN_POINT ( 'NONE',  ( 0.9772918015221170318, -18.01631053304243935, -37.83846469569905935 ) ) ;
#21057 = ORIENTED_EDGE ( 'NONE', *, *, #13368, .T. ) ;
#21058 = CARTESIAN_POINT ( 'NONE',  ( 1.092182651088187573, -21.89098211822472351, 35.74277670161973219 ) ) ;
#21059 = CONICAL_SURFACE ( 'NONE', #32112, 42.92674063221959813, 1.485477209440487556 ) ;
#21060 = CARTESIAN_POINT ( 'NONE',  ( 4.967162193818130511, 42.16965968614205451, -8.839793687084773310 ) ) ;
#21061 = ORIENTED_EDGE ( 'NONE', *, *, #15989, .T. ) ;
#21062 = CARTESIAN_POINT ( 'NONE',  ( 4.553261556744873317, 31.39705178283683296, -30.72075365562339755 ) ) ;
#21063 = CARTESIAN_POINT ( 'NONE',  ( 5.895881250540457863, -7.232970327321949000, -18.76730726162869445 ) ) ;
#21064 = CARTESIAN_POINT ( 'NONE',  ( 0.1073791018717483448, -30.14884492832410601, 30.83464511437086841 ) ) ;
#21065 = CARTESIAN_POINT ( 'NONE',  ( 3.407937589446178528, -7.243367523630944049, -11.62731850632891550 ) ) ;
#21066 = ORIENTED_EDGE ( 'NONE', *, *, #44418, .T. ) ;
#21067 = EDGE_LOOP ( 'NONE', ( #58864, #20434, #51341, #42937 ) ) ;
#21068 = CARTESIAN_POINT ( 'NONE',  ( 4.956653778116996811, 40.28700667097716348, -26.26162724282331951 ) ) ;
#21069 = ADVANCED_FACE ( 'NONE', ( #522 ), #27813, .T. ) ;
#21070 = CARTESIAN_POINT ( 'NONE',  ( 0.6000166863083106206, 16.46965316277509217, -46.26633772416342083 ) ) ;
#21071 = CARTESIAN_POINT ( 'NONE',  ( 3.660176727303348532, -16.63097650367944880, -45.06760739764693824 ) ) ;
#21072 = ORIENTED_EDGE ( 'NONE', *, *, #40830, .T. ) ;
#21073 = CARTESIAN_POINT ( 'NONE',  ( 3.559346040607745287, -43.00729280057031190, -9.154400445031974698 ) ) ;
#21074 = CARTESIAN_POINT ( 'NONE',  ( 0.7948884756798507700, 48.02008973275257375, 10.23570352533436889 ) ) ;
#21075 = EDGE_CURVE ( 'NONE', #40574, #789, #25444, .T. ) ;
#21076 = CARTESIAN_POINT ( 'NONE',  ( 5.896782393890504181, 20.06749419425504399, -1.349727247095607430 ) ) ;
#21077 = EDGE_CURVE ( 'NONE', #13041, #14464, #18493, .T. ) ;
#21078 = ORIENTED_EDGE ( 'NONE', *, *, #1107, .T. ) ;
#21079 = VERTEX_POINT ( 'NONE', #13731 ) ;
#21080 = CARTESIAN_POINT ( 'NONE',  ( 5.895596859100789899, 0.6756533542676474990, -20.10153416427100836 ) ) ;
#21081 = EDGE_CURVE ( 'NONE', #9944, #17505, #7456, .T. ) ;
#21082 = CARTESIAN_POINT ( 'NONE',  ( 0.1087620492084205859, 33.99140154262268965, 26.53886348603014511 ) ) ;
#21083 = DIRECTION ( 'NONE',  ( -1.000000000000000000, -0.000000000000000000, -0.000000000000000000 ) ) ;
#21084 = CARTESIAN_POINT ( 'NONE',  ( 4.960386119450151732, 41.17653976845452490, 14.79625078758883205 ) ) ;
#21085 = B_SPLINE_CURVE_WITH_KNOTS ( 'NONE', 3,
 ( #30111, #54205, #53903, #1587, #6274, #25410, #58920, #11325, #16648, #6580, #25727, #44865, #21033, #53292, #49844, #10404 ),
 .UNSPECIFIED., .F., .F.,
 ( 4, 3, 3, 3, 3, 4 ),
 ( 2.194378057379452319E-17, 0.0002612764279487760359, 0.0003919131003184782693, 0.0005225497727000641716, 0.0007837925190632482816, 0.001045051706266712614 ),
 .UNSPECIFIED. ) ;
#21086 = CARTESIAN_POINT ( 'NONE',  ( -99.49999999999975842, -9.057560704502469641E-15, 1.500000000000000888 ) ) ;
#21087 = B_SPLINE_CURVE_WITH_KNOTS ( 'NONE', 3,
 ( #29767, #48879, #1554, #20381, #49186, #10368 ),
 .UNSPECIFIED., .F., .F.,
 ( 4, 2, 4 ),
 ( 1.823721537572523311E-17, 0.0002293755540694312101, 0.0004587511081388441513 ),
 .UNSPECIFIED. ) ;
#21088 = CARTESIAN_POINT ( 'NONE',  ( 0.7413678028165007206, -41.21466309768522507, -15.67921036004513091 ) ) ;
#21089 = CARTESIAN_POINT ( 'NONE',  ( 4.967162193818130511, 2.375726030842579828, 43.02067033766019932 ) ) ;
#21090 = CARTESIAN_POINT ( 'NONE',  ( 0.5806925824938502512, -2.112975627976310111, -46.84824112321764744 ) ) ;
#21091 = CARTESIAN_POINT ( 'NONE',  ( -4.915099999999998914, 0.000000000000000000, 0.000000000000000000 ) ) ;
#21092 = EDGE_CURVE ( 'NONE', #7236, #40034, #28738, .T. ) ;
#21093 = CARTESIAN_POINT ( 'NONE',  ( -6.078457390727109555, 19.09737280526033487, 2.466751502363165649 ) ) ;
#21094 = CARTESIAN_POINT ( 'NONE',  ( 0.6029442701453591180, 41.20385451604330029, 26.71680366696238096 ) ) ;
#21095 = EDGE_CURVE ( 'NONE', #30298, #3027, #27515, .T. ) ;
#21096 = CARTESIAN_POINT ( 'NONE',  ( 0.7762783648524370639, 29.86325223097011161, 37.45705264446588956 ) ) ;
#21097 = CARTESIAN_POINT ( 'NONE',  ( 1.088908134280558659, 29.78762923590010914, -30.89124834763357796 ) ) ;
#21098 = DIRECTION ( 'NONE',  ( 0.000000000000000000, 0.000000000000000000, 1.000000000000000000 ) ) ;
#21099 = CARTESIAN_POINT ( 'NONE',  ( 2.624215991343608501, -47.76052319582219496, 4.864192649745223918 ) ) ;
#21100 = CARTESIAN_POINT ( 'NONE',  ( 5.959547316686252039, -2.675599016784684814, 20.35048796920732173 ) ) ;
#21101 = VECTOR ( 'NONE', #4154, 1000.000000000000114 ) ;
#21102 = CARTESIAN_POINT ( 'NONE',  ( -6.078457390727109555, -4.280596808181184265, 18.77421108870614930 ) ) ;
#21103 = FACE_OUTER_BOUND ( 'NONE', #36859, .T. ) ;
#21105 = EDGE_LOOP ( 'NONE', ( #22671, #53600, #24315, #52394 ) ) ;
#21104 = CARTESIAN_POINT ( 'NONE',  ( -6.010958268070873523, -18.68413620842265743, 2.445171577615698144 ) ) ;
#21106 = ORIENTED_EDGE ( 'NONE', *, *, #21884, .T. ) ;
#21107 = B_SPLINE_CURVE_WITH_KNOTS ( 'NONE', 3,
 ( #12949, #32048, #26400, #27640 ),
 .UNSPECIFIED., .F., .F.,
 ( 4, 4 ),
 ( 0.000000000000000000, 0.005014147105413699519 ),
 .UNSPECIFIED. ) ;
#21108 = FACE_OUTER_BOUND ( 'NONE', #4024, .T. ) ;
#21109 = DIRECTION ( 'NONE',  ( 0.000000000000000000, 0.000000000000000000, 1.000000000000000000 ) ) ;
#21110 = CARTESIAN_POINT ( 'NONE',  ( -6.016489644550736315, 18.68257207665196162, 2.455165042129801023 ) ) ;
#21111 = ORIENTED_EDGE ( 'NONE', *, *, #5545, .F. ) ;
#21112 = ORIENTED_EDGE ( 'NONE', *, *, #15022, .F. ) ;
#21113 = CARTESIAN_POINT ( 'NONE',  ( 0.8744876279028306332, 36.80052600666260787, -32.49725120702428427 ) ) ;
#21114 = CARTESIAN_POINT ( 'NONE',  ( 4.956445790443987143, 47.01859095792193699, -2.605792484304513934 ) ) ;
#21115 = CARTESIAN_POINT ( 'NONE',  ( 0.1102847568649952675, -37.30068345220706760, 21.64199720113177605 ) ) ;
#21116 = B_SPLINE_CURVE_WITH_KNOTS ( 'NONE', 3,
 ( #39240, #14496, #11028, #10717 ),
 .UNSPECIFIED., .F., .F.,
 ( 4, 4 ),
 ( 0.000000000000000000, 0.004444103432399268763 ),
 .UNSPECIFIED. ) ;
#21117 = ORIENTED_EDGE ( 'NONE', *, *, #19180, .T. ) ;
#21118 = ORIENTED_EDGE ( 'NONE', *, *, #24541, .F. ) ;
#21119 = ADVANCED_FACE ( 'NONE', ( #5823 ), #26817, .F. ) ;
#21120 = CARTESIAN_POINT ( 'NONE',  ( 5.896782393890504181, 18.99788783847860074, -6.603510017755636063 ) ) ;
#21121 = CARTESIAN_POINT ( 'NONE',  ( 0.9754292589017257153, 36.35155297207946745, 20.85406587247130261 ) ) ;
#21122 = CYLINDRICAL_SURFACE ( 'NONE', #47972, 10.00000000000000000 ) ;
#21123 = ORIENTED_EDGE ( 'NONE', *, *, #21633, .T. ) ;
#21124 = CARTESIAN_POINT ( 'NONE',  ( 0.5804410086790514622, 5.237717535875093589, 46.60564522533491782 ) ) ;
#21125 = B_SPLINE_CURVE_WITH_KNOTS ( 'NONE', 3,
 ( #32721, #22079, #60266, #36500 ),
 .UNSPECIFIED., .F., .F.,
 ( 4, 4 ),
 ( 0.000000000000000000, 0.004447772540403792906 ),
 .UNSPECIFIED. ) ;
#21126 = CARTESIAN_POINT ( 'NONE',  ( 4.291220156522059348, -45.16379180774727331, 13.40227245104937204 ) ) ;
#21127 =( BOUNDED_SURFACE ( )  B_SPLINE_SURFACE ( 3, 1, ( 
 ( #52952, #61719 ),
 ( #47054, #14458 ),
 ( #37657, #57630 ),
 ( #23845, #14766 ) ),
 .UNSPECIFIED., .F., .F., .F. ) 
 B_SPLINE_SURFACE_WITH_KNOTS ( ( 4, 4 ),
 ( 2, 2 ),
 ( 0.000000000000000000, 1.000000000000000000 ),
 ( 0.000000000000000000, 1.000000000000000000 ),
 .UNSPECIFIED. ) 
 GEOMETRIC_REPRESENTATION_ITEM ( )  RATIONAL_B_SPLINE_SURFACE ( (
 ( 1.000000000000000000, 1.000000000000000000),
 ( 0.9751682680413298332, 0.9999560080971552356),
 ( 0.9751682680413298332, 0.9999560080971552356),
 ( 1.000000000000000000, 1.000000000000000000) ) ) 
 REPRESENTATION_ITEM ( '' )  SURFACE ( )  );
#21128 = B_SPLINE_CURVE_WITH_KNOTS ( 'NONE', 3,
 ( #4725, #33287, #52055, #32982 ),
 .UNSPECIFIED., .F., .F.,
 ( 4, 4 ),
 ( 0.000000000000000000, 0.005014147105413701254 ),
 .UNSPECIFIED. ) ;
#21129 = CARTESIAN_POINT ( 'NONE',  ( -2.569797478183790229, -5.182550149005207274, -13.68441171582014348 ) ) ;
#21130 = ORIENTED_EDGE ( 'NONE', *, *, #12857, .T. ) ;
#21131 = ORIENTED_EDGE ( 'NONE', *, *, #17896, .T. ) ;
#21132 = CARTESIAN_POINT ( 'NONE',  ( 0.7954196712028477334, 44.76287685048084342, -17.60078400783977415 ) ) ;
#21133 = CARTESIAN_POINT ( 'NONE',  ( 0.6252788684277204023, -19.24757281514202489, 45.17715431387276226 ) ) ;
#21134 = EDGE_LOOP ( 'NONE', ( #5295, #30983, #360, #14678 ) ) ;
#21135 = FACE_OUTER_BOUND ( 'NONE', #26443, .T. ) ;
#21136 = CARTESIAN_POINT ( 'NONE',  ( 0.6021448801613057400, -8.095331285689143286, 48.43559383348046055 ) ) ;
#21137 = CARTESIAN_POINT ( 'NONE',  ( 0.6028618097248863439, 46.51318640245697367, 12.28244208173076757 ) ) ;
#21138 = CARTESIAN_POINT ( 'NONE',  ( 0.5838002273316434954, 12.52789267095249492, -46.22850660674009049 ) ) ;
#21139 = EDGE_LOOP ( 'NONE', ( #28490, #50414, #6791, #8920 ) ) ;
#21140 = CARTESIAN_POINT ( 'NONE',  ( 0.5806925824938502512, -13.37132486740698134, 44.94919391528425479 ) ) ;
#21141 = CARTESIAN_POINT ( 'NONE',  ( 2.881901169982995725, 1.330622528702777754E-16, 49.00591519830862808 ) ) ;
#21142 =( BOUNDED_SURFACE ( )  B_SPLINE_SURFACE ( 3, 1, ( 
 ( #25956, #50071 ),
 ( #7128, #26255 ),
 ( #45394, #35999 ),
 ( #55060, #31272 ) ),
 .UNSPECIFIED., .F., .F., .F. ) 
 B_SPLINE_SURFACE_WITH_KNOTS ( ( 4, 4 ),
 ( 2, 2 ),
 ( 0.000000000000000000, 1.000000000000000000 ),
 ( 0.000000000000000000, 1.000000000000000000 ),
 .UNSPECIFIED. ) 
 GEOMETRIC_REPRESENTATION_ITEM ( )  RATIONAL_B_SPLINE_SURFACE ( (
 ( 1.000000000000000000, 1.000000000000000000),
 ( 0.9732289882329797637, 0.9999525324661233672),
 ( 0.9732289882329797637, 0.9999525324661233672),
 ( 1.000000000000000000, 1.000000000000000000) ) ) 
 REPRESENTATION_ITEM ( '' )  SURFACE ( )  );
#21143 = VECTOR ( 'NONE', #9391, 1000.000000000000000 ) ;
#21144 = VECTOR ( 'NONE', #53058, 1000.000000000000000 ) ;
#21145 = CARTESIAN_POINT ( 'NONE',  ( 5.895881250540457863, 17.94906520685997364, 9.075171613153653283 ) ) ;
#21146 = VERTEX_POINT ( 'NONE', #10879 ) ;
#21147 = CARTESIAN_POINT ( 'NONE',  ( 5.958863334805807099, 20.52565293643016275, -0.001220270595957195347 ) ) ;
#21148 = EDGE_CURVE ( 'NONE', #31436, #6995, #53449, .T. ) ;
#21149 = CARTESIAN_POINT ( 'NONE',  ( -6.077587904424778920, 18.62786028128793347, 4.878405757493543327 ) ) ;
#21150 = ORIENTED_EDGE ( 'NONE', *, *, #23771, .F. ) ;
#21151 = CARTESIAN_POINT ( 'NONE',  ( 1.827326673878745256, 25.21837361081542639, 34.89023127623428877 ) ) ;
#21152 = CARTESIAN_POINT ( 'NONE',  ( 1.227938101723748288, 36.73927144310511750, 22.18841447410732215 ) ) ;
#21153 = ORIENTED_EDGE ( 'NONE', *, *, #28437, .F. ) ;
#21154 = DIRECTION ( 'NONE',  ( 3.273063162220399693E-16, -1.000000000000000000, -5.236901059552639509E-15 ) ) ;
#21155 = EDGE_CURVE ( 'NONE', #40746, #60883, #15712, .T. ) ;
#21156 = CARTESIAN_POINT ( 'NONE',  ( 0.1084644655670283647, -42.70194587816332898, 6.022910953206383589 ) ) ;
#21157 = CARTESIAN_POINT ( 'NONE',  ( 5.965394784446458765, -20.34787558161488974, 2.693446924985283264 ) ) ;
#21158 = CARTESIAN_POINT ( 'NONE',  ( 0.8744876279028306332, -14.81965677137948489, -46.80521149998148900 ) ) ;
#21159 = CARTESIAN_POINT ( 'NONE',  ( 0.5549461598389366923, 21.17425125324409407, 38.68938845899861434 ) ) ;
#21160 = CARTESIAN_POINT ( 'NONE',  ( 5.896782393890504181, -7.234636363571574691, 18.76662259344765715 ) ) ;
#21161 = CARTESIAN_POINT ( 'NONE',  ( 4.962356264823608143, 0.000000000000000000, 0.000000000000000000 ) ) ;
#21162 = CARTESIAN_POINT ( 'NONE',  ( 0.1092565886968783900, -41.73439049602443873, -10.86136484717955142 ) ) ;
#21163 = CARTESIAN_POINT ( 'NONE',  ( 4.335381028904216727, 48.70445384730881244, -5.256712194871631105 ) ) ;
#21164 = CARTESIAN_POINT ( 'NONE',  ( 0.5836750258453372586, 37.88760409476694235, 29.30109045202400608 ) ) ;
#21165 = CARTESIAN_POINT ( 'NONE',  ( 0.9790320750461902755, 14.98204902227782931, 39.13917908740874907 ) ) ;
#21167 = VERTEX_POINT ( 'NONE', #49078 ) ;
#21166 = ADVANCED_FACE ( 'NONE', ( #39395 ), #49686, .F. ) ;
#21168 = CARTESIAN_POINT ( 'NONE',  ( 5.860006189529234355, 36.25227510158507727, -31.81514841426720608 ) ) ;
#21169 = CARTESIAN_POINT ( 'NONE',  ( 4.958415959904820092, -31.21198115812912022, -33.00024524162255091 ) ) ;
#21171 = EDGE_CURVE ( 'NONE', #21806, #24433, #34375, .T. ) ;
#21170 = DIRECTION ( 'NONE',  ( -1.000000000000000000, -0.000000000000000000, -0.000000000000000000 ) ) ;
#21172 = DIRECTION ( 'NONE',  ( -1.000000000000000000, -0.000000000000000000, -0.000000000000000000 ) ) ;
#21173 = CARTESIAN_POINT ( 'NONE',  ( 0.6000166863083106206, -47.36892948402866210, -12.96179004788979228 ) ) ;
#21175 = B_SPLINE_CURVE_WITH_KNOTS ( 'NONE', 3,
 ( #183, #57496, #33745, #52826, #29027, #12100, #25860, #15550, #1724, #39373, #16466, #39682, #6109, #10856, #58428, #15862 ),
 .UNSPECIFIED., .F., .F.,
 ( 4, 3, 3, 3, 3, 4 ),
 ( 1.551621725782133898E-17, 0.0002732102107931849038, 0.0004098135523333775766, 0.0005464168938825013106, 0.0008195847345945452868, 0.001092771384553108951 ),
 .UNSPECIFIED. ) ;
#21174 = CARTESIAN_POINT ( 'NONE',  ( 5.960721111146673579, 20.34914600876575363, -2.685391721745826299 ) ) ;
#21176 = DIRECTION ( 'NONE',  ( -1.000000000000000000, -4.991502096677035820E-15, -5.067589380725379776E-15 ) ) ;
#21177 = CARTESIAN_POINT ( 'NONE',  ( 0.6023142530420679819, -44.34465601638714105, 18.65157113320472604 ) ) ;
#21178 = CARTESIAN_POINT ( 'NONE',  ( 0.6031357023905875581, 41.68407605450313014, -24.01594909943223044 ) ) ;
#21179 = B_SPLINE_CURVE_WITH_KNOTS ( 'NONE', 3,
 ( #9815, #35730, #11928, #51025, #12229, #36648, #26301, #59494, #20991, #50115 ),
 .UNSPECIFIED., .F., .F.,
 ( 4, 3, 3, 4 ),
 ( 4.878909776184769953E-18, 0.0002724573126191764060, 0.0004086839781548492903, 0.0005054209210070093961 ),
 .UNSPECIFIED. ) ;
#21180 = CARTESIAN_POINT ( 'NONE',  ( 4.956653778116991482, 20.77844580450620526, -43.37017594958032873 ) ) ;
#21182 = ORIENTED_EDGE ( 'NONE', *, *, #36378, .T. ) ;
#21181 = CARTESIAN_POINT ( 'NONE',  ( 2.528190830796658517, 41.96176392093605756, 1.210167259777327198 ) ) ;
#21183 = ORIENTED_EDGE ( 'NONE', *, *, #363, .F. ) ;
#21184 = CARTESIAN_POINT ( 'NONE',  ( 0.9972139404380327976, 42.45145681504345703, -6.252633471302944557 ) ) ;
#21185 = DIRECTION ( 'NONE',  ( 0.000000000000000000, 0.000000000000000000, 1.000000000000000000 ) ) ;
#21186 = DIRECTION ( 'NONE',  ( 0.000000000000000000, 0.000000000000000000, 1.000000000000000000 ) ) ;
#21187 = EDGE_LOOP ( 'NONE', ( #32588, #16208, #61855, #27975 ) ) ;
#21188 = CARTESIAN_POINT ( 'NONE',  ( 0.5807400328401574052, -11.87003418057210880, -46.40483864045157958 ) ) ;
#21189 = CARTESIAN_POINT ( 'NONE',  ( 0.7245667037590765025, 0.8205429720397920956, 48.09508190954921503 ) ) ;
#21190 = CARTESIAN_POINT ( 'NONE',  ( 0.1092355843206037486, 41.73183925352180523, -10.87081649985046283 ) ) ;
#21191 = VECTOR ( 'NONE', #45357, 999.9999999999997726 ) ;
#21192 = EDGE_LOOP ( 'NONE', ( #60858, #12082, #40825, #36472 ) ) ;
#21193 = ORIENTED_EDGE ( 'NONE', *, *, #45871, .F. ) ;
#21194 = EDGE_CURVE ( 'NONE', #60883, #49846, #38781, .T. ) ;
#21195 = CARTESIAN_POINT ( 'NONE',  ( 2.301529144917015213, -47.43735140118869253, 7.543875168382339957 ) ) ;
#21196 = DIRECTION ( 'NONE',  ( -1.000000000000000000, -0.000000000000000000, -0.000000000000000000 ) ) ;
#21197 = CARTESIAN_POINT ( 'NONE',  ( 0.5997462898726536595, 40.86908001809322855, 27.22627276398666041 ) ) ;
#21198 = VERTEX_POINT ( 'NONE', #6131 ) ;
#21199 = B_SPLINE_CURVE_WITH_KNOTS ( 'NONE', 3,
 ( #58543, #33856, #34775, #53839, #48544, #10971 ),
 .UNSPECIFIED., .F., .F.,
 ( 4, 2, 4 ),
 ( 6.805474077711127748E-18, 0.0002291472222819933421, 0.0004582944445639799079 ),
 .UNSPECIFIED. ) ;
#21200 = ORIENTED_EDGE ( 'NONE', *, *, #31635, .F. ) ;
#21201 = CARTESIAN_POINT ( 'NONE',  ( 0.1102144999581333162, -0.1260305566215071948, 43.12427761225339395 ) ) ;
#21202 = CARTESIAN_POINT ( 'NONE',  ( 0.5804410086790514622, -24.77328595090391872, 39.82215658462187946 ) ) ;
#21203 = ORIENTED_EDGE ( 'NONE', *, *, #32130, .T. ) ;
#21204 = CARTESIAN_POINT ( 'NONE',  ( 0.6039202388192953519, -14.13938383033847224, -47.02809306943408529 ) ) ;
#21205 = DIRECTION ( 'NONE',  ( -1.000000000000000000, -1.836909530733573776E-16, 1.925929944387235579E-32 ) ) ;
#21206 = VERTEX_POINT ( 'NONE', #49379 ) ;
#21207 = CARTESIAN_POINT ( 'NONE',  ( 1.157644175074337811, 5.016389116425647998, -41.61535913231781336 ) ) ;
#21208 = CARTESIAN_POINT ( 'NONE',  ( 4.975801465491695552, 0.000000000000000000, 0.000000000000000000 ) ) ;
#21209 = EDGE_LOOP ( 'NONE', ( #61258, #35094 ) ) ;
#21210 = CARTESIAN_POINT ( 'NONE',  ( 0.5806925824938502512, -44.47729014209954101, -14.86583411581937320 ) ) ;
#21211 = CARTESIAN_POINT ( 'NONE',  ( 0.6064782688330870863, 46.89167618744689037, 0.7107395798700630873 ) ) ;
#21212 = DIRECTION ( 'NONE',  ( -1.685288351013738149E-16, 1.000000000000000000, 0.000000000000000000 ) ) ;
#21213 = CARTESIAN_POINT ( 'NONE',  ( 0.8753041380234471980, -42.34096624980154644, -24.86726573039640087 ) ) ;
#21214 = ORIENTED_EDGE ( 'NONE', *, *, #2332, .F. ) ;
#21215 = CARTESIAN_POINT ( 'NONE',  ( 4.956445790444002242, -32.34643101787113295, 34.22347806032784234 ) ) ;
#21216 = CARTESIAN_POINT ( 'NONE',  ( 0.6029303876144825880, 44.49541906039127781, -18.28892193312817227 ) ) ;
#21217 = ORIENTED_EDGE ( 'NONE', *, *, #13655, .F. ) ;
#21218 = CARTESIAN_POINT ( 'NONE',  ( 50.00005079999999680, 9.539392014169456147, -3.000000000000000000 ) ) ;
#21219 = ORIENTED_EDGE ( 'NONE', *, *, #44239, .F. ) ;
#21220 = CARTESIAN_POINT ( 'NONE',  ( 5.959547316686252039, -5.308980600728594013, 19.82715097195153220 ) ) ;
#21221 = EDGE_CURVE ( 'NONE', #43044, #23359, #39531, .T. ) ;
#21222 = ORIENTED_EDGE ( 'NONE', *, *, #50625, .T. ) ;
#21223 = CARTESIAN_POINT ( 'NONE',  ( 0.8557997880470606944, 19.17299735372068525, -43.90420959842161608 ) ) ;
#21224 = CARTESIAN_POINT ( 'NONE',  ( 0.9783242366443536397, 24.64300816128945115, 33.89773796242378978 ) ) ;
#21225 =( BOUNDED_SURFACE ( )  B_SPLINE_SURFACE ( 3, 1, ( 
 ( #1928, #45201 ),
 ( #54536, #60479 ),
 ( #50782, #11663 ),
 ( #50478, #12600 ) ),
 .UNSPECIFIED., .F., .F., .F. ) 
 B_SPLINE_SURFACE_WITH_KNOTS ( ( 4, 4 ),
 ( 2, 2 ),
 ( 0.000000000000000000, 1.000000000000000000 ),
 ( 0.000000000000000000, 1.000000000000000000 ),
 .UNSPECIFIED. ) 
 GEOMETRIC_REPRESENTATION_ITEM ( )  RATIONAL_B_SPLINE_SURFACE ( (
 ( 1.000000000000000000, 1.000000000000000000),
 ( 0.9953390228620291325, 0.8624445117761032620),
 ( 0.9953390228620291325, 0.8624445117761032620),
 ( 1.000000000000000000, 1.000000000000000000) ) ) 
 REPRESENTATION_ITEM ( '' )  SURFACE ( )  );
#21226 = B_SPLINE_CURVE_WITH_KNOTS ( 'NONE', 3,
 ( #24372, #57545, #19077, #5240, #57863, #14992, #24066, #53174, #20002, #39114, #24997, #29371, #34707, #44135, #24681, #43192, #53768, #1163, #10902 ),
 .UNSPECIFIED., .F., .F.,
 ( 4, 3, 3, 3, 3, 3, 4 ),
 ( 6.939740885162003740E-18, 0.0002732106629380627572, 0.0004098138914053780341, 0.0005464171197651489665, 0.0006830203481512585849, 0.0008196235766963636329, 0.001011968216111138992 ),
 .UNSPECIFIED. ) ;
#21227 = CARTESIAN_POINT ( 'NONE',  ( 0.1102847568649952675, -26.17930421801176877, 34.26895182984652877 ) ) ;
#21228 = ORIENTED_EDGE ( 'NONE', *, *, #53938, .T. ) ;
#21229 = CARTESIAN_POINT ( 'NONE',  ( -6.017396004339687465, 7.212050743684414122, -17.40836349643160119 ) ) ;
#21230 = EDGE_CURVE ( 'NONE', #36314, #36654, #12719, .T. ) ;
#21231 = CARTESIAN_POINT ( 'NONE',  ( 0.8551540677456739292, 47.90804413217340851, 0.9122407826477398896 ) ) ;
#21232 = FACE_OUTER_BOUND ( 'NONE', #10795, .T. ) ;
#21233 = ORIENTED_EDGE ( 'NONE', *, *, #9414, .T. ) ;
#21234 = B_SPLINE_CURVE_WITH_KNOTS ( 'NONE', 3,
 ( #39083, #44697, #16177, #30561 ),
 .UNSPECIFIED., .F., .F.,
 ( 4, 4 ),
 ( 0.000000000000000000, 0.004444878191957686922 ),
 .UNSPECIFIED. ) ;
#21235 = MECHANICAL_DESIGN_GEOMETRIC_PRESENTATION_REPRESENTATION (  '', ( #60208 ), #47226 ) ;
#21236 = EDGE_CURVE ( 'NONE', #24966, #13518, #38137, .T. ) ;
#21237 = EDGE_LOOP ( 'NONE', ( #1607, #15519, #951, #22364 ) ) ;
#21238 = CIRCLE ( 'NONE', #49218, 43.08621763946400307 ) ;
#21239 = CARTESIAN_POINT ( 'NONE',  ( 0.7954190325252765703, -37.62416463577130088, 29.96539637359152053 ) ) ;
#21240 = CARTESIAN_POINT ( 'NONE',  ( 2.706805983486680223, 30.79179577033409743, 31.44266888414198036 ) ) ;
#21241 = CARTESIAN_POINT ( 'NONE',  ( 0.6026777506516367566, 33.14375390931751042, 36.23586576081520860 ) ) ;
#21242 = CARTESIAN_POINT ( 'NONE',  ( 0.2885697896453119915, 41.84838128162059689, -10.38006191081376350 ) ) ;
#21243 = DIRECTION ( 'NONE',  ( 0.07439287786467664587, -0.6174937095821814159, 0.7830499462674445077 ) ) ;
#21244 = CARTESIAN_POINT ( 'NONE',  ( 4.975610109902397937, 47.16372689271652519, 12.96272628450595832 ) ) ;
#21245 = VERTEX_POINT ( 'NONE', #15885 ) ;
#21246 = CARTESIAN_POINT ( 'NONE',  ( 2.282816707992305627, 41.06969068285943081, 22.79862876627047186 ) ) ;
#21247 = CARTESIAN_POINT ( 'NONE',  ( 0.08486401232817714080, 0.000000000000000000, 0.000000000000000000 ) ) ;
#21248 = ORIENTED_EDGE ( 'NONE', *, *, #32835, .T. ) ;
#21249 = CARTESIAN_POINT ( 'NONE',  ( -6.016761891674564211, 11.47373234755503013, 14.94721834528419002 ) ) ;
#21251 = EDGE_CURVE ( 'NONE', #45554, #55549, #59524, .T. ) ;
#21250 = CARTESIAN_POINT ( 'NONE',  ( 0.6008123274975391004, 44.05373908824402918, 21.69844749062424683 ) ) ;
#21252 = CARTESIAN_POINT ( 'NONE',  ( 0.5837800304671214580, 45.21772934546406475, 12.43359501591787719 ) ) ;
#21253 = CARTESIAN_POINT ( 'NONE',  ( -48.95476116535499500, 0.000000000000000000, 0.000000000000000000 ) ) ;
#21254 = CARTESIAN_POINT ( 'NONE',  ( 0.8751705887134553219, -47.55935879196475469, 7.160166390003496417 ) ) ;
#21255 = CARTESIAN_POINT ( 'NONE',  ( 5.896278296736517710, -17.30234040492929637, -10.25455977242977568 ) ) ;
#21256 = B_SPLINE_CURVE_WITH_KNOTS ( 'NONE', 3,
 ( #57185, #56587, #13704, #32812, #51890, #8984, #28094, #24943, #53118, #6102, #34647, #53715, #811, #58118, #34969, #19949, #24630, #43769, #15853 ),
 .UNSPECIFIED., .F., .F.,
 ( 4, 3, 3, 3, 3, 3, 4 ),
 ( 3.469685171791681197E-18, 0.0002612768053151711127, 0.0003919133833142872392, 0.0005225499612322589103, 0.0006531865391693350911, 0.0008112755173415149785, 0.0009693688056799732236 ),
 .UNSPECIFIED. ) ;
#21257 =( BOUNDED_SURFACE ( )  B_SPLINE_SURFACE ( 3, 1, ( 
 ( #19774, #49491 ),
 ( #38894, #16295 ),
 ( #6545, #35418 ),
 ( #1869, #25379 ) ),
 .UNSPECIFIED., .F., .F., .F. ) 
 B_SPLINE_SURFACE_WITH_KNOTS ( ( 4, 4 ),
 ( 2, 2 ),
 ( 0.000000000000000000, 1.000000000000000000 ),
 ( 0.000000000000000000, 1.000000000000000000 ),
 .UNSPECIFIED. ) 
 GEOMETRIC_REPRESENTATION_ITEM ( )  RATIONAL_B_SPLINE_SURFACE ( (
 ( 1.000000000000000000, 1.000000000000000000),
 ( 0.9953390228620291325, 0.8624445117761032620),
 ( 0.9953390228620291325, 0.8624445117761032620),
 ( 1.000000000000000000, 1.000000000000000000) ) ) 
 REPRESENTATION_ITEM ( '' )  SURFACE ( )  );
#21258 = LINE ( 'NONE', #60366, #38720 ) ;
#21259 = CARTESIAN_POINT ( 'NONE',  ( 0.5809828226811556418, -5.711058609465654357, 47.55412398569204413 ) ) ;
#21260 = CARTESIAN_POINT ( 'NONE',  ( 0.5850706913938533704, -18.49682194437995975, 44.18063951072215190 ) ) ;
#21261 = LINE ( 'NONE', #39158, #58821 ) ;
#21262 = CARTESIAN_POINT ( 'NONE',  ( 0.8554163680231738898, -8.703479761965578376, 46.10265624825618858 ) ) ;
#21263 = CARTESIAN_POINT ( 'NONE',  ( 0.9790320750461911636, 9.631629496021094639, 40.78687099782926140 ) ) ;
#21264 = DIRECTION ( 'NONE',  ( 0.07836865515943411409, 0.2503967164834395298, 0.9649662368512245125 ) ) ;
#21265 = CARTESIAN_POINT ( 'NONE',  ( 0.5809828226811617480, -47.41188724015875522, -6.791453954330822107 ) ) ;
#21266 = ORIENTED_EDGE ( 'NONE', *, *, #40779, .F. ) ;
#21267 = CARTESIAN_POINT ( 'NONE',  ( 0.6845945791218023269, 3.832784513613418653, -46.75164471530547416 ) ) ;
#21268 = CARTESIAN_POINT ( 'NONE',  ( 0.1098349054025746507, 43.12395110775227636, 0.2133124578266234195 ) ) ;
#21269 = CARTESIAN_POINT ( 'NONE',  ( 0.1156495703730067853, -38.51293032282120521, -21.53362837936490237 ) ) ;
#21270 = CARTESIAN_POINT ( 'NONE',  ( 0.6008123274975391004, -45.35345026050291750, -18.83133294874649977 ) ) ;
#21271 = B_SPLINE_CURVE_WITH_KNOTS ( 'NONE', 3,
 ( #11197, #2071, #1768, #40042, #49395, #54693, #25589, #6448, #20897, #16203, #35944, #54382, #11828, #59401, #7078, #26203, #45344, #37482, #23063 ),
 .UNSPECIFIED., .F., .F.,
 ( 4, 3, 3, 3, 3, 3, 4 ),
 ( 5.204170427930421283E-18, 0.0002724573126191728281, 0.0004086839781548437609, 0.0005449106435901761736, 0.0006811373090491400738, 0.0008459866663933635197, 0.001010840725717212065 ),
 .UNSPECIFIED. ) ;
#21272 = CARTESIAN_POINT ( 'NONE',  ( 2.281448460670572942, 17.13756432392898077, -44.80776276180753825 ) ) ;
#21273 = ORIENTED_EDGE ( 'NONE', *, *, #28979, .T. ) ;
#21274 = ADVANCED_FACE ( 'NONE', ( #51220, #26188 ), #22421, .F. ) ;
#21275 = CARTESIAN_POINT ( 'NONE',  ( 4.975610109902397937, -16.35148546628888866, -46.09857188876371481 ) ) ;
#21276 = CARTESIAN_POINT ( 'NONE',  ( 0.9736507210033050752, 16.83559693395318391, -39.46762617149617824 ) ) ;
#21277 = VECTOR ( 'NONE', #22271, 1000.000000000000000 ) ;
#21278 = ADVANCED_BREP_SHAPE_REPRESENTATION ( '', ( #31244, #14677 ), #21841 ) ;
#21279 = EDGE_CURVE ( 'NONE', #15433, #23834, #16523, .T. ) ;
#21280 = CARTESIAN_POINT ( 'NONE',  ( 0.6026777506516367566, -13.80536265409133101, 47.12704481108740850 ) ) ;
#21281 = CIRCLE ( 'NONE', #56275, 2.700000000000000622 ) ;
#21282 = ORIENTED_EDGE ( 'NONE', *, *, #537, .T. ) ;
#21283 = B_SPLINE_CURVE_WITH_KNOTS ( 'NONE', 3,
 ( #26581, #59465, #59789, #7451, #30980, #60092 ),
 .UNSPECIFIED., .F., .F.,
 ( 4, 2, 4 ),
 ( 7.757919228897728493E-18, 0.0002291978881530210932, 0.0004583957763060344344 ),
 .UNSPECIFIED. ) ;
#21284 = EDGE_CURVE ( 'NONE', #60643, #55418, #56067, .T. ) ;
#21285 = CARTESIAN_POINT ( 'NONE',  ( 0.3622758884714730732, 6.444611261694017657, 42.62881903538212924 ) ) ;
#21286 = ORIENTED_EDGE ( 'NONE', *, *, #31052, .F. ) ;
#21287 = CARTESIAN_POINT ( 'NONE',  ( 0.8551540677456834771, -0.9122407826472416215, -47.90804413217341562 ) ) ;
#21288 = CARTESIAN_POINT ( 'NONE',  ( 0.8557997880470599172, 7.156447707086380561, -47.37054680076698077 ) ) ;
#21289 = VERTEX_POINT ( 'NONE', #60612 ) ;
#21290 = CARTESIAN_POINT ( 'NONE',  ( 5.965394784446458765, -12.50653125158996204, -16.27505370423077125 ) ) ;
#21291 = ORIENTED_EDGE ( 'NONE', *, *, #56859, .F. ) ;
#21292 = CARTESIAN_POINT ( 'NONE',  ( 4.549368137175248350, 28.46244473166628097, 32.13400537129935230 ) ) ;
#21293 = CARTESIAN_POINT ( 'NONE',  ( 0.1145239942831223490, 20.11902381989014899, 39.27047696730160453 ) ) ;
#21294 = ORIENTED_EDGE ( 'NONE', *, *, #1194, .T. ) ;
#21295 = ORIENTED_EDGE ( 'NONE', *, *, #38727, .F. ) ;
#21296 = CARTESIAN_POINT ( 'NONE',  ( 0.9789889208857698311, 20.05614176017457240, -36.79790857831663686 ) ) ;
#21297 = CARTESIAN_POINT ( 'NONE',  ( 1.157644175074340254, 28.54093988368000367, 30.69881147594066917 ) ) ;
#21298 = ORIENTED_EDGE ( 'NONE', *, *, #43175, .F. ) ;
#21299 = EDGE_CURVE ( 'NONE', #1908, #44492, #36856, .T. ) ;
#21300 = ORIENTED_EDGE ( 'NONE', *, *, #43591, .F. ) ;
#21301 = CARTESIAN_POINT ( 'NONE',  ( 0.7245667037590793891, 34.58857005974907395, 33.42814706018032922 ) ) ;
#21302 = CARTESIAN_POINT ( 'NONE',  ( 4.549368137175248350, -13.99871866169335810, -40.58005590356685843 ) ) ;
#21303 = CARTESIAN_POINT ( 'NONE',  ( 0.6064782688330876415, -44.53025739761609714, 14.71022170196044954 ) ) ;
#21304 = B_SPLINE_CURVE_WITH_KNOTS ( 'NONE', 3,
 ( #35565, #24924, #1385, #20524 ),
 .UNSPECIFIED., .F., .F.,
 ( 4, 4 ),
 ( 0.000000000000000000, 0.005004741218457415403 ),
 .UNSPECIFIED. ) ;
#21305 = CARTESIAN_POINT ( 'NONE',  ( 0.5806925824938499181, 32.99217760300705748, -33.32774488853398509 ) ) ;
#21306 = CARTESIAN_POINT ( 'NONE',  ( 2.500000000000000000, 2.357898499370431722, -2.818925648462311528E-15 ) ) ;
#21307 = ORIENTED_EDGE ( 'NONE', *, *, #41468, .T. ) ;
#21308 = CARTESIAN_POINT ( 'NONE',  ( 0.9780303403264780648, -17.34655100543410811, 38.15018717661756398 ) ) ;
#21309 = CARTESIAN_POINT ( 'NONE',  ( 4.549368137175248350, -3.018832571116875751, 42.82045902618767030 ) ) ;
#21310 = VERTEX_POINT ( 'NONE', #40326 ) ;
#21311 = ADVANCED_FACE ( 'NONE', ( #30887 ), #10528, .F. ) ;
#21312 = ORIENTED_EDGE ( 'NONE', *, *, #3597, .T. ) ;
#21313 = CARTESIAN_POINT ( 'NONE',  ( -2.708315649062910779, -12.54007339125010034, -7.544341609839931628 ) ) ;
#21314 = CARTESIAN_POINT ( 'NONE',  ( -6.077587904424778920, 13.82827771187084664, -13.40055061993000685 ) ) ;
#21315 = CARTESIAN_POINT ( 'NONE',  ( 4.833616638992208614, -2.572717262758311918, 46.17873762321148945 ) ) ;
#21316 = EDGE_LOOP ( 'NONE', ( #12967, #19168, #34837, #11363 ) ) ;
#21317 = CARTESIAN_POINT ( 'NONE',  ( -6.077587904424778920, -16.14165210942803341, -10.49967087922893150 ) ) ;
#21318 = DIRECTION ( 'NONE',  ( 1.000000000000000000, 0.000000000000000000, 0.000000000000000000 ) ) ;
#21319 = CARTESIAN_POINT ( 'NONE',  ( 0.5988103564986355654, -0.6065102550370011780, -48.10388392110853317 ) ) ;
#21320 = CARTESIAN_POINT ( 'NONE',  ( 4.975610109902397937, 45.55079628452109830, 17.82061629079735354 ) ) ;
#21321 = ORIENTED_EDGE ( 'NONE', *, *, #34521, .F. ) ;
#21322 = CARTESIAN_POINT ( 'NONE',  ( 1.830465331921976802, 26.20437692621130665, -35.40772070873008914 ) ) ;
#21323 = ORIENTED_EDGE ( 'NONE', *, *, #13855, .T. ) ;
#21324 = DIRECTION ( 'NONE',  ( 0.000000000000000000, 0.000000000000000000, 1.000000000000000000 ) ) ;
#21326 = EDGE_CURVE ( 'NONE', #32638, #759, #36690, .T. ) ;
#21325 = FACE_OUTER_BOUND ( 'NONE', #28611, .T. ) ;
#21327 = CIRCLE ( 'NONE', #22309, 2.649999999999985700 ) ;
#21328 =( NAMED_UNIT ( * ) SI_UNIT ( $, .STERADIAN. ) SOLID_ANGLE_UNIT ( ) );
#21329 = CARTESIAN_POINT ( 'NONE',  ( 4.549368137175248350, 28.46244473166673927, -32.13400537129894730 ) ) ;
#21330 =( BOUNDED_SURFACE ( )  B_SPLINE_SURFACE ( 3, 1, ( 
 ( #21160, #45598 ),
 ( #16163, #54034 ),
 ( #44385, #54649 ),
 ( #6715, #39676 ) ),
 .UNSPECIFIED., .F., .F., .F. ) 
 B_SPLINE_SURFACE_WITH_KNOTS ( ( 4, 4 ),
 ( 2, 2 ),
 ( 0.000000000000000000, 1.000000000000000000 ),
 ( 0.000000000000000000, 1.000000000000000000 ),
 .UNSPECIFIED. ) 
 GEOMETRIC_REPRESENTATION_ITEM ( )  RATIONAL_B_SPLINE_SURFACE ( (
 ( 1.000000000000000000, 1.000000000000000000),
 ( 0.9952954269826590483, 0.8620686068821307169),
 ( 0.9952954269826590483, 0.8620686068821307169),
 ( 1.000000000000000000, 1.000000000000000000) ) ) 
 REPRESENTATION_ITEM ( '' )  SURFACE ( )  );
#21331 = ORIENTED_EDGE ( 'NONE', *, *, #23142, .T. ) ;
#21332 = DIRECTION ( 'NONE',  ( 0.000000000000000000, 0.000000000000000000, 1.000000000000000000 ) ) ;
#21333 = CARTESIAN_POINT ( 'NONE',  ( 5.960721111146673579, -16.28787783074235662, 12.49016043756443750 ) ) ;
#21334 = CARTESIAN_POINT ( 'NONE',  ( 0.1152339509894530906, -35.22763790827196573, 26.56983661709124434 ) ) ;
#21335 = CARTESIAN_POINT ( 'NONE',  ( 0.5786265663353153954, -47.39171391660397603, 6.967625775955545109 ) ) ;
#21336 = CARTESIAN_POINT ( 'NONE',  ( 0.5832655196449132440, 32.43772929586945253, 33.86781512145746120 ) ) ;
#21337 = CARTESIAN_POINT ( 'NONE',  ( 1.154321713695926732, -37.57248787340954266, 20.73950268329812374 ) ) ;
#21338 = AXIS2_PLACEMENT_3D ( 'NONE', #27964, #42093, #8853 ) ;
#21339 = CARTESIAN_POINT ( 'NONE',  ( 0.5263152470540364281, 0.000000000000000000, 0.000000000000000000 ) ) ;
#21340 = CARTESIAN_POINT ( 'NONE',  ( -90.00000000000000000, 8.239576745513314221E-16, 6.728125000000023448 ) ) ;
#21341 = CARTESIAN_POINT ( 'NONE',  ( 4.958415959904820092, -45.41969080731321640, 0.5056093261665406402 ) ) ;
#21342 = ORIENTED_EDGE ( 'NONE', *, *, #30352, .F. ) ;
#21343 = CARTESIAN_POINT ( 'NONE',  ( 0.8744876279028263033, -31.30103973185235233, 37.82320666052117275 ) ) ;
#21344 = B_SPLINE_CURVE_WITH_KNOTS ( 'NONE', 3,
 ( #26709, #19764, #39501, #38887 ),
 .UNSPECIFIED., .F., .F.,
 ( 4, 4 ),
 ( 0.000000000000000000, 0.005013413432710155451 ),
 .UNSPECIFIED. ) ;
#21345 = CARTESIAN_POINT ( 'NONE',  ( 4.956445790444003130, -40.78973928653796577, 23.53157918788916803 ) ) ;
#21346 = CARTESIAN_POINT ( 'NONE',  ( 4.060580049360325461, -41.86530176281380733, 13.37027309622913407 ) ) ;
#21347 = ORIENTED_EDGE ( 'NONE', *, *, #44287, .F. ) ;
#21348 = EDGE_CURVE ( 'NONE', #50534, #27996, #7060, .T. ) ;
#21349 = CARTESIAN_POINT ( 'NONE',  ( 0.6254087463353926735, 47.77987801197954809, 5.596276562478490924 ) ) ;
#21350 = LINE ( 'NONE', #25734, #52959 ) ;
#21351 = EDGE_CURVE ( 'NONE', #32860, #59637, #21684, .T. ) ;
#21352 = CARTESIAN_POINT ( 'NONE',  ( 4.553261556744875094, 0.000000000000000000, 0.000000000000000000 ) ) ;
#21353 = ORIENTED_EDGE ( 'NONE', *, *, #37191, .T. ) ;
#21354 = CARTESIAN_POINT ( 'NONE',  ( 0.1119899015040011631, 3.677941833846906317, 43.97083183269729290 ) ) ;
#21355 = CARTESIAN_POINT ( 'NONE',  ( 0.7048096507298635682, 34.61049487267014513, 33.41730025321766107 ) ) ;
#21356 = EDGE_CURVE ( 'NONE', #53671, #44040, #27680, .T. ) ;
#21357 = ORIENTED_EDGE ( 'NONE', *, *, #7100, .F. ) ;
#21358 = EDGE_CURVE ( 'NONE', #58092, #19302, #41243, .T. ) ;
#21359 = CARTESIAN_POINT ( 'NONE',  ( 0.6021448801613057400, 10.67258200247132294, 47.93367430134552620 ) ) ;
#21360 = EDGE_CURVE ( 'NONE', #39423, #32449, #16812, .T. ) ;
#21361 = ORIENTED_EDGE ( 'NONE', *, *, #47299, .T. ) ;
#21362 = ORIENTED_EDGE ( 'NONE', *, *, #10090, .T. ) ;
#21363 = CARTESIAN_POINT ( 'NONE',  ( 0.8744876279028263033, -39.87136468799916145, 28.64654129726773846 ) ) ;
#21364 = ORIENTED_EDGE ( 'NONE', *, *, #17206, .T. ) ;
#21365 = CARTESIAN_POINT ( 'NONE',  ( 0.8751705887134423323, 42.09020928323375443, -23.27176129838382224 ) ) ;
#21366 = VECTOR ( 'NONE', #36368, 1000.000000000000114 ) ;
#21367 = EDGE_LOOP ( 'NONE', ( #58459, #20705, #18123, #28768 ) ) ;
#21368 = CARTESIAN_POINT ( 'NONE',  ( 4.956445790443991584, 35.28522167764473494, 31.18479086508529363 ) ) ;
#21369 = EDGE_CURVE ( 'NONE', #36409, #30700, #14523, .T. ) ;
#21370 = DIRECTION ( 'NONE',  ( 0.000000000000000000, 0.000000000000000000, -1.000000000000000000 ) ) ;
#21371 = EDGE_CURVE ( 'NONE', #47629, #10066, #2057, .T. ) ;
#21372 = ORIENTED_EDGE ( 'NONE', *, *, #2000, .F. ) ;
#21373 = CARTESIAN_POINT ( 'NONE',  ( 0.6025881611877910160, -18.61132239451814741, 44.36157157392723605 ) ) ;
#21374 = CARTESIAN_POINT ( 'NONE',  ( 48.39231140143691334, 12.39600195714815456, -1.615626833367223236 ) ) ;
#21375 = LINE ( 'NONE', #54237, #44288 ) ;
#21376 = CARTESIAN_POINT ( 'NONE',  ( 0.9788927965476041937, 36.13029534060832049, 21.23530953935432919 ) ) ;
#21377 = ORIENTED_EDGE ( 'NONE', *, *, #37467, .F. ) ;
#21378 = CIRCLE ( 'NONE', #39422, 48.35291015139245019 ) ;
#21379 = ORIENTED_EDGE ( 'NONE', *, *, #61021, .F. ) ;
#21380 = CARTESIAN_POINT ( 'NONE',  ( 0.1103744047535531458, 41.64495780681022552, 11.19884698423381231 ) ) ;
#21381 = CARTESIAN_POINT ( 'NONE',  ( 0.6039202388192953519, 16.79650288729678920, -46.14586875990116965 ) ) ;
#21382 = CARTESIAN_POINT ( 'NONE',  ( 4.694002226626921015, 6.935496447963269695, 45.05755941533480069 ) ) ;
#21383 = VERTEX_POINT ( 'NONE', #2682 ) ;
#21384 = CARTESIAN_POINT ( 'NONE',  ( 0.5839880159502349732, -46.25220722086336167, -12.44022138820733936 ) ) ;
#21385 = FACE_OUTER_BOUND ( 'NONE', #54089, .T. ) ;
#21386 = CARTESIAN_POINT ( 'NONE',  ( 0.6845945791218023269, 46.90049452736490565, -0.8661026512829932411 ) ) ;
#21387 = CARTESIAN_POINT ( 'NONE',  ( 0.5809828226811626362, 29.58751527316234231, -37.66417181417519799 ) ) ;
#21388 = VERTEX_POINT ( 'NONE', #60008 ) ;
#21389 = ORIENTED_EDGE ( 'NONE', *, *, #31698, .F. ) ;
#21390 = CARTESIAN_POINT ( 'NONE',  ( 4.963659409799330291, 24.46566636552876517, -37.47512675766667911 ) ) ;
#21391 = CARTESIAN_POINT ( 'NONE',  ( 0.5549461598389366923, 42.12604207101915677, 13.06193993622417970 ) ) ;
#21392 = CARTESIAN_POINT ( 'NONE',  ( 4.956653778116987041, -47.27023054223747067, -8.845409907521421644 ) ) ;
#21394 = EDGE_CURVE ( 'NONE', #3337, #46926, #57486, .T. ) ;
#21393 = CARTESIAN_POINT ( 'NONE',  ( 0.7242003506640004584, -49.09522258624797075, 0.8190197389533786509 ) ) ;
#21395 = EDGE_CURVE ( 'NONE', #35697, #61479, #22517, .T. ) ;
#21396 = CARTESIAN_POINT ( 'NONE',  ( 1.479689385636123067, -13.65972076154995207, -41.89267088625614122 ) ) ;
#21397 = CARTESIAN_POINT ( 'NONE',  ( 2.528100132419517365, 21.22729024012173582, 36.21679068738293950 ) ) ;
#21398 = CARTESIAN_POINT ( 'NONE',  ( 0.6027935024548037868, 12.61964268015556989, -46.42277558035030438 ) ) ;
#21399 =( BOUNDED_SURFACE ( )  B_SPLINE_SURFACE ( 3, 1, ( 
 ( #28287, #23290 ),
 ( #18594, #372 ),
 ( #42416, #28901 ),
 ( #57379, #57083 ) ),
 .UNSPECIFIED., .F., .F., .F. ) 
 B_SPLINE_SURFACE_WITH_KNOTS ( ( 4, 4 ),
 ( 2, 2 ),
 ( 0.000000000000000000, 1.000000000000000000 ),
 ( 0.000000000000000000, 1.000000000000000000 ),
 .UNSPECIFIED. ) 
 GEOMETRIC_REPRESENTATION_ITEM ( )  RATIONAL_B_SPLINE_SURFACE ( (
 ( 1.000000000000000000, 1.000000000000000000),
 ( 0.7282232189291694135, 0.9929344683865672927),
 ( 0.7282232189291694135, 0.9929344683865672927),
 ( 1.000000000000000000, 1.000000000000000000) ) ) 
 REPRESENTATION_ITEM ( '' )  SURFACE ( )  );
#21400 = CARTESIAN_POINT ( 'NONE',  ( 0.8753041380234471980, 33.66554281472474486, -35.74590263041226734 ) ) ;
#21401 = CARTESIAN_POINT ( 'NONE',  ( 0.5800708119828335008, 0.6275298934114975635, 47.89175345941821149 ) ) ;
#21402 = CARTESIAN_POINT ( 'NONE',  ( 5.896782393890504181, -17.30835043929350192, -10.24436879210333906 ) ) ;
#21403 = CARTESIAN_POINT ( 'NONE',  ( -6.001507490154110336, -14.95933060264865766, -11.45906331631447017 ) ) ;
#21404 = DIRECTION ( 'NONE',  ( 0.000000000000000000, 0.000000000000000000, -1.000000000000000000 ) ) ;
#21405 = CONICAL_SURFACE ( 'NONE', #56401, 42.92674063221959813, 1.485477209440487556 ) ;
#21406 = CARTESIAN_POINT ( 'NONE',  ( 2.299746137290198611, 44.72136981280802814, 20.10672573424628240 ) ) ;
#21407 = CARTESIAN_POINT ( 'NONE',  ( 4.303969348037246512, -47.93217632892351077, 4.133486515473138390 ) ) ;
#21408 = CARTESIAN_POINT ( 'NONE',  ( 0.9780106845699469975, -22.81401109455046949, 35.15468879442924077 ) ) ;
#21409 = CARTESIAN_POINT ( 'NONE',  ( 0.8551540677456834771, 44.61036085020950992, 17.49081417858803533 ) ) ;
#21410 = CARTESIAN_POINT ( 'NONE',  ( 3.999999999999990674, -2.309401076758548221, -5.242734410091827613 ) ) ;
#21411 = CARTESIAN_POINT ( 'NONE',  ( 1.830465331921976357, 28.68895279831538403, 33.42633756806781520 ) ) ;
#21413 = EDGE_LOOP ( 'NONE', ( #24587, #40833, #16958, #9886 ) ) ;
#21412 = LINE ( 'NONE', #12043, #61332 ) ;
#21415 = VERTEX_POINT ( 'NONE', #43095 ) ;
#21414 = B_SPLINE_CURVE_WITH_KNOTS ( 'NONE', 3,
 ( #2964, #22088, #54646, #59981, #21780, #30855 ),
 .UNSPECIFIED., .F., .F.,
 ( 4, 2, 4 ),
 ( 0.000000000000000000, 0.0002291966416970778317, 0.0004583932833941556633 ),
 .UNSPECIFIED. ) ;
#21416 = CARTESIAN_POINT ( 'NONE',  ( -6.016761891674565099, -18.20023637398595540, -4.880293656735155139 ) ) ;
#21417 = CARTESIAN_POINT ( 'NONE',  ( 3.660087539127329759, -20.10768839917373541, -43.62750476736573546 ) ) ;
#21418 = CARTESIAN_POINT ( 'NONE',  ( 4.963659409799330291, -44.68724496494572662, -2.450325214228857629 ) ) ;
#21419 = ORIENTED_EDGE ( 'NONE', *, *, #60740, .F. ) ;
#21420 = EDGE_CURVE ( 'NONE', #25523, #4961, #52503, .T. ) ;
#21421 = ORIENTED_EDGE ( 'NONE', *, *, #11279, .F. ) ;
#21422 = CARTESIAN_POINT ( 'NONE',  ( 4.060580049360325461, -29.91699279630384467, 32.19380742293636644 ) ) ;
#21423 = CARTESIAN_POINT ( 'NONE',  ( 5.959828726073459926, 5.308046411394975017, 19.82738831247215217 ) ) ;
#21424 = EDGE_CURVE ( 'NONE', #34231, #60457, #17510, .T. ) ;
#21425 = ORIENTED_EDGE ( 'NONE', *, *, #6996, .F. ) ;
#21426 = ORIENTED_EDGE ( 'NONE', *, *, #23986, .F. ) ;
#21427 = CARTESIAN_POINT ( 'NONE',  ( 0.5819845901640493535, 47.89381229371849713, 0.4540519722832492833 ) ) ;
#21428 = EDGE_CURVE ( 'NONE', #46672, #41724, #30497, .T. ) ;
#21429 = ADVANCED_FACE ( 'NONE', ( #47784 ), #40933, .F. ) ;
#21430 = CARTESIAN_POINT ( 'NONE',  ( 0.8744876279028263033, -20.68330519280349122, 44.52584571550372061 ) ) ;
#21431 = CARTESIAN_POINT ( 'NONE',  ( 0.8751705887134423323, -47.79200036674284036, 5.393078191591890835 ) ) ;
#21432 = EDGE_CURVE ( 'NONE', #54810, #49073, #55280, .T. ) ;
#21433 = EDGE_LOOP ( 'NONE', ( #55457, #50143, #11277, #23360 ) ) ;
#21434 = CARTESIAN_POINT ( 'NONE',  ( 0.1119899015040013990, -17.34614229840122590, -40.57182095440284542 ) ) ;
#21435 = B_SPLINE_CURVE_WITH_KNOTS ( 'NONE', 3,
 ( #34246, #5999, #2240, #1618, #21373, #29524, #44583, #6610, #29837, #53618, #54235, #59255, #39265, #16063, #10745, #16361 ),
 .UNSPECIFIED., .F., .F.,
 ( 4, 3, 3, 3, 3, 4 ),
 ( 1.868480190406682863E-17, 0.0002618515315864458257, 0.0003927756766342040086, 0.0005236998216950610342, 0.0007855159896329934766, 0.001047349442285930689 ),
 .UNSPECIFIED. ) ;
#21436 = CARTESIAN_POINT ( 'NONE',  ( 10.00000000000002132, -80.00000000000001421, -2.532597876869216023E-31 ) ) ;
#21437 = CARTESIAN_POINT ( 'NONE',  ( 0.5980894510889448457, 19.05812566676507203, -44.17723055703932289 ) ) ;
#21438 = ORIENTED_EDGE ( 'NONE', *, *, #120, .T. ) ;
#21439 = ORIENTED_EDGE ( 'NONE', *, *, #33831, .F. ) ;
#21440 = CARTESIAN_POINT ( 'NONE',  ( 0.5782707292762423457, -20.39674625896858728, -42.23398034468063145 ) ) ;
#21441 = CARTESIAN_POINT ( 'NONE',  ( 0.8760168074887090262, 24.81951362746020706, 41.20610493656918294 ) ) ;
#21442 = VERTEX_POINT ( 'NONE', #3599 ) ;
#21443 = CARTESIAN_POINT ( 'NONE',  ( 5.960721111146673579, 14.51823969584099672, -14.50930005615001583 ) ) ;
#21444 = CARTESIAN_POINT ( 'NONE',  ( 0.3622758884714730732, -4.808133778522197588, 42.84426538328723666 ) ) ;
#21445 = DIRECTION ( 'NONE',  ( -1.000000000000000000, -0.000000000000000000, -0.000000000000000000 ) ) ;
#21446 = CARTESIAN_POINT ( 'NONE',  ( 3.221118495291109163, -43.82609091211070051, -3.746354898452465498 ) ) ;
#21447 = ORIENTED_EDGE ( 'NONE', *, *, #21703, .T. ) ;
#21448 = CARTESIAN_POINT ( 'NONE',  ( 0.5817216825391123836, -13.45861452432960625, 44.92327511761540393 ) ) ;
#21449 = DIRECTION ( 'NONE',  ( 0.000000000000000000, -0.000000000000000000, 1.000000000000000000 ) ) ;
#21450 = CARTESIAN_POINT ( 'NONE',  ( 4.956653778116973719, 21.75875759808707244, 42.88673967249138741 ) ) ;
#21451 = CARTESIAN_POINT ( 'NONE',  ( 0.9754642270333678811, -21.30186789325730601, -37.24735125696678040 ) ) ;
#21452 = VECTOR ( 'NONE', #51027, 1000.000000000000000 ) ;
#21453 = VERTEX_POINT ( 'NONE', #56232 ) ;
#21454 = CARTESIAN_POINT ( 'NONE',  ( 5.958863334805807099, 20.52565293643016275, 0.001220270596240801819 ) ) ;
#21455 = CARTESIAN_POINT ( 'NONE',  ( 0.8551540677456715978, -5.348818140990585057, -47.61725548905996419 ) ) ;
#21456 = CARTESIAN_POINT ( 'NONE',  ( 4.956445790443988031, 46.94638516972315756, 3.684422564749393558 ) ) ;
#21457 = DIRECTION ( 'NONE',  ( 0.000000000000000000, 0.000000000000000000, -1.000000000000000000 ) ) ;
#21458 = ORIENTED_EDGE ( 'NONE', *, *, #51925, .T. ) ;
#21459 = DIRECTION ( 'NONE',  ( 0.09835009131224549395, 0.3736726418952318052, -0.9223318362920749358 ) ) ;
#21460 = CARTESIAN_POINT ( 'NONE',  ( 10.00000000000000533, 1.836909530733574959E-15, -1.925929944387237167E-31 ) ) ;
#21461 = CARTESIAN_POINT ( 'NONE',  ( 0.2885700199627506679, -22.25146206940439697, -36.93108631019287458 ) ) ;
#21462 = VECTOR ( 'NONE', #55894, 999.9999999999997726 ) ;
#21463 = CARTESIAN_POINT ( 'NONE',  ( 0.8560838555295158248, 33.26091945577399400, -33.07694168205770069 ) ) ;
#21464 = CARTESIAN_POINT ( 'NONE',  ( 0.5835871038041865466, -46.80019526881169867, 2.996026652517322475 ) ) ;
#21465 = CARTESIAN_POINT ( 'NONE',  ( 5.880360259849752858, -47.04104239318760250, -9.405269135695077054 ) ) ;
#21466 = EDGE_CURVE ( 'NONE', #51708, #4904, #6669, .T. ) ;
#21467 = CARTESIAN_POINT ( 'NONE',  ( 0.9756008150404607004, -5.741579752919358626, -42.52260101821270410 ) ) ;
#21468 = CARTESIAN_POINT ( 'NONE',  ( 5.959547316686252039, -5.315863417546194292, -19.82530672674360517 ) ) ;
#21469 = FACE_OUTER_BOUND ( 'NONE', #25266, .T. ) ;
#21470 = CARTESIAN_POINT ( 'NONE',  ( 0.6029442701453592290, 41.10881650023822687, -26.86280758051954365 ) ) ;
#21471 = FACE_OUTER_BOUND ( 'NONE', #28535, .T. ) ;
#21472 = VERTEX_POINT ( 'NONE', #56845 ) ;
#21473 = CARTESIAN_POINT ( 'NONE',  ( -6.063463321072278589, 15.42324870294163830, 11.53012800998666698 ) ) ;
#21474 = CARTESIAN_POINT ( 'NONE',  ( 1.091591847532195070, -34.99102718170865245, 23.07351312056237447 ) ) ;
#21475 = DIRECTION ( 'NONE',  ( 0.000000000000000000, 0.000000000000000000, 1.000000000000000000 ) ) ;
#21476 = CARTESIAN_POINT ( 'NONE',  ( 2.618530812446111078, 29.00550538245418153, -36.99199165639262077 ) ) ;
#21477 = CARTESIAN_POINT ( 'NONE',  ( 0.8751705887134553219, 17.57879340691544101, -44.76769609654218129 ) ) ;
#21478 = APPLICATION_PROTOCOL_DEFINITION ( 'draft international standard', 'automotive_design', 1998, #60057 ) ;
#21479 = CARTESIAN_POINT ( 'NONE',  ( 3.678748215320120085, 24.27640525275985794, 42.53550237511316112 ) ) ;
#21480 = CIRCLE ( 'NONE', #15503, 15.43999999999999240 ) ;
#21481 = CARTESIAN_POINT ( 'NONE',  ( 3.894904216938897878, 35.57819931341702357, -25.81309873089577067 ) ) ;
#21482 = CARTESIAN_POINT ( 'NONE',  ( 0.5848930533535030563, -19.90539571549654241, -42.46231627922634289 ) ) ;
#21484 = ORIENTED_EDGE ( 'NONE', *, *, #19184, .F. ) ;
#21483 = CARTESIAN_POINT ( 'NONE',  ( 5.974727161628367256, -5.327229920347289926, -19.82156119440443476 ) ) ;
#21485 = ORIENTED_EDGE ( 'NONE', *, *, #677, .F. ) ;
#21486 = CARTESIAN_POINT ( 'NONE',  ( 1.231276596079887264, -27.70544295162332560, -31.45926257674220494 ) ) ;
#21487 = LINE ( 'NONE', #55293, #17490 ) ;
#21488 = DIRECTION ( 'NONE',  ( 1.000000000000000000, 1.836909530733573776E-16, -1.925929944387235853E-32 ) ) ;
#21489 = VERTEX_POINT ( 'NONE', #13977 ) ;
#21490 = CARTESIAN_POINT ( 'NONE',  ( 0.8560838555295158248, 42.82099363437792050, 19.15033519931955297 ) ) ;
#21491 = CARTESIAN_POINT ( 'NONE',  ( 0.5807400328401637335, 44.45848844984443815, 17.82553128098424366 ) ) ;
#21492 = DIRECTION ( 'NONE',  ( -1.000000000000000000, -0.000000000000000000, -0.000000000000000000 ) ) ;
#21493 = EDGE_CURVE ( 'NONE', #55243, #28634, #23659, .T. ) ;
#21494 =( BOUNDED_SURFACE ( )  B_SPLINE_SURFACE ( 3, 1, ( 
 ( #58406, #29922 ),
 ( #49032, #48117 ),
 ( #23995, #24301 ),
 ( #53700, #29609 ) ),
 .UNSPECIFIED., .F., .F., .F. ) 
 B_SPLINE_SURFACE_WITH_KNOTS ( ( 4, 4 ),
 ( 2, 2 ),
 ( 0.000000000000000000, 1.000000000000000000 ),
 ( 0.000000000000000000, 1.000000000000000000 ),
 .UNSPECIFIED. ) 
 GEOMETRIC_REPRESENTATION_ITEM ( )  RATIONAL_B_SPLINE_SURFACE ( (
 ( 1.000000000000000000, 1.000000000000000000),
 ( 0.9732289882329797637, 0.9999525324661233672),
 ( 0.9732289882329797637, 0.9999525324661233672),
 ( 1.000000000000000000, 1.000000000000000000) ) ) 
 REPRESENTATION_ITEM ( '' )  SURFACE ( )  );
#21495 = EDGE_LOOP ( 'NONE', ( #15429, #46374, #13438, #52011 ) ) ;
#21496 = EDGE_LOOP ( 'NONE', ( #13538, #7809, #36225, #51593 ) ) ;
#21497 = AXIS2_PLACEMENT_3D ( 'NONE', #60348, #36581, #55040 ) ;
#21498 = ADVANCED_FACE ( 'NONE', ( #10801 ), #6463, .F. ) ;
#21499 = CARTESIAN_POINT ( 'NONE',  ( 0.5809828226811553087, -44.03860873105708151, 18.83114015454682999 ) ) ;
#21501 = DIRECTION ( 'NONE',  ( 0.07836865515943411409, 0.9968932487286222832, 0.007886984708667934760 ) ) ;
#21500 = AXIS2_PLACEMENT_3D ( 'NONE', #9313, #519, #14655 ) ;
#21502 = CARTESIAN_POINT ( 'NONE',  ( 4.956445790444004018, -43.14021684453488348, -18.88014143872194950 ) ) ;
#21503 = ORIENTED_EDGE ( 'NONE', *, *, #16476, .F. ) ;
#21504 = ADVANCED_FACE ( 'NONE', ( #19587 ), #8497, .T. ) ;
#21505 = VECTOR ( 'NONE', #12453, 1000.000000000000000 ) ;
#21506 = ORIENTED_EDGE ( 'NONE', *, *, #35007, .F. ) ;
#21507 = CARTESIAN_POINT ( 'NONE',  ( 0.5980271706414711508, -26.05568637495964524, 41.63112357805641039 ) ) ;
#21508 = CARTESIAN_POINT ( 'NONE',  ( 2.526464513654345545, -33.34586834545791589, 27.11556434133536087 ) ) ;
#21509 = ORIENTED_EDGE ( 'NONE', *, *, #3288, .T. ) ;
#21510 =( BOUNDED_SURFACE ( )  B_SPLINE_SURFACE ( 3, 1, ( 
 ( #58636, #6010 ),
 ( #11683, #53626 ),
 ( #6943, #49256 ),
 ( #58960, #44592 ) ),
 .UNSPECIFIED., .F., .F., .F. ) 
 B_SPLINE_SURFACE_WITH_KNOTS ( ( 4, 4 ),
 ( 2, 2 ),
 ( 0.000000000000000000, 1.000000000000000000 ),
 ( 0.000000000000000000, 1.000000000000000000 ),
 .UNSPECIFIED. ) 
 GEOMETRIC_REPRESENTATION_ITEM ( )  RATIONAL_B_SPLINE_SURFACE ( (
 ( 1.000000000000000000, 1.000000000000000000),
 ( 0.7223157951917476005, 0.9931996967497186413),
 ( 0.7223157951917476005, 0.9931996967497186413),
 ( 1.000000000000000000, 1.000000000000000000) ) ) 
 REPRESENTATION_ITEM ( '' )  SURFACE ( )  );
#21511 = CARTESIAN_POINT ( 'NONE',  ( 0.5980271706414734822, 28.66946741852817837, 39.87619441194977554 ) ) ;
#21512 = CYLINDRICAL_SURFACE ( 'NONE', #39014, 13.50000000000000178 ) ;
#21513 = VERTEX_POINT ( 'NONE', #49301 ) ;
#21514 = FACE_OUTER_BOUND ( 'NONE', #58566, .T. ) ;
#21515 = EDGE_CURVE ( 'NONE', #39657, #8473, #46541, .T. ) ;
#21516 = CARTESIAN_POINT ( 'NONE',  ( -2.708315649062910779, 0.2635547933243524432, -14.63219292706382646 ) ) ;
#21517 = ORIENTED_EDGE ( 'NONE', *, *, #46850, .T. ) ;
#21518 = DIRECTION ( 'NONE',  ( -1.000000000000000000, -5.380183451256491399E-17, -1.298891185607892835E-16 ) ) ;
#21519 = CARTESIAN_POINT ( 'NONE',  ( 0.5987334363312691865, 11.51672169166321424, -47.73811923346844566 ) ) ;
#21520 = CARTESIAN_POINT ( 'NONE',  ( 4.962356264823602814, 6.570263404307167932, -41.57002810511882274 ) ) ;
#21521 = FACE_OUTER_BOUND ( 'NONE', #11813, .T. ) ;
#21522 = EDGE_CURVE ( 'NONE', #18062, #46608, #6005, .T. ) ;
#21523 = EDGE_LOOP ( 'NONE', ( #14517, #33977 ) ) ;
#21524 = CARTESIAN_POINT ( 'NONE',  ( 5.895881250540457863, -15.78739120953184916, 12.46137875218859747 ) ) ;
#21525 = CARTESIAN_POINT ( 'NONE',  ( 0.6028618097248863439, 44.37846879336933625, -18.57111736963403459 ) ) ;
#21526 = ORIENTED_EDGE ( 'NONE', *, *, #39856, .F. ) ;
#21527 = CARTESIAN_POINT ( 'NONE',  ( 0.6845945791218023269, 17.66463248440708256, 43.45534811625348226 ) ) ;
#21528 = ORIENTED_EDGE ( 'NONE', *, *, #15293, .F. ) ;
#21529 = CARTESIAN_POINT ( 'NONE',  ( 0.9783242366443551941, 3.928031727822913322, 41.72415435873735134 ) ) ;
#21530 = ORIENTED_EDGE ( 'NONE', *, *, #55068, .T. ) ;
#21531 = CARTESIAN_POINT ( 'NONE',  ( 0.9722240750034564227, 26.58024222649045498, 33.68410530487882681 ) ) ;
#21532 = CARTESIAN_POINT ( 'NONE',  ( 0.6001305935487315502, -17.92615948558569272, 44.64600790884025372 ) ) ;
#21533 = B_SPLINE_CURVE_WITH_KNOTS ( 'NONE', 3,
 ( #27775, #3632, #37196, #14622 ),
 .UNSPECIFIED., .F., .F.,
 ( 4, 4 ),
 ( 0.000000000000000000, 0.004444103432399267029 ),
 .UNSPECIFIED. ) ;
#21534 = CARTESIAN_POINT ( 'NONE',  ( 0.1145239942831223490, -43.80251030910497434, 5.318418122470812470 ) ) ;
#21535 = ORIENTED_EDGE ( 'NONE', *, *, #35754, .T. ) ;
#21536 = CARTESIAN_POINT ( 'NONE',  ( 0.1157506346131639274, -27.58342920138327869, -34.43973131856737524 ) ) ;
#21537 = CARTESIAN_POINT ( 'NONE',  ( 3.407937589446174087, 12.82481284928210563, -4.815089211104917943 ) ) ;
#21538 = DIRECTION ( 'NONE',  ( 0.000000000000000000, -1.000000000000000000, 0.000000000000000000 ) ) ;
#21540 = ORIENTED_EDGE ( 'NONE', *, *, #14513, .T. ) ;
#21539 = B_SPLINE_CURVE_WITH_KNOTS ( 'NONE', 3,
 ( #48000, #5048, #31045, #50157 ),
 .UNSPECIFIED., .F., .F.,
 ( 4, 4 ),
 ( 0.000000000000000000, 0.005013413432710146778 ),
 .UNSPECIFIED. ) ;
#21541 = B_SPLINE_CURVE_WITH_KNOTS ( 'NONE', 3,
 ( #23964, #61232, #18353, #43091, #60929, #56228, #5742, #29885, #5136, #1665, #48998, #20494, #58368, #48687, #58676, #25488, #28968, #24890, #15494 ),
 .UNSPECIFIED., .F., .F.,
 ( 4, 3, 3, 3, 3, 3, 4 ),
 ( 1.157434093048479169E-16, 0.0002618519381806257000, 0.0003927759815485974931, 0.0005237000248299428879, 0.0006546240681324978251, 0.0007855481115631320586, 0.0009699050456655107250 ),
 .UNSPECIFIED. ) ;
#21542 = VERTEX_POINT ( 'NONE', #54288 ) ;
#21543 = CARTESIAN_POINT ( 'NONE',  ( 3.660176727303402711, 16.63097650367969749, 45.06760739764692403 ) ) ;
#21544 = CARTESIAN_POINT ( 'NONE',  ( 5.959828726073459926, 19.82504517499712904, -5.316791119500882346 ) ) ;
#21545 = CARTESIAN_POINT ( 'NONE',  ( 4.975610109902397937, -37.61482235126130291, -31.26618855282533360 ) ) ;
#21546 = CARTESIAN_POINT ( 'NONE',  ( 3.376099380956838925, 0.01224625995945537518, -13.40552996569640065 ) ) ;
#21547 = EDGE_CURVE ( 'NONE', #19392, #56342, #28445, .T. ) ;
#21548 = CARTESIAN_POINT ( 'NONE',  ( -0.3263565795980851170, 4.430380094434251959, -0.2484800633750073040 ) ) ;
#21550 = CONICAL_SURFACE ( 'NONE', #56545, 44.12552607296456131, 0.04450589592585061510 ) ;
#21549 = CARTESIAN_POINT ( 'NONE',  ( -2.601141883200662974, 14.01836437022357451, -5.126488842573914795 ) ) ;
#21551 = EDGE_LOOP ( 'NONE', ( #52408, #6884, #53166, #48417 ) ) ;
#21552 = CARTESIAN_POINT ( 'NONE',  ( 0.6067375320500746350, -23.33187539052098813, -41.82999795871630511 ) ) ;
#21553 = FACE_OUTER_BOUND ( 'NONE', #34958, .T. ) ;
#21554 = EDGE_LOOP ( 'NONE', ( #44587, #58128, #1798, #17895 ) ) ;
#21555 = VECTOR ( 'NONE', #11646, 1000.000000000000114 ) ;
#21556 = CARTESIAN_POINT ( 'NONE',  ( 5.960721111146673579, -7.848955554238637333, 18.96557324978273940 ) ) ;
#21557 = EDGE_CURVE ( 'NONE', #60852, #40143, #49003, .T. ) ;
#21558 = CARTESIAN_POINT ( 'NONE',  ( 0.5980894510889448457, -28.72954109785577259, -38.59343625445439585 ) ) ;
#21559 = CARTESIAN_POINT ( 'NONE',  ( 0.6026112563231247332, 44.16843500053740712, 21.46369829520319783 ) ) ;
#21560 = AXIS2_PLACEMENT_3D ( 'NONE', #11380, #58653, #54569 ) ;
#21561 = CARTESIAN_POINT ( 'NONE',  ( 3.240649175237396040, -10.75352374005706402, -42.65708199783103538 ) ) ;
#21562 = CARTESIAN_POINT ( 'NONE',  ( 0.6039202388192953519, -47.45712035475610691, 12.62479467093167074 ) ) ;
#21563 = DIRECTION ( 'NONE',  ( -1.000000000000000000, -0.000000000000000000, -0.000000000000000000 ) ) ;
#21564 = CARTESIAN_POINT ( 'NONE',  ( 0.1154773475650540393, -12.72687235669186911, -42.24890945412192877 ) ) ;
#21565 = B_SPLINE_CURVE_WITH_KNOTS ( 'NONE', 3,
 ( #46399, #55764, #14122, #28492, #37016, #12891, #51371, #47620, #27581, #4356, #42324, #56382, #13815, #37623, #18498, #56076, #23194, #61080, #37307 ),
 .UNSPECIFIED., .F., .F.,
 ( 4, 3, 3, 3, 3, 3, 4 ),
 ( 9.813676791237319219E-18, 0.0002732106629380594504, 0.0004098138914053772210, 0.0005464171197651531949, 0.0006830203481512640059, 0.0008196235766963692708, 0.001011968216111140944 ),
 .UNSPECIFIED. ) ;
#21566 = CARTESIAN_POINT ( 'NONE',  ( 0.5807400328401574052, -33.48217046439087596, -34.25275203086270182 ) ) ;
#21567 = CARTESIAN_POINT ( 'NONE',  ( 0.1119899015040010798, 30.07795574961987484, -32.28432880077288303 ) ) ;
#21568 = CARTESIAN_POINT ( 'NONE',  ( 0.3622758884714730732, -43.10531414739105571, 0.8252992914326598983 ) ) ;
#21569 = CARTESIAN_POINT ( 'NONE',  ( 4.967162193818131399, -35.57684288741960899, -24.30453456948146851 ) ) ;
#21570 = DIRECTION ( 'NONE',  ( 0.000000000000000000, 0.000000000000000000, 1.000000000000000000 ) ) ;
#21571 = CARTESIAN_POINT ( 'NONE',  ( 2.533389852662419894, 16.67687449783081277, 40.73490381377152403 ) ) ;
#21572 = B_SPLINE_CURVE_WITH_KNOTS ( 'NONE', 3,
 ( #11033, #57674, #33920, #29194 ),
 .UNSPECIFIED., .F., .F.,
 ( 4, 4 ),
 ( 2.173710443588397387E-17, 0.004559932413162187670 ),
 .UNSPECIFIED. ) ;
#21573 = CARTESIAN_POINT ( 'NONE',  ( 0.5997462898726536595, 40.86908001809322855, 27.22627276398666041 ) ) ;
#21574 = CARTESIAN_POINT ( 'NONE',  ( 0.9754292589017186099, 38.80678075739997723, 15.82280740394609708 ) ) ;
#21575 = VERTEX_POINT ( 'NONE', #43407 ) ;
#21576 = EDGE_CURVE ( 'NONE', #22212, #54494, #50858, .T. ) ;
#21577 = CARTESIAN_POINT ( 'NONE',  ( 0.9730545539215883499, 37.40983423658472873, 21.01499094264562473 ) ) ;
#21578 = CARTESIAN_POINT ( 'NONE',  ( 0.5824936645240097466, -19.40917689265153001, -42.69100644620676377 ) ) ;
#21579 = B_SPLINE_CURVE_WITH_KNOTS ( 'NONE', 3,
 ( #5880, #25027, #38840, #57895 ),
 .UNSPECIFIED., .F., .F.,
 ( 4, 4 ),
 ( 0.002042055671079073039, 0.004446298630425058081 ),
 .UNSPECIFIED. ) ;
#21580 = CARTESIAN_POINT ( 'NONE',  ( 0.9754642270333698795, -25.98138239028835628, -34.14824330022355525 ) ) ;
#21581 = CARTESIAN_POINT ( 'NONE',  ( 0.7762783648524387292, 28.45155609988383461, -38.54028518467388409 ) ) ;
#21582 = CARTESIAN_POINT ( 'NONE',  ( 5.895881250540457863, -19.93280900245014564, -2.685294561150279868 ) ) ;
#21583 = ORIENTED_EDGE ( 'NONE', *, *, #35059, .T. ) ;
#21584 = EDGE_CURVE ( 'NONE', #12427, #35241, #33695, .T. ) ;
#21585 = CARTESIAN_POINT ( 'NONE',  ( 1.231276596079887264, -39.31472542100218703, 14.54747868495677743 ) ) ;
#21586 = DIRECTION ( 'NONE',  ( -1.000000000000000000, -5.380183451256491399E-17, -1.298891185607892835E-16 ) ) ;
#21587 = CARTESIAN_POINT ( 'NONE',  ( 0.6027444965799114707, -14.09757999337120005, 47.04037366154675226 ) ) ;
#21588 = ORIENTED_EDGE ( 'NONE', *, *, #37118, .F. ) ;
#21589 = CARTESIAN_POINT ( 'NONE',  ( -6.063463321072276813, -16.14731216720862506, -10.49212858547712557 ) ) ;
#21590 = EDGE_LOOP ( 'NONE', ( #49294, #7934, #19924, #16151 ) ) ;
#21591 = CARTESIAN_POINT ( 'NONE',  ( -2.708315649062910779, 12.80362818457445151, -7.087851317223837100 ) ) ;
#21592 = CARTESIAN_POINT ( 'NONE',  ( 0.6023143664670691511, -29.49326149840261024, 38.00627775314912071 ) ) ;
#21593 = CIRCLE ( 'NONE', #41602, 43.92652462719577500 ) ;
#21594 = VERTEX_POINT ( 'NONE', #443 ) ;
#21595 = CARTESIAN_POINT ( 'NONE',  ( 2.648799415243708655, -26.59464913125692220, -41.19759824158361283 ) ) ;
#21596 = VERTEX_POINT ( 'NONE', #57762 ) ;
#21597 = CARTESIAN_POINT ( 'NONE',  ( 0.8554163680231738898, 42.82911630180333162, 19.15391004255849694 ) ) ;
#21598 = CARTESIAN_POINT ( 'NONE',  ( 4.962356264823603702, -40.70360067759225586, -10.69824704058845022 ) ) ;
#21599 = EDGE_CURVE ( 'NONE', #57176, #44029, #19482, .T. ) ;
#21600 = CIRCLE ( 'NONE', #26599, 47.09074272231896430 ) ;
#21601 = VERTEX_POINT ( 'NONE', #58074 ) ;
#21602 = CARTESIAN_POINT ( 'NONE',  ( 0.3676999524040323597, 5.056646555325726489, -43.82215089355327109 ) ) ;
#21603 = ORIENTED_EDGE ( 'NONE', *, *, #25716, .F. ) ;
#21604 = CARTESIAN_POINT ( 'NONE',  ( 0.1092565886968784872, 11.46097737058305555, 41.57372480460688990 ) ) ;
#21605 = B_SPLINE_CURVE_WITH_KNOTS ( 'NONE', 3,
 ( #33992, #53065, #23118, #3360 ),
 .UNSPECIFIED., .F., .F.,
 ( 4, 4 ),
 ( 0.000000000000000000, 0.005014147105413698652 ),
 .UNSPECIFIED. ) ;
#21606 = ORIENTED_EDGE ( 'NONE', *, *, #56564, .T. ) ;
#21607 = ORIENTED_EDGE ( 'NONE', *, *, #54028, .F. ) ;
#21609 = AXIS2_PLACEMENT_3D ( 'NONE', #16317, #7514, #49517 ) ;
#21608 = LINE ( 'NONE', #12230, #49404 ) ;
#21610 = CARTESIAN_POINT ( 'NONE',  ( 0.5263152470540346517, 0.000000000000000000, 0.000000000000000000 ) ) ;
#21611 = CARTESIAN_POINT ( 'NONE',  ( 0.1100247026804066219, -16.65964013375411668, 39.77655614012826391 ) ) ;
#21612 = CARTESIAN_POINT ( 'NONE',  ( -5.283180000000052168, 0.000000000000000000, 0.000000000000000000 ) ) ;
#21613 = ORIENTED_EDGE ( 'NONE', *, *, #8804, .F. ) ;
#21614 = CARTESIAN_POINT ( 'NONE',  ( 0.9754642270333685472, 10.93570046136908402, 41.49150764699761140 ) ) ;
#21615 = CARTESIAN_POINT ( 'NONE',  ( 1.231276596079887264, 41.91134057782999633, -0.8463462572780159343 ) ) ;
#21616 = CYLINDRICAL_SURFACE ( 'NONE', #55889, 7.500000000000022204 ) ;
#21617 = VERTEX_POINT ( 'NONE', #53674 ) ;
#21618 = ORIENTED_EDGE ( 'NONE', *, *, #4533, .F. ) ;
#21619 = CARTESIAN_POINT ( 'NONE',  ( 0.9745511491811743587, 34.24777528633319434, -25.84997388131824891 ) ) ;
#21620 =( BOUNDED_SURFACE ( )  B_SPLINE_SURFACE ( 3, 1, ( 
 ( #25216, #54622 ),
 ( #35255, #15521 ),
 ( #39653, #49954 ),
 ( #30835, #59333 ) ),
 .UNSPECIFIED., .F., .F., .F. ) 
 B_SPLINE_SURFACE_WITH_KNOTS ( ( 4, 4 ),
 ( 2, 2 ),
 ( 0.000000000000000000, 1.000000000000000000 ),
 ( 0.000000000000000000, 1.000000000000000000 ),
 .UNSPECIFIED. ) 
 GEOMETRIC_REPRESENTATION_ITEM ( )  RATIONAL_B_SPLINE_SURFACE ( (
 ( 1.000000000000000000, 1.000000000000000000),
 ( 0.7269869731126817891, 0.9931720237060910339),
 ( 0.7269869731126817891, 0.9931720237060910339),
 ( 1.000000000000000000, 1.000000000000000000) ) ) 
 REPRESENTATION_ITEM ( '' )  SURFACE ( )  );
#21621 = CARTESIAN_POINT ( 'NONE',  ( 5.880360259849739535, -9.312491912828475549, 47.05949693022690639 ) ) ;
#21622 = CARTESIAN_POINT ( 'NONE',  ( 0.8560838555295223751, 28.55542365806889293, 37.21505896528891810 ) ) ;
#21623 = ORIENTED_EDGE ( 'NONE', *, *, #18249, .F. ) ;
#21624 = CARTESIAN_POINT ( 'NONE',  ( 0.5998501479064699549, -34.38546660123274989, -33.64490850298832925 ) ) ;
#21625 = CARTESIAN_POINT ( 'NONE',  ( 5.894904586330512508, -2.011994607810698721, -20.01202862679802408 ) ) ;
#21626 = CARTESIAN_POINT ( 'NONE',  ( -20.00618396018216671, -12.48880663681880954, -0.5456665274875781568 ) ) ;
#21627 = ORIENTED_EDGE ( 'NONE', *, *, #47893, .T. ) ;
#21628 = CARTESIAN_POINT ( 'NONE',  ( 4.967162193818130511, -40.93989340068619498, 13.42934394584149871 ) ) ;
#21629 = VERTEX_POINT ( 'NONE', #6057 ) ;
#21630 = CARTESIAN_POINT ( 'NONE',  ( 0.2279481005628795909, 39.41468212403272986, 19.82388256962714834 ) ) ;
#21631 = DIRECTION ( 'NONE',  ( 0.000000000000000000, 0.000000000000000000, 1.000000000000000000 ) ) ;
#21632 = CARTESIAN_POINT ( 'NONE',  ( 5.974727161628369032, -20.35137732084678319, 2.663664384318439105 ) ) ;
#21633 = EDGE_CURVE ( 'NONE', #5027, #6245, #1363, .T. ) ;
#21634 = LINE ( 'NONE', #36676, #23808 ) ;
#21635 = ORIENTED_EDGE ( 'NONE', *, *, #11230, .F. ) ;
#21636 = CARTESIAN_POINT ( 'NONE',  ( 0.9754402186311952327, 21.29160191075049369, -37.25324696807206237 ) ) ;
#21637 = CARTESIAN_POINT ( 'NONE',  ( 4.962356264823608143, -38.91448554252697534, 16.02805081171152324 ) ) ;
#21638 = EDGE_CURVE ( 'NONE', #45810, #10577, #33344, .T. ) ;
#21639 = CARTESIAN_POINT ( 'NONE',  ( 4.549368137175248350, -3.018832571116246477, -42.82045902618772004 ) ) ;
#21640 = CARTESIAN_POINT ( 'NONE',  ( 0.2940133293163010308, 9.030615628137779183, 43.18203944876707823 ) ) ;
#21641 = AXIS2_PLACEMENT_3D ( 'NONE', #51171, #31459, #32401 ) ;
#21642 = AXIS2_PLACEMENT_3D ( 'NONE', #50953, #8045, #36890 ) ;
#21643 = CARTESIAN_POINT ( 'NONE',  ( 0.9758171775293921213, 37.15687890897648771, -21.45936886481755934 ) ) ;
#21644 = CARTESIAN_POINT ( 'NONE',  ( 5.895596859100789899, -18.51552686702056150, -7.855154234585556949 ) ) ;
#21645 = CARTESIAN_POINT ( 'NONE',  ( 5.959828726073459926, 18.96145866559671589, -7.858992891709945638 ) ) ;
#21646 = CARTESIAN_POINT ( 'NONE',  ( -2.708315649062916552, 10.16016146078288607, -10.53288422393045920 ) ) ;
#21647 = CARTESIAN_POINT ( 'NONE',  ( 0.8557997880470599172, 47.89938907511594124, 0.9121262075947815795 ) ) ;
#21648 = EDGE_CURVE ( 'NONE', #28915, #42044, #39330, .T. ) ;
#21649 = CARTESIAN_POINT ( 'NONE',  ( 5.860006189529246790, 15.52021937683337605, -45.66786516969914800 ) ) ;
#21650 = CARTESIAN_POINT ( 'NONE',  ( 0.6000166863083106206, 27.66667954482629099, -40.57558779207448652 ) ) ;
#21651 = AXIS2_PLACEMENT_3D ( 'NONE', #3673, #13732, #51600 ) ;
#21652 = VERTEX_POINT ( 'NONE', #12350 ) ;
#21653 = CARTESIAN_POINT ( 'NONE',  ( 4.967162193818130511, -7.970725651239513709, -42.34252806656601820 ) ) ;
#21654 = CARTESIAN_POINT ( 'NONE',  ( 4.975801465491694664, 14.85979367497109571, 45.55012473237758996 ) ) ;
#21655 = CARTESIAN_POINT ( 'NONE',  ( 0.3676999524040323597, -18.60775935196367925, 39.99627326667132365 ) ) ;
#21656 = EDGE_LOOP ( 'NONE', ( #38390, #39844, #20606, #12843 ) ) ;
#21657 = EDGE_CURVE ( 'NONE', #6741, #47578, #13369, .T. ) ;
#21658 = CARTESIAN_POINT ( 'NONE',  ( 3.783278058412226308, -42.86118820526427697, -3.901118461247271352 ) ) ;
#21659 = CARTESIAN_POINT ( 'NONE',  ( 0.3676999524040323597, 16.00695768809450215, -41.10629986868669761 ) ) ;
#21660 = EDGE_CURVE ( 'NONE', #49921, #31310, #58944, .T. ) ;
#21661 = ORIENTED_EDGE ( 'NONE', *, *, #18748, .T. ) ;
#21662 = CARTESIAN_POINT ( 'NONE',  ( 0.6067375320500733027, -33.36326114377794028, -34.36594163291744053 ) ) ;
#21663 = CARTESIAN_POINT ( 'NONE',  ( 0.8557997880470599172, -41.02602466100761802, -24.73961900479294584 ) ) ;
#21664 = ORIENTED_EDGE ( 'NONE', *, *, #33254, .T. ) ;
#21665 = CARTESIAN_POINT ( 'NONE',  ( 0.5980271706414734822, 11.60998973145947311, 47.72061798926192466 ) ) ;
#21666 = ORIENTED_EDGE ( 'NONE', *, *, #39557, .T. ) ;
#21667 = VERTEX_POINT ( 'NONE', #26421 ) ;
#21668 = CARTESIAN_POINT ( 'NONE',  ( 0.9752570700956808558, -5.829291291128961383, 42.51066151201238341 ) ) ;
#21669 = ORIENTED_EDGE ( 'NONE', *, *, #28861, .F. ) ;
#21670 = CARTESIAN_POINT ( 'NONE',  ( 0.3676999524040323597, -13.34038000160386339, 42.04741186726771929 ) ) ;
#21671 = EDGE_CURVE ( 'NONE', #8492, #29973, #41793, .T. ) ;
#21672 = ORIENTED_EDGE ( 'NONE', *, *, #35528, .T. ) ;
#21673 = DIRECTION ( 'NONE',  ( 0.09722883295013595717, 0.2140925343086520494, 0.9719624173786006738 ) ) ;
#21674 = VECTOR ( 'NONE', #54956, 1000.000000000000114 ) ;
#21675 = ORIENTED_EDGE ( 'NONE', *, *, #50786, .F. ) ;
#21676 = DIRECTION ( 'NONE',  ( -1.000000000000000000, -1.836909530733573776E-16, 1.925929944387235853E-32 ) ) ;
#21677 = VECTOR ( 'NONE', #47341, 1000.000000000000000 ) ;
#21678 = CARTESIAN_POINT ( 'NONE',  ( -6.072942160501519027, -14.67202460315916923, 12.47140153845237620 ) ) ;
#21679 = CARTESIAN_POINT ( 'NONE',  ( 0.5817216825391127166, -44.44846903654827486, -14.95220895100342418 ) ) ;
#21680 = TOROIDAL_SURFACE ( 'NONE', #27722, 4.000000000000000000, 0.2500000000000000000 ) ;
#21681 = CARTESIAN_POINT ( 'NONE',  ( 0.5834584762367727162, -30.41620954169410496, 35.69439992672450046 ) ) ;
#21682 = ORIENTED_EDGE ( 'NONE', *, *, #14938, .T. ) ;
#21683 = LINE ( 'NONE', #31707, #54158 ) ;
#21684 = B_SPLINE_CURVE_WITH_KNOTS ( 'NONE', 3,
 ( #50916, #54678, #8302, #21490 ),
 .UNSPECIFIED., .F., .F.,
 ( 4, 4 ),
 ( 0.000000000000000000, 0.004447772540403783365 ),
 .UNSPECIFIED. ) ;
#21685 = ORIENTED_EDGE ( 'NONE', *, *, #14232, .T. ) ;
#21686 =( BOUNDED_SURFACE ( )  B_SPLINE_SURFACE ( 3, 1, ( 
 ( #49588, #7275 ),
 ( #20480, #44615 ),
 ( #6644, #34906 ),
 ( #39929, #1652 ) ),
 .UNSPECIFIED., .F., .F., .F. ) 
 B_SPLINE_SURFACE_WITH_KNOTS ( ( 4, 4 ),
 ( 2, 2 ),
 ( 0.000000000000000000, 1.000000000000000000 ),
 ( 0.000000000000000000, 1.000000000000000000 ),
 .UNSPECIFIED. ) 
 GEOMETRIC_REPRESENTATION_ITEM ( )  RATIONAL_B_SPLINE_SURFACE ( (
 ( 1.000000000000000000, 1.000000000000000000),
 ( 0.9952954269826590483, 0.8620686068821339365),
 ( 0.9952954269826590483, 0.8620686068821339365),
 ( 1.000000000000000000, 1.000000000000000000) ) ) 
 REPRESENTATION_ITEM ( '' )  SURFACE ( )  );
#21687 = CARTESIAN_POINT ( 'NONE',  ( 0.9756950546413937220, 26.19769393035369021, 33.98259063592730200 ) ) ;
#21688 = CARTESIAN_POINT ( 'NONE',  ( 1.479689385636123067, 14.10936131825397233, -41.74337993572934380 ) ) ;
#21689 = ORIENTED_EDGE ( 'NONE', *, *, #12064, .F. ) ;
#21690 = CARTESIAN_POINT ( 'NONE',  ( 7.000000000000005329, 2.650000000000831690, -79.99999999999998579 ) ) ;
#21691 = CARTESIAN_POINT ( 'NONE',  ( 5.901463166500146684, -1.998795974254450103, 20.01306285889146253 ) ) ;
#21692 = LINE ( 'NONE', #11688, #4608 ) ;
#21693 = CARTESIAN_POINT ( 'NONE',  ( -6.001507490154110336, -11.48377994779691136, -14.94036486426024801 ) ) ;
#21694 = ADVANCED_FACE ( 'NONE', ( #11730 ), #51679, .F. ) ;
#21695 = ORIENTED_EDGE ( 'NONE', *, *, #14463, .F. ) ;
#21696 = B_SPLINE_CURVE_WITH_KNOTS ( 'NONE', 3,
 ( #10061, #33880, #29159, #48275 ),
 .UNSPECIFIED., .F., .F.,
 ( 4, 4 ),
 ( 8.673617379884035472E-19, 0.004042984057420971958 ),
 .UNSPECIFIED. ) ;
#21697 = ORIENTED_EDGE ( 'NONE', *, *, #25166, .F. ) ;
#21698 = CARTESIAN_POINT ( 'NONE',  ( 0.2885697896453099376, 15.75356890148099609, 40.13549262224785252 ) ) ;
#21699 = CARTESIAN_POINT ( 'NONE',  ( 1.112077966505211402, 42.15317579919562974, 12.88953432714551184 ) ) ;
#21700 = EDGE_CURVE ( 'NONE', #55402, #37554, #55226, .T. ) ;
#21701 = CARTESIAN_POINT ( 'NONE',  ( -6.017396004339687465, -16.31807101179363784, -9.422598049764795647 ) ) ;
#21702 = CARTESIAN_POINT ( 'NONE',  ( 0.6030672727741701600, 6.365785297724776193, -47.68443224372865075 ) ) ;
#21703 = EDGE_CURVE ( 'NONE', #10512, #52560, #59285, .T. ) ;
#21704 = CARTESIAN_POINT ( 'NONE',  ( 3.221118495291108275, -14.31435738594796803, -41.59159280779119428 ) ) ;
#21705 = CARTESIAN_POINT ( 'NONE',  ( 4.962356264823596597, -3.779019546647577776, 41.91604238389407300 ) ) ;
#21706 = EDGE_CURVE ( 'NONE', #41414, #56562, #7269, .T. ) ;
#21707 = CARTESIAN_POINT ( 'NONE',  ( 0.6009452777970410997, 12.02913818029312765, -46.57942614304346307 ) ) ;
#21708 = EDGE_CURVE ( 'NONE', #52785, #20684, #60542, .T. ) ;
#21709 = CARTESIAN_POINT ( 'NONE',  ( -1.200000000000006617, 0.000000000000000000, -5.612499999999999822 ) ) ;
#21710 = CARTESIAN_POINT ( 'NONE',  ( 1.154321713695928509, 4.782433421670080342, 42.64911660416108674 ) ) ;
#21711 = CARTESIAN_POINT ( 'NONE',  ( 0.9789889208857693870, 32.94939794372522357, 25.89733718335546442 ) ) ;
#21712 = DIRECTION ( 'NONE',  ( -0.07500201931887529039, -0.7485533666540304942, -0.6588190604172040610 ) ) ;
#21713 = DIRECTION ( 'NONE',  ( 0.000000000000000000, 0.000000000000000000, 1.000000000000000000 ) ) ;
#21714 = CARTESIAN_POINT ( 'NONE',  ( 3.678748215320120973, 47.03014671954850456, 13.66667896151895256 ) ) ;
#21715 = CARTESIAN_POINT ( 'NONE',  ( 0.9783242366443540838, -22.77582314543713693, 35.17948791915959106 ) ) ;
#21716 = FACE_OUTER_BOUND ( 'NONE', #39740, .T. ) ;
#21717 = VECTOR ( 'NONE', #6770, 1000.000000000000000 ) ;
#21718 = ADVANCED_FACE ( 'NONE', ( #45258 ), #13302, .T. ) ;
#21719 = CARTESIAN_POINT ( 'NONE',  ( -6.016761891674564211, 18.68243340030203115, 2.456125503350775841 ) ) ;
#21720 = DIRECTION ( 'NONE',  ( 0.000000000000000000, 0.000000000000000000, 1.000000000000000000 ) ) ;
#21722 = VERTEX_POINT ( 'NONE', #59310 ) ;
#21721 = CARTESIAN_POINT ( 'NONE',  ( 4.553261556744875094, 0.000000000000000000, 0.000000000000000000 ) ) ;
#21723 = VERTEX_POINT ( 'NONE', #6984 ) ;
#21724 = STYLED_ITEM ( 'NONE', ( #59522 ), #25822 ) ;
#21725 = AXIS2_PLACEMENT_3D ( 'NONE', #4092, #45828, #46134 ) ;
#21726 = CARTESIAN_POINT ( 'NONE',  ( 0.6027444965799114707, 17.08250209178403267, -46.04048911742398786 ) ) ;
#21727 = CARTESIAN_POINT ( 'NONE',  ( 0.5809828226811553087, -18.83114015454665946, -44.03860873105715967 ) ) ;
#21729 = EDGE_CURVE ( 'NONE', #12531, #22979, #24567, .T. ) ;
#21728 = CARTESIAN_POINT ( 'NONE',  ( 0.9730545539215883499, 6.101350888305258735, -42.47233286818610054 ) ) ;
#21730 = ORIENTED_EDGE ( 'NONE', *, *, #7912, .T. ) ;
#21731 = ORIENTED_EDGE ( 'NONE', *, *, #10409, .F. ) ;
#21732 = CARTESIAN_POINT ( 'NONE',  ( 0.6000166863083106206, -30.20952222014459565, 38.71961065066439289 ) ) ;
#21733 = CARTESIAN_POINT ( 'NONE',  ( 0.1104177457020373010, -37.34442418285517817, 21.56646482560066858 ) ) ;
#21734 = EDGE_CURVE ( 'NONE', #45974, #24292, #48526, .T. ) ;
#21735 = UNCERTAINTY_MEASURE_WITH_UNIT (LENGTH_MEASURE( 1.000000000000000082E-05 ), #11246, 'distance_accuracy_value', 'NONE');
#21736 = ORIENTED_EDGE ( 'NONE', *, *, #32998, .T. ) ;
#21737 = VERTEX_POINT ( 'NONE', #27352 ) ;
#21738 = CARTESIAN_POINT ( 'NONE',  ( 0.9754292580325136797, -37.66327356036682517, 18.37948017820355062 ) ) ;
#21739 = LINE ( 'NONE', #59944, #15980 ) ;
#21740 = CARTESIAN_POINT ( 'NONE',  ( 0.6064515330803550430, 17.51642761181524577, 43.50297805618738778 ) ) ;
#21741 = ORIENTED_EDGE ( 'NONE', *, *, #19893, .F. ) ;
#21742 = CARTESIAN_POINT ( 'NONE',  ( -6.016761891674564211, -2.456125503350841566, 18.68243340030202049 ) ) ;
#21743 = ADVANCED_FACE ( 'NONE', ( #23574 ), #46478, .F. ) ;
#21744 = B_SPLINE_CURVE_WITH_KNOTS ( 'NONE', 3,
 ( #4314, #23450, #28145, #47887 ),
 .UNSPECIFIED., .F., .F.,
 ( 4, 4 ),
 ( 9.697399036122160616E-19, 0.004042984057420974560 ),
 .UNSPECIFIED. ) ;
#21745 = CARTESIAN_POINT ( 'NONE',  ( 9.500000000000000000, 0.000000000000000000, 0.000000000000000000 ) ) ;
#21746 = EDGE_CURVE ( 'NONE', #10214, #37705, #42558, .T. ) ;
#21747 = CARTESIAN_POINT ( 'NONE',  ( 0.1102144999581332885, 21.45299314243942135, 37.40973521037469851 ) ) ;
#21748 = ORIENTED_EDGE ( 'NONE', *, *, #60712, .T. ) ;
#21749 = VECTOR ( 'NONE', #1829, 1000.000000000000114 ) ;
#21750 = ORIENTED_EDGE ( 'NONE', *, *, #14463, .T. ) ;
#21751 = CARTESIAN_POINT ( 'NONE',  ( 0.3622758884714600280, 42.84426538328730771, -4.808133778521432866 ) ) ;
#21752 = LINE ( 'NONE', #43348, #4524 ) ;
#21753 = ORIENTED_EDGE ( 'NONE', *, *, #44659, .F. ) ;
#21754 = CARTESIAN_POINT ( 'NONE',  ( 0.6024113833632038784, -48.73164146766168159, 6.063743807924546481 ) ) ;
#21755 = DIRECTION ( 'NONE',  ( 0.000000000000000000, 0.000000000000000000, 1.000000000000000000 ) ) ;
#21756 = CARTESIAN_POINT ( 'NONE',  ( 0.8751705887134553219, 46.21789262997757675, -13.30665218149314200 ) ) ;
#21757 = DIRECTION ( 'NONE',  ( -0.07439287786467650709, 0.9597484305373229496, -0.2708295585864967658 ) ) ;
#21758 = ORIENTED_EDGE ( 'NONE', *, *, #38146, .F. ) ;
#21759 = CARTESIAN_POINT ( 'NONE',  ( -6.057079549204054558, 19.09779050476951667, -2.470957088998842810 ) ) ;
#21760 = CARTESIAN_POINT ( 'NONE',  ( 0.6031357023905875581, 18.36962560204156247, 44.46217339385177780 ) ) ;
#21761 = CARTESIAN_POINT ( 'NONE',  ( 0.1139756605157200703, -31.97198000184581801, -30.40966481986596293 ) ) ;
#21762 = CARTESIAN_POINT ( 'NONE',  ( 5.901463166500145796, -19.40182753204453903, 5.299713082557885535 ) ) ;
#21763 = ORIENTED_EDGE ( 'NONE', *, *, #42470, .T. ) ;
#21764 = CARTESIAN_POINT ( 'NONE',  ( 5.959547316686252039, 7.851524054666140451, 18.96456592444103606 ) ) ;
#21765 = AXIS2_PLACEMENT_3D ( 'NONE', #39975, #44358, #1387 ) ;
#21766 = CARTESIAN_POINT ( 'NONE',  ( 0.2885700199627514451, -4.828949117912088695, 42.84523253167934342 ) ) ;
#21767 = CARTESIAN_POINT ( 'NONE',  ( 0.7948878604505665857, -48.57723113705768014, 7.138015295254673376 ) ) ;
#21768 = CARTESIAN_POINT ( 'NONE',  ( -6.016104459813374383, -4.882138007282878611, 18.19977249352309201 ) ) ;
#21769 =( BOUNDED_SURFACE ( )  B_SPLINE_SURFACE ( 3, 1, ( 
 ( #59793, #12823 ),
 ( #46332, #21900 ),
 ( #55387, #2459 ),
 ( #17203, #31916 ) ),
 .UNSPECIFIED., .F., .F., .F. ) 
 B_SPLINE_SURFACE_WITH_KNOTS ( ( 4, 4 ),
 ( 2, 2 ),
 ( 0.000000000000000000, 1.000000000000000000 ),
 ( 0.000000000000000000, 1.000000000000000000 ),
 .UNSPECIFIED. ) 
 GEOMETRIC_REPRESENTATION_ITEM ( )  RATIONAL_B_SPLINE_SURFACE ( (
 ( 1.000000000000000000, 1.000000000000000000),
 ( 0.9953390228620291325, 0.8624445117761032620),
 ( 0.9953390228620291325, 0.8624445117761032620),
 ( 1.000000000000000000, 1.000000000000000000) ) ) 
 REPRESENTATION_ITEM ( '' )  SURFACE ( )  );
#21770 = VECTOR ( 'NONE', #29355, 1000.000000000000000 ) ;
#21771 = ORIENTED_EDGE ( 'NONE', *, *, #34883, .F. ) ;
#21772 = CARTESIAN_POINT ( 'NONE',  ( 1.000433927950262536, -41.76690239855643938, 3.456087626537701407 ) ) ;
#21773 = TOROIDAL_SURFACE ( 'NONE', #1759, 5.100000000000000533, 0.09999999999999982514 ) ;
#21774 = DIRECTION ( 'NONE',  ( 0.000000000000000000, 0.000000000000000000, 1.000000000000000000 ) ) ;
#21775 = EDGE_CURVE ( 'NONE', #10287, #59424, #61160, .T. ) ;
#21776 = CARTESIAN_POINT ( 'NONE',  ( 0.8557997880470599172, -0.9121262075949487791, 47.89938907511593413 ) ) ;
#21777 = B_SPLINE_CURVE_WITH_KNOTS ( 'NONE', 3,
 ( #20202, #25807, #57760, #15806, #15496, #29887 ),
 .UNSPECIFIED., .F., .F.,
 ( 4, 2, 4 ),
 ( 8.542522420166516410E-18, 0.0002291472222819941282, 0.0004582944445639797453 ),
 .UNSPECIFIED. ) ;
#21778 = PRODUCT_DEFINITION_SHAPE ( 'NONE', 'NONE',  #40600 ) ;
#21779 = EDGE_CURVE ( 'NONE', #51250, #37892, #18277, .T. ) ;
#21780 = CARTESIAN_POINT ( 'NONE',  ( 1.154321713695927398, -15.65787958845389305, -39.95809834491020496 ) ) ;
#21781 = B_SPLINE_CURVE_WITH_KNOTS ( 'NONE', 3,
 ( #11781, #50580, #1721, #2345 ),
 .UNSPECIFIED., .F., .F.,
 ( 4, 4 ),
 ( 0.000000000000000000, 0.004445488388166992516 ),
 .UNSPECIFIED. ) ;
#21782 = CARTESIAN_POINT ( 'NONE',  ( -5.995132425357893702, -16.32377331145314159, -9.414704407577975331 ) ) ;
#21783 = CARTESIAN_POINT ( 'NONE',  ( -5.995132425357893702, 18.19985213254571477, 4.885449473615395277 ) ) ;
#21784 = CARTESIAN_POINT ( 'NONE',  ( 0.9756950546413942771, -5.696573146291698642, -42.52863374229713145 ) ) ;
#21785 = CARTESIAN_POINT ( 'NONE',  ( 0.9268187852002115479, -32.35242309955501838, -29.95121120248737512 ) ) ;
#21786 = EDGE_CURVE ( 'NONE', #10837, #9740, #28336, .T. ) ;
#21787 = CARTESIAN_POINT ( 'NONE',  ( -6.017396004339686577, 2.460690056887785193, 18.68180398134251163 ) ) ;
#21788 = EDGE_CURVE ( 'NONE', #57221, #20594, #2921, .T. ) ;
#21789 = CARTESIAN_POINT ( 'NONE',  ( 0.2940133293163010864, 36.52812821143385946, 24.73734826021361854 ) ) ;
#21790 = EDGE_LOOP ( 'NONE', ( #35803, #57882, #13990, #50114 ) ) ;
#21791 = EDGE_CURVE ( 'NONE', #27783, #16005, #8263, .T. ) ;
#21792 = CARTESIAN_POINT ( 'NONE',  ( 3.782625744892852637, -41.79414713758510658, 4.526297508658760904 ) ) ;
#21793 = CARTESIAN_POINT ( 'NONE',  ( 1.231276596079881047, 41.42457922925067493, 6.425029704024775690 ) ) ;
#21794 = CYLINDRICAL_SURFACE ( 'NONE', #47994, 2.649999999999997691 ) ;
#21795 = CARTESIAN_POINT ( 'NONE',  ( 5.901463166500146684, -11.91875711499662138, 16.20065119599684422 ) ) ;
#21796 = CARTESIAN_POINT ( 'NONE',  ( 5.838029081930955932, -46.81003243000938596, -6.315530227494003945 ) ) ;
#21797 = PRODUCT_CONTEXT ( 'NONE', #44793, 'mechanical' ) ;
#21798 = DIRECTION ( 'NONE',  ( -0.1024043820194934507, -0.1428674944016075643, 0.9844298967354720986 ) ) ;
#21799 = B_SPLINE_CURVE_WITH_KNOTS ( 'NONE', 3,
 ( #17984, #37101, #56167, #13276, #61168, #56468 ),
 .UNSPECIFIED., .F., .F.,
 ( 4, 2, 4 ),
 ( 6.040475531737861741E-18, 0.0002291472222819937216, 0.0004582944445639813716 ),
 .UNSPECIFIED. ) ;
#21800 = ADVANCED_FACE ( 'NONE', ( #43018 ), #16288, .T. ) ;
#21801 = CARTESIAN_POINT ( 'NONE',  ( 0.9791128995231614951, -6.965612749997687203, 41.32575072836828411 ) ) ;
#21802 = AXIS2_PLACEMENT_3D ( 'NONE', #53072, #48383, #5445 ) ;
#21803 = CARTESIAN_POINT ( 'NONE',  ( 0.6027935024548037868, 0.1745403365871484036, -48.10716172909472022 ) ) ;
#21805 = ORIENTED_EDGE ( 'NONE', *, *, #5343, .F. ) ;
#21804 = DIRECTION ( 'NONE',  ( -0.1011922191286467460, -0.7491372366378198366, -0.6546400044837399346 ) ) ;
#21806 = VERTEX_POINT ( 'NONE', #12974 ) ;
#21807 = CARTESIAN_POINT ( 'NONE',  ( 0.9730545539215883499, 42.47233286818625686, -6.101350888304211573 ) ) ;
#21808 = CARTESIAN_POINT ( 'NONE',  ( 4.975610109902397937, 0.000000000000000000, 0.000000000000000000 ) ) ;
#21809 = CYLINDRICAL_SURFACE ( 'NONE', #8776, 72.00000000000002842 ) ;
#21810 = ORIENTED_EDGE ( 'NONE', *, *, #18753, .F. ) ;
#21811 = DIRECTION ( 'NONE',  ( 0.000000000000000000, 0.000000000000000000, 1.000000000000000000 ) ) ;
#21812 = CARTESIAN_POINT ( 'NONE',  ( 0.8751705887134423323, 41.19904111682474479, 24.81530984069222256 ) ) ;
#21813 = ORIENTED_EDGE ( 'NONE', *, *, #18988, .F. ) ;
#21814 = ORIENTED_EDGE ( 'NONE', *, *, #23611, .T. ) ;
#21815 = DIRECTION ( 'NONE',  ( -1.000000000000000000, -0.000000000000000000, -0.000000000000000000 ) ) ;
#21816 = VECTOR ( 'NONE', #9958, 1000.000000000000114 ) ;
#21817 = CARTESIAN_POINT ( 'NONE',  ( 0.1103878639767399000, -11.20830530106163891, -41.64243544356624938 ) ) ;
#21818 = B_SPLINE_CURVE_WITH_KNOTS ( 'NONE', 3,
 ( #58710, #39979, #59030, #35260 ),
 .UNSPECIFIED., .F., .F.,
 ( 4, 4 ),
 ( 9.757819552369539906E-19, 0.004446298630425105786 ),
 .UNSPECIFIED. ) ;
#21819 = CARTESIAN_POINT ( 'NONE',  ( 0.6027935024548037868, 41.57475399306886743, 24.20473723001711264 ) ) ;
#21820 = ORIENTED_EDGE ( 'NONE', *, *, #28831, .F. ) ;
#21821 = CARTESIAN_POINT ( 'NONE',  ( 0.1129192098497447394, -42.80154921430116843, -10.72283417016740259 ) ) ;
#21822 = FACE_OUTER_BOUND ( 'NONE', #26671, .T. ) ;
#21823 = ORIENTED_EDGE ( 'NONE', *, *, #19005, .F. ) ;
#21824 = EDGE_CURVE ( 'NONE', #61119, #25777, #24812, .T. ) ;
#21825 = CARTESIAN_POINT ( 'NONE',  ( 0.1119898979215349644, 29.24697001900925741, -33.03900805046971811 ) ) ;
#21826 = DIRECTION ( 'NONE',  ( -1.000000000000000000, -3.135800716341489291E-16, 1.298891185607901956E-16 ) ) ;
#21827 = ORIENTED_EDGE ( 'NONE', *, *, #47810, .T. ) ;
#21828 = CARTESIAN_POINT ( 'NONE',  ( -6.015611763856276717, -18.84324252354755203, -0.006214430185339674118 ) ) ;
#21829 = VECTOR ( 'NONE', #61505, 1000.000000000000114 ) ;
#21830 = B_SPLINE_CURVE_WITH_KNOTS ( 'NONE', 3,
 ( #50831, #59608, #17034, #36149, #44620, #55213, #60220, #20798, #39936, #58993 ),
 .UNSPECIFIED., .F., .F.,
 ( 4, 3, 3, 4 ),
 ( 1.157434093048479169E-16, 0.0002618519381806257000, 0.0003927759815485975473, 0.0004849530346207898404 ),
 .UNSPECIFIED. ) ;
#21831 = ORIENTED_EDGE ( 'NONE', *, *, #18549, .F. ) ;
#21832 = CARTESIAN_POINT ( 'NONE',  ( 0.6025881611877910160, -47.66695236827171556, -6.495537368245704712 ) ) ;
#21833 = CARTESIAN_POINT ( 'NONE',  ( 0.5832655196449136881, -19.94641636755120828, 42.44261604879714866 ) ) ;
#21834 = CARTESIAN_POINT ( 'NONE',  ( 0.5797568665920715958, 45.05935952018240442, -12.99536179691886062 ) ) ;
#21835 = CARTESIAN_POINT ( 'NONE',  ( -6.001507490154111224, 7.196845540359170457, 17.41542759839266452 ) ) ;
#21836 = ORIENTED_EDGE ( 'NONE', *, *, #19749, .T. ) ;
#21837 = CARTESIAN_POINT ( 'NONE',  ( 0.1073791018717483448, -43.12183934961191056, 0.4849339620931858996 ) ) ;
#21838 = CARTESIAN_POINT ( 'NONE',  ( 0.1139756605157204450, 39.58051477185625089, -19.50225807669184164 ) ) ;
#21839 = ORIENTED_EDGE ( 'NONE', *, *, #45305, .F. ) ;
#21840 = CARTESIAN_POINT ( 'NONE',  ( 0.2230388203127615099, 42.84312106681675658, 4.873876086128395180 ) ) ;
#21841 =( GEOMETRIC_REPRESENTATION_CONTEXT ( 3 ) GLOBAL_UNCERTAINTY_ASSIGNED_CONTEXT ( ( #23577 ) ) GLOBAL_UNIT_ASSIGNED_CONTEXT ( ( #58512, #30330, #10626 ) ) REPRESENTATION_CONTEXT ( 'NONE', 'WORKASPACE' ) );
#21842 = ORIENTED_EDGE ( 'NONE', *, *, #38177, .T. ) ;
#21843 = CARTESIAN_POINT ( 'NONE',  ( 0.000000000000000000, 0.000000000000000000, -5.294516984716111097 ) ) ;
#21844 = AXIS2_PLACEMENT_3D ( 'NONE', #61279, #33120, #18397 ) ;
#21845 = ORIENTED_EDGE ( 'NONE', *, *, #13665, .F. ) ;
#21846 = DIRECTION ( 'NONE',  ( 0.000000000000000000, 0.000000000000000000, 1.000000000000000000 ) ) ;
#21847 = DIRECTION ( 'NONE',  ( 1.000000000000000000, 0.000000000000000000, 0.000000000000000000 ) ) ;
#21848 = CARTESIAN_POINT ( 'NONE',  ( 0.1084644655670280039, -25.93599432281523676, 34.45367667780522680 ) ) ;
#21849 = ORIENTED_EDGE ( 'NONE', *, *, #32543, .T. ) ;
#21850 = CARTESIAN_POINT ( 'NONE',  ( 0.5980894510889457338, -44.17723055703965684, 19.05812566676427977 ) ) ;
#21851 = CARTESIAN_POINT ( 'NONE',  ( 0.5786265663353153954, 33.35675271369586881, -34.37803667029777444 ) ) ;
#21852 = CARTESIAN_POINT ( 'NONE',  ( 0.5824935313925951874, -41.69004938736499355, 21.47505434528411428 ) ) ;
#21853 = VERTEX_POINT ( 'NONE', #58293 ) ;
#21854 = EDGE_CURVE ( 'NONE', #31453, #1858, #47320, .T. ) ;
#21855 = EDGE_LOOP ( 'NONE', ( #9125, #18893 ) ) ;
#21856 = CARTESIAN_POINT ( 'NONE',  ( 0.9762797500689124330, 29.49606728235556830, -29.77090526101713763 ) ) ;
#21857 = CARTESIAN_POINT ( 'NONE',  ( 4.962356264823608143, 0.000000000000000000, 0.000000000000000000 ) ) ;
#21858 = DIRECTION ( 'NONE',  ( 0.000000000000000000, 0.000000000000000000, 1.000000000000000000 ) ) ;
#21859 = CARTESIAN_POINT ( 'NONE',  ( 0.9730545539215883499, -30.69604515769671949, 29.98130006528850444 ) ) ;
#21860 = CARTESIAN_POINT ( 'NONE',  ( 0.1119899015040012741, 33.23178756756905727, 29.02773851433260788 ) ) ;
#21861 = ORIENTED_EDGE ( 'NONE', *, *, #31764, .T. ) ;
#21862 = EDGE_CURVE ( 'NONE', #1609, #30886, #50741, .T. ) ;
#21863 = CARTESIAN_POINT ( 'NONE',  ( 3.238931869106853600, 12.88361013339106620, 41.01619136531531495 ) ) ;
#21864 = EDGE_CURVE ( 'NONE', #55183, #5629, #20125, .T. ) ;
#21865 = CARTESIAN_POINT ( 'NONE',  ( 4.549368137175248350, -18.79584381673559079, 38.59302160394720005 ) ) ;
#21866 = ORIENTED_EDGE ( 'NONE', *, *, #7029, .T. ) ;
#21867 = CIRCLE ( 'NONE', #10821, 43.92652462719577500 ) ;
#21868 = EDGE_CURVE ( 'NONE', #12730, #41236, #11152, .T. ) ;
#21869 = CARTESIAN_POINT ( 'NONE',  ( -6.078726893082806448, 16.77644806189609739, 9.452239506869414498 ) ) ;
#21870 = CARTESIAN_POINT ( 'NONE',  ( 4.962356264823602814, -29.56943756613081931, -29.94802096775409339 ) ) ;
#21871 = CARTESIAN_POINT ( 'NONE',  ( 0.8554163680231738898, -39.19027442586735788, 25.79395013442155715 ) ) ;
#21872 = CARTESIAN_POINT ( 'NONE',  ( -2.739355103387248747, 7.136887160706232969, 13.11153723277188732 ) ) ;
#21873 = FACE_OUTER_BOUND ( 'NONE', #46415, .T. ) ;
#21874 = FACE_OUTER_BOUND ( 'NONE', #8642, .T. ) ;
#21875 = DIRECTION ( 'NONE',  ( 0.000000000000000000, 0.000000000000000000, 1.000000000000000000 ) ) ;
#21876 = SURFACE_SIDE_STYLE ('',( #3663 ) ) ;
#21877 = CARTESIAN_POINT ( 'NONE',  ( 0.6023143664670691511, 38.00627775314922729, 29.49326149840245392 ) ) ;
#21878 =( BOUNDED_SURFACE ( )  B_SPLINE_SURFACE ( 3, 1, ( 
 ( #19894, #34288 ),
 ( #34914, #39009 ),
 ( #59300, #15185 ),
 ( #15489, #53366 ) ),
 .UNSPECIFIED., .F., .F., .F. ) 
 B_SPLINE_SURFACE_WITH_KNOTS ( ( 4, 4 ),
 ( 2, 2 ),
 ( 0.000000000000000000, 1.000000000000000000 ),
 ( 0.000000000000000000, 1.000000000000000000 ),
 .UNSPECIFIED. ) 
 GEOMETRIC_REPRESENTATION_ITEM ( )  RATIONAL_B_SPLINE_SURFACE ( (
 ( 1.000000000000000000, 1.000000000000000000),
 ( 0.9953040768229013402, 0.8617119497784988535),
 ( 0.9953040768229013402, 0.8617119497784988535),
 ( 1.000000000000000000, 1.000000000000000000) ) ) 
 REPRESENTATION_ITEM ( '' )  SURFACE ( )  );
#21879 = B_SPLINE_CURVE_WITH_KNOTS ( 'NONE', 3,
 ( #31146, #1089, #2317, #49634 ),
 .UNSPECIFIED., .F., .F.,
 ( 4, 4 ),
 ( 0.000000000000000000, 0.004447772540403811120 ),
 .UNSPECIFIED. ) ;
#21880 = CARTESIAN_POINT ( 'NONE',  ( 0.1073791018717483448, -30.83464511437118816, -30.14884492832378626 ) ) ;
#21881 = DIRECTION ( 'NONE',  ( 0.000000000000000000, 1.000000000000000000, -1.224646799147353207E-16 ) ) ;
#21882 = CARTESIAN_POINT ( 'NONE',  ( 5.958863334805807099, 7.853699934219900314, -18.96369761673811638 ) ) ;
#21884 = EDGE_CURVE ( 'NONE', #17235, #35184, #47765, .T. ) ;
#21883 = CARTESIAN_POINT ( 'NONE',  ( 4.322998006666165516, 45.10383234877033232, -16.38761975793161696 ) ) ;
#21885 = AXIS2_PLACEMENT_3D ( 'NONE', #43381, #33362, #4805 ) ;
#21886 = CARTESIAN_POINT ( 'NONE',  ( -1.500000000000001332, 0.000000000000000000, 0.000000000000000000 ) ) ;
#21887 = CARTESIAN_POINT ( 'NONE',  ( 5.895596859100789899, 16.58392706178521792, -11.37987462241457948 ) ) ;
#21888 = EDGE_CURVE ( 'NONE', #3087, #46201, #21572, .T. ) ;
#21889 = CARTESIAN_POINT ( 'NONE',  ( 1.227938101723748288, -41.23019537246701560, -11.92353943227992197 ) ) ;
#21890 = CARTESIAN_POINT ( 'NONE',  ( 0.5800708057587400379, -47.40012370174856926, -6.873290064481863304 ) ) ;
#21891 =( BOUNDED_SURFACE ( )  B_SPLINE_SURFACE ( 3, 1, ( 
 ( #39003, #58359 ),
 ( #12646, #50523 ),
 ( #2277, #55521 ),
 ( #21100, #45245 ) ),
 .UNSPECIFIED., .F., .F., .F. ) 
 B_SPLINE_SURFACE_WITH_KNOTS ( ( 4, 4 ),
 ( 2, 2 ),
 ( 0.000000000000000000, 1.000000000000000000 ),
 ( 0.000000000000000000, 1.000000000000000000 ),
 .UNSPECIFIED. ) 
 GEOMETRIC_REPRESENTATION_ITEM ( )  RATIONAL_B_SPLINE_SURFACE ( (
 ( 1.000000000000000000, 1.000000000000000000),
 ( 0.9732289882329797637, 0.9999525324661233672),
 ( 0.9732289882329797637, 0.9999525324661233672),
 ( 1.000000000000000000, 1.000000000000000000) ) ) 
 REPRESENTATION_ITEM ( '' )  SURFACE ( )  );
#21892 = ORIENTED_EDGE ( 'NONE', *, *, #15884, .T. ) ;
#21893 = DIRECTION ( 'NONE',  ( 1.000000000000000000, 0.000000000000000000, 0.000000000000000000 ) ) ;
#21894 = CARTESIAN_POINT ( 'NONE',  ( 0.5806925824938499181, -19.24316026636448029, -42.76591101925195204 ) ) ;
#21895 = B_SPLINE_CURVE_WITH_KNOTS ( 'NONE', 3,
 ( #47608, #47296, #18484, #38534 ),
 .UNSPECIFIED., .F., .F.,
 ( 4, 4 ),
 ( 0.000000000000000000, 0.004447772540403798977 ),
 .UNSPECIFIED. ) ;
#21896 = CARTESIAN_POINT ( 'NONE',  ( 0.1155031312995260795, -38.36323999597067314, -21.79916167065524846 ) ) ;
#21897 = CARTESIAN_POINT ( 'NONE',  ( 0.9762797500689124330, -41.84568905980455611, -2.294143041716810050 ) ) ;
#21898 = ORIENTED_EDGE ( 'NONE', *, *, #42724, .F. ) ;
#21899 = CARTESIAN_POINT ( 'NONE',  ( 5.965394784446460541, 20.52536205633085231, 0.01447339372460269141 ) ) ;
#21900 = CARTESIAN_POINT ( 'NONE',  ( 0.5786265663353196143, -34.37803667029834287, 33.35675271369526484 ) ) ;
#21901 = DIRECTION ( 'NONE',  ( 1.000000000000000000, 0.000000000000000000, 0.000000000000000000 ) ) ;
#21902 = ORIENTED_EDGE ( 'NONE', *, *, #30895, .T. ) ;
#21903 = EDGE_CURVE ( 'NONE', #44595, #30566, #19360, .T. ) ;
#21904 = CARTESIAN_POINT ( 'NONE',  ( 4.960386119450145515, -37.88391031994010660, -21.89168343328299216 ) ) ;
#21905 = ORIENTED_EDGE ( 'NONE', *, *, #61166, .F. ) ;
#21906 = AXIS2_PLACEMENT_3D ( 'NONE', #28811, #5291, #24418 ) ;
#21907 = CARTESIAN_POINT ( 'NONE',  ( 1.500000000000001332, 0.000000000000000000, 0.000000000000000000 ) ) ;
#21909 = FACE_OUTER_BOUND ( 'NONE', #54734, .T. ) ;
#21908 = CIRCLE ( 'NONE', #3857, 48.09070567114147110 ) ;
#21910 = VERTEX_POINT ( 'NONE', #5973 ) ;
#21911 = ORIENTED_EDGE ( 'NONE', *, *, #29576, .T. ) ;
#21912 = CARTESIAN_POINT ( 'NONE',  ( 0.7764139734771211554, 42.82684529576456356, 19.12855961434408059 ) ) ;
#21913 = CARTESIAN_POINT ( 'NONE',  ( 0.1103744047535531458, -26.22174028894846032, -34.23648668783384608 ) ) ;
#21914 = VERTEX_POINT ( 'NONE', #39550 ) ;
#21915 = FACE_OUTER_BOUND ( 'NONE', #6017, .T. ) ;
#21916 = ORIENTED_EDGE ( 'NONE', *, *, #43960, .T. ) ;
#21917 = CARTESIAN_POINT ( 'NONE',  ( 0.1145239942831223490, -1.740630560447053554, 44.08985921906205618 ) ) ;
#21918 = B_SPLINE_CURVE_WITH_KNOTS ( 'NONE', 3,
 ( #34829, #11020, #33140, #50749 ),
 .UNSPECIFIED., .F., .F.,
 ( 4, 4 ),
 ( 2.175771182130668512E-17, 0.004559932413162187670 ),
 .UNSPECIFIED. ) ;
#21919 = AXIS2_PLACEMENT_3D ( 'NONE', #53115, #56886, #28091 ) ;
#21920 = ORIENTED_EDGE ( 'NONE', *, *, #17137, .T. ) ;
#21921 = ORIENTED_EDGE ( 'NONE', *, *, #21864, .T. ) ;
#21922 = CARTESIAN_POINT ( 'NONE',  ( 0.6041374136657475802, -33.89363087703024746, -34.14050483116125179 ) ) ;
#21923 = CARTESIAN_POINT ( 'NONE',  ( -6.078726893082806448, -16.13637198556907748, 10.50768958487361537 ) ) ;
#21924 = CARTESIAN_POINT ( 'NONE',  ( 3.680974057930774812, -25.57193971028188173, 40.59247216052809648 ) ) ;
#21925 = CARTESIAN_POINT ( 'NONE',  ( 4.975610109902397937, 0.000000000000000000, 0.000000000000000000 ) ) ;
#21926 = CARTESIAN_POINT ( 'NONE',  ( 4.956653778116961284, 40.28700667097682953, 26.26162724282386662 ) ) ;
#21927 = ORIENTED_EDGE ( 'NONE', *, *, #40080, .T. ) ;
#21928 = CARTESIAN_POINT ( 'NONE',  ( 3.559346040607745287, 6.262100278120851016, 43.52259621907622034 ) ) ;
#21929 = CARTESIAN_POINT ( 'NONE',  ( 0.7245667037590747261, 7.091191019330228329, 47.57651946688181255 ) ) ;
#21930 = CARTESIAN_POINT ( 'NONE',  ( -6.063463321072278589, 16.78636876910494991, -9.436009539370331822 ) ) ;
#21931 = ORIENTED_EDGE ( 'NONE', *, *, #47323, .T. ) ;
#21932 = VERTEX_POINT ( 'NONE', #14808 ) ;
#21933 = EDGE_CURVE ( 'NONE', #25319, #55402, #34702, .T. ) ;
#21934 = DIRECTION ( 'NONE',  ( 0.000000000000000000, 0.000000000000000000, -1.000000000000000000 ) ) ;
#21935 = CARTESIAN_POINT ( 'NONE',  ( 7.999999999999983125, 80.00000000000001421, -9.340760230278089508E-32 ) ) ;
#21936 = DIRECTION ( 'NONE',  ( -0.1011922191286467460, 0.5046905544709733293, 0.8573491581704628661 ) ) ;
#21937 = VERTEX_POINT ( 'NONE', #1594 ) ;
#21938 = CARTESIAN_POINT ( 'NONE',  ( 0.1098349054025746785, -42.72717686504326196, -5.840292671757516985 ) ) ;
#21939 = LINE ( 'NONE', #36986, #49735 ) ;
#21940 = ADVANCED_FACE ( 'NONE', ( #30117 ), #16956, .F. ) ;
#21941 = VERTEX_POINT ( 'NONE', #31365 ) ;
#21942 = LINE ( 'NONE', #41080, #56942 ) ;
#21943 = ORIENTED_EDGE ( 'NONE', *, *, #43622, .T. ) ;
#21944 = B_SPLINE_CURVE_WITH_KNOTS ( 'NONE', 3,
 ( #2403, #12449, #35029, #54088, #2084, #45054, #21216, #59103, #50631, #3019, #7721, #21525, #40661, #11210, #26842, #45977 ),
 .UNSPECIFIED., .F., .F.,
 ( 4, 3, 3, 3, 3, 4 ),
 ( 1.868480190406682863E-17, 0.0002618515315864400252, 0.0003927756766341985875, 0.0005236998216950590826, 0.0007855159896329929345, 0.001047349442285931773 ),
 .UNSPECIFIED. ) ;
#21945 = EDGE_CURVE ( 'NONE', #199, #11845, #21040, .T. ) ;
#21946 = DIRECTION ( 'NONE',  ( 1.000000000000000000, 0.000000000000000000, 0.000000000000000000 ) ) ;
#21947 = CARTESIAN_POINT ( 'NONE',  ( 0.5782707292762442330, -13.20261929687983837, -45.00474638756754331 ) ) ;
#21948 = CARTESIAN_POINT ( 'NONE',  ( 0.9787284016396609054, 9.533035904949169748, -40.81001378784110045 ) ) ;
#21949 = CARTESIAN_POINT ( 'NONE',  ( 0.7246131072078564328, -5.464103862701177761, -47.79072675905339906 ) ) ;
#21950 = AXIS2_PLACEMENT_3D ( 'NONE', #38867, #4986, #57921 ) ;
#21951 = VERTEX_POINT ( 'NONE', #11976 ) ;
#21952 = CARTESIAN_POINT ( 'NONE',  ( 5.896278296736517710, 19.00178995741550025, -6.592340861078650249 ) ) ;
#21953 = FACE_OUTER_BOUND ( 'NONE', #49509, .T. ) ;
#21954 = CARTESIAN_POINT ( 'NONE',  ( 4.956445790443988031, 0.000000000000000000, 0.000000000000000000 ) ) ;
#21955 = CARTESIAN_POINT ( 'NONE',  ( 0.1103310638050661457, 21.63353985999688689, -37.30561229499308951 ) ) ;
#21956 = VECTOR ( 'NONE', #21017, 1000.000000000000227 ) ;
#21957 = B_SPLINE_CURVE_WITH_KNOTS ( 'NONE', 3,
 ( #10245, #57828, #43470, #19652, #29339, #5510, #832, #30874, #21801, #54978, #27113, #40934, #2361, #12410, #55594, #59997, #12725, #22105, #35292 ),
 .UNSPECIFIED., .F., .F.,
 ( 4, 3, 3, 3, 3, 3, 4 ),
 ( 8.674294979774126656E-18, 0.0002732106629380623777, 0.0004098138914053778715, 0.0005464171197651505928, 0.0006830203481512616207, 0.0008196235766963705718, 0.001011968216111141594 ),
 .UNSPECIFIED. ) ;
#21958 = CARTESIAN_POINT ( 'NONE',  ( 0.9757402383260946888, 37.20221273948040164, -21.38067434779540932 ) ) ;
#21959 = CARTESIAN_POINT ( 'NONE',  ( 0.8751705887134553219, -44.08562551107095828, 19.22545746485582185 ) ) ;
#21960 = CARTESIAN_POINT ( 'NONE',  ( 1.231276596079881047, 32.36747132271556637, 26.63876069172986405 ) ) ;
#21961 = ADVANCED_FACE ( 'NONE', ( #55153 ), #23342, .F. ) ;
#21962 = CARTESIAN_POINT ( 'NONE',  ( 0.5806925824938502512, -8.338382001837375768, -46.14860504863607105 ) ) ;
#21963 = CARTESIAN_POINT ( 'NONE',  ( 2.281351352603296245, 7.562287671717891513, -47.37344280316137457 ) ) ;
#21964 = B_SPLINE_CURVE_WITH_KNOTS ( 'NONE', 3,
 ( #40226, #38980, #15161, #20170 ),
 .UNSPECIFIED., .F., .F.,
 ( 4, 4 ),
 ( 2.230302957514598322E-17, 0.004564976165746189446 ),
 .UNSPECIFIED. ) ;
#21965 = CARTESIAN_POINT ( 'NONE',  ( 0.5809828226811553087, 23.47450554821769231, -41.74875432577623258 ) ) ;
#21966 = CARTESIAN_POINT ( 'NONE',  ( 0.7246131072078584312, 33.42811616637872163, 34.58859703353090964 ) ) ;
#21967 = ORIENTED_EDGE ( 'NONE', *, *, #12189, .T. ) ;
#21968 = B_SPLINE_CURVE_WITH_KNOTS ( 'NONE', 3,
 ( #35179, #39576, #1939, #40207, #53022, #10122, #38963, #24521, #20149, #15757, #48335, #58316, #15444, #34553, #25137, #44279, #41127, #35800, #50487, #21374, #54865, #50186, #32016, #45208, #36115, #8185, #22302, #2558 ),
 .UNSPECIFIED., .F., .F.,
 ( 4, 2, 2, 2, 2, 2, 2, 2, 2, 2, 2, 2, 2, 4 ),
 ( 0.008308694440061006881, 0.009347008373300980805, 0.009866165339920957358, 0.01038532230654093391, 0.01090447927316091220, 0.01142363623978088875, 0.01246195017302085400, 0.01298110713964083576, 0.01350026410626081752, 0.01401942107288079928, 0.01453857803950078104, 0.01557689197274074455, 0.01609604893936073672, 0.01661520590598072888 ),
 .UNSPECIFIED. ) ;
#21969 = VECTOR ( 'NONE', #45264, 1000.000000000000114 ) ;
#21970 = CARTESIAN_POINT ( 'NONE',  ( -1.399999999999998579, 6.184466335694134054E-16, 5.000000000000000000 ) ) ;
#21971 = CARTESIAN_POINT ( 'NONE',  ( 0.6001305935487315502, -47.62765676940948367, 6.798494447611417968 ) ) ;
#21972 = CARTESIAN_POINT ( 'NONE',  ( 4.226256110419178924, -41.83098940882571526, 13.45345959468784081 ) ) ;
#21973 = EDGE_LOOP ( 'NONE', ( #3049, #10716, #32723, #2783 ) ) ;
#21974 = CARTESIAN_POINT ( 'NONE',  ( -2.569797478183783568, -8.547745408040883675, 11.87678401312179943 ) ) ;
#21975 = CARTESIAN_POINT ( 'NONE',  ( 5.860006189529234355, -26.78264244998126742, 40.11385274514673682 ) ) ;
#21976 = LINE ( 'NONE', #30422, #43714 ) ;
#21977 = VERTEX_POINT ( 'NONE', #60163 ) ;
#21978 = FACE_OUTER_BOUND ( 'NONE', #48352, .T. ) ;
#21979 = EDGE_CURVE ( 'NONE', #60249, #28915, #11954, .T. ) ;
#21980 = LINE ( 'NONE', #6917, #52528 ) ;
#21981 = CARTESIAN_POINT ( 'NONE',  ( 2.185380717157383135, -11.14258708398306297, 42.59885627740553815 ) ) ;
#21982 = EDGE_LOOP ( 'NONE', ( #681, #32604, #21300, #11935 ) ) ;
#21983 = CARTESIAN_POINT ( 'NONE',  ( 0.5804410086790514622, 5.237717535875747288, -46.60564522533483256 ) ) ;
#21984 = VERTEX_POINT ( 'NONE', #26350 ) ;
#21985 = VERTEX_POINT ( 'NONE', #16656 ) ;
#21986 = CARTESIAN_POINT ( 'NONE',  ( 5.901764892641307547, -22.61189840244690785, -43.43608543684728573 ) ) ;
#21987 = ORIENTED_EDGE ( 'NONE', *, *, #48039, .F. ) ;
#21988 = CARTESIAN_POINT ( 'NONE',  ( 0.2279481005628811452, -13.27919661951364994, 42.07334576918279367 ) ) ;
#21989 = ORIENTED_EDGE ( 'NONE', *, *, #30896, .F. ) ;
#21990 = CARTESIAN_POINT ( 'NONE',  ( -6.078726893082806448, 16.77980020642702641, 9.446287434813308792 ) ) ;
#21991 = B_SPLINE_CURVE_WITH_KNOTS ( 'NONE', 3,
 ( #73, #14520, #56477, #24510, #33934, #52088, #18294, #28904, #37405, #13592, #32700, #51781, #9180, #28290, #47408, #4452, #23591, #42719, #34239 ),
 .UNSPECIFIED., .F., .F.,
 ( 4, 3, 3, 3, 3, 3, 4 ),
 ( 1.153344816771540786E-16, 0.0002618519381806285731, 0.0003927759815485985231, 0.0005237000248299445142, 0.0006546240681325007525, 0.0007855481115631309744, 0.0009699050456655139776 ),
 .UNSPECIFIED. ) ;
#21992 = APPLICATION_CONTEXT ( 'automotive_design' ) ;
#21993 =( BOUNDED_SURFACE ( )  B_SPLINE_SURFACE ( 3, 1, ( 
 ( #37557, #61017 ),
 ( #7782, #27513 ),
 ( #22209, #56011 ),
 ( #12510, #3380 ) ),
 .UNSPECIFIED., .F., .F., .F. ) 
 B_SPLINE_SURFACE_WITH_KNOTS ( ( 4, 4 ),
 ( 2, 2 ),
 ( 0.000000000000000000, 1.000000000000000000 ),
 ( 0.000000000000000000, 1.000000000000000000 ),
 .UNSPECIFIED. ) 
 GEOMETRIC_REPRESENTATION_ITEM ( )  RATIONAL_B_SPLINE_SURFACE ( (
 ( 1.000000000000000000, 1.000000000000000000),
 ( 0.7282232189291694135, 0.9929344683865672927),
 ( 0.7282232189291694135, 0.9929344683865672927),
 ( 1.000000000000000000, 1.000000000000000000) ) ) 
 REPRESENTATION_ITEM ( '' )  SURFACE ( )  );
#21994 = CARTESIAN_POINT ( 'NONE',  ( 0.5980271706414734822, 37.84660806146489875, 31.29989618327069323 ) ) ;
#21995 = VERTEX_POINT ( 'NONE', #39871 ) ;
#21996 = CARTESIAN_POINT ( 'NONE',  ( 42.00000000000000711, 6.547216728259810428E-15, -1.617781153285278467E-30 ) ) ;
#21997 = VECTOR ( 'NONE', #3383, 1000.000000000000000 ) ;
#21998 = CARTESIAN_POINT ( 'NONE',  ( 2.618530812446111078, -46.78761446237182753, -4.543778396737141456 ) ) ;
#21999 = CARTESIAN_POINT ( 'NONE',  ( 4.390527457369402420, -36.99449152968317378, 23.69795208638966599 ) ) ;
#22000 = CARTESIAN_POINT ( 'NONE',  ( 0.7044674535452954967, -7.005514063658970336, -48.60787483026575018 ) ) ;
#22001 = ORIENTED_EDGE ( 'NONE', *, *, #53081, .T. ) ;
#22002 = CARTESIAN_POINT ( 'NONE',  ( -4.467299999999993609, 0.000000000000000000, 0.000000000000000000 ) ) ;
#22003 = ORIENTED_EDGE ( 'NONE', *, *, #53256, .F. ) ;
#22004 = CARTESIAN_POINT ( 'NONE',  ( 5.965394784446460541, 12.48356622107654879, 16.29267539192346703 ) ) ;
#22005 = CARTESIAN_POINT ( 'NONE',  ( 0.5806925824938502512, -25.69265091979982429, -39.23149310256842170 ) ) ;
#22006 = CARTESIAN_POINT ( 'NONE',  ( 4.549368137175248350, 18.79584381673534565, -38.59302160394733505 ) ) ;
#22007 = VERTEX_POINT ( 'NONE', #45185 ) ;
#22008 = CARTESIAN_POINT ( 'NONE',  ( 0.5837374860065636106, -46.31070423340723607, -12.22086613152811196 ) ) ;
#22009 = CARTESIAN_POINT ( 'NONE',  ( 0.6001305935487315502, 11.94532529598313175, 46.60388846085727010 ) ) ;
#22010 = CARTESIAN_POINT ( 'NONE',  ( 0.3676999524040366896, 9.009680404096547690, -43.18305503711933113 ) ) ;
#22011 = SURFACE_SIDE_STYLE ('',( #2880 ) ) ;
#22012 = EDGE_CURVE ( 'NONE', #20260, #14061, #23131, .T. ) ;
#22013 = AXIS2_PLACEMENT_3D ( 'NONE', #44471, #1201, #53808 ) ;
#22014 = ORIENTED_EDGE ( 'NONE', *, *, #30480, .T. ) ;
#22015 = ORIENTED_EDGE ( 'NONE', *, *, #58446, .T. ) ;
#22016 = CARTESIAN_POINT ( 'NONE',  ( 5.895881250540457863, 0.6766202122111161232, -20.10148916614707559 ) ) ;
#22017 = CARTESIAN_POINT ( 'NONE',  ( 2.359973842542475886, 42.23244574406162144, 12.43207227727508624 ) ) ;
#22018 = EDGE_CURVE ( 'NONE', #53354, #50613, #52954, .T. ) ;
#22019 = CARTESIAN_POINT ( 'NONE',  ( 4.553261556744875094, 0.000000000000000000, 0.000000000000000000 ) ) ;
#22020 = CARTESIAN_POINT ( 'NONE',  ( 0.2940135542859004802, -18.59037419722897866, -40.00798090254521355 ) ) ;
#22021 = B_SPLINE_CURVE_WITH_KNOTS ( 'NONE', 3,
 ( #53971, #38691, #1656, #10473, #57748, #43392, #48372, #19574, #44021, #48677, #20797, #29876, #24572, #16101, #39934, #29568, #58991, #25178, #44320 ),
 .UNSPECIFIED., .F., .F.,
 ( 4, 3, 3, 3, 3, 3, 4 ),
 ( 9.813676791237319219E-18, 0.0002724573126191821523, 0.0004086839781548627887, 0.0005449106435902062060, 0.0006811373090491684799, 0.0008459866663933775059, 0.001010840725717205993 ),
 .UNSPECIFIED. ) ;
#22022 = ADVANCED_FACE ( 'NONE', ( #40479 ), #35462, .F. ) ;
#22023 = CARTESIAN_POINT ( 'NONE',  ( 0.5835226383429297226, 4.512830617619511209, -46.67844078761244475 ) ) ;
#22024 = CARTESIAN_POINT ( 'NONE',  ( 4.963659409799330291, 2.450325214228396664, 44.68724496494573373 ) ) ;
#22025 = CARTESIAN_POINT ( 'NONE',  ( 4.962356264823603702, 12.05238263218972072, -40.32338863178092225 ) ) ;
#22026 = CARTESIAN_POINT ( 'NONE',  ( 4.956445790444031552, 34.56007374686835476, -31.98654955994249960 ) ) ;
#22027 = CARTESIAN_POINT ( 'NONE',  ( 0.8753041380234530822, -48.80600061351578489, -5.395612290229643726 ) ) ;
#22028 = CARTESIAN_POINT ( 'NONE',  ( 1.827326673878743923, -15.32882202537249583, -40.22837085190305828 ) ) ;
#22029 = CARTESIAN_POINT ( 'NONE',  ( -6.078075953587585900, 7.789670135765894621, -17.61011679186406909 ) ) ;
#22030 = EDGE_CURVE ( 'NONE', #61620, #49895, #59725, .T. ) ;
#22031 = CARTESIAN_POINT ( 'NONE',  ( 0.5786265663353153954, -47.58023467411535279, -5.535668456754443412 ) ) ;
#22032 = CARTESIAN_POINT ( 'NONE',  ( 0.6029303876144825880, -33.92442033626760178, -34.10953954078129158 ) ) ;
#22033 = DIRECTION ( 'NONE',  ( 0.000000000000000000, 0.000000000000000000, 1.000000000000000000 ) ) ;
#22034 = CARTESIAN_POINT ( 'NONE',  ( 0.9790850452238870627, -22.50762242264617541, 35.35172220900689410 ) ) ;
#22035 = CARTESIAN_POINT ( 'NONE',  ( 0.7242003506639987931, -38.85571581871069213, 30.02074320102056149 ) ) ;
#22036 = B_SPLINE_CURVE_WITH_KNOTS ( 'NONE', 3,
 ( #13028, #41529, #60285, #41225 ),
 .UNSPECIFIED., .F., .F.,
 ( 4, 4 ),
 ( 9.757819552369539906E-19, 0.004444878191957645289 ),
 .UNSPECIFIED. ) ;
#22037 = CARTESIAN_POINT ( 'NONE',  ( 0.9762797500689124330, -41.16654106227479559, 7.851158013551082782 ) ) ;
#22038 = CARTESIAN_POINT ( 'NONE',  ( 0.6016118706126977189, -47.58863909114165125, 12.11909585063984629 ) ) ;
#22040 = ORIENTED_EDGE ( 'NONE', *, *, #11084, .T. ) ;
#22039 = DIRECTION ( 'NONE',  ( -1.000000000000000000, -0.000000000000000000, -0.000000000000000000 ) ) ;
#22041 = EDGE_LOOP ( 'NONE', ( #5003, #30018, #52197, #21425 ) ) ;
#22042 = CARTESIAN_POINT ( 'NONE',  ( 1.000433927950263202, -11.78619540624106854, 40.21820825818511480 ) ) ;
#22043 = CARTESIAN_POINT ( 'NONE',  ( 0.8560838555295158248, -18.91252766612255698, -42.92655508376930129 ) ) ;
#22044 = LINE ( 'NONE', #42098, #19736 ) ;
#22045 = ORIENTED_EDGE ( 'NONE', *, *, #49421, .T. ) ;
#22046 = ORIENTED_EDGE ( 'NONE', *, *, #19966, .T. ) ;
#22047 = CARTESIAN_POINT ( 'NONE',  ( -6.078726893082806448, 12.00325722817150620, -15.05708661006732108 ) ) ;
#22048 = CARTESIAN_POINT ( 'NONE',  ( 0.000000000000000000, 1.178949249685212974, -2.042000000000001148 ) ) ;
#22050 = VERTEX_POINT ( 'NONE', #35776 ) ;
#22049 = AXIS2_PLACEMENT_3D ( 'NONE', #22673, #17988, #11742 ) ;
#22051 = ORIENTED_EDGE ( 'NONE', *, *, #7104, .F. ) ;
#22052 = DIRECTION ( 'NONE',  ( -1.000000000000000000, -0.000000000000000000, -0.000000000000000000 ) ) ;
#22053 = CIRCLE ( 'NONE', #23046, 2.649999999999985700 ) ;
#22054 = CARTESIAN_POINT ( 'NONE',  ( 0.5980894510889457338, -33.52121017007851123, 34.51330645350343929 ) ) ;
#22055 = EDGE_CURVE ( 'NONE', #17208, #15365, #38794, .T. ) ;
#22056 = ORIENTED_EDGE ( 'NONE', *, *, #6674, .T. ) ;
#22057 = FACE_OUTER_BOUND ( 'NONE', #30813, .T. ) ;
#22058 = ADVANCED_FACE ( 'NONE', ( #20733 ), #57697, .F. ) ;
#22059 = CARTESIAN_POINT ( 'NONE',  ( 0.5998501479064708430, -18.89267974119696447, 44.24259072156053918 ) ) ;
#22060 =( BOUNDED_SURFACE ( )  B_SPLINE_SURFACE ( 3, 1, ( 
 ( #40066, #59113 ),
 ( #39434, #15922 ),
 ( #54404, #11526 ),
 ( #39127, #58186 ) ),
 .UNSPECIFIED., .F., .F., .F. ) 
 B_SPLINE_SURFACE_WITH_KNOTS ( ( 4, 4 ),
 ( 2, 2 ),
 ( 0.000000000000000000, 1.000000000000000000 ),
 ( 0.000000000000000000, 1.000000000000000000 ),
 .UNSPECIFIED. ) 
 GEOMETRIC_REPRESENTATION_ITEM ( )  RATIONAL_B_SPLINE_SURFACE ( (
 ( 1.000000000000000000, 1.000000000000000000),
 ( 0.7282232189291694135, 0.9929344683865672927),
 ( 0.7282232189291694135, 0.9929344683865672927),
 ( 1.000000000000000000, 1.000000000000000000) ) ) 
 REPRESENTATION_ITEM ( '' )  SURFACE ( )  );
#22061 = DIRECTION ( 'NONE',  ( -1.000000000000000000, -0.000000000000000000, -0.000000000000000000 ) ) ;
#22062 = ORIENTED_EDGE ( 'NONE', *, *, #19734, .T. ) ;
#22063 = EDGE_CURVE ( 'NONE', #14998, #55315, #8926, .T. ) ;
#22064 = ORIENTED_EDGE ( 'NONE', *, *, #48521, .F. ) ;
#22065 = FACE_OUTER_BOUND ( 'NONE', #35233, .T. ) ;
#22066 = B_SPLINE_CURVE_WITH_KNOTS ( 'NONE', 3,
 ( #5189, #29023, #23709, #61889 ),
 .UNSPECIFIED., .F., .F.,
 ( 4, 4 ),
 ( 1.998817200139820460E-17, 0.004444306975806115029 ),
 .UNSPECIFIED. ) ;
#22067 = EDGE_LOOP ( 'NONE', ( #16947, #15040, #61663, #17651 ) ) ;
#22068 = CARTESIAN_POINT ( 'NONE',  ( 0.9972139404380306882, 20.88226186415282015, -37.48536715150202525 ) ) ;
#22069 = CARTESIAN_POINT ( 'NONE',  ( -6.078075953587585900, 9.986729131371225421, 16.46391252114020887 ) ) ;
#22070 = CARTESIAN_POINT ( 'NONE',  ( -2.569797478183783568, -14.01151037928426035, 4.218948559326007874 ) ) ;
#22071 = CARTESIAN_POINT ( 'NONE',  ( -6.077587904424778920, 12.00112336472165353, 15.05885318935882644 ) ) ;
#22072 = CARTESIAN_POINT ( 'NONE',  ( 0.5839880159502345292, 12.44022138820751167, -46.25220722086333325 ) ) ;
#22073 = ORIENTED_EDGE ( 'NONE', *, *, #17457, .F. ) ;
#22074 = LINE ( 'NONE', #2947, #48907 ) ;
#22075 = CARTESIAN_POINT ( 'NONE',  ( 4.958415959904820980, 37.73202888843250236, -25.28829669600411023 ) ) ;
#22076 = VERTEX_POINT ( 'NONE', #30734 ) ;
#22077 = DIRECTION ( 'NONE',  ( 0.000000000000000000, 0.8660254037844380415, -0.5000000000000012212 ) ) ;
#22078 = DIRECTION ( 'NONE',  ( 1.000000000000000000, 0.000000000000000000, 0.000000000000000000 ) ) ;
#22079 = CARTESIAN_POINT ( 'NONE',  ( 3.661933894777868570, 9.064104546016615416, 46.15704901453876374 ) ) ;
#22080 = CARTESIAN_POINT ( 'NONE',  ( 0.2885700199627513340, 29.91358789498782045, -31.05173037893211330 ) ) ;
#22081 = EDGE_CURVE ( 'NONE', #26674, #57948, #7337, .T. ) ;
#22082 = VERTEX_POINT ( 'NONE', #41713 ) ;
#22083 = FACE_OUTER_BOUND ( 'NONE', #12464, .T. ) ;
#22084 = ADVANCED_FACE ( 'NONE', ( #8784 ), #47306, .F. ) ;
#22085 = LINE ( 'NONE', #59978, #48680 ) ;
#22086 = CARTESIAN_POINT ( 'NONE',  ( 2.526464513654346433, 37.81242626108694793, 20.43088802552575700 ) ) ;
#22087 = EDGE_CURVE ( 'NONE', #32685, #29292, #44017, .T. ) ;
#22088 = CARTESIAN_POINT ( 'NONE',  ( 0.9722240741986374335, -15.88116971565358959, -39.86121768686903977 ) ) ;
#22089 = CARTESIAN_POINT ( 'NONE',  ( 0.5806925824938499181, -46.82446035038572063, 2.586943222941027631 ) ) ;
#22090 = CARTESIAN_POINT ( 'NONE',  ( 0.7056313189692764443, 40.77721431583525913, 23.17255783460248963 ) ) ;
#22091 = CARTESIAN_POINT ( 'NONE',  ( 0.9741495583595166652, -5.208308905147834622, -42.59115242362814513 ) ) ;
#22092 = FACE_OUTER_BOUND ( 'NONE', #51832, .T. ) ;
#22093 = CARTESIAN_POINT ( 'NONE',  ( -6.017396004339687465, 2.458362590802789072, 18.68211039806564600 ) ) ;
#22094 = CARTESIAN_POINT ( 'NONE',  ( 5.895596859100789899, -4.666058297670421240, -19.56415301451173150 ) ) ;
#22095 = VERTEX_POINT ( 'NONE', #37949 ) ;
#22096 = CARTESIAN_POINT ( 'NONE',  ( -6.017396004339687465, 2.460690056888055643, -18.68180398134247255 ) ) ;
#22097 = CARTESIAN_POINT ( 'NONE',  ( 1.000110580585048092, -18.23585865330004552, 37.73421447372084714 ) ) ;
#22098 = CARTESIAN_POINT ( 'NONE',  ( 0.5806925824938499181, -38.96949031362449745, 26.08833430941674436 ) ) ;
#22099 = CARTESIAN_POINT ( 'NONE',  ( 0.5837800304671215690, -34.74999798522668470, -31.49087125193968717 ) ) ;
#22100 = EDGE_CURVE ( 'NONE', #54494, #24199, #6271, .T. ) ;
#22101 = CARTESIAN_POINT ( 'NONE',  ( 0.8551540677456715978, -46.51172240253112733, -11.51835730326528306 ) ) ;
#22102 = CARTESIAN_POINT ( 'NONE',  ( 0.9787464366903554369, -31.20010594550945981, 27.98012476525880032 ) ) ;
#22103 = SHAPE_DEFINITION_REPRESENTATION ( #60273, #44881 ) ;
#22104 = CARTESIAN_POINT ( 'NONE',  ( 5.896782393890504181, 17.94821721415871352, -9.076760749925545824 ) ) ;
#22105 = CARTESIAN_POINT ( 'NONE',  ( 0.9769922540276030354, -7.405947219671726423, 41.24904242361952811 ) ) ;
#22106 = CARTESIAN_POINT ( 'NONE',  ( 4.956653778116991482, 20.77844580450620526, -43.37017594958032873 ) ) ;
#22108 = ORIENTED_EDGE ( 'NONE', *, *, #56431, .T. ) ;
#22107 = CARTESIAN_POINT ( 'NONE',  ( 2.528190830796657629, -13.58807975251270861, 39.71924250023358383 ) ) ;
#22109 = VERTEX_POINT ( 'NONE', #14127 ) ;
#22110 = CARTESIAN_POINT ( 'NONE',  ( 2.643462169533600914, 46.73820883660206249, -11.09243630552484383 ) ) ;
#22111 = CARTESIAN_POINT ( 'NONE',  ( 0.5830081025819928708, -7.530652408779095808, 46.28737742279633238 ) ) ;
#22112 = LINE ( 'NONE', #41240, #49784 ) ;
#22113 = B_SPLINE_CURVE_WITH_KNOTS ( 'NONE', 3,
 ( #47065, #7896, #36743, #22622 ),
 .UNSPECIFIED., .F., .F.,
 ( 4, 4 ),
 ( 2.033478910116247305E-17, 0.004444306975806115896 ),
 .UNSPECIFIED. ) ;
#22114 = VERTEX_POINT ( 'NONE', #33228 ) ;
#22115 = CARTESIAN_POINT ( 'NONE',  ( 0.6254087463353902310, -38.58044986685671063, -28.73645667569937245 ) ) ;
#22116 = CARTESIAN_POINT ( 'NONE',  ( 0.7056555295713323739, -23.21854706865607554, 41.89804573586724956 ) ) ;
#22117 = CARTESIAN_POINT ( 'NONE',  ( 0.9762797500689124330, 29.49606728235512776, 29.77090526101756751 ) ) ;
#22118 = ORIENTED_EDGE ( 'NONE', *, *, #49394, .F. ) ;
#22119 = VERTEX_POINT ( 'NONE', #51072 ) ;
#22120 = CARTESIAN_POINT ( 'NONE',  ( 4.958415959904816539, 33.34645430971464464, -30.84182126257697121 ) ) ;
#22121 = CARTESIAN_POINT ( 'NONE',  ( 2.879087469061463178, 37.79288285606617848, 22.53441106865315646 ) ) ;
#22122 = B_SPLINE_CURVE_WITH_KNOTS ( 'NONE', 3,
 ( #29629, #6409, #54339, #25245 ),
 .UNSPECIFIED., .F., .F.,
 ( 4, 4 ),
 ( 4.670885906470169154E-18, 0.004566006591234646368 ),
 .UNSPECIFIED. ) ;
#22123 = CARTESIAN_POINT ( 'NONE',  ( 0.6031356219577719280, 41.70591683999472110, 23.97811961689702542 ) ) ;
#22124 = EDGE_LOOP ( 'NONE', ( #1169, #50108, #59833, #54220 ) ) ;
#22125 = ADVANCED_FACE ( 'NONE', ( #51691 ), #56069, .F. ) ;
#22126 = CARTESIAN_POINT ( 'NONE',  ( 0.9730545539215892381, 39.44597740938061037, 16.88610103448572630 ) ) ;
#22127 = ADVANCED_FACE ( 'NONE', ( #18198 ), #60463, .F. ) ;
#22128 = CARTESIAN_POINT ( 'NONE',  ( 0.1140933569871965536, -42.58338260172239131, -11.55878351208433230 ) ) ;
#22129 = VECTOR ( 'NONE', #24799, 1000.000000000000114 ) ;
#22130 = CARTESIAN_POINT ( 'NONE',  ( 0.2285344041767134737, 33.09684643513740099, -29.17361695683942102 ) ) ;
#22131 = LINE ( 'NONE', #61554, #6936 ) ;
#22132 = ORIENTED_EDGE ( 'NONE', *, *, #4432, .F. ) ;
#22133 = ADVANCED_FACE ( 'NONE', ( #36703 ), #19689, .F. ) ;
#22134 =( BOUNDED_SURFACE ( )  B_SPLINE_SURFACE ( 3, 1, ( 
 ( #1771, #59717 ),
 ( #7081, #16833 ),
 ( #12142, #31223 ),
 ( #53764, #6149 ) ),
 .UNSPECIFIED., .F., .F., .F. ) 
 B_SPLINE_SURFACE_WITH_KNOTS ( ( 4, 4 ),
 ( 2, 2 ),
 ( 0.000000000000000000, 1.000000000000000000 ),
 ( 0.000000000000000000, 1.000000000000000000 ),
 .UNSPECIFIED. ) 
 GEOMETRIC_REPRESENTATION_ITEM ( )  RATIONAL_B_SPLINE_SURFACE ( (
 ( 1.000000000000000000, 1.000000000000000000),
 ( 0.9732289882329797637, 0.9999525324661233672),
 ( 0.9732289882329797637, 0.9999525324661233672),
 ( 1.000000000000000000, 1.000000000000000000) ) ) 
 REPRESENTATION_ITEM ( '' )  SURFACE ( )  );
#22135 = EDGE_CURVE ( 'NONE', #58704, #355, #18579, .T. ) ;
#22136 = CARTESIAN_POINT ( 'NONE',  ( 0.6252788684277231779, 22.10253682748975734, -43.85113678073950894 ) ) ;
#22137 = CARTESIAN_POINT ( 'NONE',  ( 0.3676999524040323597, -32.25712563511804376, 30.09033780274075198 ) ) ;
#22138 = ORIENTED_EDGE ( 'NONE', *, *, #21708, .T. ) ;
#22139 = CARTESIAN_POINT ( 'NONE',  ( 0.9762797500689124330, -22.12212327108638377, 35.59405072711678741 ) ) ;
#22140 = EDGE_CURVE ( 'NONE', #9409, #6250, #29772, .T. ) ;
#22141 = CARTESIAN_POINT ( 'NONE',  ( 2.185380717157383135, 39.02616721911296338, -20.39063695064556114 ) ) ;
#22142 = CARTESIAN_POINT ( 'NONE',  ( 0.5326698147273788431, 0.000000000000000000, -41.88877248453276536 ) ) ;
#22143 = ORIENTED_EDGE ( 'NONE', *, *, #27421, .T. ) ;
#22144 = ORIENTED_EDGE ( 'NONE', *, *, #13183, .T. ) ;
#22145 = DIRECTION ( 'NONE',  ( -1.000000000000000000, -0.000000000000000000, -0.000000000000000000 ) ) ;
#22146 = CARTESIAN_POINT ( 'NONE',  ( 0.1155031312995260795, 39.82731631370493375, -18.99280147266069108 ) ) ;
#22147 = VERTEX_POINT ( 'NONE', #61084 ) ;
#22148 = FACE_OUTER_BOUND ( 'NONE', #48759, .T. ) ;
#22149 = EDGE_CURVE ( 'NONE', #35726, #3284, #56690, .T. ) ;
#22150 = B_SPLINE_CURVE_WITH_KNOTS ( 'NONE', 3,
 ( #11493, #2688, #22120, #17124 ),
 .UNSPECIFIED., .F., .F.,
 ( 4, 4 ),
 ( 0.000000000000000000, 0.005004948556313797495 ),
 .UNSPECIFIED. ) ;
#22151 = ORIENTED_EDGE ( 'NONE', *, *, #22530, .F. ) ;
#22152 = CARTESIAN_POINT ( 'NONE',  ( 5.981074661064941900, -12.48781255314301397, 16.28853686865577544 ) ) ;
#22153 = VERTEX_POINT ( 'NONE', #38550 ) ;
#22154 = DIRECTION ( 'NONE',  ( -1.000000000000000000, -0.000000000000000000, -0.000000000000000000 ) ) ;
#22155 = CARTESIAN_POINT ( 'NONE',  ( -2.601141883200662974, 3.756714151559825687, 14.44584806277771705 ) ) ;
#22156 = EDGE_CURVE ( 'NONE', #52389, #34292, #15322, .T. ) ;
#22157 =( BOUNDED_SURFACE ( )  B_SPLINE_SURFACE ( 3, 1, ( 
 ( #33582, #37994 ),
 ( #28546, #18872 ),
 ( #13866, #8832 ),
 ( #57649, #47987 ) ),
 .UNSPECIFIED., .F., .F., .F. ) 
 B_SPLINE_SURFACE_WITH_KNOTS ( ( 4, 4 ),
 ( 2, 2 ),
 ( 0.000000000000000000, 1.000000000000000000 ),
 ( 0.000000000000000000, 1.000000000000000000 ),
 .UNSPECIFIED. ) 
 GEOMETRIC_REPRESENTATION_ITEM ( )  RATIONAL_B_SPLINE_SURFACE ( (
 ( 1.000000000000000000, 1.000000000000000000),
 ( 0.9953040768229013402, 0.8617119497784988535),
 ( 0.9953040768229013402, 0.8617119497784988535),
 ( 1.000000000000000000, 1.000000000000000000) ) ) 
 REPRESENTATION_ITEM ( '' )  SURFACE ( )  );
#22158 = CARTESIAN_POINT ( 'NONE',  ( 0.1101816497532063510, -26.14462713083321077, 34.29544870207467966 ) ) ;
#22159 = ORIENTED_EDGE ( 'NONE', *, *, #40341, .T. ) ;
#22160 = CARTESIAN_POINT ( 'NONE',  ( 0.1149546198390366814, 43.25733823727443195, 8.703404715929053737 ) ) ;
#22161 = CARTESIAN_POINT ( 'NONE',  ( 1.154321713695930507, -11.90271797554042976, 41.23280394713391672 ) ) ;
#22162 =( BOUNDED_SURFACE ( )  B_SPLINE_SURFACE ( 3, 1, ( 
 ( #9322, #18744 ),
 ( #24356, #19358 ),
 ( #33152, #19985 ),
 ( #19063, #33777 ) ),
 .UNSPECIFIED., .F., .F., .F. ) 
 B_SPLINE_SURFACE_WITH_KNOTS ( ( 4, 4 ),
 ( 2, 2 ),
 ( 0.000000000000000000, 1.000000000000000000 ),
 ( 0.000000000000000000, 1.000000000000000000 ),
 .UNSPECIFIED. ) 
 GEOMETRIC_REPRESENTATION_ITEM ( )  RATIONAL_B_SPLINE_SURFACE ( (
 ( 1.000000000000000000, 1.000000000000000000),
 ( 0.7211978278499968642, 0.9934217856018975334),
 ( 0.7211978278499968642, 0.9934217856018975334),
 ( 1.000000000000000000, 1.000000000000000000) ) ) 
 REPRESENTATION_ITEM ( '' )  SURFACE ( )  );
#22163 = CARTESIAN_POINT ( 'NONE',  ( 4.975801465491694664, 47.10002938642141856, -8.787181743659651545 ) ) ;
#22164 = EDGE_LOOP ( 'NONE', ( #20426, #31622, #50744, #39972 ) ) ;
#22165 = ORIENTED_EDGE ( 'NONE', *, *, #25591, .F. ) ;
#22166 = CARTESIAN_POINT ( 'NONE',  ( 0.6253024248130467644, -38.93995934748834031, -29.91861951082636040 ) ) ;
#22167 = CARTESIAN_POINT ( 'NONE',  ( 0.6001305935487315502, -44.64600790884068715, 17.92615948558460559 ) ) ;
#22168 = CARTESIAN_POINT ( 'NONE',  ( 0.9790320750461891652, 38.61669752663120647, -16.28151727201333188 ) ) ;
#22169 = CARTESIAN_POINT ( 'NONE',  ( 3.783278058412223199, 41.98530666033914827, 9.462251542473966381 ) ) ;
#22170 = CARTESIAN_POINT ( 'NONE',  ( 4.956653778116827169, 32.11725092155053574, 35.79382859084104496 ) ) ;
#22171 = VERTEX_POINT ( 'NONE', #39172 ) ;
#22172 = CARTESIAN_POINT ( 'NONE',  ( 5.896782393890504181, 20.06834277495334362, -1.337050913387380691 ) ) ;
#22173 = CARTESIAN_POINT ( 'NONE',  ( 0.8557997880470690211, -46.50333260518550560, -11.51622788066506686 ) ) ;
#22174 = ORIENTED_EDGE ( 'NONE', *, *, #24415, .T. ) ;
#22175 = CARTESIAN_POINT ( 'NONE',  ( 0.9752132459055847802, -30.17566824627268218, 30.50512806189400550 ) ) ;
#22176 = CARTESIAN_POINT ( 'NONE',  ( 0.9968887458511644928, 42.90440775986218114, 0.6574002966409985271 ) ) ;
#22177 = CARTESIAN_POINT ( 'NONE',  ( 0.7764146366350260786, -42.25777079059512431, -20.35488347986028046 ) ) ;
#22178 = CARTESIAN_POINT ( 'NONE',  ( 0.1119899015040013573, -38.16786807883124055, -22.13989960477330499 ) ) ;
#22179 = EDGE_CURVE ( 'NONE', #2691, #5234, #33851, .T. ) ;
#22180 = CARTESIAN_POINT ( 'NONE',  ( 0.5807400328401637335, 23.47602859900714023, 41.75144119563894662 ) ) ;
#22181 = CARTESIAN_POINT ( 'NONE',  ( 3.661921753702003013, -45.68403764746661722, 11.20713290984310895 ) ) ;
#22182 = CIRCLE ( 'NONE', #33190, 48.91267123290010943 ) ;
#22183 = FACE_OUTER_BOUND ( 'NONE', #17672, .T. ) ;
#22184 =( LENGTH_UNIT ( ) NAMED_UNIT ( * ) SI_UNIT ( .MILLI., .METRE. ) );
#22185 = CARTESIAN_POINT ( 'NONE',  ( 0.5824936645240090805, 10.51679990701790679, 45.70158748617006239 ) ) ;
#22186 = CIRCLE ( 'NONE', #145, 0.2800000000000024691 ) ;
#22187 = EDGE_CURVE ( 'NONE', #52958, #16350, #58284, .T. ) ;
#22188 = CARTESIAN_POINT ( 'NONE',  ( 0.9754642270333679921, -39.70914670678644853, 16.25787253057921689 ) ) ;
#22189 = CARTESIAN_POINT ( 'NONE',  ( 1.231276596079887931, -39.86997064245532840, -12.94844438486017779 ) ) ;
#22190 = CARTESIAN_POINT ( 'NONE',  ( 0.6008123274975391004, 23.09929101554148900, -43.33563551787122492 ) ) ;
#22191 = CARTESIAN_POINT ( 'NONE',  ( 5.901764892641288895, 45.40663509823448152, 18.33654701669480147 ) ) ;
#22192 = CARTESIAN_POINT ( 'NONE',  ( 4.956653778116966613, 0.000000000000000000, 0.000000000000000000 ) ) ;
#22193 = LINE ( 'NONE', #14574, #43255 ) ;
#22194 = PLANE ( 'NONE',  #50757 ) ;
#22195 = PRODUCT_DEFINITION ( 'UNKNOWN', '', #7877, #1597 ) ;
#22196 = DIRECTION ( 'NONE',  ( 0.09722883295013594329, -0.7930735330831515384, 0.6013159944373356325 ) ) ;
#22197 = CARTESIAN_POINT ( 'NONE',  ( 0.9754292580325143458, -41.18084053248014698, 7.775978391330924389 ) ) ;
#22198 = ORIENTED_EDGE ( 'NONE', *, *, #43085, .T. ) ;
#22199 = B_SPLINE_CURVE_WITH_KNOTS ( 'NONE', 3,
 ( #37515, #14628, #5185, #19023, #57184, #38140 ),
 .UNSPECIFIED., .F., .F.,
 ( 4, 2, 4 ),
 ( 2.279404534222591916E-18, 0.0002447193893791696538, 0.0004894387787583370309 ),
 .UNSPECIFIED. ) ;
#22200 = CARTESIAN_POINT ( 'NONE',  ( 2.009741617377216460, -32.57420985222115206, -29.63823426127985528 ) ) ;
#22201 = CARTESIAN_POINT ( 'NONE',  ( 0.9736507210033057413, -39.46762617149622798, -16.83559693395306311 ) ) ;
#22202 = CARTESIAN_POINT ( 'NONE',  ( 4.956445790443988031, 0.000000000000000000, 0.000000000000000000 ) ) ;
#22203 = ORIENTED_EDGE ( 'NONE', *, *, #24470, .T. ) ;
#22204 = EDGE_CURVE ( 'NONE', #23496, #47332, #53872, .T. ) ;
#22205 = CARTESIAN_POINT ( 'NONE',  ( 1.479689385636123067, -40.38744186525652680, 17.61926175661785976 ) ) ;
#22206 = FACE_OUTER_BOUND ( 'NONE', #33124, .T. ) ;
#22207 = B_SPLINE_CURVE_WITH_KNOTS ( 'NONE', 3,
 ( #27270, #12882, #17884, #55758, #32596, #56378, #47304, #42316, #37008, #4658, #42618, #51677, #18809, #56682, #13807, #27573 ),
 .UNSPECIFIED., .F., .F.,
 ( 4, 3, 3, 3, 3, 4 ),
 ( 1.250973872328959318E-17, 0.0002732102107931902706, 0.0004098135523333833229, 0.0005464168938825049969, 0.0008195847345945408416, 0.001092771384553101579 ),
 .UNSPECIFIED. ) ;
#22208 = EDGE_CURVE ( 'NONE', #58926, #54112, #53834, .T. ) ;
#22209 = CARTESIAN_POINT ( 'NONE',  ( 5.910764540655178756, 16.59011036809707917, 11.36967354164229604 ) ) ;
#22210 = ORIENTED_EDGE ( 'NONE', *, *, #561, .T. ) ;
#22211 = CARTESIAN_POINT ( 'NONE',  ( 4.999999999999997335, -2.784000523420839360E-13, 80.00000000000001421 ) ) ;
#22212 = VERTEX_POINT ( 'NONE', #10030 ) ;
#22213 = EDGE_CURVE ( 'NONE', #21596, #1942, #31479, .T. ) ;
#22214 = CARTESIAN_POINT ( 'NONE',  ( -6.057079549204054558, 12.01317374117813230, 15.05041154799451242 ) ) ;
#22215 = CARTESIAN_POINT ( 'NONE',  ( -1.660531772554312280, 3.660093687634848436, -5.600000000000003197 ) ) ;
#22216 = ORIENTED_EDGE ( 'NONE', *, *, #42055, .T. ) ;
#22217 = CARTESIAN_POINT ( 'NONE',  ( 2.528190830796659405, -30.30926884989141712, -29.04483358427122752 ) ) ;
#22218 = EDGE_CURVE ( 'NONE', #5679, #36885, #44271, .T. ) ;
#22219 = CARTESIAN_POINT ( 'NONE',  ( 2.301430502907644282, 34.86297247504474939, -33.04218380901183139 ) ) ;
#22220 = ORIENTED_EDGE ( 'NONE', *, *, #25693, .T. ) ;
#22221 = CARTESIAN_POINT ( 'NONE',  ( 4.956445790443988031, 0.000000000000000000, 0.000000000000000000 ) ) ;
#22222 = CARTESIAN_POINT ( 'NONE',  ( 4.694002226626920127, 1.116723307533209475, -45.57452907601510361 ) ) ;
#22223 = AXIS2_PLACEMENT_3D ( 'NONE', #32353, #57351, #60832 ) ;
#22224 = ORIENTED_EDGE ( 'NONE', *, *, #61957, .T. ) ;
#22226 = B_SPLINE_CURVE_WITH_KNOTS ( 'NONE', 3,
 ( #53396, #53094, #28369, #19607, #38728, #787 ),
 .UNSPECIFIED., .F., .F.,
 ( 4, 2, 4 ),
 ( 1.738108305489988542E-18, 0.0002291966416970804066, 0.0004583932833941590785 ),
 .UNSPECIFIED. ) ;
#22225 = CARTESIAN_POINT ( 'NONE',  ( 3.782542959838393504, 40.96636395946045184, -9.433709627584986990 ) ) ;
#22227 = ORIENTED_EDGE ( 'NONE', *, *, #30712, .T. ) ;
#22228 = CARTESIAN_POINT ( 'NONE',  ( 0.5804410086790514622, -38.35366574782019455, 26.99103880105172237 ) ) ;
#22229 = AXIS2_PLACEMENT_3D ( 'NONE', #39714, #21196, #26505 ) ;
#22230 = ORIENTED_EDGE ( 'NONE', *, *, #24282, .T. ) ;
#22231 = EDGE_LOOP ( 'NONE', ( #43837, #27157, #51868, #8607 ) ) ;
#22232 = CARTESIAN_POINT ( 'NONE',  ( 0.8557997880470697982, 11.51622788066522851, -46.50333260518546297 ) ) ;
#22233 = DIRECTION ( 'NONE',  ( 0.09722883295013598492, -0.4097642837406538785, 0.9069949205004753656 ) ) ;
#22234 = LINE ( 'NONE', #36044, #41508 ) ;
#22235 = CARTESIAN_POINT ( 'NONE',  ( 3.240649175237396484, 42.29049807985159504, -12.11522552640768779 ) ) ;
#22236 = CARTESIAN_POINT ( 'NONE',  ( 6.566016632731837888, -8.528786624275497275, -2.999999999999986677 ) ) ;
#22237 = ORIENTED_EDGE ( 'NONE', *, *, #51749, .F. ) ;
#22238 = CARTESIAN_POINT ( 'NONE',  ( -6.078075953587585900, -1.854308114363064419, 19.16655200248973401 ) ) ;
#22239 = FACE_OUTER_BOUND ( 'NONE', #8866, .T. ) ;
#22240 = CARTESIAN_POINT ( 'NONE',  ( 4.956653778116992370, 3.690426056930664611, -47.94889704119048446 ) ) ;
#22241 = VERTEX_POINT ( 'NONE', #20356 ) ;
#22242 =( BOUNDED_SURFACE ( )  B_SPLINE_SURFACE ( 3, 1, ( 
 ( #39399, #38787 ),
 ( #29052, #43804 ),
 ( #24979, #48772 ),
 ( #14974, #29974 ) ),
 .UNSPECIFIED., .F., .F., .F. ) 
 B_SPLINE_SURFACE_WITH_KNOTS ( ( 4, 4 ),
 ( 2, 2 ),
 ( 0.000000000000000000, 1.000000000000000000 ),
 ( 0.000000000000000000, 1.000000000000000000 ),
 .UNSPECIFIED. ) 
 GEOMETRIC_REPRESENTATION_ITEM ( )  RATIONAL_B_SPLINE_SURFACE ( (
 ( 1.000000000000000000, 1.000000000000000000),
 ( 0.9729067724841187204, 0.9999501103223794596),
 ( 0.9729067724841187204, 0.9999501103223794596),
 ( 1.000000000000000000, 1.000000000000000000) ) ) 
 REPRESENTATION_ITEM ( '' )  SURFACE ( )  );
#22243 = ORIENTED_EDGE ( 'NONE', *, *, #7051, .F. ) ;
#22244 = CARTESIAN_POINT ( 'NONE',  ( 0.7044674535452954967, 44.60554499456301158, -20.54624244354476659 ) ) ;
#22245 = CARTESIAN_POINT ( 'NONE',  ( -99.49999999999975842, -9.184850993605117179E-15, 3.081487911019577365E-29 ) ) ;
#22246 = CARTESIAN_POINT ( 'NONE',  ( 0.5837799406558231707, -44.27132707568020464, 15.46910302943734372 ) ) ;
#22247 = ORIENTED_EDGE ( 'NONE', *, *, #24762, .T. ) ;
#22248 = CARTESIAN_POINT ( 'NONE',  ( 0.1129192098497455998, 14.78321943369591196, 41.57412910645692961 ) ) ;
#22249 = CARTESIAN_POINT ( 'NONE',  ( -2.569797478183790229, -11.87678401312200371, 8.547745408040595905 ) ) ;
#22250 = B_SPLINE_CURVE_WITH_KNOTS ( 'NONE', 3,
 ( #45006, #49667, #46230, #59365, #54972, #6723 ),
 .UNSPECIFIED., .F., .F.,
 ( 4, 2, 4 ),
 ( 0.006456566858647394894, 0.007625406818786665576, 0.008794246778925936259 ),
 .UNSPECIFIED. ) ;
#22251 = VERTEX_POINT ( 'NONE', #47939 ) ;
#22252 = CARTESIAN_POINT ( 'NONE',  ( 4.967162193818130511, 40.93989340068610261, 13.42934394584178648 ) ) ;
#22253 = ORIENTED_EDGE ( 'NONE', *, *, #57953, .T. ) ;
#22254 = B_SPLINE_CURVE_WITH_KNOTS ( 'NONE', 3,
 ( #15537, #5785, #34641, #1102, #44074, #24937, #53110, #5484, #20240, #24622, #39354, #43758, #39053, #58110, #15231, #58413 ),
 .UNSPECIFIED., .F., .F.,
 ( 4, 3, 3, 3, 3, 4 ),
 ( 1.250973872328959318E-17, 0.0002724568934985518065, 0.0004086836638483732080, 0.0005449104342063575135, 0.0008173270854453600597, 0.001089761613562685756 ),
 .UNSPECIFIED. ) ;
#22255 = CARTESIAN_POINT ( 'NONE',  ( 4.975610109902397937, 30.94437158899580353, 37.88001153774800400 ) ) ;
#22256 = CARTESIAN_POINT ( 'NONE',  ( 0.9749527285493297946, -34.21468599366731667, 25.89384247702557929 ) ) ;
#22257 = CARTESIAN_POINT ( 'NONE',  ( 2.879087469061463178, -43.38468303210888166, 7.339683575388114001 ) ) ;
#22258 = EDGE_CURVE ( 'NONE', #26853, #7974, #23277, .T. ) ;
#22259 = ORIENTED_EDGE ( 'NONE', *, *, #2554, .F. ) ;
#22260 = CARTESIAN_POINT ( 'NONE',  ( 5.895596859100789899, 19.00119700155561020, -6.594141014609973261 ) ) ;
#22261 = CARTESIAN_POINT ( 'NONE',  ( 0.8554163680231816613, -18.91615390926536477, 42.93465493506153052 ) ) ;
#22262 = DIRECTION ( 'NONE',  ( -0.07439287786467650709, 0.2453289374370270781, -0.9665813013808153276 ) ) ;
#22263 = CARTESIAN_POINT ( 'NONE',  ( 0.1102847568649952675, -16.58813073670681604, -39.80641842112238749 ) ) ;
#22264 = DIRECTION ( 'NONE',  ( 0.09835009131224552170, -0.9855991218957039779, 0.1375559175655126365 ) ) ;
#22265 = CARTESIAN_POINT ( 'NONE',  ( 0.5848930533535030563, -45.92005787004959672, 9.519525597363298175 ) ) ;
#22266 = DIRECTION ( 'NONE',  ( 1.000000000000000000, 0.000000000000000000, 0.000000000000000000 ) ) ;
#22267 = CARTESIAN_POINT ( 'NONE',  ( 0.6029442701453591180, -49.10740919470779176, 0.08710534889204829545 ) ) ;
#22268 = VECTOR ( 'NONE', #8451, 1000.000000000000227 ) ;
#22269 = CARTESIAN_POINT ( 'NONE',  ( 0.5980894510889448457, 28.72954109785552745, 38.59343625445455928 ) ) ;
#22270 = CIRCLE ( 'NONE', #51267, 47.09074272231896430 ) ;
#22271 = DIRECTION ( 'NONE',  ( -0.1011922191286467598, -0.2088217057275243982, -0.9727042870291398025 ) ) ;
#22272 = CARTESIAN_POINT ( 'NONE',  ( 5.901764892641307547, 39.27045567455346742, -29.25444886769549413 ) ) ;
#22273 = VERTEX_POINT ( 'NONE', #602 ) ;
#22274 = CARTESIAN_POINT ( 'NONE',  ( -2.569797478183783568, -0.4487456364277818133, -14.62602397812941213 ) ) ;
#22275 = CARTESIAN_POINT ( 'NONE',  ( 5.960221823109900008, -18.96526051813986413, 7.849768660536222242 ) ) ;
#22276 = FACE_OUTER_BOUND ( 'NONE', #3124, .T. ) ;
#22277 = CARTESIAN_POINT ( 'NONE',  ( 0.5809828226811617480, 44.45562576850627323, -17.82437196699632054 ) ) ;
#22278 = ORIENTED_EDGE ( 'NONE', *, *, #7952, .F. ) ;
#22279 = CARTESIAN_POINT ( 'NONE',  ( 0.6000166863083090663, -13.47152005829862098, 47.22649287240490423 ) ) ;
#22280 = CARTESIAN_POINT ( 'NONE',  ( 0.9789889208857702751, -41.82137578286608459, -2.703225049948740910 ) ) ;
#22281 = EDGE_CURVE ( 'NONE', #28495, #35248, #33065, .T. ) ;
#22282 = VERTEX_POINT ( 'NONE', #15047 ) ;
#22283 = CARTESIAN_POINT ( 'NONE',  ( -5.272380000000000067, 1.883773750090843600E-15, -15.38217999999999996 ) ) ;
#22284 = CARTESIAN_POINT ( 'NONE',  ( 0.9752570700956806338, -41.38610171411350080, -11.32817567195955810 ) ) ;
#22285 = EDGE_CURVE ( 'NONE', #1532, #49867, #52440, .T. ) ;
#22286 = CARTESIAN_POINT ( 'NONE',  ( 3.221118495291109163, -10.69297281925443244, 42.66640073815035095 ) ) ;
#22287 = ORIENTED_EDGE ( 'NONE', *, *, #53780, .T. ) ;
#22288 = CARTESIAN_POINT ( 'NONE',  ( 0.5782707292762442330, 5.414380361654997031, -46.58777563918396680 ) ) ;
#22289 = ORIENTED_EDGE ( 'NONE', *, *, #49945, .T. ) ;
#22290 = EDGE_CURVE ( 'NONE', #35128, #22938, #34493, .T. ) ;
#22291 = ORIENTED_EDGE ( 'NONE', *, *, #59898, .F. ) ;
#22292 = CARTESIAN_POINT ( 'NONE',  ( 3.680974057930773924, 42.44218549341211144, -22.36814223828923787 ) ) ;
#22293 = VERTEX_POINT ( 'NONE', #35084 ) ;
#22294 = CARTESIAN_POINT ( 'NONE',  ( 5.958863334805807099, -0.001220270596028860026, -20.52565293643016275 ) ) ;
#22295 = PRODUCT_DEFINITION_SHAPE ( 'NONE', 'NONE',  #61986 ) ;
#22296 = ORIENTED_EDGE ( 'NONE', *, *, #47556, .F. ) ;
#22297 = CARTESIAN_POINT ( 'NONE',  ( 4.975610109902397937, 0.9924324126403755164, 48.90260202733708894 ) ) ;
#22298 = CARTESIAN_POINT ( 'NONE',  ( 1.296416391601052487, -0.3014346417254653576, 44.07058555582086257 ) ) ;
#22299 = VERTEX_POINT ( 'NONE', #40724 ) ;
#22300 = CARTESIAN_POINT ( 'NONE',  ( 0.1152339509894530906, 15.44841342848934040, 41.33145549091772608 ) ) ;
#22301 = EDGE_CURVE ( 'NONE', #38660, #27238, #36066, .T. ) ;
#22302 = CARTESIAN_POINT ( 'NONE',  ( 50.32441585594579436, 12.21587082446438011, -2.649999999999992806 ) ) ;
#22303 = CARTESIAN_POINT ( 'NONE',  ( 1.657374760986086493, -37.76384079651226955, 22.68882490451896317 ) ) ;
#22304 = FACE_OUTER_BOUND ( 'NONE', #22810, .T. ) ;
#22305 = ORIENTED_EDGE ( 'NONE', *, *, #32821, .F. ) ;
#22306 = DIRECTION ( 'NONE',  ( 0.000000000000000000, 1.000000000000000000, 0.000000000000000000 ) ) ;
#22307 = EDGE_CURVE ( 'NONE', #32810, #35884, #9855, .T. ) ;
#22308 = ORIENTED_EDGE ( 'NONE', *, *, #30909, .F. ) ;
#22309 = AXIS2_PLACEMENT_3D ( 'NONE', #57527, #52853, #5527 ) ;
#22310 = CARTESIAN_POINT ( 'NONE',  ( 0.9756008150404595902, -42.90824081423206593, 0.1421465480001363191 ) ) ;
#22311 = ORIENTED_EDGE ( 'NONE', *, *, #30602, .F. ) ;
#22312 = CARTESIAN_POINT ( 'NONE',  ( 4.956445790443998689, 1.033212179477464909, 47.07940656732852602 ) ) ;
#22313 = CARTESIAN_POINT ( 'NONE',  ( 2.879087469061463178, 13.55971874537538824, -41.85971457534910911 ) ) ;
#22314 = ORIENTED_EDGE ( 'NONE', *, *, #20936, .F. ) ;
#22315 = CARTESIAN_POINT ( 'NONE',  ( 0.5827359174754822568, -46.16863801597755668, -12.74690115177656224 ) ) ;
#22316 = CARTESIAN_POINT ( 'NONE',  ( 4.956445790444002242, -36.61936279692601204, 29.60676136436992678 ) ) ;
#22317 = CARTESIAN_POINT ( 'NONE',  ( 4.999999999999983125, 80.00000000000001421, -3.562970397116383044E-32 ) ) ;
#22318 = ORIENTED_EDGE ( 'NONE', *, *, #7150, .T. ) ;
#22319 = ORIENTED_EDGE ( 'NONE', *, *, #30946, .F. ) ;
#22320 = CARTESIAN_POINT ( 'NONE',  ( 0.3622758884714600280, 15.73321244754796666, 40.13994584881788086 ) ) ;
#22321 = CARTESIAN_POINT ( 'NONE',  ( 5.974727161628369032, 18.96851388233658398, -7.840226266082345852 ) ) ;
#22322 = CARTESIAN_POINT ( 'NONE',  ( 0.6001305935487422083, 41.92422178329137239, 23.60027211631843969 ) ) ;
#22324 = B_SPLINE_CURVE_WITH_KNOTS ( 'NONE', 3,
 ( #46020, #8685, #27804, #3060 ),
 .UNSPECIFIED., .F., .F.,
 ( 4, 4 ),
 ( 3.469446951953613804E-18, 0.005004948556313820046 ),
 .UNSPECIFIED. ) ;
#22323 = CARTESIAN_POINT ( 'NONE',  ( 0.5804410086790514622, 45.08525424748444976, -12.91664435118819121 ) ) ;
#22325 = EDGE_CURVE ( 'NONE', #53301, #6381, #55083, .T. ) ;
#22326 = CARTESIAN_POINT ( 'NONE',  ( 0.9762797500689124330, 41.90547441298052433, 0.5059638413352746111 ) ) ;
#22327 = CARTESIAN_POINT ( 'NONE',  ( 5.331200000000000827, 0.000000000000000000, 0.000000000000000000 ) ) ;
#22328 = CARTESIAN_POINT ( 'NONE',  ( 5.283180000000047727, 15.43999999999999240, 0.000000000000000000 ) ) ;
#22329 = DIRECTION ( 'NONE',  ( -1.000000000000000000, -0.000000000000000000, -0.000000000000000000 ) ) ;
#22330 = CARTESIAN_POINT ( 'NONE',  ( 0.9780303403264750672, 33.08964503960959291, 25.71798990099589943 ) ) ;
#22331 = CARTESIAN_POINT ( 'NONE',  ( 4.962356264823596597, 39.89814050050772920, 13.39305724859313429 ) ) ;
#22332 = LINE ( 'NONE', #56751, #14147 ) ;
#22333 = CARTESIAN_POINT ( 'NONE',  ( 0.5837800005270554760, -13.89417140152258234, -44.79048179811078967 ) ) ;
#22334 = CARTESIAN_POINT ( 'NONE',  ( 4.967162193818130511, 3.259922920618364639, -42.96271701169381885 ) ) ;
#22335 = CARTESIAN_POINT ( 'NONE',  ( 4.549368137175248350, -32.41327393324159800, 28.14399996863441800 ) ) ;
#22336 = B_SPLINE_CURVE_WITH_KNOTS ( 'NONE', 3,
 ( #16486, #25884, #53144, #10251 ),
 .UNSPECIFIED., .F., .F.,
 ( 4, 4 ),
 ( 0.000000000000000000, 0.004446298630425058948 ),
 .UNSPECIFIED. ) ;
#22337 = CARTESIAN_POINT ( 'NONE',  ( 0.6029443199889047422, 16.96000599311128454, 46.08574441807392930 ) ) ;
#22338 = CARTESIAN_POINT ( 'NONE',  ( 0.6008122571543325074, -47.38919495537865600, 12.87706301710256440 ) ) ;
#22340 = ORIENTED_EDGE ( 'NONE', *, *, #44998, .T. ) ;
#22339 = CARTESIAN_POINT ( 'NONE',  ( 0.5848930533535030563, -41.93775812029553407, -20.98803292905613205 ) ) ;
#22341 = VERTEX_POINT ( 'NONE', #31290 ) ;
#22342 = FACE_OUTER_BOUND ( 'NONE', #61542, .T. ) ;
#22343 = CARTESIAN_POINT ( 'NONE',  ( 4.975801465491695552, 26.14269827151680659, -40.15204426031507268 ) ) ;
#22344 = CARTESIAN_POINT ( 'NONE',  ( 2.643462169533613793, 34.93025802711680683, 32.97543604874687873 ) ) ;
#22345 = ORIENTED_EDGE ( 'NONE', *, *, #25432, .T. ) ;
#22346 = ORIENTED_EDGE ( 'NONE', *, *, #55566, .F. ) ;
#22347 = CARTESIAN_POINT ( 'NONE',  ( 4.956445790443988031, 0.000000000000000000, 0.000000000000000000 ) ) ;
#22348 = DIRECTION ( 'NONE',  ( 0.000000000000000000, 0.000000000000000000, 1.000000000000000000 ) ) ;
#22349 = CIRCLE ( 'NONE', #16354, 43.92652462719577500 ) ;
#22350 = ORIENTED_EDGE ( 'NONE', *, *, #55081, .T. ) ;
#22351 = ORIENTED_EDGE ( 'NONE', *, *, #61664, .T. ) ;
#22352 =( BOUNDED_SURFACE ( )  B_SPLINE_SURFACE ( 3, 1, ( 
 ( #47628, #28818 ),
 ( #33853, #43562 ),
 ( #14432, #29431 ),
 ( #48248, #53231 ) ),
 .UNSPECIFIED., .F., .F., .F. ) 
 B_SPLINE_SURFACE_WITH_KNOTS ( ( 4, 4 ),
 ( 2, 2 ),
 ( 0.000000000000000000, 1.000000000000000000 ),
 ( 0.000000000000000000, 1.000000000000000000 ),
 .UNSPECIFIED. ) 
 GEOMETRIC_REPRESENTATION_ITEM ( )  RATIONAL_B_SPLINE_SURFACE ( (
 ( 1.000000000000000000, 1.000000000000000000),
 ( 0.7211978278499968642, 0.9934217856018975334),
 ( 0.7211978278499968642, 0.9934217856018975334),
 ( 1.000000000000000000, 1.000000000000000000) ) ) 
 REPRESENTATION_ITEM ( '' )  SURFACE ( )  );
#22353 = CARTESIAN_POINT ( 'NONE',  ( 1.000433927950262536, 19.56092357721248831, -37.06465899558902777 ) ) ;
#22354 = EDGE_CURVE ( 'NONE', #2002, #58167, #15078, .T. ) ;
#22355 = FACE_OUTER_BOUND ( 'NONE', #3018, .T. ) ;
#22356 = CARTESIAN_POINT ( 'NONE',  ( 0.1129192098497447394, 39.96249028893947752, 18.70698152272492365 ) ) ;
#22357 = ADVANCED_FACE ( 'NONE', ( #2769 ), #42560, .F. ) ;
#22358 = ORIENTED_EDGE ( 'NONE', *, *, #47810, .F. ) ;
#22359 = CARTESIAN_POINT ( 'NONE',  ( 0.2279481005628783974, -17.16174681686966963, -40.64453140665511910 ) ) ;
#22360 = VECTOR ( 'NONE', #35025, 1000.000000000000227 ) ;
#22361 = CARTESIAN_POINT ( 'NONE',  ( 0.5980271706414734822, -42.44486003424520959, 24.70795619866194315 ) ) ;
#22362 = EDGE_CURVE ( 'NONE', #56380, #49641, #54645, .T. ) ;
#22363 = CARTESIAN_POINT ( 'NONE',  ( 0.1073791018717578927, 21.14095454447508615, 37.58707531572213156 ) ) ;
#22364 = ORIENTED_EDGE ( 'NONE', *, *, #32537, .F. ) ;
#22365 = VERTEX_POINT ( 'NONE', #30660 ) ;
#22366 = CARTESIAN_POINT ( 'NONE',  ( 3.661921753701995019, 47.00091123480373057, -1.882941032570424111 ) ) ;
#22367 = ORIENTED_EDGE ( 'NONE', *, *, #21599, .T. ) ;
#22368 = CARTESIAN_POINT ( 'NONE',  ( 0.5837374860065644988, 44.18034382476647437, -18.49670552082908159 ) ) ;
#22369 = DIRECTION ( 'NONE',  ( 0.000000000000000000, 0.000000000000000000, 1.000000000000000000 ) ) ;
#22370 = CARTESIAN_POINT ( 'NONE',  ( 4.833616638992208614, 30.15290813935903103, -35.06988470649537959 ) ) ;
#22371 = CARTESIAN_POINT ( 'NONE',  ( 0.6252788684277222897, -30.07747058975758492, 38.81739422083782642 ) ) ;
#22372 = CARTESIAN_POINT ( 'NONE',  ( -69.95594261585601714, 0.000000000000000000, 0.000000000000000000 ) ) ;
#22373 = EDGE_CURVE ( 'NONE', #35226, #61413, #56871, .T. ) ;
#22374 = B_SPLINE_CURVE_WITH_KNOTS ( 'NONE', 3,
 ( #40683, #59750, #25316, #54731 ),
 .UNSPECIFIED., .F., .F.,
 ( 4, 4 ),
 ( 0.000000000000000000, 0.004442905043737214836 ),
 .UNSPECIFIED. ) ;
#22375 = EDGE_LOOP ( 'NONE', ( #34370, #38667, #35614, #57003 ) ) ;
#22376 = DIRECTION ( 'NONE',  ( -0.000000000000000000, 0.000000000000000000, -1.000000000000000000 ) ) ;
#22377 = CARTESIAN_POINT ( 'NONE',  ( 2.648799415243696664, 6.085982952329662687, -48.65673925360751895 ) ) ;
#22378 = CARTESIAN_POINT ( 'NONE',  ( 0.6845945791218034371, 42.84081778543538377, 19.10682737110132123 ) ) ;
#22379 = ORIENTED_EDGE ( 'NONE', *, *, #51400, .F. ) ;
#22380 = CARTESIAN_POINT ( 'NONE',  ( 1.157643937452371041, -35.01838089395619846, -23.03725839071476145 ) ) ;
#22381 = CARTESIAN_POINT ( 'NONE',  ( 2.643462169533613793, -34.93025802711703420, -32.97543604874663714 ) ) ;
#22382 = LINE ( 'NONE', #13615, #31659 ) ;
#22383 = CARTESIAN_POINT ( 'NONE',  ( 0.8554163680231738898, 46.61139063278412209, -5.346376005279195986 ) ) ;
#22384 = B_SPLINE_CURVE_WITH_KNOTS ( 'NONE', 3,
 ( #52361, #9454, #28563, #19192, #43006, #24486, #38929, #43624, #58282, #48298, #34832, #5962, #43942, #14488, #53286, #980, #19493, #9769, #667 ),
 .UNSPECIFIED., .F., .F.,
 ( 4, 3, 3, 3, 3, 3, 4 ),
 ( 0.000000000000000000, 0.0002612768053151725764, 0.0003919133833142917386, 0.0005225499612322563082, 0.0006531865391693363922, 0.0008112755173415148700, 0.0009693688056799733320 ),
 .UNSPECIFIED. ) ;
#22385 = EDGE_LOOP ( 'NONE', ( #60194, #44417, #38280, #53803 ) ) ;
#22386 = CARTESIAN_POINT ( 'NONE',  ( 5.974727161628369032, 10.24903993264984514, 17.78288073588506180 ) ) ;
#22387 = CARTESIAN_POINT ( 'NONE',  ( 4.967162193818131399, 35.57684288741977241, 24.30453456948122692 ) ) ;
#22388 = CARTESIAN_POINT ( 'NONE',  ( -6.016489644550737204, -0.004404229197908116067, 18.84320342686341121 ) ) ;
#22389 = CONICAL_SURFACE ( 'NONE', #14405, 48.09070567114147110, 0.04450589592585947607 ) ;
#22390 = FACE_OUTER_BOUND ( 'NONE', #55025, .T. ) ;
#22391 = CARTESIAN_POINT ( 'NONE',  ( 0.6024113833632039894, -42.89465211219818030, 23.90796288424339977 ) ) ;
#22392 = CARTESIAN_POINT ( 'NONE',  ( 0.9749527285493316819, 42.90750796893246388, 0.2856147164660120530 ) ) ;
#22393 = CARTESIAN_POINT ( 'NONE',  ( 0.9762797500689124330, 32.57381952463229169, 26.36799322592426975 ) ) ;
#22394 = CARTESIAN_POINT ( 'NONE',  ( 4.962356264823596597, 1.841560470688234474, 42.04574000888969465 ) ) ;
#22395 = FACE_OUTER_BOUND ( 'NONE', #6147, .T. ) ;
#22396 = CARTESIAN_POINT ( 'NONE',  ( 2.281351352603295357, -47.37344280316140299, -7.562287671717704995 ) ) ;
#22397 = ORIENTED_EDGE ( 'NONE', *, *, #12883, .F. ) ;
#22398 = ADVANCED_FACE ( 'NONE', ( #54768 ), #34145, .F. ) ;
#22399 = CARTESIAN_POINT ( 'NONE',  ( 0.5998501479064699549, -0.5236536531311584142, -48.10473956285919428 ) ) ;
#22400 = CYLINDRICAL_SURFACE ( 'NONE', #2380, 2.649999999999992806 ) ;
#22401 = CARTESIAN_POINT ( 'NONE',  ( 4.956653778116987041, -47.94889704119048446, -3.690426056930470988 ) ) ;
#22402 = DIRECTION ( 'NONE',  ( -0.07439287786467650709, 0.8569499480575054617, -0.5100024374914788883 ) ) ;
#22403 = VECTOR ( 'NONE', #13773, 1000.000000000000000 ) ;
#22404 = B_SPLINE_CURVE_WITH_KNOTS ( 'NONE', 3,
 ( #53103, #1393, #10209, #53407 ),
 .UNSPECIFIED., .F., .F.,
 ( 4, 4 ),
 ( 2.194270917860438266E-17, 0.005004948556313820046 ),
 .UNSPECIFIED. ) ;
#22405 = CARTESIAN_POINT ( 'NONE',  ( 0.6000166863083106206, -19.40010892967683986, 45.11606427011477649 ) ) ;
#22406 = CARTESIAN_POINT ( 'NONE',  ( 5.959547316686252039, 20.34955788964376566, -2.682663672454702830 ) ) ;
#22407 = EDGE_CURVE ( 'NONE', #49553, #32791, #44805, .T. ) ;
#22408 = APPLICATION_PROTOCOL_DEFINITION ( 'draft international standard', 'automotive_design', 1998, #51153 ) ;
#22409 = CARTESIAN_POINT ( 'NONE',  ( 0.5987334308729319599, -2.178790671009264379, -49.05930877806629553 ) ) ;
#22410 =( BOUNDED_SURFACE ( )  B_SPLINE_SURFACE ( 3, 1, ( 
 ( #29917, #49027 ),
 ( #6078, #25217 ),
 ( #59026, #35256 ),
 ( #25835, #44972 ) ),
 .UNSPECIFIED., .F., .F., .F. ) 
 B_SPLINE_SURFACE_WITH_KNOTS ( ( 4, 4 ),
 ( 2, 2 ),
 ( 0.000000000000000000, 1.000000000000000000 ),
 ( 0.000000000000000000, 1.000000000000000000 ),
 .UNSPECIFIED. ) 
 GEOMETRIC_REPRESENTATION_ITEM ( )  RATIONAL_B_SPLINE_SURFACE ( (
 ( 1.000000000000000000, 1.000000000000000000),
 ( 0.9952954269826590483, 0.8620686068821339365),
 ( 0.9952954269826590483, 0.8620686068821339365),
 ( 1.000000000000000000, 1.000000000000000000) ) ) 
 REPRESENTATION_ITEM ( '' )  SURFACE ( )  );
#22411 = CARTESIAN_POINT ( 'NONE',  ( 1.479689385636123067, 36.27458947416105417, -25.01475572034986072 ) ) ;
#22412 = EDGE_CURVE ( 'NONE', #5908, #42065, #27052, .T. ) ;
#22413 = CARTESIAN_POINT ( 'NONE',  ( 0.2885697896453107147, 6.424755442172600972, -42.63514065501009043 ) ) ;
#22415 = VERTEX_POINT ( 'NONE', #2458 ) ;
#22414 = CARTESIAN_POINT ( 'NONE',  ( 2.624215991343608501, 11.05657803851045529, 46.71702075422656009 ) ) ;
#22416 = ORIENTED_EDGE ( 'NONE', *, *, #23344, .F. ) ;
#22417 = LINE ( 'NONE', #35071, #18163 ) ;
#22418 = CARTESIAN_POINT ( 'NONE',  ( 4.962356264823608143, 0.000000000000000000, 0.000000000000000000 ) ) ;
#22419 = CARTESIAN_POINT ( 'NONE',  ( -2.569797478183783568, -3.352038560006015189, 14.24379821351251429 ) ) ;
#22420 = VERTEX_POINT ( 'NONE', #25977 ) ;
#22421 = PLANE ( 'NONE',  #41538 ) ;
#22422 = CARTESIAN_POINT ( 'NONE',  ( 0.5835871038041855474, -45.98328870143440383, 9.207150107499908032 ) ) ;
#22423 = CARTESIAN_POINT ( 'NONE',  ( 0.1073791018717483448, 5.147744207006859973, -42.81622261970989030 ) ) ;
#22424 =( BOUNDED_SURFACE ( )  B_SPLINE_SURFACE ( 3, 1, ( 
 ( #52214, #28730 ),
 ( #24030, #52522 ),
 ( #33139, #28112 ),
 ( #4278, #47851 ) ),
 .UNSPECIFIED., .F., .F., .F. ) 
 B_SPLINE_SURFACE_WITH_KNOTS ( ( 4, 4 ),
 ( 2, 2 ),
 ( 0.000000000000000000, 1.000000000000000000 ),
 ( 0.000000000000000000, 1.000000000000000000 ),
 .UNSPECIFIED. ) 
 GEOMETRIC_REPRESENTATION_ITEM ( )  RATIONAL_B_SPLINE_SURFACE ( (
 ( 1.000000000000000000, 1.000000000000000000),
 ( 0.7223157951917480446, 0.9931996967497186413),
 ( 0.7223157951917480446, 0.9931996967497186413),
 ( 1.000000000000000000, 1.000000000000000000) ) ) 
 REPRESENTATION_ITEM ( '' )  SURFACE ( )  );
#22425 = VERTEX_POINT ( 'NONE', #21585 ) ;
#22426 = ORIENTED_EDGE ( 'NONE', *, *, #659, .F. ) ;
#22427 = PLANE ( 'NONE',  #38333 ) ;
#22428 = ADVANCED_FACE ( 'NONE', ( #59792 ), #6840, .F. ) ;
#22429 = CARTESIAN_POINT ( 'NONE',  ( 2.706805983486680223, 37.76032296520254761, 22.60385194791702901 ) ) ;
#22430 = CARTESIAN_POINT ( 'NONE',  ( 0.6031357023905874470, 41.64046004335383344, 24.09149424676630957 ) ) ;
#22431 = ORIENTED_EDGE ( 'NONE', *, *, #45416, .F. ) ;
#22432 = EDGE_CURVE ( 'NONE', #60557, #28087, #4597, .T. ) ;
#22433 = CARTESIAN_POINT ( 'NONE',  ( 4.390527457369401532, -43.86299345468695066, 2.494622581215259149 ) ) ;
#22434 = B_SPLINE_CURVE_WITH_KNOTS ( 'NONE', 3,
 ( #59790, #25656, #11257, #2135 ),
 .UNSPECIFIED., .F., .F.,
 ( 4, 4 ),
 ( 0.000000000000000000, 0.004442905043737215703 ),
 .UNSPECIFIED. ) ;
#22435 = VECTOR ( 'NONE', #29572, 1000.000000000000000 ) ;
#22436 = FACE_OUTER_BOUND ( 'NONE', #29815, .T. ) ;
#22437 = ADVANCED_FACE ( 'NONE', ( #4839 ), #43579, .T. ) ;
#22438 = CARTESIAN_POINT ( 'NONE',  ( 0.5980271706414711508, 27.52111707190132961, 40.67723390247133608 ) ) ;
#22439 = CARTESIAN_POINT ( 'NONE',  ( 0.1156867017252034557, 33.51703926206629802, 28.69757631543633991 ) ) ;
#22440 = ORIENTED_EDGE ( 'NONE', *, *, #11415, .T. ) ;
#22441 = CARTESIAN_POINT ( 'NONE',  ( 2.643462169533613793, -47.78621045426871916, -4.896978544601982897 ) ) ;
#22442 = CARTESIAN_POINT ( 'NONE',  ( 0.5786265663353196143, -47.39171391660386234, -6.967625775956209466 ) ) ;
#22443 = VERTEX_POINT ( 'NONE', #37800 ) ;
#22444 = CARTESIAN_POINT ( 'NONE',  ( 0.7948884756798525464, -20.66454828366466501, 44.53846751777887647 ) ) ;
#22445 = CARTESIAN_POINT ( 'NONE',  ( 0.1064266379913941241, 34.55203636557774161, 25.80493164505215375 ) ) ;
#22446 = CARTESIAN_POINT ( 'NONE',  ( 1.834102595619085285, 39.10291415957683370, -20.27707693644353171 ) ) ;
#22447 = DIRECTION ( 'NONE',  ( 0.000000000000000000, 0.000000000000000000, 1.000000000000000000 ) ) ;
#22448 = EDGE_CURVE ( 'NONE', #37659, #6381, #7611, .T. ) ;
#22449 = AXIS2_PLACEMENT_3D ( 'NONE', #36649, #55105, #8414 ) ;
#22450 = ORIENTED_EDGE ( 'NONE', *, *, #53326, .F. ) ;
#22451 = VERTEX_POINT ( 'NONE', #57450 ) ;
#22452 = CARTESIAN_POINT ( 'NONE',  ( 5.960721111146673579, -7.848955554238637333, 18.96557324978273940 ) ) ;
#22453 = DIRECTION ( 'NONE',  ( 0.000000000000000000, 0.000000000000000000, -1.000000000000000000 ) ) ;
#22454 = ORIENTED_EDGE ( 'NONE', *, *, #9982, .F. ) ;
#22455 = CARTESIAN_POINT ( 'NONE',  ( 0.1064266418746777770, 25.80493189480185379, 34.55203617814598260 ) ) ;
#22456 = ORIENTED_EDGE ( 'NONE', *, *, #3371, .F. ) ;
#22457 = CARTESIAN_POINT ( 'NONE',  ( 2.299652685299200083, -40.05308401807694452, 28.28484020635476170 ) ) ;
#22458 = EDGE_LOOP ( 'NONE', ( #2687, #18736, #35193, #17515 ) ) ;
#22459 = CARTESIAN_POINT ( 'NONE',  ( 3.727782113643637096, 43.51027460820039749, 6.295536468401055075 ) ) ;
#22460 = CARTESIAN_POINT ( 'NONE',  ( 0.9790320750461898314, 24.79011560905074063, 33.79034330444261514 ) ) ;
#22461 = LINE ( 'NONE', #41585, #29227 ) ;
#22462 = VERTEX_POINT ( 'NONE', #9558 ) ;
#22463 = CARTESIAN_POINT ( 'NONE',  ( 4.291220156522060236, -33.45801620160754908, 33.16549636532919010 ) ) ;
#22464 = LINE ( 'NONE', #12161, #44684 ) ;
#22465 = CARTESIAN_POINT ( 'NONE',  ( 1.091591847532192183, 29.69394621724348227, -29.58088147779393040 ) ) ;
#22466 = ORIENTED_EDGE ( 'NONE', *, *, #3210, .T. ) ;
#22467 = CARTESIAN_POINT ( 'NONE',  ( 0.5998501479064699549, -37.84527566984877467, 29.69975237324549155 ) ) ;
#22468 = CARTESIAN_POINT ( 'NONE',  ( 0.8760168074886965917, -44.77533136581894269, 17.58183840866320224 ) ) ;
#22469 = VECTOR ( 'NONE', #37460, 1000.000000000000114 ) ;
#22470 = CARTESIAN_POINT ( 'NONE',  ( 4.291220156522060236, 46.35409538318327094, -8.407546521574817078 ) ) ;
#22471 = CARTESIAN_POINT ( 'NONE',  ( 0.5998501479064708430, -11.94461217097437000, -46.60114184914313995 ) ) ;
#22472 = VERTEX_POINT ( 'NONE', #43102 ) ;
#22473 = CARTESIAN_POINT ( 'NONE',  ( 2.624215991343620935, 7.662883702704664124, 47.39206852872460018 ) ) ;
#22474 = EDGE_CURVE ( 'NONE', #10386, #61727, #38278, .T. ) ;
#22475 = CARTESIAN_POINT ( 'NONE',  ( 0.5987334308729322929, -48.77819069500445437, -5.678998071095664457 ) ) ;
#22476 = ORIENTED_EDGE ( 'NONE', *, *, #9134, .F. ) ;
#22477 = EDGE_CURVE ( 'NONE', #27319, #54223, #24052, .T. ) ;
#22478 = CARTESIAN_POINT ( 'NONE',  ( 0.2500000000000002220, 0.000000000000000000, 4.000000000000000000 ) ) ;
#22479 = CARTESIAN_POINT ( 'NONE',  ( 5.901764892641307547, 42.68902166415596611, -23.99247583716404719 ) ) ;
#22480 = B_SPLINE_CURVE_WITH_KNOTS ( 'NONE', 3,
 ( #29750, #40126, #16283, #1236, #20369, #35406, #46051, #2151, #45425, #17216, #36637, #40422, #26288, #59485, #41047, #21293, #30998, #36337, #49794 ),
 .UNSPECIFIED., .F., .F.,
 ( 4, 3, 3, 3, 3, 3, 4 ),
 ( 3.469552829456483146E-18, 0.0002612768053151735522, 0.0003919133833142943407, 0.0005225499612322647650, 0.0006531865391693365006, 0.0008112755173415180142, 0.0009693688056799728983 ),
 .UNSPECIFIED. ) ;
#22481 = DIRECTION ( 'NONE',  ( -1.000000000000000000, -0.000000000000000000, 1.925929944387235853E-32 ) ) ;
#22482 = CARTESIAN_POINT ( 'NONE',  ( 0.1064266418746778603, -11.70292610004353762, 41.50637583369802286 ) ) ;
#22483 = CARTESIAN_POINT ( 'NONE',  ( 1.231276596079887931, -40.90292846002456173, 9.177538581350681568 ) ) ;
#22484 = CARTESIAN_POINT ( 'NONE',  ( 5.917102823773431552, 17.95415397368191179, 9.063005745395072310 ) ) ;
#22485 = DIRECTION ( 'NONE',  ( 0.09722883295013595717, 0.9754357953229587652, 0.1976652808305532638 ) ) ;
#22486 = EDGE_CURVE ( 'NONE', #34885, #24606, #57524, .T. ) ;
#22487 = SHAPE_REPRESENTATION_RELATIONSHIP ( 'NONE' , 'NONE' ,  #19619, #35493 ) ;
#22488 = CARTESIAN_POINT ( 'NONE',  ( 4.975610109902397937, -48.84566763821283786, 2.559328059280373768 ) ) ;
#22489 = FACE_OUTER_BOUND ( 'NONE', #61558, .T. ) ;
#22490 = CARTESIAN_POINT ( 'NONE',  ( 1.091591847532193293, 19.45518260472246652, 37.12485502695927408 ) ) ;
#22491 = CONICAL_SURFACE ( 'NONE', #5462, 42.92674063221959813, 1.485477209440487556 ) ;
#22492 = EDGE_CURVE ( 'NONE', #24440, #27931, #61850, .T. ) ;
#22493 = CARTESIAN_POINT ( 'NONE',  ( 4.975610109902397937, 19.27143522741655701, 44.95621415792550124 ) ) ;
#22494 = AXIS2_PLACEMENT_3D ( 'NONE', #22192, #7762, #36002 ) ;
#22495 = CARTESIAN_POINT ( 'NONE',  ( 5.860006189529234355, 21.34829429597467509, 43.25137511473258911 ) ) ;
#22496 = CARTESIAN_POINT ( 'NONE',  ( 4.999999999999984901, 72.00000000000002842, -9.629649721936170507E-32 ) ) ;
#22497 = CARTESIAN_POINT ( 'NONE',  ( 1.112077966505212068, 16.20463149544202253, 40.99317312950392989 ) ) ;
#22498 = AXIS2_PLACEMENT_3D ( 'NONE', #22911, #13514, #18517 ) ;
#22499 = CARTESIAN_POINT ( 'NONE',  ( 0.8751705887134553219, -44.76769609654225235, -17.57879340691528469 ) ) ;
#22500 = CARTESIAN_POINT ( 'NONE',  ( 3.680974057930773480, -10.62112035260209808, -46.78530430706934595 ) ) ;
#22501 = CARTESIAN_POINT ( 'NONE',  ( 0.9268187852002115479, 32.91938759995093022, -29.32692027732920437 ) ) ;
#22502 = EDGE_CURVE ( 'NONE', #43289, #12977, #24831, .T. ) ;
#22503 = ORIENTED_EDGE ( 'NONE', *, *, #40907, .T. ) ;
#22504 = B_SPLINE_CURVE_WITH_KNOTS ( 'NONE', 3,
 ( #19483, #38599, #39529, #24476 ),
 .UNSPECIFIED., .F., .F.,
 ( 4, 4 ),
 ( 0.000000000000000000, 0.004446090762761374660 ),
 .UNSPECIFIED. ) ;
#22505 = CARTESIAN_POINT ( 'NONE',  ( 4.956653778116996811, 45.35992544608552635, -15.97476558431834626 ) ) ;
#22506 = ADVANCED_FACE ( 'NONE', ( #29588 ), #14940, .F. ) ;
#22507 =( BOUNDED_SURFACE ( )  B_SPLINE_SURFACE ( 3, 1, ( 
 ( #44008, #20178 ),
 ( #49903, #11704 ),
 ( #30783, #20785 ),
 ( #25466, #59286 ) ),
 .UNSPECIFIED., .F., .F., .F. ) 
 B_SPLINE_SURFACE_WITH_KNOTS ( ( 4, 4 ),
 ( 2, 2 ),
 ( 0.000000000000000000, 1.000000000000000000 ),
 ( 0.000000000000000000, 1.000000000000000000 ),
 .UNSPECIFIED. ) 
 GEOMETRIC_REPRESENTATION_ITEM ( )  RATIONAL_B_SPLINE_SURFACE ( (
 ( 1.000000000000000000, 1.000000000000000000),
 ( 0.9732289882329797637, 0.9999525324661233672),
 ( 0.9732289882329797637, 0.9999525324661233672),
 ( 1.000000000000000000, 1.000000000000000000) ) ) 
 REPRESENTATION_ITEM ( '' )  SURFACE ( )  );
#22508 = B_SPLINE_CURVE_WITH_KNOTS ( 'NONE', 3,
 ( #51967, #24090, #46677, #3722 ),
 .UNSPECIFIED., .F., .F.,
 ( 4, 4 ),
 ( 0.000000000000000000, 0.004444103432399267896 ),
 .UNSPECIFIED. ) ;
#22509 = CARTESIAN_POINT ( 'NONE',  ( -6.001507490154110336, -11.45906331631441866, 14.95933060264870029 ) ) ;
#22510 = CARTESIAN_POINT ( 'NONE',  ( 3.894904216938897878, 27.86699861404660439, -33.99345114460909656 ) ) ;
#22511 = CARTESIAN_POINT ( 'NONE',  ( 5.896782393890504181, 10.81700609697876736, 16.95636948099257424 ) ) ;
#22512 = ORIENTED_EDGE ( 'NONE', *, *, #53281, .F. ) ;
#22513 = CARTESIAN_POINT ( 'NONE',  ( 5.981074661064941900, 10.26976685693798608, 17.77058762078881315 ) ) ;
#22514 = FACE_OUTER_BOUND ( 'NONE', #14582, .T. ) ;
#22515 = EDGE_CURVE ( 'NONE', #17505, #16995, #59874, .T. ) ;
#22516 = ORIENTED_EDGE ( 'NONE', *, *, #9504, .T. ) ;
#22517 = CIRCLE ( 'NONE', #44547, 0.05882000000000109363 ) ;
#22518 = CARTESIAN_POINT ( 'NONE',  ( 4.553261556744875094, -25.31600221269659201, 35.89762663172006540 ) ) ;
#22519 = VERTEX_POINT ( 'NONE', #30500 ) ;
#22520 =( BOUNDED_SURFACE ( )  B_SPLINE_SURFACE ( 3, 1, ( 
 ( #57742, #19881 ),
 ( #14874, #17878 ),
 ( #22570, #37002 ),
 ( #37296, #41093 ) ),
 .UNSPECIFIED., .F., .F., .F. ) 
 B_SPLINE_SURFACE_WITH_KNOTS ( ( 4, 4 ),
 ( 2, 2 ),
 ( 0.000000000000000000, 1.000000000000000000 ),
 ( 0.000000000000000000, 1.000000000000000000 ),
 .UNSPECIFIED. ) 
 GEOMETRIC_REPRESENTATION_ITEM ( )  RATIONAL_B_SPLINE_SURFACE ( (
 ( 1.000000000000000000, 1.000000000000000000),
 ( 0.9732289882329797637, 0.9999525324661233672),
 ( 0.9732289882329797637, 0.9999525324661233672),
 ( 1.000000000000000000, 1.000000000000000000) ) ) 
 REPRESENTATION_ITEM ( '' )  SURFACE ( )  );
#22521 = CARTESIAN_POINT ( 'NONE',  ( 5.901764892641288895, -28.05153439369972901, -40.13854613210049394 ) ) ;
#22522 = CARTESIAN_POINT ( 'NONE',  ( 0.8760168074887076939, -46.68716261866168082, -11.58706983520309208 ) ) ;
#22523 = ORIENTED_EDGE ( 'NONE', *, *, #44485, .T. ) ;
#22524 = CARTESIAN_POINT ( 'NONE',  ( 0.6001305935487422083, 17.92615948558477967, 44.64600790884061610 ) ) ;
#22525 = CARTESIAN_POINT ( 'NONE',  ( 3.680974057930773924, 35.20670187740660140, -32.59081219553993236 ) ) ;
#22526 = ORIENTED_EDGE ( 'NONE', *, *, #19402, .F. ) ;
#22527 = CARTESIAN_POINT ( 'NONE',  ( -14.84250595937557016, -4.999999999999995559, 10.00000000000000711 ) ) ;
#22528 = CARTESIAN_POINT ( 'NONE',  ( 4.967162193818131399, -14.26841313271251543, -40.65506779172179108 ) ) ;
#22529 =( BOUNDED_SURFACE ( )  B_SPLINE_SURFACE ( 3, 1, ( 
 ( #8394, #51006 ),
 ( #46960, #61020 ),
 ( #32541, #51620 ),
 ( #31919, #12827 ) ),
 .UNSPECIFIED., .F., .F., .F. ) 
 B_SPLINE_SURFACE_WITH_KNOTS ( ( 4, 4 ),
 ( 2, 2 ),
 ( 0.000000000000000000, 1.000000000000000000 ),
 ( 0.000000000000000000, 1.000000000000000000 ),
 .UNSPECIFIED. ) 
 GEOMETRIC_REPRESENTATION_ITEM ( )  RATIONAL_B_SPLINE_SURFACE ( (
 ( 1.000000000000000000, 1.000000000000000000),
 ( 0.9953485035131437453, 0.8621029689291515030),
 ( 0.9953485035131437453, 0.8621029689291515030),
 ( 1.000000000000000000, 1.000000000000000000) ) ) 
 REPRESENTATION_ITEM ( '' )  SURFACE ( )  );
#22530 = EDGE_CURVE ( 'NONE', #20695, #49095, #10637, .T. ) ;
#22531 = VERTEX_POINT ( 'NONE', #1370 ) ;
#22532 = CARTESIAN_POINT ( 'NONE',  ( -6.072942160501519027, 13.84283391500593119, -13.38581755032474874 ) ) ;
#22533 = EDGE_LOOP ( 'NONE', ( #16616, #49701, #33795, #44184 ) ) ;
#22534 = CARTESIAN_POINT ( 'NONE',  ( 0.8760168074887090262, -0.8912768426702896152, -48.09529047980637273 ) ) ;
#22535 = ADVANCED_FACE ( 'NONE', ( #34011 ), #13284, .F. ) ;
#22536 = VERTEX_POINT ( 'NONE', #24592 ) ;
#22537 = ORIENTED_EDGE ( 'NONE', *, *, #59158, .T. ) ;
#22538 = LINE ( 'NONE', #51951, #38702 ) ;
#22539 = CARTESIAN_POINT ( 'NONE',  ( 4.975801465491695552, 46.87746200127456575, -9.906103548667728020 ) ) ;
#22540 = CARTESIAN_POINT ( 'NONE',  ( 0.8751705887134423323, -24.81530984069236823, 41.19904111682465242 ) ) ;
#22541 = CIRCLE ( 'NONE', #55551, 48.09070567114147110 ) ;
#22542 = LINE ( 'NONE', #60726, #11265 ) ;
#22543 = CARTESIAN_POINT ( 'NONE',  ( -2.708315649062916552, -11.44805714186577639, 9.116606751444143342 ) ) ;
#22544 = ORIENTED_EDGE ( 'NONE', *, *, #46152, .T. ) ;
#22545 = CARTESIAN_POINT ( 'NONE',  ( 4.390527457369401532, 6.694952568920494507, 43.42076630747694566 ) ) ;
#22546 = CARTESIAN_POINT ( 'NONE',  ( 2.618530812446115519, -42.57172246446581454, -19.93427288883888338 ) ) ;
#22547 = CARTESIAN_POINT ( 'NONE',  ( -5.331200000000000827, 0.000000000000000000, 15.38218000000000174 ) ) ;
#22548 = AXIS2_PLACEMENT_3D ( 'NONE', #17761, #2716, #37193 ) ;
#22549 = VERTEX_POINT ( 'NONE', #53082 ) ;
#22550 = ORIENTED_EDGE ( 'NONE', *, *, #50068, .T. ) ;
#22551 = CARTESIAN_POINT ( 'NONE',  ( 4.553261556744875094, 0.000000000000000000, 0.000000000000000000 ) ) ;
#22552 = CARTESIAN_POINT ( 'NONE',  ( 1.830465331921976579, 32.72788206612836603, 29.48324594314511771 ) ) ;
#22553 = CARTESIAN_POINT ( 'NONE',  ( 4.553261556744873317, -3.993093339917161977, 43.74465420371208069 ) ) ;
#22554 = VERTEX_POINT ( 'NONE', #49615 ) ;
#22555 = CARTESIAN_POINT ( 'NONE',  ( 2.528100132419516033, 35.48725650258067077, -22.42561937945352923 ) ) ;
#22556 = VERTEX_POINT ( 'NONE', #49310 ) ;
#22557 = CARTESIAN_POINT ( 'NONE',  ( 0.5839879327111925367, 47.49806740880208622, 6.161619650335476095 ) ) ;
#22558 = ADVANCED_FACE ( 'NONE', ( #10187 ), #29775, .T. ) ;
#22559 = CARTESIAN_POINT ( 'NONE',  ( 2.299652685299200527, 32.00015747886172335, 37.15200729686356595 ) ) ;
#22560 = CARTESIAN_POINT ( 'NONE',  ( 0.9740398440564312921, -33.78760696452724233, 26.44872719679357687 ) ) ;
#22561 = CARTESIAN_POINT ( 'NONE',  ( 0.5817217712918333339, -41.64824464290960293, -21.55594285046991487 ) ) ;
#22562 = CARTESIAN_POINT ( 'NONE',  ( 0.8560838555295223751, 37.37287335782406217, 28.34856559090382078 ) ) ;
#22563 = EDGE_CURVE ( 'NONE', #47431, #50643, #14301, .T. ) ;
#22564 = DIRECTION ( 'NONE',  ( -1.000000000000000000, -1.836909530733573776E-16, 1.925929944387235853E-32 ) ) ;
#22565 = EDGE_LOOP ( 'NONE', ( #59151, #11549, #10681, #46916 ) ) ;
#22566 = CARTESIAN_POINT ( 'NONE',  ( 0.8551540677456715978, 38.56334384152469852, -28.44084013485079154 ) ) ;
#22567 = EDGE_CURVE ( 'NONE', #35268, #17533, #26264, .T. ) ;
#22568 = CARTESIAN_POINT ( 'NONE',  ( 0.7954190325252789018, 46.22745637125041895, -13.28627193046320620 ) ) ;
#22569 = ADVANCED_FACE ( 'NONE', ( #14905 ), #38517, .T. ) ;
#22570 = CARTESIAN_POINT ( 'NONE',  ( 5.958863334805807099, -12.49425770716499784, 16.28483817244718068 ) ) ;
#22571 = ADVANCED_FACE ( 'NONE', ( #20212 ), #19975, .T. ) ;
#22572 = CARTESIAN_POINT ( 'NONE',  ( 0.5848930533535030563, -45.99261677209119625, -9.162547944928565613 ) ) ;
#22573 = CARTESIAN_POINT ( 'NONE',  ( 1.140000000000008784, 6.898680348956876061E-16, 5.633200000000004870 ) ) ;
#22574 = DIRECTION ( 'NONE',  ( 1.000000000000000000, 0.000000000000000000, 0.000000000000000000 ) ) ;
#22575 = CARTESIAN_POINT ( 'NONE',  ( 0.6846871229502899947, -11.56285438919665154, 46.49193983736587654 ) ) ;
#22576 = EDGE_CURVE ( 'NONE', #28235, #30729, #32273, .T. ) ;
#22577 = B_SPLINE_CURVE_WITH_KNOTS ( 'NONE', 3,
 ( #27114, #8931, #27413, #51211, #55913, #60924, #17408, #46544, #45941, #13037, #32132, #18036, #23345, #36531, #3589, #37153 ),
 .UNSPECIFIED., .F., .F.,
 ( 4, 3, 3, 3, 3, 4 ),
 ( 2.081781105835003463E-17, 0.0002612764279487748975, 0.0003919131003184791909, 0.0005225497727000653642, 0.0007837925190632464385, 0.001045051706266716517 ),
 .UNSPECIFIED. ) ;
#22578 = VECTOR ( 'NONE', #37720, 1000.000000000000114 ) ;
#22579 = CARTESIAN_POINT ( 'NONE',  ( -90.00000000000000000, 9.184850993605177527E-16, 7.500000000000022204 ) ) ;
#22580 = CARTESIAN_POINT ( 'NONE',  ( 0.5836750258453351492, -29.01293504009516866, -38.10871351907219662 ) ) ;
#22581 = ORIENTED_EDGE ( 'NONE', *, *, #6430, .F. ) ;
#22582 = CARTESIAN_POINT ( 'NONE',  ( 2.648799415243696664, -49.01629645596155171, -1.385692978581185342 ) ) ;
#22583 = AXIS2_PLACEMENT_3D ( 'NONE', #47715, #4762, #13914 ) ;
#22584 = CARTESIAN_POINT ( 'NONE',  ( 0.5839879882012681822, 46.26395995854837651, 12.39635945868979050 ) ) ;
#22585 = CARTESIAN_POINT ( 'NONE',  ( -2.601141883200665639, 10.36212650428638682, -10.74345204199070380 ) ) ;
#22586 = CARTESIAN_POINT ( 'NONE',  ( 3.680974057930773036, 47.28851186370997084, 8.091325130366584517 ) ) ;
#22587 = ORIENTED_EDGE ( 'NONE', *, *, #50182, .F. ) ;
#22588 = CARTESIAN_POINT ( 'NONE',  ( -5.995132425357893702, 4.885449473615331328, 18.19985213254573964 ) ) ;
#22589 = CIRCLE ( 'NONE', #11595, 9.500000000000000000 ) ;
#22590 = CARTESIAN_POINT ( 'NONE',  ( 0.8557997880470599172, -47.89938907511592703, -0.9121262075951160897 ) ) ;
#22591 = FILL_AREA_STYLE ('',( #27590 ) ) ;
#22592 = ORIENTED_EDGE ( 'NONE', *, *, #40276, .F. ) ;
#22593 = CARTESIAN_POINT ( 'NONE',  ( 0.6000166863083106206, -49.10753961887881758, -0.5225268306040948829 ) ) ;
#22594 = CARTESIAN_POINT ( 'NONE',  ( 0.7048096507298579061, -33.41730025321730579, -34.61049487267047908 ) ) ;
#22595 = CARTESIAN_POINT ( 'NONE',  ( 3.661933894777896104, 41.39923993790886669, -22.33235539559372995 ) ) ;
#22596 = VERTEX_POINT ( 'NONE', #59319 ) ;
#22597 = CARTESIAN_POINT ( 'NONE',  ( 3.270143674763207553, -12.53844339339238445, 5.490410281242732893 ) ) ;
#22598 = ORIENTED_EDGE ( 'NONE', *, *, #47647, .F. ) ;
#22599 = VERTEX_POINT ( 'NONE', #36475 ) ;
#22600 = CARTESIAN_POINT ( 'NONE',  ( 0.5836750258453350382, -6.071582023533952821, -47.50958153310757837 ) ) ;
#22601 = ORIENTED_EDGE ( 'NONE', *, *, #4754, .T. ) ;
#22602 = FACE_OUTER_BOUND ( 'NONE', #29884, .T. ) ;
#22603 = ORIENTED_EDGE ( 'NONE', *, *, #57664, .F. ) ;
#22604 = CARTESIAN_POINT ( 'NONE',  ( -2.739355103387247858, 3.064916856561431313, 14.61005994557799781 ) ) ;
#22605 =( BOUNDED_SURFACE ( )  B_SPLINE_SURFACE ( 3, 1, ( 
 ( #60656, #17459 ),
 ( #41285, #31875 ),
 ( #13389, #55650 ),
 ( #3037, #3951 ) ),
 .UNSPECIFIED., .F., .F., .F. ) 
 B_SPLINE_SURFACE_WITH_KNOTS ( ( 4, 4 ),
 ( 2, 2 ),
 ( 0.000000000000000000, 1.000000000000000000 ),
 ( 0.000000000000000000, 1.000000000000000000 ),
 .UNSPECIFIED. ) 
 GEOMETRIC_REPRESENTATION_ITEM ( )  RATIONAL_B_SPLINE_SURFACE ( (
 ( 1.000000000000000000, 1.000000000000000000),
 ( 0.9729067724841187204, 0.9999501103223794596),
 ( 0.9729067724841187204, 0.9999501103223794596),
 ( 1.000000000000000000, 1.000000000000000000) ) ) 
 REPRESENTATION_ITEM ( '' )  SURFACE ( )  );
#22606 = EDGE_CURVE ( 'NONE', #42072, #31462, #6823, .T. ) ;
#22607 = CARTESIAN_POINT ( 'NONE',  ( 3.782542959838398833, 8.059551392177747076, 41.25871404628865946 ) ) ;
#22608 = ORIENTED_EDGE ( 'NONE', *, *, #61962, .T. ) ;
#22609 = DIRECTION ( 'NONE',  ( 1.000000000000000000, 1.558861125776144859E-16, -3.851859888774471706E-32 ) ) ;
#22610 = CARTESIAN_POINT ( 'NONE',  ( -25.39999999999999858, 0.000000000000000000, 12.49999999999999822 ) ) ;
#22611 = CARTESIAN_POINT ( 'NONE',  ( 4.833616638992208614, -30.15290813935929748, 35.06988470649517353 ) ) ;
#22612 = CARTESIAN_POINT ( 'NONE',  ( 0.6254311100348634023, -41.31309618784398907, -24.64676532715779800 ) ) ;
#22613 = EDGE_LOOP ( 'NONE', ( #56496, #48479, #50061, #4448 ) ) ;
#22614 = FACE_OUTER_BOUND ( 'NONE', #42054, .T. ) ;
#22615 = ORIENTED_EDGE ( 'NONE', *, *, #19031, .T. ) ;
#22616 = CARTESIAN_POINT ( 'NONE',  ( 0.8551540677456834771, -29.88829867897789683, -37.45266983663526617 ) ) ;
#22617 = VERTEX_POINT ( 'NONE', #21430 ) ;
#22618 = CARTESIAN_POINT ( 'NONE',  ( 0.7056313189692702270, -25.94337377925174692, -39.07288063232081754 ) ) ;
#22619 = CARTESIAN_POINT ( 'NONE',  ( 0.6001305935487422083, -28.87057754790966513, 38.48510059943998129 ) ) ;
#22620 = VERTEX_POINT ( 'NONE', #54607 ) ;
#22621 = LINE ( 'NONE', #21690, #41606 ) ;
#22622 = CARTESIAN_POINT ( 'NONE',  ( 4.975801465491694664, 47.84403947906843513, -2.564218696446985302 ) ) ;
#22623 = CARTESIAN_POINT ( 'NONE',  ( 0.6039202388192952409, 48.16848798300480183, 9.558267535495888367 ) ) ;
#22624 = CARTESIAN_POINT ( 'NONE',  ( 0.3622758884714600280, -4.808133778521581192, -42.84426538328729350 ) ) ;
#22625 = AXIS2_PLACEMENT_3D ( 'NONE', #5540, #53471, #38188 ) ;
#22626 = ORIENTED_EDGE ( 'NONE', *, *, #60033, .T. ) ;
#22627 = CARTESIAN_POINT ( 'NONE',  ( 4.549368137175248350, -28.14399996863474129, -32.41327393324131378 ) ) ;
#22628 = CARTESIAN_POINT ( 'NONE',  ( 0.9784957157296367836, -41.79884784847546797, 3.031398280062871375 ) ) ;
#22629 = FACE_OUTER_BOUND ( 'NONE', #15889, .T. ) ;
#22630 = AXIS2_PLACEMENT_3D ( 'NONE', #19754, #29438, #5916 ) ;
#22631 = CARTESIAN_POINT ( 'NONE',  ( -6.078726893082806448, -18.27610589745697567, 6.064486333866907053 ) ) ;
#22632 = EDGE_CURVE ( 'NONE', #27783, #19981, #50854, .T. ) ;
#22633 = CARTESIAN_POINT ( 'NONE',  ( 4.962356264823608143, -41.65024625884313991, -6.040909239515997342 ) ) ;
#22634 = CARTESIAN_POINT ( 'NONE',  ( 1.555521457401304097, -0.4925839501666971487, 49.06288516100940456 ) ) ;
#22635 = CARTESIAN_POINT ( 'NONE',  ( 0.1073791018717578927, 39.65380858626191696, 16.95003405440326816 ) ) ;
#22636 = ADVANCED_FACE ( 'NONE', ( #22355 ), #46981, .T. ) ;
#22637 = CIRCLE ( 'NONE', #44650, 16.00000000000000000 ) ;
#22638 = FACE_OUTER_BOUND ( 'NONE', #30386, .T. ) ;
#22639 = EDGE_CURVE ( 'NONE', #32675, #58502, #21739, .T. ) ;
#22640 = ADVANCED_FACE ( 'NONE', ( #55540 ), #23703, .F. ) ;
#22641 = CARTESIAN_POINT ( 'NONE',  ( -2.739355103387247858, -13.73625580088950748, -5.844898931850437407 ) ) ;
#22642 = CARTESIAN_POINT ( 'NONE',  ( 0.2230388203127557090, -15.79641846944945094, 40.12182516270770805 ) ) ;
#22643 = CARTESIAN_POINT ( 'NONE',  ( 4.975801465491695552, 46.87746200127456575, -9.906103548667728020 ) ) ;
#22644 = CARTESIAN_POINT ( 'NONE',  ( 4.967162193818132288, -24.30453456948087521, -35.57684288742000689 ) ) ;
#22645 = DIRECTION ( 'NONE',  ( -1.000000000000000000, -1.836909530733573776E-16, 1.925929944387235579E-32 ) ) ;
#22646 = CARTESIAN_POINT ( 'NONE',  ( 4.553261556744875094, 12.71466023209559104, -42.04612920360213479 ) ) ;
#22647 = CARTESIAN_POINT ( 'NONE',  ( 0.3676999524040323597, -17.09834788623527047, -40.66444494744902727 ) ) ;
#22648 = CARTESIAN_POINT ( 'NONE',  ( 0.8751705887134553219, 42.09020928323342758, 23.27176129838440488 ) ) ;
#22649 = CARTESIAN_POINT ( 'NONE',  ( 4.322998006666165516, 10.36018990813247775, 46.85697641700711813 ) ) ;
#22650 = CARTESIAN_POINT ( 'NONE',  ( 4.975801465491695552, -21.70134120755170315, -42.71626295676257001 ) ) ;
#22652 = ORIENTED_EDGE ( 'NONE', *, *, #61796, .F. ) ;
#22651 = CARTESIAN_POINT ( 'NONE',  ( 0.9745511491811756910, 39.51062171155258795, 16.73445648040586420 ) ) ;
#22653 = VERTEX_POINT ( 'NONE', #35548 ) ;
#22654 = EDGE_CURVE ( 'NONE', #44040, #30112, #852, .T. ) ;
#22655 = CARTESIAN_POINT ( 'NONE',  ( 0.5997462898726536595, 48.09935696025637952, -9.899671214446758682 ) ) ;
#22656 = FACE_OUTER_BOUND ( 'NONE', #56872, .T. ) ;
#22657 = CARTESIAN_POINT ( 'NONE',  ( 58.00000000000000000, 8.437969416220405915E-15, -2.995852231480068572E-16 ) ) ;
#22658 = ORIENTED_EDGE ( 'NONE', *, *, #29550, .T. ) ;
#22659 = EDGE_CURVE ( 'NONE', #37338, #14715, #41486, .T. ) ;
#22660 = VERTEX_POINT ( 'NONE', #59628 ) ;
#22661 = CARTESIAN_POINT ( 'NONE',  ( 1.479689385636123067, -30.82386906365282542, 31.48766331778968919 ) ) ;
#22662 = CARTESIAN_POINT ( 'NONE',  ( 0.2940133293163004202, 43.14164474393039228, 9.221661366941855675 ) ) ;
#22663 = VERTEX_POINT ( 'NONE', #60548 ) ;
#22664 = EDGE_LOOP ( 'NONE', ( #32165, #48785, #33569, #19365 ) ) ;
#22665 = CARTESIAN_POINT ( 'NONE',  ( 0.3622758884714600280, -26.89560658783410574, 33.69533458712297147 ) ) ;
#22666 = CIRCLE ( 'NONE', #30651, 5.000000000000000000 ) ;
#22667 = LINE ( 'NONE', #47705, #7957 ) ;
#22668 = CARTESIAN_POINT ( 'NONE',  ( 0.9736507210033057413, -41.56063510425039453, 10.66979144439354421 ) ) ;
#22669 = B_SPLINE_CURVE_WITH_KNOTS ( 'NONE', 3,
 ( #33792, #9650, #52871, #29073 ),
 .UNSPECIFIED., .F., .F.,
 ( 4, 4 ),
 ( 0.000000000000000000, 0.005004741218457411066 ),
 .UNSPECIFIED. ) ;
#22670 = CIRCLE ( 'NONE', #9647, 48.91267123290010943 ) ;
#22671 = ORIENTED_EDGE ( 'NONE', *, *, #15646, .F. ) ;
#22672 = VERTEX_POINT ( 'NONE', #26427 ) ;
#22673 = CARTESIAN_POINT ( 'NONE',  ( 1.155036213957052500E-14, 4.618802153517020059, -5.599999999999999645 ) ) ;
#22674 = CARTESIAN_POINT ( 'NONE',  ( 4.975801465491695552, 0.000000000000000000, 0.000000000000000000 ) ) ;
#22675 = EDGE_CURVE ( 'NONE', #44582, #21914, #25945, .T. ) ;
#22676 = CARTESIAN_POINT ( 'NONE',  ( 1.399999999999998579, 0.000000000000000000, -7.500000000000022204 ) ) ;
#22677 = VERTEX_POINT ( 'NONE', #45563 ) ;
#22678 = VECTOR ( 'NONE', #16257, 1000.000000000000000 ) ;
#22679 = ORIENTED_EDGE ( 'NONE', *, *, #40986, .F. ) ;
#22680 = CARTESIAN_POINT ( 'NONE',  ( 2.624215991343608501, -19.66774719433009722, 43.79392271049062657 ) ) ;
#22681 = ORIENTED_EDGE ( 'NONE', *, *, #45155, .T. ) ;
#22682 = CARTESIAN_POINT ( 'NONE',  ( 0.5807400328401637335, -33.48217046439135203, 34.25275203086223286 ) ) ;
#22683 = CARTESIAN_POINT ( 'NONE',  ( 0.6041374136657475802, 34.14050483116137258, -33.89363087703013377 ) ) ;
#22684 = CARTESIAN_POINT ( 'NONE',  ( 0.6027935024548038978, 34.14031893787224448, -33.89348162668942166 ) ) ;
#22685 = CARTESIAN_POINT ( 'NONE',  ( -6.078075953587585900, 12.00179475453279387, 15.05828997320761786 ) ) ;
#22686 = CARTESIAN_POINT ( 'NONE',  ( 0.7242486021783849370, -2.392220701665511040, 49.04374315331669720 ) ) ;
#22687 = ORIENTED_EDGE ( 'NONE', *, *, #44411, .T. ) ;
#22688 = CARTESIAN_POINT ( 'NONE',  ( -6.017396004339687465, 9.422598049764850714, -16.31807101179360942 ) ) ;
#22689 = CARTESIAN_POINT ( 'NONE',  ( -6.057079549204054558, -1.840653143754622523, 19.16880870331082320 ) ) ;
#22690 = B_SPLINE_CURVE_WITH_KNOTS ( 'NONE', 3,
 ( #53793, #6176, #43844, #30619 ),
 .UNSPECIFIED., .F., .F.,
 ( 4, 4 ),
 ( 6.992893892674702526E-18, 0.005014147105413695182 ),
 .UNSPECIFIED. ) ;
#22691 = CARTESIAN_POINT ( 'NONE',  ( 0.8554163680231708922, 42.82911630180332452, 19.15391004255850405 ) ) ;
#22692 = ORIENTED_EDGE ( 'NONE', *, *, #54001, .T. ) ;
#22693 = CARTESIAN_POINT ( 'NONE',  ( 2.528190830796656297, -37.99746236544471145, 17.84508307460686183 ) ) ;
#22694 = CARTESIAN_POINT ( 'NONE',  ( 0.1129192098497455998, 30.02178898772931603, -32.33641869102712718 ) ) ;
#22695 = CARTESIAN_POINT ( 'NONE',  ( 3.238018933889920792, -13.06836926121502707, 2.936872012904754747 ) ) ;
#22696 = VERTEX_POINT ( 'NONE', #7302 ) ;
#22697 = CARTESIAN_POINT ( 'NONE',  ( 0.6846871229502932144, -43.92355552798024121, -19.12907057981251313 ) ) ;
#22698 = CARTESIAN_POINT ( 'NONE',  ( 4.967162193818131399, 35.57684288741977241, 24.30453456948122692 ) ) ;
#22699 = DIRECTION ( 'NONE',  ( 0.000000000000000000, 0.000000000000000000, 1.000000000000000000 ) ) ;
#22700 = CARTESIAN_POINT ( 'NONE',  ( 5.981074661064941900, -14.50705827991436081, -14.51919955600730638 ) ) ;
#22701 = CARTESIAN_POINT ( 'NONE',  ( 0.000000000000000000, 2.357898499370431722, -2.818925648462311528E-15 ) ) ;
#22702 = CARTESIAN_POINT ( 'NONE',  ( -6.010958268070873523, -16.32616437357105710, -9.409153349053758220 ) ) ;
#22703 = CARTESIAN_POINT ( 'NONE',  ( 0.1073791018717483448, 42.68962945260953035, -6.109314776652274404 ) ) ;
#22704 = CARTESIAN_POINT ( 'NONE',  ( 1.088313998177381281, 20.77783415101626829, 37.54798835078467789 ) ) ;
#22705 = CARTESIAN_POINT ( 'NONE',  ( 5.901463166500145796, -17.31230476672938323, 10.23728352662539542 ) ) ;
#22706 = ADVANCED_FACE ( 'NONE', ( #31445 ), #59731, .F. ) ;
#22707 = CARTESIAN_POINT ( 'NONE',  ( 0.9787284016396609054, -1.587498718041325363, -41.87858458387827909 ) ) ;
#22708 = CARTESIAN_POINT ( 'NONE',  ( 0.5797568599927135358, 11.48244781954172922, -45.46843631292489363 ) ) ;
#22709 = ORIENTED_EDGE ( 'NONE', *, *, #5018, .F. ) ;
#22710 = COLOUR_RGB ( '', 0.40784314, 0.44705882, 0.49803922) ;
#22711 = B_SPLINE_CURVE_WITH_KNOTS ( 'NONE', 3,
 ( #22518, #9024, #41637, #28133, #9330, #14060, #27517, #17822, #33160, #42264, #37249, #13752, #27829, #51934, #56318, #36946, #56013, #47249, #13132, #41956, #56939, #4299, #3687, #23437, #3081 ),
 .UNSPECIFIED., .F., .F.,
 ( 4, 3, 3, 3, 3, 3, 3, 3, 4 ),
 ( 6.254634441385501517E-18, 0.0005656085177311398569, 0.001131215744874499406, 0.001696821861372766783, 0.002262427090022500319, 0.002828031679238746793, 0.003393635864401604862, 0.003977030878808132490, 0.004561030005651160735 ),
 .UNSPECIFIED. ) ;
#22712 = AXIS2_PLACEMENT_3D ( 'NONE', #53271, #10383, #9436 ) ;
#22713 = EDGE_CURVE ( 'NONE', #23510, #27918, #36788, .T. ) ;
#22714 = DIRECTION ( 'NONE',  ( -1.000000000000000000, -0.000000000000000000, -0.000000000000000000 ) ) ;
#22715 = CARTESIAN_POINT ( 'NONE',  ( -6.015611763856276717, -18.68122482568278286, -2.465697960551244350 ) ) ;
#22716 = CARTESIAN_POINT ( 'NONE',  ( 0.1158816050234199313, -35.36510507486345745, -26.38657583600091527 ) ) ;
#22717 = CARTESIAN_POINT ( 'NONE',  ( 0.5997462898726536595, -39.66574928371219499, -28.95133786038212875 ) ) ;
#22718 = CARTESIAN_POINT ( 'NONE',  ( -2.569797478183790229, -9.259773107243150392, 11.33042594333532271 ) ) ;
#22719 = CARTESIAN_POINT ( 'NONE',  ( 5.959828726073459926, 0.004526594003093787483, 20.52560994243598813 ) ) ;
#22720 = APPLICATION_PROTOCOL_DEFINITION ( 'draft international standard', 'automotive_design', 1998, #21992 ) ;
#22721 = CARTESIAN_POINT ( 'NONE',  ( 0.5817217712918332229, -25.61649477199477332, 39.28142244884644896 ) ) ;
#22722 =( BOUNDED_SURFACE ( )  B_SPLINE_SURFACE ( 3, 1, ( 
 ( #49045, #58117 ),
 ( #53420, #34346 ),
 ( #1409, #1716 ),
 ( #49349, #491 ) ),
 .UNSPECIFIED., .F., .F., .F. ) 
 B_SPLINE_SURFACE_WITH_KNOTS ( ( 4, 4 ),
 ( 2, 2 ),
 ( 0.000000000000000000, 1.000000000000000000 ),
 ( 0.000000000000000000, 1.000000000000000000 ),
 .UNSPECIFIED. ) 
 GEOMETRIC_REPRESENTATION_ITEM ( )  RATIONAL_B_SPLINE_SURFACE ( (
 ( 1.000000000000000000, 1.000000000000000000),
 ( 0.7211978278499968642, 0.9934217856018975334),
 ( 0.7211978278499968642, 0.9934217856018975334),
 ( 1.000000000000000000, 1.000000000000000000) ) ) 
 REPRESENTATION_ITEM ( '' )  SURFACE ( )  );
#22723 = B_SPLINE_CURVE_WITH_KNOTS ( 'NONE', 3,
 ( #27025, #46154, #35206, #35825 ),
 .UNSPECIFIED., .F., .F.,
 ( 4, 4 ),
 ( 0.000000000000000000, 0.005013413432710148512 ),
 .UNSPECIFIED. ) ;
#22724 = CARTESIAN_POINT ( 'NONE',  ( 0.8557997880470690211, -33.22501220301925429, 34.51495345639537504 ) ) ;
#22725 = CARTESIAN_POINT ( 'NONE',  ( 0.3622758884714600280, 33.69533458712307095, 26.89560658783397074 ) ) ;
#22727 = ORIENTED_EDGE ( 'NONE', *, *, #8754, .F. ) ;
#22726 = CARTESIAN_POINT ( 'NONE',  ( 0.6009452777970410997, -46.57942614304348439, -12.02913818029296422 ) ) ;
#22728 = ORIENTED_EDGE ( 'NONE', *, *, #31282, .T. ) ;
#22729 = CARTESIAN_POINT ( 'NONE',  ( 0.1135584504625009039, -7.468331181319575407, 43.48765435731597506 ) ) ;
#22730 = LINE ( 'NONE', #50001, #54776 ) ;
#22731 = ADVANCED_FACE ( 'NONE', ( #31766 ), #36904, .F. ) ;
#22732 = ORIENTED_EDGE ( 'NONE', *, *, #26251, .T. ) ;
#22733 = CARTESIAN_POINT ( 'NONE',  ( 0.5817217712918331118, 22.13702057711616789, 41.34231819790357321 ) ) ;
#22734 = CARTESIAN_POINT ( 'NONE',  ( 0.8744876279028306332, 5.599149760997630842, 48.77498920895230583 ) ) ;
#22735 = CARTESIAN_POINT ( 'NONE',  ( 0.1098349054025746785, 5.840292671757666199, -42.72717686504323353 ) ) ;
#22736 = ORIENTED_EDGE ( 'NONE', *, *, #12964, .T. ) ;
#22737 = ORIENTED_EDGE ( 'NONE', *, *, #8240, .T. ) ;
#22738 = B_SPLINE_CURVE_WITH_KNOTS ( 'NONE', 3,
 ( #24086, #249, #37911, #38513, #14394, #33502 ),
 .UNSPECIFIED., .F., .F.,
 ( 4, 2, 4 ),
 ( 6.946513017424995024E-18, 0.0002291966416970849874, 0.0004583932833941630359 ),
 .UNSPECIFIED. ) ;
#22739 = CARTESIAN_POINT ( 'NONE',  ( 0.9756008150404588131, 41.48296819691553594, 10.96816689273711809 ) ) ;
#22740 = B_SPLINE_CURVE_WITH_KNOTS ( 'NONE', 3,
 ( #35263, #20236, #44667, #49336, #34637, #6388 ),
 .UNSPECIFIED., .F., .F.,
 ( 4, 2, 4 ),
 ( 1.534030753529914427E-16, 0.0002445252820015203824, 0.0004890505640028873502 ),
 .UNSPECIFIED. ) ;
#22741 = CARTESIAN_POINT ( 'NONE',  ( 0.8760168074886965917, 46.22580377597767409, 13.30888447662096929 ) ) ;
#22742 = CARTESIAN_POINT ( 'NONE',  ( 0.9785694773339259633, 33.02736108081276001, -25.79784537034606018 ) ) ;
#22743 = CARTESIAN_POINT ( 'NONE',  ( 3.894904216938897878, -43.89961190414321379, 2.224501549068497841 ) ) ;
#22744 = CARTESIAN_POINT ( 'NONE',  ( 0.6021448801613057400, 48.98911663091443103, 3.406991392652731765 ) ) ;
#22745 = EDGE_CURVE ( 'NONE', #1357, #42003, #52384, .T. ) ;
#22746 = CARTESIAN_POINT ( 'NONE',  ( 0.5997462898726536595, -25.00873172704263325, 42.26245340191598387 ) ) ;
#22747 = AXIS2_PLACEMENT_3D ( 'NONE', #44268, #16050, #5678 ) ;
#22748 = ORIENTED_EDGE ( 'NONE', *, *, #26650, .T. ) ;
#22749 = CARTESIAN_POINT ( 'NONE',  ( 4.834790513006553603, 45.81970208965029201, -11.53881455523394095 ) ) ;
#22750 = FACE_OUTER_BOUND ( 'NONE', #57893, .T. ) ;
#22751 = ORIENTED_EDGE ( 'NONE', *, *, #35132, .T. ) ;
#22752 = CARTESIAN_POINT ( 'NONE',  ( 0.6253024248130503171, -20.50354113282875090, 44.62117242332436717 ) ) ;
#22753 = DIRECTION ( 'NONE',  ( 0.000000000000000000, 0.000000000000000000, -1.000000000000000000 ) ) ;
#22754 = CARTESIAN_POINT ( 'NONE',  ( 4.226256110419178924, 38.48784581281913120, -21.20172103098821736 ) ) ;
#22755 = CARTESIAN_POINT ( 'NONE',  ( 4.967162193818129623, -18.65818244221285127, 38.83676580803761169 ) ) ;
#22756 = VERTEX_POINT ( 'NONE', #61463 ) ;
#22758 = EDGE_CURVE ( 'NONE', #60897, #61018, #31986, .T. ) ;
#22757 = EDGE_LOOP ( 'NONE', ( #46138, #48319, #26068, #31129 ) ) ;
#22759 = CARTESIAN_POINT ( 'NONE',  ( 0.1145239942831223490, -44.12299651911310860, -0.3265867097808889952 ) ) ;
#22760 = CARTESIAN_POINT ( 'NONE',  ( 0.5980271706414711508, -47.32398142236174010, -13.13354579607594275 ) ) ;
#22761 = CARTESIAN_POINT ( 'NONE',  ( 4.956445790443998689, -4.175462451062247560, 46.90526157542890218 ) ) ;
#22762 = ORIENTED_EDGE ( 'NONE', *, *, #34391, .T. ) ;
#22763 = DIRECTION ( 'NONE',  ( 1.000000000000000000, 0.000000000000000000, 0.000000000000000000 ) ) ;
#22764 = ADVANCED_FACE ( 'NONE', ( #41799 ), #17983, .F. ) ;
#22765 = ORIENTED_EDGE ( 'NONE', *, *, #37568, .F. ) ;
#22766 = CARTESIAN_POINT ( 'NONE',  ( 2.533389852662419894, 43.47932600038843276, 6.855562871534678138 ) ) ;
#22767 = CARTESIAN_POINT ( 'NONE',  ( 4.956653778116994147, 39.67974989265076857, -27.17045123668430406 ) ) ;
#22768 = CARTESIAN_POINT ( 'NONE',  ( 0.1158816050234198619, 36.97683962690370407, -24.07603315563850543 ) ) ;
#22769 = ORIENTED_EDGE ( 'NONE', *, *, #59754, .F. ) ;
#22770 = CARTESIAN_POINT ( 'NONE',  ( 0.7242003506639993482, -8.644113737957038524, -48.33519392545445470 ) ) ;
#22771 = CARTESIAN_POINT ( 'NONE',  ( 4.962356264823593044, 12.88441948660167391, 40.06528837230087703 ) ) ;
#22772 = CARTESIAN_POINT ( 'NONE',  ( 3.680882792899938138, 47.28852514876955837, -8.091276083384906670 ) ) ;
#22773 = AXIS2_PLACEMENT_3D ( 'NONE', #58122, #2031, #39995 ) ;
#22774 =( BOUNDED_SURFACE ( )  B_SPLINE_SURFACE ( 3, 1, ( 
 ( #29146, #10360 ),
 ( #58873, #44822 ),
 ( #5926, #35103 ),
 ( #54162, #20988 ) ),
 .UNSPECIFIED., .F., .F., .F. ) 
 B_SPLINE_SURFACE_WITH_KNOTS ( ( 4, 4 ),
 ( 2, 2 ),
 ( 0.000000000000000000, 1.000000000000000000 ),
 ( 0.000000000000000000, 1.000000000000000000 ),
 .UNSPECIFIED. ) 
 GEOMETRIC_REPRESENTATION_ITEM ( )  RATIONAL_B_SPLINE_SURFACE ( (
 ( 1.000000000000000000, 1.000000000000000000),
 ( 0.9732289882329797637, 0.9999525324661233672),
 ( 0.9732289882329797637, 0.9999525324661233672),
 ( 1.000000000000000000, 1.000000000000000000) ) ) 
 REPRESENTATION_ITEM ( '' )  SURFACE ( )  );
#22775 = VERTEX_POINT ( 'NONE', #22983 ) ;
#22776 = CARTESIAN_POINT ( 'NONE',  ( 4.549368137175248350, 0.000000000000000000, 0.000000000000000000 ) ) ;
#22777 = DIRECTION ( 'NONE',  ( 0.000000000000000000, 0.000000000000000000, -1.000000000000000000 ) ) ;
#22778 = CARTESIAN_POINT ( 'NONE',  ( 0.8744876279028263033, -43.20725972823498040, 23.31271664041618052 ) ) ;
#22779 = CARTESIAN_POINT ( 'NONE',  ( 0.6027935024548037868, 47.71838037711334124, -6.106197519200991408 ) ) ;
#22780 = VERTEX_POINT ( 'NONE', #42707 ) ;
#22781 = EDGE_CURVE ( 'NONE', #21489, #3989, #47101, .T. ) ;
#22782 = AXIS2_PLACEMENT_3D ( 'NONE', #43404, #8613, #47469 ) ;
#22783 = CARTESIAN_POINT ( 'NONE',  ( 0.8554163680231816613, -46.74230100997663584, 4.045092014349752851 ) ) ;
#22784 = FACE_OUTER_BOUND ( 'NONE', #21495, .T. ) ;
#22785 = ORIENTED_EDGE ( 'NONE', *, *, #49749, .T. ) ;
#22786 = EDGE_CURVE ( 'NONE', #32724, #37323, #36971, .T. ) ;
#22787 = FACE_OUTER_BOUND ( 'NONE', #8778, .T. ) ;
#22788 = CARTESIAN_POINT ( 'NONE',  ( -6.077587904424778920, -18.27702681447052768, 6.061873655649367088 ) ) ;
#22789 = CARTESIAN_POINT ( 'NONE',  ( 4.549368137175248350, 40.71620287708324781, 13.59764261105765826 ) ) ;
#22790 = CARTESIAN_POINT ( 'NONE',  ( 0.5848930533535030563, 40.44226001967956563, -23.74229742228383344 ) ) ;
#22791 = FACE_OUTER_BOUND ( 'NONE', #36163, .T. ) ;
#22792 = FACE_OUTER_BOUND ( 'NONE', #34074, .T. ) ;
#22793 = CARTESIAN_POINT ( 'NONE',  ( 4.956445790443996913, 7.299064093730984304, 46.52162629890795387 ) ) ;
#22794 = EDGE_CURVE ( 'NONE', #35559, #46325, #46365, .T. ) ;
#22795 =( LENGTH_UNIT ( ) NAMED_UNIT ( * ) SI_UNIT ( .MILLI., .METRE. ) );
#22796 = CARTESIAN_POINT ( 'NONE',  ( 0.1147471544378676628, -12.85192855149397317, -42.21113740448768681 ) ) ;
#22797 =( BOUNDED_SURFACE ( )  B_SPLINE_SURFACE ( 3, 1, ( 
 ( #20345, #592 ),
 ( #14418, #275 ),
 ( #57909, #19730 ),
 ( #5586, #19423 ) ),
 .UNSPECIFIED., .F., .F., .F. ) 
 B_SPLINE_SURFACE_WITH_KNOTS ( ( 4, 4 ),
 ( 2, 2 ),
 ( 0.000000000000000000, 1.000000000000000000 ),
 ( 0.000000000000000000, 1.000000000000000000 ),
 .UNSPECIFIED. ) 
 GEOMETRIC_REPRESENTATION_ITEM ( )  RATIONAL_B_SPLINE_SURFACE ( (
 ( 1.000000000000000000, 1.000000000000000000),
 ( 0.9732289882329797637, 0.9999525324661233672),
 ( 0.9732289882329797637, 0.9999525324661233672),
 ( 1.000000000000000000, 1.000000000000000000) ) ) 
 REPRESENTATION_ITEM ( '' )  SURFACE ( )  );
#22798 = CARTESIAN_POINT ( 'NONE',  ( 0.8551540677456715978, 41.03346287276462334, -24.74404575822732610 ) ) ;
#22799 = CARTESIAN_POINT ( 'NONE',  ( 4.691466044806103852, -43.66525414675648875, 9.025781474740702137 ) ) ;
#22800 = DIRECTION ( 'NONE',  ( 0.1011922191286468292, 0.9018493587347812257, 0.4200331759962346312 ) ) ;
#22801 = ORIENTED_EDGE ( 'NONE', *, *, #19107, .T. ) ;
#22802 = AXIS2_PLACEMENT_3D ( 'NONE', #28320, #47139, #4182 ) ;
#22803 = CARTESIAN_POINT ( 'NONE',  ( 0.8551540677456739292, 23.16399837394546424, 41.94570365541211032 ) ) ;
#22804 = CARTESIAN_POINT ( 'NONE',  ( 0.6846871229502899947, -44.58493949243992915, -17.53234844287788974 ) ) ;
#22805 = CARTESIAN_POINT ( 'NONE',  ( 0.5848930533535030563, 40.44226001967923878, 23.74229742228440898 ) ) ;
#22806 = EDGE_CURVE ( 'NONE', #2408, #53354, #22667, .T. ) ;
#22807 = DIRECTION ( 'NONE',  ( 0.1011922191286468153, 0.5585841627631871198, -0.8232520075274455396 ) ) ;
#22808 = CARTESIAN_POINT ( 'NONE',  ( 0.1064266418746775411, 26.69589626339711685, -33.86837517279519716 ) ) ;
#22809 = CARTESIAN_POINT ( 'NONE',  ( 0.5549461598389361372, 33.00765054922539576, -29.25256742043379532 ) ) ;
#22810 = EDGE_LOOP ( 'NONE', ( #31383, #15800, #22159, #48725 ) ) ;
#22811 = B_SPLINE_CURVE_WITH_KNOTS ( 'NONE', 3,
 ( #9368, #47914, #4641, #23789, #59132, #59762 ),
 .UNSPECIFIED., .F., .F.,
 ( 4, 2, 4 ),
 ( 0.000000000000000000, 0.0002447195606305743666, 0.0004894391212611487333 ),
 .UNSPECIFIED. ) ;
#22812 = CARTESIAN_POINT ( 'NONE',  ( 0.8560838555295223751, -38.14845555156087187, 27.29593693413575295 ) ) ;
#22814 = AXIS2_PLACEMENT_3D ( 'NONE', #5340, #53274, #10388 ) ;
#22813 = CARTESIAN_POINT ( 'NONE',  ( 4.975610109902397937, 47.45567470742089000, 11.84940273605495520 ) ) ;
#22815 = DIRECTION ( 'NONE',  ( 0.000000000000000000, 0.000000000000000000, -1.000000000000000000 ) ) ;
#22816 = ORIENTED_EDGE ( 'NONE', *, *, #60017, .T. ) ;
#22817 = CARTESIAN_POINT ( 'NONE',  ( 4.291220156522060236, -3.725477031302460329, -46.96285572870259273 ) ) ;
#22818 = CONICAL_SURFACE ( 'NONE', #3790, 43.08621763946400307, 1.568696531533066763 ) ;
#22819 = CARTESIAN_POINT ( 'NONE',  ( 0.8744876279028263033, -48.57046782678510510, -7.159588358748426806 ) ) ;
#22820 = ORIENTED_EDGE ( 'NONE', *, *, #47061, .T. ) ;
#22821 = DIRECTION ( 'NONE',  ( 1.000000000000000000, 0.000000000000000000, 0.000000000000000000 ) ) ;
#22822 = AXIS2_PLACEMENT_3D ( 'NONE', #42222, #19024, #22777 ) ;
#22823 = ORIENTED_EDGE ( 'NONE', *, *, #7063, .F. ) ;
#22824 = CARTESIAN_POINT ( 'NONE',  ( 0.9762797500689124330, 20.58271139965541963, -36.50584578699964311 ) ) ;
#22825 = CARTESIAN_POINT ( 'NONE',  ( 4.549368137175248350, -42.84816078363928682, -2.596185425821792236 ) ) ;
#22826 = VERTEX_POINT ( 'NONE', #13902 ) ;
#22827 = CARTESIAN_POINT ( 'NONE',  ( 0.1129192098497447394, -27.13044910148925837, 34.79785222304180081 ) ) ;
#22828 = ORIENTED_EDGE ( 'NONE', *, *, #4066, .F. ) ;
#22829 = LINE ( 'NONE', #61031, #11716 ) ;
#22830 = CARTESIAN_POINT ( 'NONE',  ( -1.114299999999999624, 8.409404640385035208E-16, 6.866799999999992465 ) ) ;
#22831 = EDGE_CURVE ( 'NONE', #33142, #14421, #41156, .T. ) ;
#22832 = ORIENTED_EDGE ( 'NONE', *, *, #16348, .T. ) ;
#22833 = ADVANCED_FACE ( 'NONE', ( #37100 ), #18989, .F. ) ;
#22834 = DIRECTION ( 'NONE',  ( -0.07836865515943411409, -0.2656332009267247662, -0.9608836331491571459 ) ) ;
#22835 = ORIENTED_EDGE ( 'NONE', *, *, #47760, .T. ) ;
#22836 = CARTESIAN_POINT ( 'NONE',  ( 0.8551540677456715978, -28.44084013485144524, 38.56334384152421535 ) ) ;
#22837 = ORIENTED_EDGE ( 'NONE', *, *, #14428, .T. ) ;
#22838 = EDGE_CURVE ( 'NONE', #44393, #18771, #2939, .T. ) ;
#22839 = ORIENTED_EDGE ( 'NONE', *, *, #33544, .F. ) ;
#22840 = CARTESIAN_POINT ( 'NONE',  ( 4.833616638992205949, 45.27110352095233736, 9.466882727842298451 ) ) ;
#22841 = FACE_OUTER_BOUND ( 'NONE', #52448, .T. ) ;
#22842 = CIRCLE ( 'NONE', #23824, 2.649999999999997691 ) ;
#22843 = CARTESIAN_POINT ( 'NONE',  ( -4.467299999999993609, 0.000000000000000000, 0.000000000000000000 ) ) ;
#22844 = CIRCLE ( 'NONE', #61804, 15.71999999999999353 ) ;
#22845 = CARTESIAN_POINT ( 'NONE',  ( 0.1102847568649952675, -16.41780866919068771, 39.87696813145900876 ) ) ;
#22846 = CARTESIAN_POINT ( 'NONE',  ( 4.390527457369401532, -29.29850356886337082, -32.73809745928922865 ) ) ;
#22847 = ORIENTED_EDGE ( 'NONE', *, *, #14134, .T. ) ;
#22848 = CARTESIAN_POINT ( 'NONE',  ( 0.9754402186311941225, 11.28658745892519022, 41.39745964575698878 ) ) ;
#22849 = CARTESIAN_POINT ( 'NONE',  ( 5.895596859100789899, -19.39920506799832722, 5.310275505304355548 ) ) ;
#22850 = CARTESIAN_POINT ( 'NONE',  ( 0.8753041380234465318, 48.36002538446257404, -8.511537621788184182 ) ) ;
#22851 = ORIENTED_EDGE ( 'NONE', *, *, #59385, .T. ) ;
#22852 = VERTEX_POINT ( 'NONE', #61769 ) ;
#22853 = CARTESIAN_POINT ( 'NONE',  ( 0.7242003506639999033, 11.72319998681805409, 47.68205381687218392 ) ) ;
#22854 = DIRECTION ( 'NONE',  ( 0.000000000000000000, 0.000000000000000000, 1.000000000000000000 ) ) ;
#22855 = DIRECTION ( 'NONE',  ( 1.000000000000000000, 0.000000000000000000, 0.000000000000000000 ) ) ;
#22856 = DIRECTION ( 'NONE',  ( -1.000000000000000000, -0.000000000000000000, -0.000000000000000000 ) ) ;
#22857 = B_SPLINE_CURVE_WITH_KNOTS ( 'NONE', 3,
 ( #59846, #36076, #8151, #46089, #3135, #55134, #22263, #12260, #60445, #51055, #27266, #52285, #29111, #32592, #33833, #33214, #47926, #27882, #47010 ),
 .UNSPECIFIED., .F., .F.,
 ( 4, 3, 3, 3, 3, 3, 4 ),
 ( 1.153344816771540786E-16, 0.0002618519381806349699, 0.0003927759815486002036, 0.0005237000248299497184, 0.0006546240681325027040, 0.0007855481115631361786, 0.0009699050456655135440 ),
 .UNSPECIFIED. ) ;
#22858 = CARTESIAN_POINT ( 'NONE',  ( 0.6001305935487422083, 41.40054608060292907, -24.50730504006414634 ) ) ;
#22859 = EDGE_CURVE ( 'NONE', #1548, #21722, #40384, .T. ) ;
#22860 = AXIS2_PLACEMENT_3D ( 'NONE', #45094, #60682, #59453 ) ;
#22861 = VERTEX_POINT ( 'NONE', #4750 ) ;
#22862 = CARTESIAN_POINT ( 'NONE',  ( 0.5837374860065648319, 47.50965286059334858, 6.071555045024764397 ) ) ;
#22863 = ADVANCED_FACE ( 'NONE', ( #52647 ), #29162, .F. ) ;
#22864 = CARTESIAN_POINT ( 'NONE',  ( 1.157643937452368599, -16.89177053992790789, 38.36235606191540626 ) ) ;
#22866 = B_SPLINE_CURVE_WITH_KNOTS ( 'NONE', 3,
 ( #44414, #7369, #1751, #30574, #20885, #35621 ),
 .UNSPECIFIED., .F., .F.,
 ( 4, 2, 4 ),
 ( 1.208227429106116496E-16, 0.0002448718616795937469, 0.0004897437233590666052 ),
 .UNSPECIFIED. ) ;
#22865 = CARTESIAN_POINT ( 'NONE',  ( 49.81163791968438659, 15.28633307723669077, 2.564998524509804145 ) ) ;
#22867 = DIRECTION ( 'NONE',  ( 0.000000000000000000, 0.000000000000000000, 1.000000000000000000 ) ) ;
#22868 = CARTESIAN_POINT ( 'NONE',  ( 1.112077966505211402, -43.57125842763898760, 6.676508380916812868 ) ) ;
#22869 = EDGE_CURVE ( 'NONE', #24288, #26981, #4906, .T. ) ;
#22870 =( NAMED_UNIT ( * ) PLANE_ANGLE_UNIT ( ) SI_UNIT ( $, .RADIAN. ) );
#22871 = MECHANICAL_DESIGN_GEOMETRIC_PRESENTATION_REPRESENTATION (  '', ( #49872 ), #60856 ) ;
#22872 = ORIENTED_EDGE ( 'NONE', *, *, #28790, .T. ) ;
#22873 = CARTESIAN_POINT ( 'NONE',  ( 0.9730545539215883499, 21.89037132892487847, -36.90443313492307453 ) ) ;
#22874 = DIRECTION ( 'NONE',  ( 0.000000000000000000, 0.000000000000000000, 1.000000000000000000 ) ) ;
#22875 =( BOUNDED_SURFACE ( )  B_SPLINE_SURFACE ( 3, 1, ( 
 ( #4076, #47331 ),
 ( #9725, #18519 ),
 ( #18215, #18842 ),
 ( #56095, #37965 ) ),
 .UNSPECIFIED., .F., .F., .F. ) 
 B_SPLINE_SURFACE_WITH_KNOTS ( ( 4, 4 ),
 ( 2, 2 ),
 ( 0.000000000000000000, 1.000000000000000000 ),
 ( 0.000000000000000000, 1.000000000000000000 ),
 .UNSPECIFIED. ) 
 GEOMETRIC_REPRESENTATION_ITEM ( )  RATIONAL_B_SPLINE_SURFACE ( (
 ( 1.000000000000000000, 1.000000000000000000),
 ( 0.9953390228620291325, 0.8624445117760984880),
 ( 0.9953390228620291325, 0.8624445117760984880),
 ( 1.000000000000000000, 1.000000000000000000) ) ) 
 REPRESENTATION_ITEM ( '' )  SURFACE ( )  );
#22876 = CARTESIAN_POINT ( 'NONE',  ( -6.010958268070873523, -9.409153349053701376, 16.32616437357108907 ) ) ;
#22877 = CARTESIAN_POINT ( 'NONE',  ( 0.1073791018717578927, 21.98088480513665388, -37.10214135362866728 ) ) ;
#22878 = VECTOR ( 'NONE', #30794, 1000.000000000000000 ) ;
#22879 = CARTESIAN_POINT ( 'NONE',  ( -6.077587904424778920, 0.6233693561568425245, 19.24597183931575373 ) ) ;
#22880 = DIRECTION ( 'NONE',  ( 0.000000000000000000, 3.491481338843138088E-15, -1.000000000000000000 ) ) ;
#22881 = EDGE_CURVE ( 'NONE', #51544, #34106, #13517, .T. ) ;
#22882 = DIRECTION ( 'NONE',  ( 0.1011922191286468015, 0.2088217057275386090, -0.9727042870291366938 ) ) ;
#22883 = CARTESIAN_POINT ( 'NONE',  ( 3.238018933889920792, 9.111992562714036126, 9.817284955867229712 ) ) ;
#22884 = B_SPLINE_CURVE_WITH_KNOTS ( 'NONE', 3,
 ( #3781, #16996, #36727, #54864 ),
 .UNSPECIFIED., .F., .F.,
 ( 4, 4 ),
 ( 1.301042606982605321E-18, 0.004041751736740994277 ),
 .UNSPECIFIED. ) ;
#22885 = B_SPLINE_CURVE_WITH_KNOTS ( 'NONE', 3,
 ( #41720, #3456, #28503, #47631 ),
 .UNSPECIFIED., .F., .F.,
 ( 4, 4 ),
 ( 0.000000000000000000, 0.005004741218457452699 ),
 .UNSPECIFIED. ) ;
#22886 = ADVANCED_FACE ( 'NONE', ( #38905 ), #29728, .F. ) ;
#22887 = CARTESIAN_POINT ( 'NONE',  ( 2.678494666091051357, 3.072372537026354156, -0.03421028094653023183 ) ) ;
#22888 = AXIS2_PLACEMENT_3D ( 'NONE', #52991, #10094, #5362 ) ;
#22889 = ORIENTED_EDGE ( 'NONE', *, *, #46774, .F. ) ;
#22890 = AXIS2_PLACEMENT_3D ( 'NONE', #389, #52720, #38655 ) ;
#22891 = CARTESIAN_POINT ( 'NONE',  ( 0.1129192098497447394, -6.563350895509266536, 43.63340707310824484 ) ) ;
#22892 = CARTESIAN_POINT ( 'NONE',  ( 1.834102595619085729, 24.12078293692350428, -36.85628271227993480 ) ) ;
#22893 = DIRECTION ( 'NONE',  ( 1.000000000000000000, 0.000000000000000000, 0.000000000000000000 ) ) ;
#22894 = CARTESIAN_POINT ( 'NONE',  ( 0.8551540677456739292, 41.94570365541235191, -23.16399837394502725 ) ) ;
#22895 = ORIENTED_EDGE ( 'NONE', *, *, #38677, .T. ) ;
#22896 =( BOUNDED_SURFACE ( )  B_SPLINE_SURFACE ( 3, 1, ( 
 ( #53318, #48330 ),
 ( #43039, #47718 ),
 ( #701, #33937 ),
 ( #37725, #10117 ) ),
 .UNSPECIFIED., .F., .F., .F. ) 
 B_SPLINE_SURFACE_WITH_KNOTS ( ( 4, 4 ),
 ( 2, 2 ),
 ( 0.000000000000000000, 1.000000000000000000 ),
 ( 0.000000000000000000, 1.000000000000000000 ),
 .UNSPECIFIED. ) 
 GEOMETRIC_REPRESENTATION_ITEM ( )  RATIONAL_B_SPLINE_SURFACE ( (
 ( 1.000000000000000000, 1.000000000000000000),
 ( 0.7282232189291694135, 0.9929344683865672927),
 ( 0.7282232189291694135, 0.9929344683865672927),
 ( 1.000000000000000000, 1.000000000000000000) ) ) 
 REPRESENTATION_ITEM ( '' )  SURFACE ( )  );
#22897 = CARTESIAN_POINT ( 'NONE',  ( 0.5800708119828337228, 46.09746484493497576, -13.00144522946610515 ) ) ;
#22898 = CARTESIAN_POINT ( 'NONE',  ( 0.9790724872846782167, -41.81234597974636102, -2.839530533634436527 ) ) ;
#22899 = B_SPLINE_CURVE_WITH_KNOTS ( 'NONE', 3,
 ( #10919, #30004, #20313, #5861, #49115, #48491 ),
 .UNSPECIFIED., .F., .F.,
 ( 4, 2, 4 ),
 ( 1.495080201624372079E-16, 0.0002445252820015202740, 0.0004890505640028910365 ),
 .UNSPECIFIED. ) ;
#22900 =( NAMED_UNIT ( * ) PLANE_ANGLE_UNIT ( ) SI_UNIT ( $, .RADIAN. ) );
#22901 = ORIENTED_EDGE ( 'NONE', *, *, #51226, .T. ) ;
#22902 = CARTESIAN_POINT ( 'NONE',  ( 4.956653778116991482, -2.599733001514001440, -48.02038484091103498 ) ) ;
#22903 = DIRECTION ( 'NONE',  ( 0.000000000000000000, 0.000000000000000000, 1.000000000000000000 ) ) ;
#22904 = CARTESIAN_POINT ( 'NONE',  ( 4.549368137175248350, -8.166781970325423856, -42.14271863032831078 ) ) ;
#22905 = ORIENTED_EDGE ( 'NONE', *, *, #5204, .T. ) ;
#22906 = DIRECTION ( 'NONE',  ( -0.07836865515943411409, -0.9179910502197385913, 0.3887811538706100745 ) ) ;
#22907 = AXIS2_PLACEMENT_3D ( 'NONE', #28033, #47448, #9526 ) ;
#22908 = ORIENTED_EDGE ( 'NONE', *, *, #43419, .T. ) ;
#22909 = EDGE_LOOP ( 'NONE', ( #39283, #29471, #52803, #14220 ) ) ;
#22910 = CARTESIAN_POINT ( 'NONE',  ( 0.5809828226811617480, -5.711058609464997105, -47.55412398569212939 ) ) ;
#22911 = CARTESIAN_POINT ( 'NONE',  ( 4.549368137175248350, 0.000000000000000000, 0.000000000000000000 ) ) ;
#22912 = EDGE_CURVE ( 'NONE', #59245, #30839, #53565, .T. ) ;
#22913 = VERTEX_POINT ( 'NONE', #1564 ) ;
#22914 = FACE_OUTER_BOUND ( 'NONE', #34724, .T. ) ;
#22915 = ORIENTED_EDGE ( 'NONE', *, *, #10005, .F. ) ;
#22916 = EDGE_CURVE ( 'NONE', #51439, #46801, #32152, .T. ) ;
#22917 = CARTESIAN_POINT ( 'NONE',  ( -6.001507490154111224, 16.31148204059947204, 9.435425682280875748 ) ) ;
#22918 = AXIS2_PLACEMENT_3D ( 'NONE', #6117, #829, #11170 ) ;
#22919 = CARTESIAN_POINT ( 'NONE',  ( 0.8751705887134423323, 48.08707113907594533, 0.8911681664090089772 ) ) ;
#22920 = CARTESIAN_POINT ( 'NONE',  ( 0.7242003506640004584, 40.69931820417237844, -27.46956810438689800 ) ) ;
#22921 = EDGE_CURVE ( 'NONE', #17913, #46201, #41977, .T. ) ;
#22922 = EDGE_LOOP ( 'NONE', ( #12293, #55597, #26307, #57638 ) ) ;
#22923 = EDGE_CURVE ( 'NONE', #34886, #59557, #59086, .T. ) ;
#22924 = DIRECTION ( 'NONE',  ( -1.000000000000000000, -0.000000000000000000, -0.000000000000000000 ) ) ;
#22925 = CARTESIAN_POINT ( 'NONE',  ( 2.648799415243708655, -47.76469914295812913, -11.09283458239118580 ) ) ;
#22926 = CARTESIAN_POINT ( 'NONE',  ( 4.691466044806103852, 44.46979273209135641, -3.249105306917955627 ) ) ;
#22927 = CARTESIAN_POINT ( 'NONE',  ( 0.8560838555295223751, 46.89922841446243496, -0.9138972643637069959 ) ) ;
#22929 = EDGE_CURVE ( 'NONE', #15738, #36038, #35935, .T. ) ;
#22928 = ORIENTED_EDGE ( 'NONE', *, *, #6123, .F. ) ;
#22930 = CARTESIAN_POINT ( 'NONE',  ( 4.975801465491694664, -31.15993731089097452, -36.39623109580456628 ) ) ;
#22931 = CARTESIAN_POINT ( 'NONE',  ( 5.894904586330512508, 14.91761050190863003, -13.49052663816309661 ) ) ;
#22932 = ORIENTED_EDGE ( 'NONE', *, *, #33275, .T. ) ;
#22933 = CARTESIAN_POINT ( 'NONE',  ( 0.9749527285493307938, -42.90750796893248520, -0.2856147164663118132 ) ) ;
#22934 = ORIENTED_EDGE ( 'NONE', *, *, #6875, .F. ) ;
#22935 = CARTESIAN_POINT ( 'NONE',  ( 1.827119703190779765, -6.838980420687682305, -42.50321986945166230 ) ) ;
#22936 = ADVANCED_FACE ( 'NONE', ( #26014 ), #58077, .F. ) ;
#22937 = CARTESIAN_POINT ( 'NONE',  ( 0.8551540677456715978, -23.16399837394516581, -41.94570365541226664 ) ) ;
#22938 = VERTEX_POINT ( 'NONE', #2179 ) ;
#22939 = CARTESIAN_POINT ( 'NONE',  ( 0.5830081025819923157, 4.965830163467174430, 46.63231245788532675 ) ) ;
#22940 = CARTESIAN_POINT ( 'NONE',  ( 4.956653778116949738, -36.51451553856396970, -31.29546495791881000 ) ) ;
#22941 = CARTESIAN_POINT ( 'NONE',  ( 0.5998501479064708430, 47.76154736470757456, -5.759754759340284913 ) ) ;
#22942 = CARTESIAN_POINT ( 'NONE',  ( 0.5806925824938499181, -1.020860314012482561, -46.88475452172953339 ) ) ;
#22943 = AXIS2_PLACEMENT_3D ( 'NONE', #20512, #7865, #31374 ) ;
#22944 = ORIENTED_EDGE ( 'NONE', *, *, #1727, .T. ) ;
#22945 = CARTESIAN_POINT ( 'NONE',  ( 1.154321485836933281, 41.66001465002027970, 10.30834589251726285 ) ) ;
#22946 = FACE_OUTER_BOUND ( 'NONE', #60230, .T. ) ;
#22947 = CARTESIAN_POINT ( 'NONE',  ( 5.959547316686252039, -12.49238070347965035, -16.28624005235095495 ) ) ;
#22948 = CARTESIAN_POINT ( 'NONE',  ( 0.6001305935487422083, -47.76436356026972163, 5.760103278697227935 ) ) ;
#22949 = CARTESIAN_POINT ( 'NONE',  ( 0.9730545539215883499, 42.60426903087353878, 5.099196237955034405 ) ) ;
#22950 = DIRECTION ( 'NONE',  ( -1.000000000000000000, -0.000000000000000000, -0.000000000000000000 ) ) ;
#22951 = CARTESIAN_POINT ( 'NONE',  ( 0.5819845079324655890, -46.14435090135486206, 12.83441846783114570 ) ) ;
#22952 = CARTESIAN_POINT ( 'NONE',  ( 0.5998501479064708430, 38.48283596222029956, -28.86886762351084812 ) ) ;
#22953 = VECTOR ( 'NONE', #25625, 1000.000000000000114 ) ;
#22954 = CARTESIAN_POINT ( 'NONE',  ( 0.9762797500689124330, -12.89881610234976961, 39.87411852747928265 ) ) ;
#22955 = CARTESIAN_POINT ( 'NONE',  ( 2.526552050251864134, 6.809858322089650251, -42.43615142762118353 ) ) ;
#22956 = FACE_OUTER_BOUND ( 'NONE', #32450, .T. ) ;
#22957 = EDGE_CURVE ( 'NONE', #51700, #6891, #27710, .T. ) ;
#22958 = CARTESIAN_POINT ( 'NONE',  ( 4.322998006666179727, 16.38761975793208947, -45.10383234877016889 ) ) ;
#22959 = CARTESIAN_POINT ( 'NONE',  ( -6.016761891674565099, -11.46828378093549361, -14.95139917749716041 ) ) ;
#22960 = CARTESIAN_POINT ( 'NONE',  ( 4.967162193818130511, 43.02067033766019932, -2.375726030842729486 ) ) ;
#22961 = CARTESIAN_POINT ( 'NONE',  ( 2.879087469061463622, -21.31151173680148503, 38.49572890952385507 ) ) ;
#22962 = CARTESIAN_POINT ( 'NONE',  ( 0.7056313189692764443, 42.84374994564657868, -19.08302215458729023 ) ) ;
#22963 = EDGE_CURVE ( 'NONE', #44029, #15738, #26143, .T. ) ;
#22964 = CARTESIAN_POINT ( 'NONE',  ( 0.9749527285493325701, -37.01618455594557133, -21.70110358462078182 ) ) ;
#22965 = CARTESIAN_POINT ( 'NONE',  ( 4.975801465491695552, 9.906103548667566372, 46.87746200127460128 ) ) ;
#22966 = CARTESIAN_POINT ( 'NONE',  ( 0.6008123274975392114, -47.61009137730950158, 12.03468945185942651 ) ) ;
#22967 = ORIENTED_EDGE ( 'NONE', *, *, #38713, .F. ) ;
#22968 = ORIENTED_EDGE ( 'NONE', *, *, #24500, .T. ) ;
#22969 = CARTESIAN_POINT ( 'NONE',  ( 0.5997462898726536595, -39.66574928371259290, 28.95133786038155321 ) ) ;
#22970 = CARTESIAN_POINT ( 'NONE',  ( 0.5809828226811553087, 24.41822904836923058, 41.20389530892317254 ) ) ;
#22971 = DIRECTION ( 'NONE',  ( 0.09722883295013592941, 0.6635018476521751252, -0.7418300696286881379 ) ) ;
#22972 = ORIENTED_EDGE ( 'NONE', *, *, #38218, .F. ) ;
#22973 = EDGE_LOOP ( 'NONE', ( #11127, #23838, #33345, #30199 ) ) ;
#22974 = CARTESIAN_POINT ( 'NONE',  ( 0.5832367798473377940, -34.05962365606842468, 33.67436043247250410 ) ) ;
#22975 = CARTESIAN_POINT ( 'NONE',  ( 1.231276596079881935, -39.31472542100197387, -14.54747868495734053 ) ) ;
#22976 =( BOUNDED_SURFACE ( )  B_SPLINE_SURFACE ( 3, 1, ( 
 ( #32972, #61736 ),
 ( #37993, #33581 ),
 ( #52658, #57045 ),
 ( #52350, #42993 ) ),
 .UNSPECIFIED., .F., .F., .F. ) 
 B_SPLINE_SURFACE_WITH_KNOTS ( ( 4, 4 ),
 ( 2, 2 ),
 ( 0.000000000000000000, 1.000000000000000000 ),
 ( 0.000000000000000000, 1.000000000000000000 ),
 .UNSPECIFIED. ) 
 GEOMETRIC_REPRESENTATION_ITEM ( )  RATIONAL_B_SPLINE_SURFACE ( (
 ( 1.000000000000000000, 1.000000000000000000),
 ( 0.9729067724841187204, 0.9999501103223794596),
 ( 0.9729067724841187204, 0.9999501103223794596),
 ( 1.000000000000000000, 1.000000000000000000) ) ) 
 REPRESENTATION_ITEM ( '' )  SURFACE ( )  );
#22977 = UNCERTAINTY_MEASURE_WITH_UNIT (LENGTH_MEASURE( 1.000000000000000082E-05 ), #55629, 'distance_accuracy_value', 'NONE');
#22978 = VECTOR ( 'NONE', #59240, 1000.000000000000114 ) ;
#22979 = VERTEX_POINT ( 'NONE', #59199 ) ;
#22980 = EDGE_LOOP ( 'NONE', ( #55773, #20747, #46954, #44261 ) ) ;
#22981 = CARTESIAN_POINT ( 'NONE',  ( 0.6025881611877910160, -38.03302298778322665, -29.45877655626779656 ) ) ;
#22982 = VECTOR ( 'NONE', #54860, 1000.000000000000000 ) ;
#22983 = CARTESIAN_POINT ( 'NONE',  ( 1.399999999999998579, 9.184850993605177527E-16, 7.500000000000022204 ) ) ;
#22984 = CARTESIAN_POINT ( 'NONE',  ( 4.975610109902397937, 48.90928568712960356, 0.5754830253899292369 ) ) ;
#22985 = ORIENTED_EDGE ( 'NONE', *, *, #36962, .T. ) ;
#22986 = ORIENTED_EDGE ( 'NONE', *, *, #8686, .T. ) ;
#22987 = DIRECTION ( 'NONE',  ( 1.000000000000000000, 0.000000000000000000, 0.000000000000000000 ) ) ;
#22988 = ORIENTED_EDGE ( 'NONE', *, *, #23615, .T. ) ;
#22989 = CARTESIAN_POINT ( 'NONE',  ( 0.2885700199627520002, 15.75356883787153528, -40.13549263616307883 ) ) ;
#22990 = CARTESIAN_POINT ( 'NONE',  ( 4.553261556744873317, -14.95853073564509828, 41.30111286702087625 ) ) ;
#22991 = CARTESIAN_POINT ( 'NONE',  ( 2.299746137290199943, -31.56858058830529146, -37.51940907484834753 ) ) ;
#22992 = VERTEX_POINT ( 'NONE', #49815 ) ;
#22993 = EDGE_CURVE ( 'NONE', #13851, #23055, #2275, .T. ) ;
#22994 = CARTESIAN_POINT ( 'NONE',  ( 0.6009453534118439633, -48.10564080474284765, -0.4363813339956353898 ) ) ;
#22995 = EDGE_CURVE ( 'NONE', #1858, #31453, #6906, .T. ) ;
#22996 = ORIENTED_EDGE ( 'NONE', *, *, #889, .T. ) ;
#22997 = ORIENTED_EDGE ( 'NONE', *, *, #55972, .T. ) ;
#22998 = EDGE_CURVE ( 'NONE', #14276, #58372, #728, .T. ) ;
#22999 = CARTESIAN_POINT ( 'NONE',  ( 0.5980271706414734822, -0.8742700727941912220, 49.10483575658797406 ) ) ;
#23000 = ORIENTED_EDGE ( 'NONE', *, *, #53462, .F. ) ;
#23001 = CARTESIAN_POINT ( 'NONE',  ( 0.9268187852002115479, 34.20493226694245692, 27.81684636191718241 ) ) ;
#23002 = FACE_OUTER_BOUND ( 'NONE', #61271, .T. ) ;
#23003 = CARTESIAN_POINT ( 'NONE',  ( 2.281448460670563616, 38.84544723616143358, 28.15071835136410883 ) ) ;
#23004 = EDGE_CURVE ( 'NONE', #24004, #3087, #40446, .T. ) ;
#23005 = CARTESIAN_POINT ( 'NONE',  ( 0.8744876279028306332, 16.11801507201633399, -46.37412684372340266 ) ) ;
#23006 = CARTESIAN_POINT ( 'NONE',  ( -69.95594261585600293, 0.000000000000000000, 0.000000000000000000 ) ) ;
#23007 = VERTEX_POINT ( 'NONE', #50727 ) ;
#23008 = CARTESIAN_POINT ( 'NONE',  ( 0.8753041380234471980, -31.30612550145435335, 37.82941757363136048 ) ) ;
#23009 = CARTESIAN_POINT ( 'NONE',  ( 0.8560838555295223751, 16.00311602465208694, -44.09391240957481273 ) ) ;
#23010 = B_SPLINE_CURVE_WITH_KNOTS ( 'NONE', 3,
 ( #1440, #52534, #53747, #9628, #24041, #57843 ),
 .UNSPECIFIED., .F., .F.,
 ( 4, 2, 4 ),
 ( 1.527179101177669750E-16, 0.0002445252820015209245, 0.0004890505640028891933 ),
 .UNSPECIFIED. ) ;
#23011 = B_SPLINE_CURVE_WITH_KNOTS ( 'NONE', 3,
 ( #48393, #16423, #24590, #19914, #39025, #29279, #58080, #29587, #53382, #44043, #48699, #39321, #59011, #11118, #6063, #6364 ),
 .UNSPECIFIED., .F., .F.,
 ( 4, 3, 3, 3, 3, 4 ),
 ( 2.501947744657918636E-17, 0.0002618515315864388868, 0.0003927756766341969612, 0.0005236998216950529026, 0.0007855159896329866462, 0.001047349442285926135 ),
 .UNSPECIFIED. ) ;
#23012 = CARTESIAN_POINT ( 'NONE',  ( 0.1073791018717483448, 39.65380858626214433, -16.95003405440273525 ) ) ;
#23013 = VERTEX_POINT ( 'NONE', #55120 ) ;
#23014 = CARTESIAN_POINT ( 'NONE',  ( 0.5786265663353153954, -18.99608782658000905, -43.97352617418637521 ) ) ;
#23015 = FACE_OUTER_BOUND ( 'NONE', #3493, .T. ) ;
#23016 = CARTESIAN_POINT ( 'NONE',  ( 0.9745511491811750249, 30.09905547141354276, 30.58068216140344120 ) ) ;
#23017 = FACE_OUTER_BOUND ( 'NONE', #42504, .T. ) ;
#23018 = EDGE_CURVE ( 'NONE', #50394, #37784, #49328, .T. ) ;
#23019 = ORIENTED_EDGE ( 'NONE', *, *, #12447, .F. ) ;
#23020 = CARTESIAN_POINT ( 'NONE',  ( 4.335381028904201628, -44.56680861641509495, -20.33608658056349228 ) ) ;
#23021 = CARTESIAN_POINT ( 'NONE',  ( -6.016489644550736315, 18.84320342686341121, -0.004404229197841518298 ) ) ;
#23022 = CARTESIAN_POINT ( 'NONE',  ( 4.549368137175248350, -42.14271863032827525, -8.166781970325585505 ) ) ;
#23023 = CARTESIAN_POINT ( 'NONE',  ( -1.660531772554312280, 3.660093687634848436, 2.744386749103932310E-15 ) ) ;
#23024 = CARTESIAN_POINT ( 'NONE',  ( 0.3676999524040323597, -38.83470403830501994, 20.92406140260764857 ) ) ;
#23025 = SURFACE_STYLE_USAGE ( .BOTH. , #48059 ) ;
#23026 = CARTESIAN_POINT ( 'NONE',  ( 0.8551540677456715978, 11.51835730326544649, -46.51172240253109180 ) ) ;
#23027 = CARTESIAN_POINT ( 'NONE',  ( 0.3622758884714600280, 42.84426538328730771, -4.808133778521432866 ) ) ;
#23028 = CARTESIAN_POINT ( 'NONE',  ( 1.154321713695929175, -22.16897764010631633, 36.74718012229649844 ) ) ;
#23029 = CARTESIAN_POINT ( 'NONE',  ( 0.1119898979215349921, -22.39193976382053819, 38.02055157234389071 ) ) ;
#23030 = CARTESIAN_POINT ( 'NONE',  ( 0.5807400328401574052, -24.41979442053140303, -41.20655774452995246 ) ) ;
#23031 = VERTEX_POINT ( 'NONE', #58890 ) ;
#23032 = B_SPLINE_CURVE_WITH_KNOTS ( 'NONE', 3,
 ( #46082, #41084, #16952, #50739, #36672, #17555 ),
 .UNSPECIFIED., .F., .F.,
 ( 4, 2, 4 ),
 ( 1.266058488688919593E-17, 0.0002448709889506565061, 0.0004897419779013003271 ),
 .UNSPECIFIED. ) ;
#23033 = CYLINDRICAL_SURFACE ( 'NONE', #54897, 0.7500000000000015543 ) ;
#23034 = FACE_OUTER_BOUND ( 'NONE', #43648, .T. ) ;
#23035 = B_SPLINE_CURVE_WITH_KNOTS ( 'NONE', 3,
 ( #23605, #51172, #28303, #47420 ),
 .UNSPECIFIED., .F., .F.,
 ( 4, 4 ),
 ( 5.553824967135426632E-18, 0.004566006591234645501 ),
 .UNSPECIFIED. ) ;
#23036 = CARTESIAN_POINT ( 'NONE',  ( 2.299746137290199055, 9.651167162349302941, -48.07427909070013783 ) ) ;
#23037 = CARTESIAN_POINT ( 'NONE',  ( 4.553261556744873317, -24.94552653848474222, 36.15605442441679429 ) ) ;
#23038 = CARTESIAN_POINT ( 'NONE',  ( 0.1100247026804066219, 42.73303500775678998, 5.797046384220007731 ) ) ;
#23039 = FACE_OUTER_BOUND ( 'NONE', #50184, .T. ) ;
#23040 = EDGE_CURVE ( 'NONE', #16730, #21951, #47140, .T. ) ;
#23041 = CARTESIAN_POINT ( 'NONE',  ( 58.00000000000000000, 8.437969416220405915E-15, -2.995852231480068572E-16 ) ) ;
#23042 = DIRECTION ( 'NONE',  ( -1.000000000000000000, -0.000000000000000000, -0.000000000000000000 ) ) ;
#23044 = EDGE_LOOP ( 'NONE', ( #19691, #9159 ) ) ;
#23043 = CARTESIAN_POINT ( 'NONE',  ( 1.154321485836933725, -36.74718014677581834, 22.16897757994461671 ) ) ;
#23045 = ORIENTED_EDGE ( 'NONE', *, *, #16560, .T. ) ;
#23046 = AXIS2_PLACEMENT_3D ( 'NONE', #3435, #37299, #22880 ) ;
#23047 = CARTESIAN_POINT ( 'NONE',  ( 0.5800708119828332787, -37.61306658477494125, 29.65250521075930834 ) ) ;
#23048 = LINE ( 'NONE', #42781, #3461 ) ;
#23049 = CARTESIAN_POINT ( 'NONE',  ( 2.624215991343608501, 32.93378783738849336, 34.92983774302978617 ) ) ;
#23050 = ORIENTED_EDGE ( 'NONE', *, *, #53645, .T. ) ;
#23051 = CARTESIAN_POINT ( 'NONE',  ( 0.6008123274975391004, 11.35154294343716863, -47.77757867412034898 ) ) ;
#23052 = CARTESIAN_POINT ( 'NONE',  ( -90.00000000000000000, 0.000000000000000000, 0.000000000000000000 ) ) ;
#23053 = CARTESIAN_POINT ( 'NONE',  ( 0.6009453534118440743, -44.27682103112819334, -18.81239552212969457 ) ) ;
#23054 = B_SPLINE_CURVE_WITH_KNOTS ( 'NONE', 3,
 ( #56359, #37602, #3733, #4643, #42302, #13173, #37289, #51974, #8143, #42919, #18796, #32584, #51353, #52276, #47600, #9066, #37922, #8758, #38223, #61971, #56978, #19110, #47289, #13794, #28173 ),
 .UNSPECIFIED., .F., .F.,
 ( 4, 3, 3, 3, 3, 3, 3, 3, 4 ),
 ( 6.254634441385501517E-18, 0.0005656085177311386642, 0.001131215744874498972, 0.001696821861372766350, 0.002262427090022497717, 0.002828031679238744624, 0.003393635864401602694, 0.003977030878808130755, 0.004561030005651157265 ),
 .UNSPECIFIED. ) ;
#23055 = VERTEX_POINT ( 'NONE', #18787 ) ;
#23056 = EDGE_LOOP ( 'NONE', ( #30708, #53711, #25845, #7005 ) ) ;
#23057 = CARTESIAN_POINT ( 'NONE',  ( 0.9745511491811748028, 41.35688774886286723, 11.43411988112617372 ) ) ;
#23058 = CARTESIAN_POINT ( 'NONE',  ( 0.7413678028165006095, 37.45741361428792970, 23.26861098343432843 ) ) ;
#23059 = DIRECTION ( 'NONE',  ( 0.000000000000000000, -0.7071067811865449082, -0.7071067811865500152 ) ) ;
#23060 = CARTESIAN_POINT ( 'NONE',  ( -7.459310946700270506E-14, -4.618802153517020948, -5.242734410091827613 ) ) ;
#23061 = CARTESIAN_POINT ( 'NONE',  ( 0.6026112563231247332, 48.99508032062211527, 3.320105311582033814 ) ) ;
#23062 = EDGE_CURVE ( 'NONE', #19953, #38564, #58922, .T. ) ;
#23063 = CARTESIAN_POINT ( 'NONE',  ( 0.9730545539215883499, 41.57420493492400482, -10.61654491617520080 ) ) ;
#23064 = EDGE_CURVE ( 'NONE', #1029, #39188, #38001, .T. ) ;
#23065 = ORIENTED_EDGE ( 'NONE', *, *, #35663, .T. ) ;
#23066 = CIRCLE ( 'NONE', #1044, 42.92674063221959813 ) ;
#23067 = CARTESIAN_POINT ( 'NONE',  ( 3.661933894777876120, -33.59527226767167463, -32.92398587979079849 ) ) ;
#23068 = ORIENTED_EDGE ( 'NONE', *, *, #12109, .F. ) ;
#23069 = DIRECTION ( 'NONE',  ( 0.1736481776669314969, -0.9848077530122079093, -4.496403249731880833E-15 ) ) ;
#23070 = FACE_OUTER_BOUND ( 'NONE', #19135, .T. ) ;
#23071 = EDGE_CURVE ( 'NONE', #19824, #21951, #32892, .T. ) ;
#23072 = CARTESIAN_POINT ( 'NONE',  ( 0.6064782688330857541, 46.37855233655766796, 6.954446748947744616 ) ) ;
#23073 = DIRECTION ( 'NONE',  ( -0.000000000000000000, 1.000000000000000000, -0.000000000000000000 ) ) ;
#23074 = ORIENTED_EDGE ( 'NONE', *, *, #26576, .F. ) ;
#23075 = ORIENTED_EDGE ( 'NONE', *, *, #34113, .T. ) ;
#23076 = CARTESIAN_POINT ( 'NONE',  ( 0.9752132459055842251, 0.2329632697543913833, 42.90780255730426518 ) ) ;
#23077 = FACE_OUTER_BOUND ( 'NONE', #277, .T. ) ;
#23078 = CARTESIAN_POINT ( 'NONE',  ( -6.078726893082806448, -6.647148524917478873, -18.07233957617019371 ) ) ;
#23079 = AXIS2_PLACEMENT_3D ( 'NONE', #48868, #941, #52942 ) ;
#23080 = VERTEX_POINT ( 'NONE', #41369 ) ;
#23081 = CARTESIAN_POINT ( 'NONE',  ( 5.960721111146673579, -12.49016043756483363, 16.28787783074205819 ) ) ;
#23082 = EDGE_LOOP ( 'NONE', ( #43201, #1103, #24743, #17646 ) ) ;
#23083 = CARTESIAN_POINT ( 'NONE',  ( 4.390527457369401532, 43.53099151023969426, 5.936170041707031331 ) ) ;
#23084 = CARTESIAN_POINT ( 'NONE',  ( 6.999999999999995559, 54.69470952477936976, 58.44237546506825964 ) ) ;
#23085 = EDGE_CURVE ( 'NONE', #33072, #55726, #10974, .T. ) ;
#23086 = CARTESIAN_POINT ( 'NONE',  ( 4.549368137175248350, 28.46244473166673927, -32.13400537129894730 ) ) ;
#23087 = ORIENTED_EDGE ( 'NONE', *, *, #1646, .F. ) ;
#23088 = CARTESIAN_POINT ( 'NONE',  ( 0.5809828226811617480, -47.41188724015875522, -6.791453954330822107 ) ) ;
#23089 = CARTESIAN_POINT ( 'NONE',  ( 0.1140933569871964981, -27.80654152114252753, 34.25997954927705536 ) ) ;
#23090 = EDGE_CURVE ( 'NONE', #1476, #48507, #51037, .T. ) ;
#23091 = CARTESIAN_POINT ( 'NONE',  ( 1.227938101723756947, -42.91134962331487657, 0.8460948827223682134 ) ) ;
#23092 = ORIENTED_EDGE ( 'NONE', *, *, #20591, .T. ) ;
#23093 = CARTESIAN_POINT ( 'NONE',  ( 0.5839879327111922036, -18.41291455875270344, -44.21534283185622627 ) ) ;
#23094 = LINE ( 'NONE', #32494, #49484 ) ;
#23095 = CARTESIAN_POINT ( 'NONE',  ( 0.7048096507298579061, -44.76417498422327412, 17.62869676200329749 ) ) ;
#23096 = CARTESIAN_POINT ( 'NONE',  ( -2.601141883200665639, -0.9259886695528269929, 14.89758277215630677 ) ) ;
#23097 =( BOUNDED_SURFACE ( )  B_SPLINE_SURFACE ( 3, 1, ( 
 ( #42352, #52328 ),
 ( #46739, #61406 ),
 ( #43831, #37652 ),
 ( #13845, #32949 ) ),
 .UNSPECIFIED., .F., .F., .F. ) 
 B_SPLINE_SURFACE_WITH_KNOTS ( ( 4, 4 ),
 ( 2, 2 ),
 ( 0.000000000000000000, 1.000000000000000000 ),
 ( 0.000000000000000000, 1.000000000000000000 ),
 .UNSPECIFIED. ) 
 GEOMETRIC_REPRESENTATION_ITEM ( )  RATIONAL_B_SPLINE_SURFACE ( (
 ( 1.000000000000000000, 1.000000000000000000),
 ( 0.9754377213608244057, 0.9999580625633939235),
 ( 0.9754377213608244057, 0.9999580625633939235),
 ( 1.000000000000000000, 1.000000000000000000) ) ) 
 REPRESENTATION_ITEM ( '' )  SURFACE ( )  );
#23098 = CARTESIAN_POINT ( 'NONE',  ( 3.270143674763207553, 0.2742231296309522448, 13.68510027222513514 ) ) ;
#23099 = VERTEX_POINT ( 'NONE', #22553 ) ;
#23100 = CARTESIAN_POINT ( 'NONE',  ( -2.708315649062916552, 14.63219292706383001, -0.2635547933242103902 ) ) ;
#23101 = CARTESIAN_POINT ( 'NONE',  ( 0.5998501479064699549, 29.69975237324562656, 37.84527566984866809 ) ) ;
#23102 = ORIENTED_EDGE ( 'NONE', *, *, #5792, .T. ) ;
#23103 = FACE_OUTER_BOUND ( 'NONE', #59273, .T. ) ;
#23104 = CARTESIAN_POINT ( 'NONE',  ( 0.9790850452238870627, -27.01872131543053968, 32.03632358343099185 ) ) ;
#23105 = CARTESIAN_POINT ( 'NONE',  ( 0.3676999524040366896, -34.85286720109691316, 27.04123205746257241 ) ) ;
#23106 = CARTESIAN_POINT ( 'NONE',  ( 0.5998501479064708430, -23.59887241503325228, -41.92175333043611829 ) ) ;
#23107 = B_SPLINE_CURVE_WITH_KNOTS ( 'NONE', 3,
 ( #43861, #904, #25033, #20040 ),
 .UNSPECIFIED., .F., .F.,
 ( 4, 4 ),
 ( 6.254634441385501517E-18, 0.004566006591234646368 ),
 .UNSPECIFIED. ) ;
#23108 = CARTESIAN_POINT ( 'NONE',  ( 2.648799415243696664, -12.61806922346143089, -47.38461556625244953 ) ) ;
#23109 = CARTESIAN_POINT ( 'NONE',  ( 0.5988103564986354543, -41.35593036885951790, 24.57719524907170339 ) ) ;
#23110 = FACE_OUTER_BOUND ( 'NONE', #7160, .T. ) ;
#23111 =( NAMED_UNIT ( * ) SI_UNIT ( $, .STERADIAN. ) SOLID_ANGLE_UNIT ( ) );
#23112 = CARTESIAN_POINT ( 'NONE',  ( 4.962356264823593044, 18.10963840443015016, 37.99048031708913697 ) ) ;
#23113 = EDGE_CURVE ( 'NONE', #55532, #28847, #61658, .T. ) ;
#23114 = CARTESIAN_POINT ( 'NONE',  ( 0.6000166863083090663, -30.20952222014459210, 38.71961065066439289 ) ) ;
#23115 = CARTESIAN_POINT ( 'NONE',  ( 0.5998501479064699549, -34.38546660123274989, -33.64490850298832925 ) ) ;
#23116 = ORIENTED_EDGE ( 'NONE', *, *, #1228, .F. ) ;
#23117 = CARTESIAN_POINT ( 'NONE',  ( 0.8751705887134423323, 47.55935879196461968, 7.160166390004468973 ) ) ;
#23118 = CARTESIAN_POINT ( 'NONE',  ( 4.691466044806102076, -43.79545162262314761, 8.371234562541101099 ) ) ;
#23119 = CARTESIAN_POINT ( 'NONE',  ( 5.981074661064941900, -2.670494474392148376, 20.35019299530684123 ) ) ;
#23120 = CARTESIAN_POINT ( 'NONE',  ( 1.091591847532194626, -16.93206997590070628, -38.34141360574806612 ) ) ;
#23121 = CARTESIAN_POINT ( 'NONE',  ( 0.2885697896453115474, 26.88157175352887762, -33.71073718007512099 ) ) ;
#23122 = CARTESIAN_POINT ( 'NONE',  ( 21.00000000000000355, 0.000000000000000000, 0.000000000000000000 ) ) ;
#23123 = CONICAL_SURFACE ( 'NONE', #31113, 43.92652462719577500, 1.486293639869522343 ) ;
#23124 = ORIENTED_EDGE ( 'NONE', *, *, #2787, .F. ) ;
#23125 = CARTESIAN_POINT ( 'NONE',  ( 3.270143674763207553, -12.53844339339230451, -5.490410281242913193 ) ) ;
#23126 = CARTESIAN_POINT ( 'NONE',  ( 4.322998006666165516, 47.25487450103524623, 8.359821156456641589 ) ) ;
#23127 = CARTESIAN_POINT ( 'NONE',  ( 4.226256110419179812, 27.71872288846495991, -34.09544913063436411 ) ) ;
#23128 = CARTESIAN_POINT ( 'NONE',  ( -19.36110035657940287, -7.842565309080231195, -1.582362494774802730 ) ) ;
#23129 = ORIENTED_EDGE ( 'NONE', *, *, #27805, .T. ) ;
#23130 = CARTESIAN_POINT ( 'NONE',  ( -6.001507490154111224, -4.862106078787797436, -18.20581304543303247 ) ) ;
#23131 = B_SPLINE_CURVE_WITH_KNOTS ( 'NONE', 3,
 ( #50765, #12585, #50464, #17276 ),
 .UNSPECIFIED., .F., .F.,
 ( 4, 4 ),
 ( 6.992893892674702526E-18, 0.004042984057420977162 ),
 .UNSPECIFIED. ) ;
#23132 = CARTESIAN_POINT ( 'NONE',  ( 0.6031356219577719280, 23.97811961689687976, -41.70591683999481347 ) ) ;
#23133 = EDGE_LOOP ( 'NONE', ( #676, #11609, #24763, #17296 ) ) ;
#23134 = CARTESIAN_POINT ( 'NONE',  ( 4.924595438175366269, 0.7801755544698232292, 3.000000000000058620 ) ) ;
#23135 = ADVANCED_FACE ( 'NONE', ( #4330 ), #2461, .F. ) ;
#23136 = ORIENTED_EDGE ( 'NONE', *, *, #40080, .F. ) ;
#23137 = CARTESIAN_POINT ( 'NONE',  ( -6.016489644550737204, -11.46752133529374973, -14.95199950534959754 ) ) ;
#23138 = CARTESIAN_POINT ( 'NONE',  ( 0.2230388203127549596, 22.21453373073337900, 36.95676097786386549 ) ) ;
#23139 = ORIENTED_EDGE ( 'NONE', *, *, #35309, .F. ) ;
#23140 = FACE_OUTER_BOUND ( 'NONE', #12659, .T. ) ;
#23141 = CARTESIAN_POINT ( 'NONE',  ( 0.1104177457020372732, 26.25638621857945765, 34.20994892372218033 ) ) ;
#23143 = EDGE_LOOP ( 'NONE', ( #49072, #33096, #8411, #43349 ) ) ;
#23142 = EDGE_CURVE ( 'NONE', #20774, #60202, #24716, .T. ) ;
#23144 = CARTESIAN_POINT ( 'NONE',  ( 0.5832655196449137991, -7.575620595315191608, -46.28007298578045692 ) ) ;
#23145 = CARTESIAN_POINT ( 'NONE',  ( 0.8753041380234465318, -48.80600061351585595, 5.395612290228925190 ) ) ;
#23146 = ORIENTED_EDGE ( 'NONE', *, *, #41759, .F. ) ;
#23147 = CARTESIAN_POINT ( 'NONE',  ( 0.9789889208857702751, -7.065452030934339156, -41.30876766064238126 ) ) ;
#23148 = EDGE_CURVE ( 'NONE', #16218, #35743, #35152, .T. ) ;
#23150 = EDGE_LOOP ( 'NONE', ( #47324, #46052, #39309, #51880 ) ) ;
#23149 =( BOUNDED_SURFACE ( )  B_SPLINE_SURFACE ( 3, 1, ( 
 ( #51190, #3567 ),
 ( #23021, #51808 ),
 ( #55892, #38065 ),
 ( #52420, #52116 ) ),
 .UNSPECIFIED., .F., .F., .F. ) 
 B_SPLINE_SURFACE_WITH_KNOTS ( ( 4, 4 ),
 ( 2, 2 ),
 ( 0.000000000000000000, 1.000000000000000000 ),
 ( 0.000000000000000000, 1.000000000000000000 ),
 .UNSPECIFIED. ) 
 GEOMETRIC_REPRESENTATION_ITEM ( )  RATIONAL_B_SPLINE_SURFACE ( (
 ( 1.000000000000000000, 1.000000000000000000),
 ( 0.9953040768229013402, 0.8617119497784988535),
 ( 0.9953040768229013402, 0.8617119497784988535),
 ( 1.000000000000000000, 1.000000000000000000) ) ) 
 REPRESENTATION_ITEM ( '' )  SURFACE ( )  );
#23151 = LINE ( 'NONE', #57241, #31151 ) ;
#23152 = VERTEX_POINT ( 'NONE', #17859 ) ;
#23153 = ORIENTED_EDGE ( 'NONE', *, *, #48397, .F. ) ;
#23154 = FACE_OUTER_BOUND ( 'NONE', #60178, .T. ) ;
#23155 = FACE_OUTER_BOUND ( 'NONE', #38116, .T. ) ;
#23156 = CARTESIAN_POINT ( 'NONE',  ( 0.5800708119828336118, 46.42229822050698118, 11.78915056783724502 ) ) ;
#23157 = FACE_OUTER_BOUND ( 'NONE', #36622, .T. ) ;
#23158 = VERTEX_POINT ( 'NONE', #36984 ) ;
#23159 = CARTESIAN_POINT ( 'NONE',  ( 0.8557997880470599172, -46.03118133706016835, -13.27832040216687304 ) ) ;
#23160 = CARTESIAN_POINT ( 'NONE',  ( 0.1129192098497455998, -27.13044910148877165, -34.79785222304216319 ) ) ;
#23161 = ADVANCED_FACE ( 'NONE', ( #56044 ), #27731, .F. ) ;
#23162 = CARTESIAN_POINT ( 'NONE',  ( 0.5998501479064708430, -24.50586714782633280, 41.39809967730445095 ) ) ;
#23163 = ORIENTED_EDGE ( 'NONE', *, *, #59745, .T. ) ;
#23164 = CIRCLE ( 'NONE', #3155, 42.08604991992415023 ) ;
#23165 = ORIENTED_EDGE ( 'NONE', *, *, #14785, .F. ) ;
#23166 =( BOUNDED_SURFACE ( )  B_SPLINE_SURFACE ( 3, 1, ( 
 ( #54365, #26498 ),
 ( #45627, #40949 ),
 ( #34682, #2058 ),
 ( #10880, #49079 ) ),
 .UNSPECIFIED., .F., .F., .F. ) 
 B_SPLINE_SURFACE_WITH_KNOTS ( ( 4, 4 ),
 ( 2, 2 ),
 ( 0.000000000000000000, 1.000000000000000000 ),
 ( 0.000000000000000000, 1.000000000000000000 ),
 .UNSPECIFIED. ) 
 GEOMETRIC_REPRESENTATION_ITEM ( )  RATIONAL_B_SPLINE_SURFACE ( (
 ( 1.000000000000000000, 1.000000000000000000),
 ( 0.7282232189291694135, 0.9929344683865672927),
 ( 0.7282232189291694135, 0.9929344683865672927),
 ( 1.000000000000000000, 1.000000000000000000) ) ) 
 REPRESENTATION_ITEM ( '' )  SURFACE ( )  );
#23167 = CARTESIAN_POINT ( 'NONE',  ( 5.901764892641288895, 13.97448418306270490, 46.93298689894995590 ) ) ;
#23168 = CARTESIAN_POINT ( 'NONE',  ( 2.500000000000000000, 2.357898499370431722, -2.818925648462311528E-15 ) ) ;
#23169 = CARTESIAN_POINT ( 'NONE',  ( 0.1103310638050662013, -34.26302445194765056, 26.18709435931468121 ) ) ;
#23170 = CARTESIAN_POINT ( 'NONE',  ( 3.240649175237397372, -37.40057439548368734, -23.16164830674929576 ) ) ;
#23171 = ORIENTED_EDGE ( 'NONE', *, *, #14953, .F. ) ;
#23172 = CARTESIAN_POINT ( 'NONE',  ( 0.5827359174754822568, 47.43746338751532932, 6.611633125156963331 ) ) ;
#23173 = CARTESIAN_POINT ( 'NONE',  ( 0.3622758884714730732, -10.35929834645951964, 41.85013935980084199 ) ) ;
#23174 = CARTESIAN_POINT ( 'NONE',  ( 0.9268187852002115479, 43.07451267043047238, -9.398972875455658738 ) ) ;
#23175 = DIRECTION ( 'NONE',  ( -1.000000000000000000, -0.000000000000000000, -0.000000000000000000 ) ) ;
#23176 = CARTESIAN_POINT ( 'NONE',  ( 3.390910168358336918, -41.46266722896311308, -14.66098096287914743 ) ) ;
#23177 = FILL_AREA_STYLE ('',( #4037 ) ) ;
#23178 = DIRECTION ( 'NONE',  ( 0.000000000000000000, 0.000000000000000000, -1.000000000000000000 ) ) ;
#23179 = VERTEX_POINT ( 'NONE', #23168 ) ;
#23180 = FACE_OUTER_BOUND ( 'NONE', #17724, .T. ) ;
#23181 = CARTESIAN_POINT ( 'NONE',  ( -4.214292481396491930, -11.25702090725073035, -1.199999999999999956 ) ) ;
#23182 = CARTESIAN_POINT ( 'NONE',  ( 0.6000166863083106206, -7.321729200003417759, 48.56146376737702752 ) ) ;
#23183 = CARTESIAN_POINT ( 'NONE',  ( 0.000000000000000000, -1.178949249685214307, 2.042000000000001592 ) ) ;
#23184 = FACE_OUTER_BOUND ( 'NONE', #50504, .T. ) ;
#23185 = EDGE_CURVE ( 'NONE', #60457, #44492, #61311, .T. ) ;
#23186 = DIRECTION ( 'NONE',  ( 1.000000000000000000, 0.000000000000000000, 0.000000000000000000 ) ) ;
#23187 = CARTESIAN_POINT ( 'NONE',  ( 0.6028777368367059797, -49.10735432294857361, -0.08706728120422242700 ) ) ;
#23188 = CARTESIAN_POINT ( 'NONE',  ( 4.549368137175248350, 35.80950303116100741, -23.67244292351601942 ) ) ;
#23189 = EDGE_CURVE ( 'NONE', #32871, #48869, #61351, .T. ) ;
#23190 = EDGE_CURVE ( 'NONE', #38885, #23714, #39140, .T. ) ;
#23191 = CARTESIAN_POINT ( 'NONE',  ( 5.838029081930957709, 30.51096402024676024, 36.05753919374044614 ) ) ;
#23192 = EDGE_LOOP ( 'NONE', ( #14302, #5554 ) ) ;
#23193 = CARTESIAN_POINT ( 'NONE',  ( 2.281351352603295357, 13.68106635380627800, -45.98107981851849502 ) ) ;
#23194 = CARTESIAN_POINT ( 'NONE',  ( 0.9775691876210972353, 19.80844148971958774, 36.93182035505898853 ) ) ;
#23195 = CARTESIAN_POINT ( 'NONE',  ( 4.553261556744875094, 0.000000000000000000, 0.000000000000000000 ) ) ;
#23196 = CARTESIAN_POINT ( 'NONE',  ( 5.965394784446458765, -17.76824826579361982, 10.27521535480955528 ) ) ;
#23197 = ORIENTED_EDGE ( 'NONE', *, *, #28516, .F. ) ;
#23198 = CARTESIAN_POINT ( 'NONE',  ( 5.880360259849739535, -9.405269135694920735, -47.04104239318763803 ) ) ;
#23199 = CARTESIAN_POINT ( 'NONE',  ( 0.5997462898726536595, 44.46857747280041195, -20.83500054451300088 ) ) ;
#23200 = AXIS2_PLACEMENT_3D ( 'NONE', #5550, #53479, #43829 ) ;
#23201 = SURFACE_STYLE_USAGE ( .BOTH. , #42629 ) ;
#23202 = CIRCLE ( 'NONE', #31206, 43.12527911185304674 ) ;
#23203 = ORIENTED_EDGE ( 'NONE', *, *, #34467, .F. ) ;
#23204 = CARTESIAN_POINT ( 'NONE',  ( 3.270143674763207553, 5.490410281242775525, 12.53844339339236491 ) ) ;
#23205 = CARTESIAN_POINT ( 'NONE',  ( 4.960156602257184133, 2.524999074838214508, -46.35381625054453991 ) ) ;
#23206 = CARTESIAN_POINT ( 'NONE',  ( 0.8560838555295158248, 40.81790744942473737, -23.11430867518922128 ) ) ;
#23207 = EDGE_CURVE ( 'NONE', #35477, #2725, #3717, .T. ) ;
#23208 = ORIENTED_EDGE ( 'NONE', *, *, #27943, .T. ) ;
#23209 = CARTESIAN_POINT ( 'NONE',  ( 0.6254311100348646235, 46.28443883864375152, 13.11433105842157509 ) ) ;
#23210 = ORIENTED_EDGE ( 'NONE', *, *, #26544, .T. ) ;
#23211 = ORIENTED_EDGE ( 'NONE', *, *, #30141, .F. ) ;
#23212 = CARTESIAN_POINT ( 'NONE',  ( 0.5832366564991502411, -6.521686574605801923, -47.44984844891996545 ) ) ;
#23213 = DIRECTION ( 'NONE',  ( 0.000000000000000000, 0.000000000000000000, 1.000000000000000000 ) ) ;
#23214 = ORIENTED_EDGE ( 'NONE', *, *, #6697, .F. ) ;
#23215 = FACE_OUTER_BOUND ( 'NONE', #46641, .T. ) ;
#23216 = ORIENTED_EDGE ( 'NONE', *, *, #44649, .T. ) ;
#23217 = CARTESIAN_POINT ( 'NONE',  ( 0.5797568665920714848, 11.48244725320605042, 45.46843645518516297 ) ) ;
#23218 = EDGE_CURVE ( 'NONE', #23536, #39132, #46008, .T. ) ;
#23219 = B_SPLINE_CURVE_WITH_KNOTS ( 'NONE', 3,
 ( #26978, #55459, #56083, #22590 ),
 .UNSPECIFIED., .F., .F.,
 ( 4, 4 ),
 ( 0.000000000000000000, 0.004446090762761370323 ),
 .UNSPECIFIED. ) ;
#23220 = CARTESIAN_POINT ( 'NONE',  ( 0.5804410086790514622, -20.23572001627559303, -42.30881098870894874 ) ) ;
#23221 = CARTESIAN_POINT ( 'NONE',  ( 2.624215991343608501, 44.87417713512112982, -17.05978231157355296 ) ) ;
#23222 = ORIENTED_EDGE ( 'NONE', *, *, #36166, .F. ) ;
#23223 = CARTESIAN_POINT ( 'NONE',  ( 0.6845945791218034371, 46.36658412396714368, 7.109598961194799394 ) ) ;
#23224 = FACE_OUTER_BOUND ( 'NONE', #48500, .T. ) ;
#23225 = CARTESIAN_POINT ( 'NONE',  ( 0.5804410086790514622, -42.10186154173687356, 20.66284362269179553 ) ) ;
#23226 = CARTESIAN_POINT ( 'NONE',  ( 4.962356264823603702, 41.96072444189417183, -3.245489512195726789 ) ) ;
#23227 = ORIENTED_EDGE ( 'NONE', *, *, #37519, .F. ) ;
#23228 = CARTESIAN_POINT ( 'NONE',  ( 0.5804410086790514622, -2.113107284889295556, 46.85141011173457315 ) ) ;
#23229 = EDGE_CURVE ( 'NONE', #13648, #50298, #48556, .T. ) ;
#23230 = CARTESIAN_POINT ( 'NONE',  ( 0.1140933569871965397, -31.43159979652969227, -30.96779753735644292 ) ) ;
#23231 = ORIENTED_EDGE ( 'NONE', *, *, #40952, .T. ) ;
#23232 = CARTESIAN_POINT ( 'NONE',  ( 0.9758171775293923433, -42.90848549292462621, 0.005919131624846820337 ) ) ;
#23233 = B_SPLINE_CURVE_WITH_KNOTS ( 'NONE', 3,
 ( #24069, #4312, #61634, #18766 ),
 .UNSPECIFIED., .F., .F.,
 ( 4, 4 ),
 ( 0.000000000000000000, 0.004445488388166991649 ),
 .UNSPECIFIED. ) ;
#23234 = B_SPLINE_CURVE_WITH_KNOTS ( 'NONE', 3,
 ( #37251, #3998, #7464, #41342, #46341, #17210, #36949, #55700, #26912, #3385 ),
 .UNSPECIFIED., .F., .F.,
 ( 4, 3, 3, 4 ),
 ( 0.0005448802484329447627, 0.0005449104342063602240, 0.0008173270854453676491, 0.001089761613562688792 ),
 .UNSPECIFIED. ) ;
#23235 = VERTEX_POINT ( 'NONE', #10613 ) ;
#23236 = CARTESIAN_POINT ( 'NONE',  ( 5.896782393890504181, 12.99025607003319038, -15.35510775321938404 ) ) ;
#23237 = CARTESIAN_POINT ( 'NONE',  ( 4.967162193818130511, 32.68434214048205888, -28.07411493385260925 ) ) ;
#23238 = ORIENTED_EDGE ( 'NONE', *, *, #30185, .T. ) ;
#23239 = CARTESIAN_POINT ( 'NONE',  ( 0.9762797500689124330, -34.83496347773922963, -23.29914386174477059 ) ) ;
#23240 = CARTESIAN_POINT ( 'NONE',  ( 0.5980894510889448457, 46.65000524237087376, -11.77356634613269470 ) ) ;
#23241 = CARTESIAN_POINT ( 'NONE',  ( 5.974727161628367256, 14.52429704002343769, 14.50236057684849911 ) ) ;
#23242 = DIRECTION ( 'NONE',  ( -1.000000000000000000, 0.000000000000000000, 0.000000000000000000 ) ) ;
#23243 = ORIENTED_EDGE ( 'NONE', *, *, #330, .T. ) ;
#23244 = CARTESIAN_POINT ( 'NONE',  ( 4.975610109902397937, -22.11219452748553138, -43.62912170003438916 ) ) ;
#23245 = CARTESIAN_POINT ( 'NONE',  ( 0.9772918015221170318, -41.78532364903834662, 3.213033348067860562 ) ) ;
#23246 = CARTESIAN_POINT ( 'NONE',  ( 2.643462169533613793, 43.83256147628732435, -19.65219740572143792 ) ) ;
#23247 = CARTESIAN_POINT ( 'NONE',  ( 5.981074661064941900, -10.25489689131142867, 17.77917279944614393 ) ) ;
#23248 = CIRCLE ( 'NONE', #22223, 42.08604991992415023 ) ;
#23249 = CARTESIAN_POINT ( 'NONE',  ( 4.967162193818130511, 28.07411493385340862, -32.68434214048137676 ) ) ;
#23250 = CARTESIAN_POINT ( 'NONE',  ( -6.063463321072278589, 5.464110623309939463, 18.46520911269897880 ) ) ;
#23251 = CYLINDRICAL_SURFACE ( 'NONE', #19238, 6.728125000000023448 ) ;
#23252 = DIRECTION ( 'NONE',  ( 0.000000000000000000, 0.000000000000000000, 1.000000000000000000 ) ) ;
#23253 = B_SPLINE_CURVE_WITH_KNOTS ( 'NONE', 3,
 ( #33570, #61722, #37979, #42657, #56727, #57634 ),
 .UNSPECIFIED., .F., .F.,
 ( 4, 2, 4 ),
 ( 8.787390050835121380E-18, 0.0002445244328975383239, 0.0004890488657950678658 ),
 .UNSPECIFIED. ) ;
#23254 = LINE ( 'NONE', #22641, #24219 ) ;
#23255 = DIRECTION ( 'NONE',  ( 0.000000000000000000, 0.000000000000000000, -1.000000000000000000 ) ) ;
#23256 = EDGE_CURVE ( 'NONE', #2406, #55928, #10931, .T. ) ;
#23257 = CARTESIAN_POINT ( 'NONE',  ( 5.901764892641307547, -10.93876531158323040, 47.73190631954460628 ) ) ;
#23258 = CARTESIAN_POINT ( 'NONE',  ( 2.500000000000000000, -1.178949249685214307, 2.042000000000001592 ) ) ;
#23259 = CARTESIAN_POINT ( 'NONE',  ( 1.231276596079881047, 38.25526645152027072, 17.14092645516147684 ) ) ;
#23260 = CARTESIAN_POINT ( 'NONE',  ( 1.231276596079881047, -23.26513148155264332, 34.87134107206281186 ) ) ;
#23262 = EDGE_CURVE ( 'NONE', #40345, #39908, #41940, .T. ) ;
#23261 = CARTESIAN_POINT ( 'NONE',  ( 4.390527457369401532, -20.60499138400743036, 38.80231522336777772 ) ) ;
#23263 = DIRECTION ( 'NONE',  ( 0.1024043820194936172, 0.2447326578667328445, -0.9641676559171078464 ) ) ;
#23264 = ADVANCED_FACE ( 'NONE', ( #61963 ), #53316, .F. ) ;
#23265 = CARTESIAN_POINT ( 'NONE',  ( 0.2111111111111110827, -9.497654031326126400, 0.000000000000000000 ) ) ;
#23266 = EDGE_CURVE ( 'NONE', #25227, #59695, #57569, .T. ) ;
#23268 = ORIENTED_EDGE ( 'NONE', *, *, #48642, .T. ) ;
#23267 = CARTESIAN_POINT ( 'NONE',  ( 4.694002226626921015, -38.01786027345620056, -25.15804188871017999 ) ) ;
#23269 = FACE_OUTER_BOUND ( 'NONE', #2998, .T. ) ;
#23270 = CARTESIAN_POINT ( 'NONE',  ( 0.5837374860065626114, 24.10515569139049674, 41.38807031854324947 ) ) ;
#23271 = EDGE_CURVE ( 'NONE', #6350, #2855, #24707, .T. ) ;
#23272 = CARTESIAN_POINT ( 'NONE',  ( 0.8557997880470690211, 41.93815086860257679, 23.15977007032337553 ) ) ;
#23273 = EDGE_LOOP ( 'NONE', ( #23214, #47346, #22143, #44459 ) ) ;
#23274 = ORIENTED_EDGE ( 'NONE', *, *, #45112, .F. ) ;
#23275 = CARTESIAN_POINT ( 'NONE',  ( 1.657374760986086493, -30.77364477053859559, 31.52575510259740454 ) ) ;
#23276 = CARTESIAN_POINT ( 'NONE',  ( 4.967162193818129623, -19.45289607368849616, 38.44485641567065670 ) ) ;
#23277 = B_SPLINE_CURVE_WITH_KNOTS ( 'NONE', 3,
 ( #58536, #48850, #15665, #34767 ),
 .UNSPECIFIED., .F., .F.,
 ( 4, 4 ),
 ( 4.443059973708341306E-17, 0.005004948556313850404 ),
 .UNSPECIFIED. ) ;
#23278 = EDGE_LOOP ( 'NONE', ( #19215, #37894, #15188, #55171 ) ) ;
#23279 = ORIENTED_EDGE ( 'NONE', *, *, #55791, .T. ) ;
#23280 = EDGE_CURVE ( 'NONE', #32472, #21489, #19706, .T. ) ;
#23281 = B_SPLINE_CURVE_WITH_KNOTS ( 'NONE', 3,
 ( #34903, #53965, #44613, #53355 ),
 .UNSPECIFIED., .F., .F.,
 ( 4, 4 ),
 ( 1.969819611697804288E-17, 0.004444306975806115896 ),
 .UNSPECIFIED. ) ;
#23282 = CARTESIAN_POINT ( 'NONE',  ( 0.6023142530420679819, -38.32506243004171864, -29.07781306567088109 ) ) ;
#23283 = ADVANCED_FACE ( 'NONE', ( #38515 ), #14966, .T. ) ;
#23284 = CARTESIAN_POINT ( 'NONE',  ( 0.7056313189692712262, 3.855069639226469391, -46.74277572025726357 ) ) ;
#23285 = CARTESIAN_POINT ( 'NONE',  ( 0.9757892942422834448, -41.43309903783660531, 11.15510465568985587 ) ) ;
#23286 = ORIENTED_EDGE ( 'NONE', *, *, #26219, .F. ) ;
#23287 = VERTEX_POINT ( 'NONE', #38830 ) ;
#23288 = CARTESIAN_POINT ( 'NONE',  ( 3.238018933889920792, 10.33920672294413912, -8.515180368487779816 ) ) ;
#23289 = VERTEX_POINT ( 'NONE', #57887 ) ;
#23290 = CARTESIAN_POINT ( 'NONE',  ( 0.8554163680231738898, 9.985124899324343772, 45.84215040611328362 ) ) ;
#23291 = CARTESIAN_POINT ( 'NONE',  ( 4.694002226626921015, 18.13772657221498719, 41.82472529781519199 ) ) ;
#23292 = AXIS2_PLACEMENT_3D ( 'NONE', #2281, #12041, #31115 ) ;
#23293 = CARTESIAN_POINT ( 'NONE',  ( 0.6000166863083106206, -45.32251430608251752, -18.91277818522173959 ) ) ;
#23294 = ORIENTED_EDGE ( 'NONE', *, *, #24397, .T. ) ;
#23295 = CARTESIAN_POINT ( 'NONE',  ( 0.9784957157296367836, -39.51281881580939626, 13.96675360351822981 ) ) ;
#23296 = ORIENTED_EDGE ( 'NONE', *, *, #49157, .F. ) ;
#23297 = ORIENTED_EDGE ( 'NONE', *, *, #32461, .T. ) ;
#23298 = CARTESIAN_POINT ( 'NONE',  ( 0.5980894510889448457, -29.84264441023806569, 37.73932204245466693 ) ) ;
#23299 = VERTEX_POINT ( 'NONE', #34124 ) ;
#23300 = CARTESIAN_POINT ( 'NONE',  ( 0.3676999524040366896, 34.11874447324979087, 27.96179284115963171 ) ) ;
#23301 = CARTESIAN_POINT ( 'NONE',  ( 1.088908134280559326, 17.14055988408919617, 39.34174992079760358 ) ) ;
#23302 = CARTESIAN_POINT ( 'NONE',  ( 0.9757954354143124620, -0.01316335317099341304, 42.90846090505963417 ) ) ;
#23303 = CARTESIAN_POINT ( 'NONE',  ( -6.016489644550737204, 11.46752133529384565, 14.95199950534952293 ) ) ;
#23304 = CARTESIAN_POINT ( 'NONE',  ( -6.015611763856276717, 2.453375430804066504, 18.68284711750059301 ) ) ;
#23305 = EDGE_CURVE ( 'NONE', #43871, #58483, #4486, .T. ) ;
#23306 = B_SPLINE_CURVE_WITH_KNOTS ( 'NONE', 3,
 ( #47772, #38388, #57436, #53066 ),
 .UNSPECIFIED., .F., .F.,
 ( 4, 4 ),
 ( 2.384850491544188529E-17, 0.004564976165746187711 ),
 .UNSPECIFIED. ) ;
#23307 = VERTEX_POINT ( 'NONE', #30947 ) ;
#23308 = CARTESIAN_POINT ( 'NONE',  ( -6.017396004339686577, 9.420565012089657131, -16.31924478664265621 ) ) ;
#23309 = CARTESIAN_POINT ( 'NONE',  ( -79.49999999999975842, -1.460391307983213802E-14, 1.540743955509788682E-30 ) ) ;
#23310 = B_SPLINE_CURVE_WITH_KNOTS ( 'NONE', 3,
 ( #32322, #51398, #27303, #3785, #17300, #22927 ),
 .UNSPECIFIED., .F., .F.,
 ( 4, 2, 4 ),
 ( 9.553906862710701093E-18, 0.0002448709889506563977, 0.0004897419779013032545 ),
 .UNSPECIFIED. ) ;
#23311 = EDGE_CURVE ( 'NONE', #36718, #13235, #18735, .T. ) ;
#23312 = CARTESIAN_POINT ( 'NONE',  ( -6.016489644550737204, -18.68257207665197939, 2.455165042129670905 ) ) ;
#23313 = VECTOR ( 'NONE', #23816, 1000.000000000000114 ) ;
#23314 = ORIENTED_EDGE ( 'NONE', *, *, #25556, .T. ) ;
#23315 = CARTESIAN_POINT ( 'NONE',  ( 4.291220156522059348, 46.35409538318315015, 8.407546521575474330 ) ) ;
#23316 = DIRECTION ( 'NONE',  ( -1.000000000000000000, -3.673819061467147552E-16, 1.925929944387234758E-32 ) ) ;
#23317 = CARTESIAN_POINT ( 'NONE',  ( -6.078075953587585900, 13.83625866740996813, 13.39227838478794652 ) ) ;
#23318 = ORIENTED_EDGE ( 'NONE', *, *, #59797, .F. ) ;
#23319 = ORIENTED_EDGE ( 'NONE', *, *, #48428, .T. ) ;
#23320 = CARTESIAN_POINT ( 'NONE',  ( -6.077587904424778920, 17.85108912406241899, 7.220432014686572586 ) ) ;
#23321 = CARTESIAN_POINT ( 'NONE',  ( 4.549368137175248350, 0.000000000000000000, 0.000000000000000000 ) ) ;
#23322 = CARTESIAN_POINT ( 'NONE',  ( 5.896278296736517710, -9.670675947512847870, -17.63533402951529538 ) ) ;
#23323 = CARTESIAN_POINT ( 'NONE',  ( 4.553261556744873317, -43.82122302957819215, 3.039733214543990591 ) ) ;
#23324 = CARTESIAN_POINT ( 'NONE',  ( 0.5804410086790514622, -44.48029469925780433, -14.86685021524652228 ) ) ;
#23325 = CARTESIAN_POINT ( 'NONE',  ( 0.5807400328401637335, 46.12278621143515522, -12.92266817605966978 ) ) ;
#23326 = CARTESIAN_POINT ( 'NONE',  ( 1.827326673878743923, -33.38933471001457320, -27.17438009792320486 ) ) ;
#23327 = CARTESIAN_POINT ( 'NONE',  ( 0.5850706913938534814, -29.01314519953824700, 38.10903744847131236 ) ) ;
#23328 = DIRECTION ( 'NONE',  ( 0.1024043820194936449, -0.9641676559171085126, -0.2447326578667294861 ) ) ;
#23329 = CARTESIAN_POINT ( 'NONE',  ( 5.838029081930955932, -4.747847248974867540, 46.99492530745549601 ) ) ;
#23330 = CARTESIAN_POINT ( 'NONE',  ( 0.2285344041767104206, -22.21790586462361361, 38.11647713635377244 ) ) ;
#23331 = FACE_OUTER_BOUND ( 'NONE', #57735, .T. ) ;
#23332 = ORIENTED_EDGE ( 'NONE', *, *, #46215, .T. ) ;
#23333 = CARTESIAN_POINT ( 'NONE',  ( 7.000000000000006217, -2.780326704359372228E-13, 80.00000000000001421 ) ) ;
#23334 = CARTESIAN_POINT ( 'NONE',  ( 0.2940133293163013639, -35.83075917510851127, 25.73707921488799855 ) ) ;
#23335 = CARTESIAN_POINT ( 'NONE',  ( 0.8551540677456739292, -13.28067116677233805, 46.03951182599424641 ) ) ;
#23336 = CARTESIAN_POINT ( 'NONE',  ( 0.6016118706126976079, -39.14612183274096679, -29.65016357864037033 ) ) ;
#23337 = CARTESIAN_POINT ( 'NONE',  ( 3.559346040607745287, -24.52570418190676094, -36.49548076027481613 ) ) ;
#23338 = VECTOR ( 'NONE', #9319, 1000.000000000000114 ) ;
#23339 = CARTESIAN_POINT ( 'NONE',  ( 4.960156602257181468, -34.56254177294292873, 30.99165383632755066 ) ) ;
#23341 = EDGE_CURVE ( 'NONE', #49359, #42620, #61190, .T. ) ;
#23340 = CARTESIAN_POINT ( 'NONE',  ( 4.975801465491694664, 47.76942479135480824, 3.702618843597622167 ) ) ;
#23342 =( BOUNDED_SURFACE ( )  B_SPLINE_SURFACE ( 3, 1, ( 
 ( #6912, #41106 ),
 ( #59229, #54522 ),
 ( #54843, #1915 ),
 ( #11332, #55458 ) ),
 .UNSPECIFIED., .F., .F., .F. ) 
 B_SPLINE_SURFACE_WITH_KNOTS ( ( 4, 4 ),
 ( 2, 2 ),
 ( 0.000000000000000000, 1.000000000000000000 ),
 ( 0.000000000000000000, 1.000000000000000000 ),
 .UNSPECIFIED. ) 
 GEOMETRIC_REPRESENTATION_ITEM ( )  RATIONAL_B_SPLINE_SURFACE ( (
 ( 1.000000000000000000, 1.000000000000000000),
 ( 0.9953485035131437453, 0.8621029689291515030),
 ( 0.9953485035131437453, 0.8621029689291515030),
 ( 1.000000000000000000, 1.000000000000000000) ) ) 
 REPRESENTATION_ITEM ( '' )  SURFACE ( )  );
#23343 = CARTESIAN_POINT ( 'NONE',  ( 0.8560838555295158248, -44.60403252362548443, 14.52078223488980768 ) ) ;
#23344 = EDGE_CURVE ( 'NONE', #23911, #27511, #44050, .T. ) ;
#23345 = CARTESIAN_POINT ( 'NONE',  ( 0.6021447746440204973, -1.312817911176840546, 49.08989354460427990 ) ) ;
#23346 = EDGE_CURVE ( 'NONE', #30431, #30079, #8166, .T. ) ;
#23348 = ORIENTED_EDGE ( 'NONE', *, *, #53235, .T. ) ;
#23347 = CARTESIAN_POINT ( 'NONE',  ( 4.967162193818130511, 0.000000000000000000, 0.000000000000000000 ) ) ;
#23349 = VERTEX_POINT ( 'NONE', #21859 ) ;
#23350 = CARTESIAN_POINT ( 'NONE',  ( 0.1158816050234199174, -7.036604598242554687, 43.55947930167616278 ) ) ;
#23351 = CARTESIAN_POINT ( 'NONE',  ( 0.2940135542859019235, 14.47847097612530298, -41.67270601826714227 ) ) ;
#23352 = EDGE_CURVE ( 'NONE', #13765, #49641, #45077, .T. ) ;
#23353 = DIRECTION ( 'NONE',  ( 1.000000000000000000, 0.000000000000000000, 0.000000000000000000 ) ) ;
#23354 = ORIENTED_EDGE ( 'NONE', *, *, #56476, .T. ) ;
#23355 = DIRECTION ( 'NONE',  ( 0.000000000000000000, 0.000000000000000000, 1.000000000000000000 ) ) ;
#23357 = CARTESIAN_POINT ( 'NONE',  ( 0.8753041380234524160, 16.12068986424834449, -46.38169559399161557 ) ) ;
#23356 = VECTOR ( 'NONE', #48552, 1000.000000000000000 ) ;
#23358 = CARTESIAN_POINT ( 'NONE',  ( 4.967162193818130511, 0.000000000000000000, 0.000000000000000000 ) ) ;
#23359 = VERTEX_POINT ( 'NONE', #50055 ) ;
#23360 = ORIENTED_EDGE ( 'NONE', *, *, #11424, .F. ) ;
#23361 = EDGE_CURVE ( 'NONE', #58926, #14715, #25370, .T. ) ;
#23362 = LINE ( 'NONE', #42485, #44337 ) ;
#23363 = CARTESIAN_POINT ( 'NONE',  ( 3.559346040607745287, -39.94197359654808821, 18.38665349525692960 ) ) ;
#23364 = CARTESIAN_POINT ( 'NONE',  ( 0.8753041380234524160, 41.63161868429038037, 26.03740873433498848 ) ) ;
#23365 = CARTESIAN_POINT ( 'NONE',  ( -6.016104459813374383, 13.32039631884684638, 13.32794178585002243 ) ) ;
#23366 = CARTESIAN_POINT ( 'NONE',  ( 0.1064266379913941102, 10.61815631313362118, -41.79703901861807935 ) ) ;
#23367 = CARTESIAN_POINT ( 'NONE',  ( 5.896782393890504181, 5.965008392936887560, 19.20793486427431418 ) ) ;
#23368 = ORIENTED_EDGE ( 'NONE', *, *, #60245, .F. ) ;
#23369 = CARTESIAN_POINT ( 'NONE',  ( 4.962356264823608143, 18.10963840443066530, -37.99048031708887407 ) ) ;
#23370 = DIRECTION ( 'NONE',  ( 0.09835009131224567436, -0.1222230102474943930, -0.9876177374393970698 ) ) ;
#23371 = EDGE_LOOP ( 'NONE', ( #53850, #11685, #22118, #1689 ) ) ;
#23372 = CARTESIAN_POINT ( 'NONE',  ( 0.9788927965476044157, -37.46797425825765515, -18.77465093188997969 ) ) ;
#23373 = DIRECTION ( 'NONE',  ( 0.000000000000000000, 0.000000000000000000, 1.000000000000000000 ) ) ;
#23374 = CARTESIAN_POINT ( 'NONE',  ( 0.9789233960466710016, 4.325698577799566458, -41.68483007817547303 ) ) ;
#23375 = CARTESIAN_POINT ( 'NONE',  ( 0.6253024248130488738, 23.32030274153287763, -43.21582704821111776 ) ) ;
#23376 = VECTOR ( 'NONE', #35679, 1000.000000000000114 ) ;
#23377 = ORIENTED_EDGE ( 'NONE', *, *, #20591, .F. ) ;
#23378 = ORIENTED_EDGE ( 'NONE', *, *, #11192, .F. ) ;
#23379 = CARTESIAN_POINT ( 'NONE',  ( 0.1157991065609915854, -44.12409475290455418, -0.08141114419867848118 ) ) ;
#23380 = CARTESIAN_POINT ( 'NONE',  ( 0.5809828226811617480, 41.20389530892307306, 24.41822904836939401 ) ) ;
#23381 = DIRECTION ( 'NONE',  ( 0.000000000000000000, 0.000000000000000000, 1.000000000000000000 ) ) ;
#23382 = EDGE_CURVE ( 'NONE', #23759, #38660, #22374, .T. ) ;
#23383 = ORIENTED_EDGE ( 'NONE', *, *, #38525, .F. ) ;
#23384 = CARTESIAN_POINT ( 'NONE',  ( 0.6067099128993235224, 41.82996792600780367, 23.33192673707546660 ) ) ;
#23385 = ORIENTED_EDGE ( 'NONE', *, *, #49210, .T. ) ;
#23386 = CARTESIAN_POINT ( 'NONE',  ( 2.009741617377216460, 43.46874900317952495, 7.069083230633559367 ) ) ;
#23387 = CARTESIAN_POINT ( 'NONE',  ( 0.5830081025819919827, 28.03721062606959791, 37.59184558772897589 ) ) ;
#23388 = B_SPLINE_CURVE_WITH_KNOTS ( 'NONE', 3,
 ( #24720, #5885, #1205, #39460 ),
 .UNSPECIFIED., .F., .F.,
 ( 4, 4 ),
 ( 2.860979249076398407E-17, 0.005004948556313843465 ),
 .UNSPECIFIED. ) ;
#23389 = ORIENTED_EDGE ( 'NONE', *, *, #50619, .F. ) ;
#23390 = CARTESIAN_POINT ( 'NONE',  ( 0.5834872094924179464, -47.45604551759231526, -6.476680342367071574 ) ) ;
#23391 = CARTESIAN_POINT ( 'NONE',  ( 0.8554163680231738898, -2.480940174720807079, 46.85136507041471532 ) ) ;
#23392 = DIRECTION ( 'NONE',  ( -0.1011922191286467460, -0.9481578383257858178, 0.3012587731655177459 ) ) ;
#23393 = CIRCLE ( 'NONE', #40409, 42.92674063221959813 ) ;
#23394 = B_SPLINE_CURVE_WITH_KNOTS ( 'NONE', 3,
 ( #53051, #14562, #19258, #47150 ),
 .UNSPECIFIED., .F., .F.,
 ( 4, 4 ),
 ( 0.000000000000000000, 0.004048833967417082152 ),
 .UNSPECIFIED. ) ;
#23395 = DIRECTION ( 'NONE',  ( -1.655270492344281801E-16, 1.000000000000000000, 0.000000000000000000 ) ) ;
#23396 = CARTESIAN_POINT ( 'NONE',  ( 0.3676999524040323597, 19.66859742988730986, 39.48540057367873857 ) ) ;
#23397 = CARTESIAN_POINT ( 'NONE',  ( 4.549368137175248350, 0.000000000000000000, 0.000000000000000000 ) ) ;
#23398 = CARTESIAN_POINT ( 'NONE',  ( 0.1092355843206037486, 26.49036028133781429, -34.02913268098563293 ) ) ;
#23399 = DIRECTION ( 'NONE',  ( 0.000000000000000000, 0.000000000000000000, -1.000000000000000000 ) ) ;
#23400 = ORIENTED_EDGE ( 'NONE', *, *, #12329, .F. ) ;
#23401 = DIRECTION ( 'NONE',  ( 0.000000000000000000, 0.000000000000000000, 1.000000000000000000 ) ) ;
#23402 = CARTESIAN_POINT ( 'NONE',  ( 0.5797568599927143129, 40.02504816884456318, 24.43810196706526838 ) ) ;
#23403 = ORIENTED_EDGE ( 'NONE', *, *, #21903, .F. ) ;
#23404 = CARTESIAN_POINT ( 'NONE',  ( 0.5800708119828335008, 38.37709857409269887, 28.65679933661808221 ) ) ;
#23405 = CARTESIAN_POINT ( 'NONE',  ( 0.5809828226811617480, 0.5448590168539207967, -47.89273459658652854 ) ) ;
#23406 = EDGE_CURVE ( 'NONE', #33579, #46829, #45377, .T. ) ;
#23407 = CARTESIAN_POINT ( 'NONE',  ( 0.9757402383260943557, 5.684842778069837621, -42.53022961222597331 ) ) ;
#23408 = FACE_OUTER_BOUND ( 'NONE', #54711, .T. ) ;
#23409 = CARTESIAN_POINT ( 'NONE',  ( -6.079354080745853928, -4.285997663762476151, -18.77293741731390853 ) ) ;
#23410 = CARTESIAN_POINT ( 'NONE',  ( 0.6846871229502899947, -43.92355552798050411, 19.12907057981189496 ) ) ;
#23411 = CARTESIAN_POINT ( 'NONE',  ( 20.50003018527262455, 1.544988095791843818E-15, 1.507911437718603435E-16 ) ) ;
#23413 = EDGE_CURVE ( 'NONE', #7392, #37162, #15623, .T. ) ;
#23412 = CARTESIAN_POINT ( 'NONE',  ( 4.960386119450141962, -30.07757850721755588, 31.77696863790668758 ) ) ;
#23414 = CARTESIAN_POINT ( 'NONE',  ( -6.077587904424778920, 12.01079512011154193, -15.05114022181160927 ) ) ;
#23415 = ADVANCED_FACE ( 'NONE', ( #55971 ), #53677, .F. ) ;
#23416 = CARTESIAN_POINT ( 'NONE',  ( 4.960156602257182357, 15.40604254112643723, 43.79161740034479777 ) ) ;
#23417 = CARTESIAN_POINT ( 'NONE',  ( 4.962356264823608143, 0.000000000000000000, 0.000000000000000000 ) ) ;
#23418 = EDGE_LOOP ( 'NONE', ( #2694, #51702, #57366, #10517 ) ) ;
#23419 = DIRECTION ( 'NONE',  ( 1.836766033387207149E-16, -1.000000000000000000, 0.000000000000000000 ) ) ;
#23420 = EDGE_CURVE ( 'NONE', #19355, #7571, #13090, .T. ) ;
#23421 = CARTESIAN_POINT ( 'NONE',  ( 0.5806925824938499181, 27.37593026015182218, 38.07598724570208049 ) ) ;
#23422 = CIRCLE ( 'NONE', #12428, 85.00000000000001421 ) ;
#23423 = CARTESIAN_POINT ( 'NONE',  ( 0.8560838555295223751, 23.34035564869547841, 40.68907263964295851 ) ) ;
#23424 = CARTESIAN_POINT ( 'NONE',  ( 0.5837800304671215690, 46.47150964378750615, 6.295722643737187596 ) ) ;
#23425 = CARTESIAN_POINT ( 'NONE',  ( 0.6017666602106488405, -37.95277954208655302, 29.56224131406205657 ) ) ;
#23426 = B_SPLINE_CURVE_WITH_KNOTS ( 'NONE', 3,
 ( #55246, #50868, #22370, #60564 ),
 .UNSPECIFIED., .F., .F.,
 ( 4, 4 ),
 ( 0.000000000000000000, 0.005014147105413709060 ),
 .UNSPECIFIED. ) ;
#23427 = VERTEX_POINT ( 'NONE', #17779 ) ;
#23428 = CARTESIAN_POINT ( 'NONE',  ( 0.9757787079277433495, 11.14366644276469032, -41.43615150473004860 ) ) ;
#23429 = EDGE_CURVE ( 'NONE', #29382, #42725, #55983, .T. ) ;
#23430 = CARTESIAN_POINT ( 'NONE',  ( 5.895881250540457863, 10.81854556178467242, 16.95543433639758391 ) ) ;
#23431 = ORIENTED_EDGE ( 'NONE', *, *, #57047, .F. ) ;
#23432 = EDGE_CURVE ( 'NONE', #40711, #12159, #52206, .T. ) ;
#23433 = CARTESIAN_POINT ( 'NONE',  ( 4.549368137175248350, 0.000000000000000000, 0.000000000000000000 ) ) ;
#23434 = AXIS2_PLACEMENT_3D ( 'NONE', #55334, #31547, #21847 ) ;
#23435 = CARTESIAN_POINT ( 'NONE',  ( 5.896278296736517710, -19.39967646272022961, -5.308439766651063429 ) ) ;
#23436 = VERTEX_POINT ( 'NONE', #3341 ) ;
#23437 = CARTESIAN_POINT ( 'NONE',  ( 0.5549461598389364703, -26.80708097326903072, 35.02282263266913986 ) ) ;
#23438 = ORIENTED_EDGE ( 'NONE', *, *, #59754, .T. ) ;
#23439 = CARTESIAN_POINT ( 'NONE',  ( 0.6041374136657475802, -44.51224464245012058, 18.24862627831457118 ) ) ;
#23440 = CARTESIAN_POINT ( 'NONE',  ( 0.5997462898726536595, 17.44942740672405534, 45.90282249842351803 ) ) ;
#23441 = B_SPLINE_CURVE_WITH_KNOTS ( 'NONE', 3,
 ( #31228, #60035, #1465, #35024, #15906, #7395 ),
 .UNSPECIFIED., .F., .F.,
 ( 4, 2, 4 ),
 ( 0.002336974151641604130, 0.003500975885716476211, 0.004664977619791348291 ),
 .UNSPECIFIED. ) ;
#23442 = ORIENTED_EDGE ( 'NONE', *, *, #15010, .T. ) ;
#23443 = CARTESIAN_POINT ( 'NONE',  ( 3.238931869106854489, 42.82436385108074717, 3.793313187127091979 ) ) ;
#23444 = CARTESIAN_POINT ( 'NONE',  ( 0.1092355843206037486, 26.01340835034366705, 34.39511076960612002 ) ) ;
#23445 = CARTESIAN_POINT ( 'NONE',  ( 0.6252788684277218456, -43.12018560342360018, -23.49667901427708472 ) ) ;
#23446 = CARTESIAN_POINT ( 'NONE',  ( 5.896278296736517710, 12.98123568145678774, 15.36276341667920420 ) ) ;
#23447 = ORIENTED_EDGE ( 'NONE', *, *, #38321, .F. ) ;
#23448 = FACE_OUTER_BOUND ( 'NONE', #38121, .T. ) ;
#23449 = VERTEX_POINT ( 'NONE', #18399 ) ;
#23450 = CARTESIAN_POINT ( 'NONE',  ( 3.782625744892851749, 42.00313906590235291, -1.724648574484051622 ) ) ;
#23451 = EDGE_CURVE ( 'NONE', #20684, #14890, #36599, .T. ) ;
#23452 = ORIENTED_EDGE ( 'NONE', *, *, #57592, .T. ) ;
#23453 = VERTEX_POINT ( 'NONE', #37520 ) ;
#23454 = CARTESIAN_POINT ( 'NONE',  ( 1.157643937452369487, 28.54093992520408563, -30.69881142293044718 ) ) ;
#23455 = CARTESIAN_POINT ( 'NONE',  ( 0.6845945791218023269, -24.50629722879055450, 39.99809891542494000 ) ) ;
#23456 = CARTESIAN_POINT ( 'NONE',  ( 2.533389852662419894, -28.66318653646339953, -33.40467436317140937 ) ) ;
#23457 = VERTEX_POINT ( 'NONE', #14020 ) ;
#23458 = CARTESIAN_POINT ( 'NONE',  ( 2.643462169533613793, 19.65219740572127094, 43.83256147628741672 ) ) ;
#23459 = CARTESIAN_POINT ( 'NONE',  ( -90.00000000000000000, 0.000000000000000000, -5.000000000000000888 ) ) ;
#23460 = EDGE_CURVE ( 'NONE', #36253, #56952, #3648, .T. ) ;
#23461 = EDGE_LOOP ( 'NONE', ( #30666, #38837, #58549, #3238 ) ) ;
#23462 = ORIENTED_EDGE ( 'NONE', *, *, #7655, .T. ) ;
#23463 = CARTESIAN_POINT ( 'NONE',  ( -6.016489644550736315, -2.463898142942639424, -18.68142234211826747 ) ) ;
#23464 = CARTESIAN_POINT ( 'NONE',  ( 2.624215991343608501, 45.98641578154030185, 13.78323291683799212 ) ) ;
#23465 = DIRECTION ( 'NONE',  ( 2.168404344971009361E-16, -1.000000000000000000, 0.000000000000000000 ) ) ;
#23466 = CARTESIAN_POINT ( 'NONE',  ( 4.694002226626920127, 45.16857381419794848, -6.171281150416436212 ) ) ;
#23468 = VECTOR ( 'NONE', #61492, 1000.000000000000000 ) ;
#23467 = CARTESIAN_POINT ( 'NONE',  ( 0.8760168074887076939, 42.09738177923922819, 23.27577685234612304 ) ) ;
#23469 = ORIENTED_EDGE ( 'NONE', *, *, #57047, .T. ) ;
#23470 = ORIENTED_EDGE ( 'NONE', *, *, #8440, .F. ) ;
#23471 = LINE ( 'NONE', #42603, #25343 ) ;
#23472 = CARTESIAN_POINT ( 'NONE',  ( 0.7048096507298579061, 37.64898672361912446, 29.95256433478738600 ) ) ;
#23473 = CIRCLE ( 'NONE', #24457, 42.08604991992415023 ) ;
#23474 = DIRECTION ( 'NONE',  ( 0.000000000000000000, 0.000000000000000000, 1.000000000000000000 ) ) ;
#23475 = CARTESIAN_POINT ( 'NONE',  ( 0.5786265663353153954, 5.535668456754629041, -47.58023467411533147 ) ) ;
#23476 = CARTESIAN_POINT ( 'NONE',  ( 2.624215991343608501, -44.87417713512100192, 17.05978231157389047 ) ) ;
#23477 = VERTEX_POINT ( 'NONE', #60660 ) ;
#23478 = CARTESIAN_POINT ( 'NONE',  ( 4.956653778116475451, 47.27023054223744225, 8.845409907520236814 ) ) ;
#23479 = DIRECTION ( 'NONE',  ( -0.07500201931887529039, 0.8510178133413054402, -0.5197531899602676475 ) ) ;
#23480 = EDGE_CURVE ( 'NONE', #40820, #28284, #19393, .T. ) ;
#23481 = CARTESIAN_POINT ( 'NONE',  ( 5.981074661064941900, -20.35019299530686610, -2.670494474391926332 ) ) ;
#23482 = CARTESIAN_POINT ( 'NONE',  ( 0.6039202388192953519, 22.55960655125616299, -43.61912269981493750 ) ) ;
#23483 = CARTESIAN_POINT ( 'NONE',  ( 0.8551540677456834771, 19.17641535420853316, 43.91216198251545677 ) ) ;
#23484 = EDGE_CURVE ( 'NONE', #1947, #331, #2154, .T. ) ;
#23485 = FACE_BOUND ( 'NONE', #52507, .T. ) ;
#23486 = FACE_OUTER_BOUND ( 'NONE', #3719, .T. ) ;
#23487 = VECTOR ( 'NONE', #60292, 1000.000000000000000 ) ;
#23488 = B_SPLINE_CURVE_WITH_KNOTS ( 'NONE', 3,
 ( #47021, #57291, #4055, #13498 ),
 .UNSPECIFIED., .F., .F.,
 ( 4, 4 ),
 ( 2.168404344971008868E-19, 0.004041751736740988206 ),
 .UNSPECIFIED. ) ;
#23489 = CARTESIAN_POINT ( 'NONE',  ( -6.077587904424778920, -12.95044751835525609, -14.25068175450762809 ) ) ;
#23490 = ORIENTED_EDGE ( 'NONE', *, *, #50720, .F. ) ;
#23491 = CARTESIAN_POINT ( 'NONE',  ( 5.901764892641288895, -48.87142464753282667, -3.094401454271686447 ) ) ;
#23492 = CARTESIAN_POINT ( 'NONE',  ( 0.8560838555295223751, -29.58154842764516701, 36.40473632241573654 ) ) ;
#23493 = B_SPLINE_CURVE_WITH_KNOTS ( 'NONE', 3,
 ( #15469, #29244, #6028, #34580 ),
 .UNSPECIFIED., .F., .F.,
 ( 4, 4 ),
 ( 0.000000000000000000, 0.004042984057420971958 ),
 .UNSPECIFIED. ) ;
#23494 = CARTESIAN_POINT ( 'NONE',  ( -6.016489644550737204, -4.872725758886062408, -18.20227673842149585 ) ) ;
#23495 = CARTESIAN_POINT ( 'NONE',  ( 4.958415959904820092, -16.79601473596521544, -42.20305489904586693 ) ) ;
#23496 = VERTEX_POINT ( 'NONE', #28709 ) ;
#23497 = ADVANCED_FACE ( 'NONE', ( #29624 ), #76, .F. ) ;
#23498 = CARTESIAN_POINT ( 'NONE',  ( 0.8554163680231720024, -45.78608427674281955, 10.23913862172123679 ) ) ;
#23499 = CARTESIAN_POINT ( 'NONE',  ( 5.896782393890504181, -15.78847575145207038, -12.45994062280484016 ) ) ;
#23500 =( BOUNDED_SURFACE ( )  B_SPLINE_SURFACE ( 3, 1, ( 
 ( #16464, #26167 ),
 ( #18636, #43070 ),
 ( #42454, #32117 ),
 ( #57122, #57422 ) ),
 .UNSPECIFIED., .F., .F., .F. ) 
 B_SPLINE_SURFACE_WITH_KNOTS ( ( 4, 4 ),
 ( 2, 2 ),
 ( 0.000000000000000000, 1.000000000000000000 ),
 ( 0.000000000000000000, 1.000000000000000000 ),
 .UNSPECIFIED. ) 
 GEOMETRIC_REPRESENTATION_ITEM ( )  RATIONAL_B_SPLINE_SURFACE ( (
 ( 1.000000000000000000, 1.000000000000000000),
 ( 0.7211978278499970862, 0.9934217856018976445),
 ( 0.7211978278499970862, 0.9934217856018976445),
 ( 1.000000000000000000, 1.000000000000000000) ) ) 
 REPRESENTATION_ITEM ( '' )  SURFACE ( )  );
#23501 = ORIENTED_EDGE ( 'NONE', *, *, #18436, .T. ) ;
#23502 = DIRECTION ( 'NONE',  ( -0.1011922191286467598, 0.7895409829358833731, 0.6052975888374734215 ) ) ;
#23503 = CARTESIAN_POINT ( 'NONE',  ( 0.5837157313716038187, -45.93808755675273403, -9.430226678619181513 ) ) ;
#23504 = CARTESIAN_POINT ( 'NONE',  ( 0.6001305935487315502, -5.760103278697686235, -47.76436356026965768 ) ) ;
#23505 = ORIENTED_EDGE ( 'NONE', *, *, #7847, .T. ) ;
#23506 = B_SPLINE_CURVE_WITH_KNOTS ( 'NONE', 3,
 ( #10823, #35254, #6376, #44655, #1694, #39973, #59024, #54310, #11433, #50255, #7959, #22368, #41498, #13291, #32090, #45576 ),
 .UNSPECIFIED., .F., .F.,
 ( 4, 3, 3, 3, 3, 4 ),
 ( 3.469446951953614189E-18, 0.0002724568934985621064, 0.0004086836638483854595, 0.0005449104342063774628, 0.0008173270854453849963, 0.001089761613562692478 ),
 .UNSPECIFIED. ) ;
#23507 = CARTESIAN_POINT ( 'NONE',  ( 4.963659409799326738, -14.83726297270310823, 42.22332985082307744 ) ) ;
#23508 = VECTOR ( 'NONE', #17413, 1000.000000000000227 ) ;
#23509 = ORIENTED_EDGE ( 'NONE', *, *, #41247, .T. ) ;
#23510 = VERTEX_POINT ( 'NONE', #43451 ) ;
#23511 = CARTESIAN_POINT ( 'NONE',  ( 0.5832367798473389042, -5.981481162905404325, -47.52096797443093834 ) ) ;
#23512 = CARTESIAN_POINT ( 'NONE',  ( 4.956653778116966613, 0.000000000000000000, 0.000000000000000000 ) ) ;
#23513 = ORIENTED_EDGE ( 'NONE', *, *, #605, .T. ) ;
#23514 = CARTESIAN_POINT ( 'NONE',  ( 3.660176727303398714, 27.72864483302518224, 39.22755245663856982 ) ) ;
#23515 = VECTOR ( 'NONE', #5406, 1000.000000000000114 ) ;
#23516 = ORIENTED_EDGE ( 'NONE', *, *, #9631, .T. ) ;
#23517 = CARTESIAN_POINT ( 'NONE',  ( 0.5827357941260203900, 0.3632531319014370430, 47.89462047563813485 ) ) ;
#23518 =( BOUNDED_SURFACE ( )  B_SPLINE_SURFACE ( 3, 1, ( 
 ( #24487, #9770 ),
 ( #53287, #53899 ),
 ( #48913, #43625 ),
 ( #668, #19808 ) ),
 .UNSPECIFIED., .F., .F., .F. ) 
 B_SPLINE_SURFACE_WITH_KNOTS ( ( 4, 4 ),
 ( 2, 2 ),
 ( 0.000000000000000000, 1.000000000000000000 ),
 ( 0.000000000000000000, 1.000000000000000000 ),
 .UNSPECIFIED. ) 
 GEOMETRIC_REPRESENTATION_ITEM ( )  RATIONAL_B_SPLINE_SURFACE ( (
 ( 1.000000000000000000, 1.000000000000000000),
 ( 0.9953040768229013402, 0.8617119497784988535),
 ( 0.9953040768229013402, 0.8617119497784988535),
 ( 1.000000000000000000, 1.000000000000000000) ) ) 
 REPRESENTATION_ITEM ( '' )  SURFACE ( )  );
#23519 = CARTESIAN_POINT ( 'NONE',  ( 0.1129192098497455998, -0.9297496242496093855, -44.11448008785053787 ) ) ;
#23520 = VERTEX_POINT ( 'NONE', #4565 ) ;
#23521 = CARTESIAN_POINT ( 'NONE',  ( 0.9758171775293917882, -16.42583507057837622, -39.64000636436379210 ) ) ;
#23522 = CARTESIAN_POINT ( 'NONE',  ( 0.5848930533535030563, -41.77346544155656005, 21.31315714272848538 ) ) ;
#23523 = CARTESIAN_POINT ( 'NONE',  ( 0.5837800005270540327, 16.85481827636133545, 43.76243091411424047 ) ) ;
#23524 = ORIENTED_EDGE ( 'NONE', *, *, #43626, .F. ) ;
#23525 = CARTESIAN_POINT ( 'NONE',  ( 5.959828726073459926, -5.308046411395112685, -19.82738831247212019 ) ) ;
#23526 = CARTESIAN_POINT ( 'NONE',  ( 0.5850706913938533704, -29.01314519953773186, -38.10903744847171026 ) ) ;
#23527 = B_SPLINE_CURVE_WITH_KNOTS ( 'NONE', 3,
 ( #27321, #32969, #4713, #4402 ),
 .UNSPECIFIED., .F., .F.,
 ( 4, 4 ),
 ( 2.297383214701472214E-17, 0.004564976165746187711 ),
 .UNSPECIFIED. ) ;
#23528 = ORIENTED_EDGE ( 'NONE', *, *, #49097, .T. ) ;
#23529 = CARTESIAN_POINT ( 'NONE',  ( 5.960721111146673579, -16.28018152803701213, 12.50019045452710742 ) ) ;
#23530 = EDGE_CURVE ( 'NONE', #61531, #19087, #32826, .T. ) ;
#23531 = B_SPLINE_CURVE_WITH_KNOTS ( 'NONE', 3,
 ( #32319, #27610, #46126, #22300, #40821, #46427, #45819, #3172, #16675, #50486, #41735, #60486, #17602, #17921, #2863, #55795, #37041, #42969, #23839 ),
 .UNSPECIFIED., .F., .F.,
 ( 4, 3, 3, 3, 3, 3, 4 ),
 ( 1.355252715606880543E-20, 0.0002612768053151702996, 0.0003919133833142921181, 0.0005225499612322598861, 0.0006531865391693344406, 0.0008112755173415187732, 0.0009693688056799728983 ),
 .UNSPECIFIED. ) ;
#23532 = EDGE_LOOP ( 'NONE', ( #14229, #11429, #52645, #2686 ) ) ;
#23533 = CARTESIAN_POINT ( 'NONE',  ( 3.661933894777871679, -21.49232232567767653, 41.84150147880487225 ) ) ;
#23534 = APPLICATION_CONTEXT ( 'automotive_design' ) ;
#23535 = CARTESIAN_POINT ( 'NONE',  ( -6.016761891674565099, 11.47373234755524862, -14.94721834528402660 ) ) ;
#23536 = VERTEX_POINT ( 'NONE', #24320 ) ;
#23537 = CARTESIAN_POINT ( 'NONE',  ( 0.2230388203127589286, -37.71673103297349883, -20.89822698305252402 ) ) ;
#23538 = CARTESIAN_POINT ( 'NONE',  ( 0.7044674535453004927, 33.63530026269737050, 35.78364569253805882 ) ) ;
#23539 = ADVANCED_FACE ( 'NONE', ( #19323 ), #35985, .F. ) ;
#23540 = DIRECTION ( 'NONE',  ( 0.000000000000000000, 0.000000000000000000, 1.000000000000000000 ) ) ;
#23541 = CARTESIAN_POINT ( 'NONE',  ( 0.5817216825391118284, -2.022013777143747859, -46.85238961347116060 ) ) ;
#23542 = VERTEX_POINT ( 'NONE', #61888 ) ;
#23543 = CARTESIAN_POINT ( 'NONE',  ( 0.9730545539215883499, 41.57420493492384850, 10.61654491617579055 ) ) ;
#23544 = CARTESIAN_POINT ( 'NONE',  ( 0.8551540677456715978, -41.03346287276445992, 24.74404575822761032 ) ) ;
#23545 = CARTESIAN_POINT ( 'NONE',  ( 3.782542959838396168, -41.79414908755126135, -4.526251809622206856 ) ) ;
#23546 = CARTESIAN_POINT ( 'NONE',  ( 0.5838002273316419410, -44.19779719735685575, -18.45474575185561505 ) ) ;
#23547 = CARTESIAN_POINT ( 'NONE',  ( -6.078726893082806448, 9.979253153318763836, 16.46841060244423360 ) ) ;
#23548 = CARTESIAN_POINT ( 'NONE',  ( 0.6001305935487315502, 41.40054608060292907, -24.50730504006414634 ) ) ;
#23549 = VECTOR ( 'NONE', #37411, 1000.000000000000114 ) ;
#23550 = CARTESIAN_POINT ( 'NONE',  ( 0.8744876279028263033, -45.16590161814997373, -19.24555484778471026 ) ) ;
#23551 = EDGE_CURVE ( 'NONE', #35170, #1703, #52985, .T. ) ;
#23552 = CARTESIAN_POINT ( 'NONE',  ( 42.00000000000000711, 16.00000000000000355, -1.502225356622044491E-30 ) ) ;
#23553 = CIRCLE ( 'NONE', #60518, 42.08604991992415023 ) ;
#23554 = CARTESIAN_POINT ( 'NONE',  ( 0.5837800005270556980, 40.34938032117881335, -23.89901182766041643 ) ) ;
#23555 = EDGE_CURVE ( 'NONE', #19529, #58674, #12635, .T. ) ;
#23556 = CARTESIAN_POINT ( 'NONE',  ( -15.25000000000000711, -2.688986455804108555, -9.952330921218299798E-16 ) ) ;
#23557 = CARTESIAN_POINT ( 'NONE',  ( 0.9730545539215883499, 30.69604515769692554, -29.98130006528829483 ) ) ;
#23558 = VECTOR ( 'NONE', #15778, 1000.000000000000114 ) ;
#23559 = DIRECTION ( 'NONE',  ( 0.000000000000000000, 0.000000000000000000, 1.000000000000000000 ) ) ;
#23560 = CARTESIAN_POINT ( 'NONE',  ( 0.5997462898726536595, -42.52950339524468859, -24.55184251941555118 ) ) ;
#23561 = CARTESIAN_POINT ( 'NONE',  ( 0.9752132459055854463, 37.27572867006962554, 21.25214916889604666 ) ) ;
#23562 = CARTESIAN_POINT ( 'NONE',  ( 0.5804410086790514622, 17.36461428077188174, -43.56592731407666008 ) ) ;
#23563 = EDGE_CURVE ( 'NONE', #4858, #42220, #38442, .T. ) ;
#23564 = CARTESIAN_POINT ( 'NONE',  ( 0.8551540677456715978, -23.16399837394575556, 41.94570365541196111 ) ) ;
#23565 = CARTESIAN_POINT ( 'NONE',  ( 3.680974057930773924, 10.62112035260176945, 46.78530430706942411 ) ) ;
#23566 = CARTESIAN_POINT ( 'NONE',  ( 0.1139756605157203478, 37.19545956418076571, 23.73716511094820092 ) ) ;
#23568 = EDGE_LOOP ( 'NONE', ( #52271, #9737, #47648, #49736 ) ) ;
#23567 = CARTESIAN_POINT ( 'NONE',  ( 0.9754642270333695464, 39.57465882553928793, 16.58255499746090322 ) ) ;
#23569 = CARTESIAN_POINT ( 'NONE',  ( 0.6008122571543325074, -39.09350205120696131, 29.71956675050282470 ) ) ;
#23570 = CARTESIAN_POINT ( 'NONE',  ( 0.5797568599927146460, -19.16764036586056363, -42.79984662911815008 ) ) ;
#23571 = CARTESIAN_POINT ( 'NONE',  ( 5.896782393890504181, -2.019528367549316084, -20.01118667272572793 ) ) ;
#23572 = EDGE_LOOP ( 'NONE', ( #55713, #33798, #39352, #42783 ) ) ;
#23573 = EDGE_CURVE ( 'NONE', #52918, #45306, #60401, .T. ) ;
#23574 = FACE_OUTER_BOUND ( 'NONE', #46921, .T. ) ;
#23575 = CARTESIAN_POINT ( 'NONE',  ( 0.5804410086790514622, 36.46521478791906645, 29.49250688439903811 ) ) ;
#23576 = B_SPLINE_CURVE_WITH_KNOTS ( 'NONE', 3,
 ( #31978, #41096, #51059, #8153 ),
 .UNSPECIFIED., .F., .F.,
 ( 4, 4 ),
 ( 0.000000000000000000, 0.004442905043737213969 ),
 .UNSPECIFIED. ) ;
#23577 = UNCERTAINTY_MEASURE_WITH_UNIT (LENGTH_MEASURE( 1.000000000000000082E-05 ), #58512, 'distance_accuracy_value', 'NONE');
#23578 = ORIENTED_EDGE ( 'NONE', *, *, #56692, .T. ) ;
#23579 = ORIENTED_EDGE ( 'NONE', *, *, #41689, .T. ) ;
#23580 = B_SPLINE_CURVE_WITH_KNOTS ( 'NONE', 3,
 ( #21020, #40161, #59208, #40771 ),
 .UNSPECIFIED., .F., .F.,
 ( 4, 4 ),
 ( 5.553824967135426632E-18, 0.004566006591234644633 ),
 .UNSPECIFIED. ) ;
#23581 = CARTESIAN_POINT ( 'NONE',  ( 0.5997462898726536595, 37.72933316221968170, 31.43324751403423534 ) ) ;
#23582 = ORIENTED_EDGE ( 'NONE', *, *, #51323, .T. ) ;
#23583 = CARTESIAN_POINT ( 'NONE',  ( 4.549368137175248350, 0.000000000000000000, 0.000000000000000000 ) ) ;
#23584 = CARTESIAN_POINT ( 'NONE',  ( 0.9762797500689124330, 25.26481495167865532, 33.43671500974846822 ) ) ;
#23585 = ORIENTED_EDGE ( 'NONE', *, *, #43586, .T. ) ;
#23586 = ORIENTED_EDGE ( 'NONE', *, *, #12776, .F. ) ;
#23587 = CARTESIAN_POINT ( 'NONE',  ( 4.975610109902397937, -23.13264022976521161, -43.09675583078175265 ) ) ;
#23588 = ORIENTED_EDGE ( 'NONE', *, *, #6617, .F. ) ;
#23589 = CARTESIAN_POINT ( 'NONE',  ( 0.6000166863083090663, 33.40185771989303731, -36.00193581695955913 ) ) ;
#23590 = CARTESIAN_POINT ( 'NONE',  ( 0.8753041380234471980, 21.91949880997691480, 43.93943445007457171 ) ) ;
#23591 = CARTESIAN_POINT ( 'NONE',  ( 0.1087620492084205026, -30.23658359364800319, -30.74858804150676050 ) ) ;
#23592 = ORIENTED_EDGE ( 'NONE', *, *, #37834, .T. ) ;
#23593 = FACE_OUTER_BOUND ( 'NONE', #54792, .T. ) ;
#23594 = CARTESIAN_POINT ( 'NONE',  ( 0.9790850452238870627, -39.57319415496242243, 13.79491336097644805 ) ) ;
#23595 = VERTEX_POINT ( 'NONE', #58423 ) ;
#23596 = VERTEX_POINT ( 'NONE', #33122 ) ;
#23597 = ADVANCED_FACE ( 'NONE', ( #2030 ), #40560, .F. ) ;
#23598 = CARTESIAN_POINT ( 'NONE',  ( 3.376099380956838925, 5.244649644334623773, -12.33701883520681974 ) ) ;
#23599 = VECTOR ( 'NONE', #11823, 1000.000000000000000 ) ;
#23600 = VERTEX_POINT ( 'NONE', #30543 ) ;
#23601 = CARTESIAN_POINT ( 'NONE',  ( 1.296416391601052931, 34.26782981329887434, 27.71323174880446416 ) ) ;
#23602 = DIRECTION ( 'NONE',  ( -1.000000000000000000, -0.000000000000000000, -0.000000000000000000 ) ) ;
#23603 = CARTESIAN_POINT ( 'NONE',  ( 5.958863334805807099, 16.28335246510350842, 12.49619391867187801 ) ) ;
#23604 = CARTESIAN_POINT ( 'NONE',  ( 0.1100247026804066219, 5.460606496326332326, 42.77732815928602150 ) ) ;
#23605 = CARTESIAN_POINT ( 'NONE',  ( 4.549368137175248350, 28.46244473166673927, -32.13400537129894730 ) ) ;
#23606 = ADVANCED_FACE ( 'NONE', ( #49974 ), #21330, .F. ) ;
#23607 = AXIS2_PLACEMENT_3D ( 'NONE', #47999, #44246, #53587 ) ;
#23608 = ORIENTED_EDGE ( 'NONE', *, *, #34873, .T. ) ;
#23609 = LINE ( 'NONE', #4779, #879 ) ;
#23610 = CARTESIAN_POINT ( 'NONE',  ( 0.5806925824938499181, 46.54710689580866756, -5.708695295225145294 ) ) ;
#23611 = EDGE_CURVE ( 'NONE', #10962, #16304, #16385, .T. ) ;
#23612 = CARTESIAN_POINT ( 'NONE',  ( 0.8554163680231816613, -44.61245466728215092, -14.52357950615188997 ) ) ;
#23613 = ORIENTED_EDGE ( 'NONE', *, *, #51058, .T. ) ;
#23614 = DIRECTION ( 'NONE',  ( 1.000000000000000000, 1.836909530733573776E-16, -1.925929944387235853E-32 ) ) ;
#23615 = EDGE_CURVE ( 'NONE', #6126, #58704, #27589, .T. ) ;
#23616 = CARTESIAN_POINT ( 'NONE',  ( 4.549368137175248350, 0.000000000000000000, 0.000000000000000000 ) ) ;
#23617 = CARTESIAN_POINT ( 'NONE',  ( 2.281448460670560952, -4.956513608981508945, 47.71650330356585101 ) ) ;
#23618 = AXIS2_PLACEMENT_3D ( 'NONE', #2820, #60147, #44548 ) ;
#23619 = ORIENTED_EDGE ( 'NONE', *, *, #55948, .F. ) ;
#23620 = EDGE_LOOP ( 'NONE', ( #11998, #52864, #55257, #20365 ) ) ;
#23621 = LINE ( 'NONE', #48353, #27892 ) ;
#23622 = DIRECTION ( 'NONE',  ( 0.000000000000000000, 0.000000000000000000, 1.000000000000000000 ) ) ;
#23623 = DIRECTION ( 'NONE',  ( 0.000000000000000000, 0.000000000000000000, 1.000000000000000000 ) ) ;
#23624 = CARTESIAN_POINT ( 'NONE',  ( 2.648799415243696664, -43.38879977521501985, 22.84577679475794199 ) ) ;
#23625 = CARTESIAN_POINT ( 'NONE',  ( 3.783278058412224976, 7.325100730114287195, 42.41041238787298084 ) ) ;
#23626 = CARTESIAN_POINT ( 'NONE',  ( 0.1129192098497455998, -17.41650932123162931, -40.54154647825617275 ) ) ;
#23627 = CARTESIAN_POINT ( 'NONE',  ( 5.965394784446460541, 10.27521535480986614, -17.76824826579344574 ) ) ;
#23628 = DIRECTION ( 'NONE',  ( 1.000000000000000000, 1.836909530733573776E-16, -1.925929944387235579E-32 ) ) ;
#23629 =( BOUNDED_SURFACE ( )  B_SPLINE_SURFACE ( 3, 1, ( 
 ( #7950, #2934 ),
 ( #12063, #46187 ),
 ( #36172, #22361 ),
 ( #31138, #50246 ) ),
 .UNSPECIFIED., .F., .F., .F. ) 
 B_SPLINE_SURFACE_WITH_KNOTS ( ( 4, 4 ),
 ( 2, 2 ),
 ( 0.000000000000000000, 1.000000000000000000 ),
 ( 0.000000000000000000, 1.000000000000000000 ),
 .UNSPECIFIED. ) 
 GEOMETRIC_REPRESENTATION_ITEM ( )  RATIONAL_B_SPLINE_SURFACE ( (
 ( 1.000000000000000000, 1.000000000000000000),
 ( 0.9953485035131437453, 0.8621029689291515030),
 ( 0.9953485035131437453, 0.8621029689291515030),
 ( 1.000000000000000000, 1.000000000000000000) ) ) 
 REPRESENTATION_ITEM ( '' )  SURFACE ( )  );
#23630 = CARTESIAN_POINT ( 'NONE',  ( 4.833616638992205949, -14.43699082351681540, -43.93936707042095691 ) ) ;
#23631 = DIRECTION ( 'NONE',  ( -1.000000000000000000, -0.000000000000000000, -0.000000000000000000 ) ) ;
#23632 = EDGE_CURVE ( 'NONE', #18593, #9726, #38826, .T. ) ;
#23633 = CARTESIAN_POINT ( 'NONE',  ( -6.010958268070873523, 2.473955915502482394, -18.68034667844846552 ) ) ;
#23634 = CARTESIAN_POINT ( 'NONE',  ( 0.8760168074886965917, -44.09317760313739143, -19.22870327415289182 ) ) ;
#23635 = ORIENTED_EDGE ( 'NONE', *, *, #23341, .F. ) ;
#23636 = EDGE_CURVE ( 'NONE', #35697, #33056, #16973, .T. ) ;
#23637 = CARTESIAN_POINT ( 'NONE',  ( 45.00000000000001421, 0.000000000000000000, 0.000000000000000000 ) ) ;
#23638 = CARTESIAN_POINT ( 'NONE',  ( 0.3676999524040323597, 19.66859742988730986, 39.48540057367873857 ) ) ;
#23639 = CARTESIAN_POINT ( 'NONE',  ( 5.981074661064941900, 5.303881226583676778, -19.82752479807522406 ) ) ;
#23640 = CARTESIAN_POINT ( 'NONE',  ( -6.015611763856276717, -0.006214430185009750529, -18.84324252354755203 ) ) ;
#23641 = CARTESIAN_POINT ( 'NONE',  ( 4.999999999999986677, 54.69470952477936976, 58.44237546506825964 ) ) ;
#23642 = CARTESIAN_POINT ( 'NONE',  ( 0.7048096507298579061, 44.11842270945945899, 19.18768066167137576 ) ) ;
#23643 = ITEM_DEFINED_TRANSFORMATION ( 'NONE', 'NONE', #5836,  #14677 ) ;
#23644 = DIRECTION ( 'NONE',  ( 0.000000000000000000, 0.000000000000000000, -1.000000000000000000 ) ) ;
#23645 = EDGE_CURVE ( 'NONE', #38027, #3479, #27019, .T. ) ;
#23646 = CARTESIAN_POINT ( 'NONE',  ( 0.6029443449137436017, 48.21014671922638684, -9.344586202395333885 ) ) ;
#23647 = CARTESIAN_POINT ( 'NONE',  ( 0.5827359174754831450, 12.04517879102136924, 46.35666395585276689 ) ) ;
#23648 = AXIS2_PLACEMENT_3D ( 'NONE', #16000, #49493, #15694 ) ;
#23649 = CARTESIAN_POINT ( 'NONE',  ( 4.975801465491695552, 45.18341283946458020, -15.94009207553003016 ) ) ;
#23651 = VERTEX_POINT ( 'NONE', #15855 ) ;
#23650 = CARTESIAN_POINT ( 'NONE',  ( 3.407937589446174087, -11.62731850632879116, -7.243367523631146554 ) ) ;
#23652 = ORIENTED_EDGE ( 'NONE', *, *, #58391, .F. ) ;
#23653 = CARTESIAN_POINT ( 'NONE',  ( 0.3676999524040366896, 42.11837424242170158, 13.11461530118771179 ) ) ;
#23654 = CARTESIAN_POINT ( 'NONE',  ( 5.901463166500146684, 5.945065151443822415, -19.21390305705025270 ) ) ;
#23655 = AXIS2_PLACEMENT_3D ( 'NONE', #28769, #61339, #37269 ) ;
#23656 = CARTESIAN_POINT ( 'NONE',  ( 3.678748215320120085, -48.30244781633944484, 8.092363637979213209 ) ) ;
#23657 = EDGE_CURVE ( 'NONE', #8619, #52291, #35045, .T. ) ;
#23658 = EDGE_LOOP ( 'NONE', ( #26044, #36485, #19381, #36696 ) ) ;
#23659 = LINE ( 'NONE', #42784, #3483 ) ;
#23660 = CYLINDRICAL_SURFACE ( 'NONE', #6135, 13.00000000000000178 ) ;
#23661 = CARTESIAN_POINT ( 'NONE',  ( 0.1103744047535531458, 5.667281528142393832, -42.75042227379822180 ) ) ;
#23663 = EDGE_CURVE ( 'NONE', #58552, #12007, #24597, .T. ) ;
#23662 = ORIENTED_EDGE ( 'NONE', *, *, #404, .T. ) ;
#23664 = ORIENTED_EDGE ( 'NONE', *, *, #36444, .T. ) ;
#23665 = SURFACE_SIDE_STYLE ('',( #46878 ) ) ;
#23666 = VECTOR ( 'NONE', #42012, 1000.000000000000114 ) ;
#23667 = CARTESIAN_POINT ( 'NONE',  ( 2.533389852662419894, -40.17945474350555912, 17.97392411935152978 ) ) ;
#23668 = CARTESIAN_POINT ( 'NONE',  ( 4.834790513006553603, 29.09828987666518429, 37.22739404226336291 ) ) ;
#23669 = DIRECTION ( 'NONE',  ( -1.000000000000000000, -0.000000000000000000, -0.000000000000000000 ) ) ;
#23670 = CARTESIAN_POINT ( 'NONE',  ( 0.8744876279028306332, 48.01195819035234535, -10.25679877482985169 ) ) ;
#23671 = CARTESIAN_POINT ( 'NONE',  ( 0.5809828226811553087, 37.66417181417592275, -29.58751527316140795 ) ) ;
#23672 = VERTEX_POINT ( 'NONE', #50891 ) ;
#23673 = DIRECTION ( 'NONE',  ( -1.000000000000000000, -0.000000000000000000, -0.000000000000000000 ) ) ;
#23674 = CARTESIAN_POINT ( 'NONE',  ( -6.001507490154110336, 13.31361390284178370, -13.33564355450094396 ) ) ;
#23675 = EDGE_LOOP ( 'NONE', ( #19424, #50331, #53026, #60044 ) ) ;
#23676 = CARTESIAN_POINT ( 'NONE',  ( -49.49999999999975842, 1.232595164407830946E-29, 1.078520768856852078E-29 ) ) ;
#23677 = CARTESIAN_POINT ( 'NONE',  ( 0.7056313189692706711, -0.7243877018920470423, 46.89588368305800259 ) ) ;
#23678 = CARTESIAN_POINT ( 'NONE',  ( 0.5998501479064708430, 46.33007877220720871, 12.95623334615518374 ) ) ;
#23679 = CARTESIAN_POINT ( 'NONE',  ( 0.5988103622719989083, -6.880137819455214299, 47.61318311633112188 ) ) ;
#23680 = EDGE_CURVE ( 'NONE', #8101, #32248, #8952, .T. ) ;
#23681 = ORIENTED_EDGE ( 'NONE', *, *, #53944, .F. ) ;
#23682 = VERTEX_POINT ( 'NONE', #3885 ) ;
#23683 = CARTESIAN_POINT ( 'NONE',  ( 0.1156495703730067576, -44.12396594495942281, 0.1363177139302391427 ) ) ;
#23684 = CARTESIAN_POINT ( 'NONE',  ( 5.896278296736517710, 5.964180709076918774, -19.20821511967883310 ) ) ;
#23685 = EDGE_CURVE ( 'NONE', #59114, #45338, #50006, .T. ) ;
#23686 = CARTESIAN_POINT ( 'NONE',  ( 4.956653778116995035, 36.51451553856460919, -31.29546495791814209 ) ) ;
#23687 = VERTEX_POINT ( 'NONE', #17093 ) ;
#23688 = CARTESIAN_POINT ( 'NONE',  ( 0.6008122571543325074, 4.281854884450230436, -48.92055058167095893 ) ) ;
#23689 = VECTOR ( 'NONE', #8907, 1000.000000000000114 ) ;
#23691 = ORIENTED_EDGE ( 'NONE', *, *, #18748, .F. ) ;
#23690 = EDGE_CURVE ( 'NONE', #47578, #39264, #20172, .T. ) ;
#23692 = CARTESIAN_POINT ( 'NONE',  ( 4.694002226626920127, -15.42074131724428376, 42.90088004543460443 ) ) ;
#23693 = CARTESIAN_POINT ( 'NONE',  ( 0.9762797500689124330, -18.09842611962761083, -37.79909730639192844 ) ) ;
#23694 = EDGE_CURVE ( 'NONE', #29824, #32705, #42591, .T. ) ;
#23695 = ORIENTED_EDGE ( 'NONE', *, *, #11690, .F. ) ;
#23696 = CARTESIAN_POINT ( 'NONE',  ( 0.5809828226811553087, -47.55412398569202281, -5.711058609465819558 ) ) ;
#23697 = CIRCLE ( 'NONE', #3681, 43.92652462719577500 ) ;
#23698 = EDGE_CURVE ( 'NONE', #45872, #12531, #53748, .T. ) ;
#23699 = CARTESIAN_POINT ( 'NONE',  ( 0.1129192098497447394, -27.13044910148925837, 34.79785222304180081 ) ) ;
#23700 = CARTESIAN_POINT ( 'NONE',  ( 0.9745511491811748028, 26.39034508612584062, -33.83313387735761779 ) ) ;
#23701 = EDGE_LOOP ( 'NONE', ( #12682, #48932, #26531, #36226 ) ) ;
#23702 = CARTESIAN_POINT ( 'NONE',  ( 0.5809828226811553087, -18.83114015454665946, -44.03860873105715967 ) ) ;
#23703 =( BOUNDED_SURFACE ( )  B_SPLINE_SURFACE ( 3, 1, ( 
 ( #35854, #40566 ),
 ( #55859, #12358 ),
 ( #17659, #2300 ),
 ( #26748, #3533 ) ),
 .UNSPECIFIED., .F., .F., .F. ) 
 B_SPLINE_SURFACE_WITH_KNOTS ( ( 4, 4 ),
 ( 2, 2 ),
 ( 0.000000000000000000, 1.000000000000000000 ),
 ( 0.000000000000000000, 1.000000000000000000 ),
 .UNSPECIFIED. ) 
 GEOMETRIC_REPRESENTATION_ITEM ( )  RATIONAL_B_SPLINE_SURFACE ( (
 ( 1.000000000000000000, 1.000000000000000000),
 ( 0.9732289882329797637, 0.9999525324661233672),
 ( 0.9732289882329797637, 0.9999525324661233672),
 ( 1.000000000000000000, 1.000000000000000000) ) ) 
 REPRESENTATION_ITEM ( '' )  SURFACE ( )  );
#23704 = CARTESIAN_POINT ( 'NONE',  ( 4.553261556744873317, -43.07273893850290136, 8.618510669437750238 ) ) ;
#23705 = DIRECTION ( 'NONE',  ( -1.000000000000000000, -0.000000000000000000, -0.000000000000000000 ) ) ;
#23706 = ADVANCED_FACE ( 'NONE', ( #27096 ), #46957, .F. ) ;
#23707 = CARTESIAN_POINT ( 'NONE',  ( 0.3676999524040323597, -7.853951980432424484, 43.40813312746703190 ) ) ;
#23708 = B_SPLINE_CURVE_WITH_KNOTS ( 'NONE', 3,
 ( #49350, #2342, #20855, #30857 ),
 .UNSPECIFIED., .F., .F.,
 ( 4, 4 ),
 ( 2.183987964099527011E-17, 0.004559932413162188537 ),
 .UNSPECIFIED. ) ;
#23709 = CARTESIAN_POINT ( 'NONE',  ( 3.680882792899937250, 10.62117075007648204, -46.78529781139678079 ) ) ;
#23710 = ORIENTED_EDGE ( 'NONE', *, *, #19107, .F. ) ;
#23711 = VECTOR ( 'NONE', #4132, 1000.000000000000114 ) ;
#23712 = CARTESIAN_POINT ( 'NONE',  ( 2.643462169533600914, -37.25264019563393703, -30.32726672320786676 ) ) ;
#23713 = CARTESIAN_POINT ( 'NONE',  ( 3.559346040607745287, -15.90101677405797531, 40.99497465657363904 ) ) ;
#23714 = VERTEX_POINT ( 'NONE', #32423 ) ;
#23715 = CARTESIAN_POINT ( 'NONE',  ( 0.6064515330803560422, 16.19003797393982680, -44.01382744592287111 ) ) ;
#23716 = CARTESIAN_POINT ( 'NONE',  ( 0.8760168074887090262, 28.57146030081980470, -38.69913431881793286 ) ) ;
#23717 = CARTESIAN_POINT ( 'NONE',  ( 5.896782393890504181, 14.92098591823861220, 13.48666994130638663 ) ) ;
#23718 = CARTESIAN_POINT ( 'NONE',  ( 0.2285344041767119194, 19.73012571914551572, -39.46166886235511839 ) ) ;
#23719 = DIRECTION ( 'NONE',  ( -1.000000000000000000, 0.000000000000000000, 0.000000000000000000 ) ) ;
#23720 = CARTESIAN_POINT ( 'NONE',  ( 4.962356264823608143, 0.000000000000000000, 0.000000000000000000 ) ) ;
#23721 = VECTOR ( 'NONE', #59450, 1000.000000000000000 ) ;
#23722 = CARTESIAN_POINT ( 'NONE',  ( 0.5837374860065642768, -47.89569815517035067, 0.1816420316513765454 ) ) ;
#23723 = DIRECTION ( 'NONE',  ( 1.000000000000000000, 0.000000000000000000, 0.000000000000000000 ) ) ;
#23724 = CARTESIAN_POINT ( 'NONE',  ( 0.5806925824938502512, 11.40214825760292250, 45.48860711711456872 ) ) ;
#23725 = CARTESIAN_POINT ( 'NONE',  ( 0.8753041380234530822, -29.91468680897855492, 38.93905290314216927 ) ) ;
#23726 = CARTESIAN_POINT ( 'NONE',  ( 1.227938101723748288, -39.96870412324346944, 15.63977281655828300 ) ) ;
#23727 = CARTESIAN_POINT ( 'NONE',  ( 0.3622758884714600280, 22.26738722580168073, -36.91764744403298693 ) ) ;
#23728 = VERTEX_POINT ( 'NONE', #41217 ) ;
#23729 = DIRECTION ( 'NONE',  ( -1.000000000000000000, -1.836909530733573776E-16, 1.925929944387235579E-32 ) ) ;
#23730 = CARTESIAN_POINT ( 'NONE',  ( 47.93459374525478722, 15.48572582901846140, -0.6863552170468703029 ) ) ;
#23731 = B_SPLINE_CURVE_WITH_KNOTS ( 'NONE', 3,
 ( #54887, #39911, #40843, #6324, #16084, #36133, #26703, #12317, #30158, #25459, #59904, #30461, #6630, #55196, #25779, #1956, #21082, #40225, #59275 ),
 .UNSPECIFIED., .F., .F.,
 ( 4, 3, 3, 3, 3, 3, 4 ),
 ( 1.138109825968292890E-16, 0.0002618519381806229352, 0.0003927759815485970052, 0.0005237000248299436469, 0.0006546240681325005356, 0.0007855481115631335765, 0.0009699050456655113756 ),
 .UNSPECIFIED. ) ;
#23732 = DIRECTION ( 'NONE',  ( 0.000000000000000000, 0.000000000000000000, 1.000000000000000000 ) ) ;
#23733 = CARTESIAN_POINT ( 'NONE',  ( 0.9757892942422828897, 42.53466646637867399, -5.651566539685394908 ) ) ;
#23734 = CARTESIAN_POINT ( 'NONE',  ( 1.231276596079881047, -41.87427716283725943, 1.954912557623087022 ) ) ;
#23735 = EDGE_CURVE ( 'NONE', #13776, #27177, #8276, .T. ) ;
#23736 = ORIENTED_EDGE ( 'NONE', *, *, #35691, .T. ) ;
#23737 = CIRCLE ( 'NONE', #34748, 0.1000000000000002554 ) ;
#23738 = CARTESIAN_POINT ( 'NONE',  ( -2.601141883200662974, -9.652501068366079906, -11.38528219213649173 ) ) ;
#23739 = AXIS2_PLACEMENT_3D ( 'NONE', #43596, #38899, #15077 ) ;
#23740 = CARTESIAN_POINT ( 'NONE',  ( -19.02812962168027511, -7.790324327006077354, -1.821248266840887364 ) ) ;
#23741 = AXIS2_PLACEMENT_3D ( 'NONE', #19616, #25220, #38736 ) ;
#23742 = CARTESIAN_POINT ( 'NONE',  ( 4.975801465491695552, 21.70134120755140827, 42.71626295676271212 ) ) ;
#23743 = ORIENTED_EDGE ( 'NONE', *, *, #3280, .T. ) ;
#23744 = B_SPLINE_CURVE_WITH_KNOTS ( 'NONE', 3,
 ( #18056, #50926, #3303, #46565 ),
 .UNSPECIFIED., .F., .F.,
 ( 4, 4 ),
 ( 0.002320612883253031153, 0.004444103432399267896 ),
 .UNSPECIFIED. ) ;
#23745 = CARTESIAN_POINT ( 'NONE',  ( 4.975801465491695552, 26.14269827151680659, -40.15204426031507268 ) ) ;
#23746 = CARTESIAN_POINT ( 'NONE',  ( 3.238018933889920792, 7.722174679335471303, -10.94419986063316763 ) ) ;
#23747 = EDGE_LOOP ( 'NONE', ( #47633, #1295, #58452, #30748 ) ) ;
#23748 = CARTESIAN_POINT ( 'NONE',  ( 0.7057020205115013267, 28.48867101281825498, 38.50899875908065439 ) ) ;
#23749 = ORIENTED_EDGE ( 'NONE', *, *, #59109, .F. ) ;
#23750 = CARTESIAN_POINT ( 'NONE',  ( 0.9972139404380298000, 42.90441115546387607, -0.6581143129161796113 ) ) ;
#23751 = ORIENTED_EDGE ( 'NONE', *, *, #59597, .F. ) ;
#23752 = CARTESIAN_POINT ( 'NONE',  ( 4.549368137175248350, 42.82045902618768451, 3.018832571116707442 ) ) ;
#23753 = CARTESIAN_POINT ( 'NONE',  ( 3.680882792899936362, -40.59250320379031507, 25.57189948075115637 ) ) ;
#23754 = CARTESIAN_POINT ( 'NONE',  ( 4.975610109902397937, -44.31543648230385202, -20.70245146161840211 ) ) ;
#23755 = DIRECTION ( 'NONE',  ( 0.9848077530122077983, 0.1736481776669316079, -1.387778780781445367E-17 ) ) ;
#23756 = ORIENTED_EDGE ( 'NONE', *, *, #2821, .T. ) ;
#23757 = CARTESIAN_POINT ( 'NONE',  ( 0.8751705887134423323, 29.98056538504960855, -37.60752970653798855 ) ) ;
#23758 = ADVANCED_FACE ( 'NONE', ( #13020 ), #49306, .F. ) ;
#23759 = VERTEX_POINT ( 'NONE', #18633 ) ;
#23760 = CARTESIAN_POINT ( 'NONE',  ( 0.6064515330803558202, -39.06165493752520490, -25.95229179819768106 ) ) ;
#23762 = ADVANCED_FACE ( 'NONE', ( #52122 ), #4094, .F. ) ;
#23761 = VERTEX_POINT ( 'NONE', #28627 ) ;
#23763 = CIRCLE ( 'NONE', #56789, 2.649999999999985700 ) ;
#23764 = ORIENTED_EDGE ( 'NONE', *, *, #5421, .T. ) ;
#23765 = FACE_BOUND ( 'NONE', #30585, .T. ) ;
#23766 = CARTESIAN_POINT ( 'NONE',  ( 0.9790724872846766624, -37.42248053063311630, 18.86513082159360621 ) ) ;
#23767 = EDGE_CURVE ( 'NONE', #7563, #14241, #58193, .T. ) ;
#23768 = CARTESIAN_POINT ( 'NONE',  ( 0.5809828226811553087, 46.40184912890838831, 11.86925843957183879 ) ) ;
#23769 = CARTESIAN_POINT ( 'NONE',  ( 2.359973842542475442, -28.61238109696261844, -33.45844501160621576 ) ) ;
#23770 = EDGE_LOOP ( 'NONE', ( #18091, #28523, #30716, #9970 ) ) ;
#23771 = EDGE_CURVE ( 'NONE', #61953, #1809, #105, .T. ) ;
#23772 = DIRECTION ( 'NONE',  ( 0.000000000000000000, 0.000000000000000000, 1.000000000000000000 ) ) ;
#23773 = CARTESIAN_POINT ( 'NONE',  ( 0.5786265663353153954, -38.43785771743185364, -28.58414684753526558 ) ) ;
#23774 = ORIENTED_EDGE ( 'NONE', *, *, #60365, .F. ) ;
#23775 = B_SPLINE_CURVE_WITH_KNOTS ( 'NONE', 3,
 ( #34416, #58800, #34725, #20921, #44453, #882, #48809, #49730, #5863, #2096, #30006, #44151, #40364, #59115, #35040, #1178 ),
 .UNSPECIFIED., .F., .F.,
 ( 4, 3, 3, 3, 3, 4 ),
 ( 1.301087781288862954E-17, 0.0002724568934985555470, 0.0004086836638483815022, 0.0005449104342063617419, 0.0008173270854453690585, 0.001089761613562690093 ),
 .UNSPECIFIED. ) ;
#23776 = ORIENTED_EDGE ( 'NONE', *, *, #38954, .T. ) ;
#23777 = CARTESIAN_POINT ( 'NONE',  ( 0.7948884756798503259, -49.09120184641267315, -0.8674940201074746726 ) ) ;
#23778 = DIRECTION ( 'NONE',  ( -1.000000000000000000, -0.000000000000000000, -0.000000000000000000 ) ) ;
#23779 = CARTESIAN_POINT ( 'NONE',  ( -2.708315649062916552, -13.41752550814514677, 5.842990691604369680 ) ) ;
#23780 = CARTESIAN_POINT ( 'NONE',  ( 0.5997462898726536595, 37.72933316222010802, -31.43324751403371664 ) ) ;
#23781 = CARTESIAN_POINT ( 'NONE',  ( 5.960721111146673579, 12.49016043756471284, -16.28787783074214701 ) ) ;
#23782 = VERTEX_POINT ( 'NONE', #15167 ) ;
#23783 =( BOUNDED_SURFACE ( )  B_SPLINE_SURFACE ( 3, 1, ( 
 ( #2390, #51238 ),
 ( #50621, #55317 ),
 ( #40652, #22441 ),
 ( #26831, #60628 ) ),
 .UNSPECIFIED., .F., .F., .F. ) 
 B_SPLINE_SURFACE_WITH_KNOTS ( ( 4, 4 ),
 ( 2, 2 ),
 ( 0.000000000000000000, 1.000000000000000000 ),
 ( 0.000000000000000000, 1.000000000000000000 ),
 .UNSPECIFIED. ) 
 GEOMETRIC_REPRESENTATION_ITEM ( )  RATIONAL_B_SPLINE_SURFACE ( (
 ( 1.000000000000000000, 1.000000000000000000),
 ( 0.7223157951917476005, 0.9931996967497186413),
 ( 0.7223157951917476005, 0.9931996967497186413),
 ( 1.000000000000000000, 1.000000000000000000) ) ) 
 REPRESENTATION_ITEM ( '' )  SURFACE ( )  );
#23784 = ADVANCED_FACE ( 'NONE', ( #24555 ), #8494, .F. ) ;
#23785 = VERTEX_POINT ( 'NONE', #14251 ) ;
#23786 = AXIS2_PLACEMENT_3D ( 'NONE', #18165, #23778, #22854 ) ;
#23787 = VECTOR ( 'NONE', #53190, 1000.000000000000114 ) ;
#23788 = ADVANCED_FACE ( 'NONE', ( #18950 ), #4491, .F. ) ;
#23789 = CARTESIAN_POINT ( 'NONE',  ( 0.7242003506639987931, -34.69774349674525382, 34.74303196844081754 ) ) ;
#23790 = CARTESIAN_POINT ( 'NONE',  ( 0.9780303403264775097, -41.00319591444414868, 8.664729551278226083 ) ) ;
#23791 = CARTESIAN_POINT ( 'NONE',  ( 0.3622758884714600280, -31.06363466427748321, 29.89648521331577058 ) ) ;
#23792 = B_SPLINE_CURVE_WITH_KNOTS ( 'NONE', 3,
 ( #59885, #55178, #33563, #43279, #4696, #33875 ),
 .UNSPECIFIED., .F., .F.,
 ( 4, 2, 4 ),
 ( 1.268633296668913999E-16, 0.0002450741128632358658, 0.0004901482257263448800 ),
 .UNSPECIFIED. ) ;
#23793 = CARTESIAN_POINT ( 'NONE',  ( 0.8744876279028263033, -48.79802643035343834, 5.394688766001209501 ) ) ;
#23794 = DIRECTION ( 'NONE',  ( -1.000000000000000000, -0.000000000000000000, -0.000000000000000000 ) ) ;
#23795 =( NAMED_UNIT ( * ) SI_UNIT ( $, .STERADIAN. ) SOLID_ANGLE_UNIT ( ) );
#23796 = CARTESIAN_POINT ( 'NONE',  ( 0.6031356755852232965, 8.546889573354048380E-06, 48.10744332413860747 ) ) ;
#23797 = EDGE_LOOP ( 'NONE', ( #39753, #8241, #22928, #21054 ) ) ;
#23798 = CARTESIAN_POINT ( 'NONE',  ( 2.299652685299199195, -31.56856304606662889, 37.51942899438463286 ) ) ;
#23799 = CARTESIAN_POINT ( 'NONE',  ( -6.063463321072276813, 9.995861580987984496, 16.45913739335079384 ) ) ;
#23800 = CARTESIAN_POINT ( 'NONE',  ( 4.303969348037246512, 47.36875205922773091, 8.413118729224215997 ) ) ;
#23801 = B_SPLINE_CURVE_WITH_KNOTS ( 'NONE', 3,
 ( #39149, #5576, #53205, #25326, #10310, #24713 ),
 .UNSPECIFIED., .F., .F.,
 ( 4, 2, 4 ),
 ( 1.492775917167880503E-16, 0.0002445252820015208161, 0.0004890505640028923375 ),
 .UNSPECIFIED. ) ;
#23802 = CONICAL_SURFACE ( 'NONE', #4752, 42.08604991992415023, 1.569615340895231137 ) ;
#23803 = DIRECTION ( 'NONE',  ( 0.07500201931887538753, 0.5251354798924551259, 0.8477071574878980442 ) ) ;
#23804 = CARTESIAN_POINT ( 'NONE',  ( 3.376099380956842921, 8.983142335927920996, -9.950454130567432998 ) ) ;
#23805 = VECTOR ( 'NONE', #13091, 1000.000000000000227 ) ;
#23806 = CARTESIAN_POINT ( 'NONE',  ( 3.270143674763207553, -10.69018354892881462, -8.548517033725367753 ) ) ;
#23807 = EDGE_CURVE ( 'NONE', #39562, #46978, #30992, .T. ) ;
#23808 = VECTOR ( 'NONE', #13175, 1000.000000000000114 ) ;
#23809 = CARTESIAN_POINT ( 'NONE',  ( -6.057079549204054558, -12.95277456599821164, -14.24980217905386404 ) ) ;
#23810 = VERTEX_POINT ( 'NONE', #43374 ) ;
#23811 = CARTESIAN_POINT ( 'NONE',  ( 0.1103310638050661874, 37.30561229499300424, 21.63353985999701479 ) ) ;
#23812 = CARTESIAN_POINT ( 'NONE',  ( 0.5807400328401574052, -41.20655774452952613, -24.41979442053212779 ) ) ;
#23813 = CARTESIAN_POINT ( 'NONE',  ( 0.7242486021783853811, -42.37565498843926548, -24.80555031993310777 ) ) ;
#23814 = CARTESIAN_POINT ( 'NONE',  ( 0.5797568665920719289, 42.92520464323349927, -18.88523536889057652 ) ) ;
#23815 = ORIENTED_EDGE ( 'NONE', *, *, #12396, .F. ) ;
#23816 = DIRECTION ( 'NONE',  ( -0.9848077530122079093, -0.1736481776669316079, 5.551115123125783935E-17 ) ) ;
#23817 = CARTESIAN_POINT ( 'NONE',  ( 2.618530812446111078, 36.00211569111120014, 30.22539420689239975 ) ) ;
#23818 = LINE ( 'NONE', #47940, #6490 ) ;
#23819 = EDGE_LOOP ( 'NONE', ( #19516, #43572, #26992, #33604 ) ) ;
#23820 = CARTESIAN_POINT ( 'NONE',  ( 0.1158816050234199035, 4.231281718317980278, -43.92081848423808310 ) ) ;
#23821 = CARTESIAN_POINT ( 'NONE',  ( 4.694002226626920127, 32.98704702821290624, 31.46648216443339408 ) ) ;
#23822 = CARTESIAN_POINT ( 'NONE',  ( -6.063463321072276813, -19.21612852159696061, 1.249342675544900638 ) ) ;
#23823 = ORIENTED_EDGE ( 'NONE', *, *, #4363, .T. ) ;
#23824 = AXIS2_PLACEMENT_3D ( 'NONE', #37484, #61857, #38114 ) ;
#23825 = CARTESIAN_POINT ( 'NONE',  ( 4.967162193818130511, -14.26841313271309808, 40.65506779172159924 ) ) ;
#23826 = CIRCLE ( 'NONE', #50821, 48.91267123290010943 ) ;
#23827 = ORIENTED_EDGE ( 'NONE', *, *, #32836, .T. ) ;
#23828 = DIRECTION ( 'NONE',  ( -1.000000000000000000, -1.836909530733573776E-16, 1.925929944387235853E-32 ) ) ;
#23829 = ORIENTED_EDGE ( 'NONE', *, *, #39633, .T. ) ;
#23830 = CARTESIAN_POINT ( 'NONE',  ( 1.231276596079881047, -6.136529359146127405, -41.46829847537036784 ) ) ;
#23831 = CARTESIAN_POINT ( 'NONE',  ( 3.678834586032787346, 47.68471048368242293, 11.17053068192113763 ) ) ;
#23832 = ORIENTED_EDGE ( 'NONE', *, *, #28630, .F. ) ;
#23833 = CARTESIAN_POINT ( 'NONE',  ( 0.8554163680231816613, 31.95314001164609152, -34.35407277904558043 ) ) ;
#23834 = VERTEX_POINT ( 'NONE', #53348 ) ;
#23835 = CARTESIAN_POINT ( 'NONE',  ( 0.2940133293163008643, -43.84964716027407405, 4.842416080585272731 ) ) ;
#23836 = CARTESIAN_POINT ( 'NONE',  ( 0.5824935313925959646, 40.53383721374637361, 23.58487264717254561 ) ) ;
#23837 = EDGE_CURVE ( 'NONE', #22451, #19448, #47795, .T. ) ;
#23838 = ORIENTED_EDGE ( 'NONE', *, *, #16154, .T. ) ;
#23839 = CARTESIAN_POINT ( 'NONE',  ( 0.1129192098497455998, 14.78321943369591196, 41.57412910645692961 ) ) ;
#23840 = CONICAL_SURFACE ( 'NONE', #2851, 42.92674063221959813, 1.485477209440487556 ) ;
#23841 = CARTESIAN_POINT ( 'NONE',  ( 0.9730545539215883499, 36.90443313492362165, -21.89037132892396897 ) ) ;
#23842 = CARTESIAN_POINT ( 'NONE',  ( -31.75000000000000000, 15.14599999999999369, 0.000000000000000000 ) ) ;
#23843 = ORIENTED_EDGE ( 'NONE', *, *, #8623, .F. ) ;
#23844 = EDGE_CURVE ( 'NONE', #19546, #351, #20058, .T. ) ;
#23845 = CARTESIAN_POINT ( 'NONE',  ( -6.016761891674564211, 9.424569481870250343, 16.31696541414275359 ) ) ;
#23846 = CARTESIAN_POINT ( 'NONE',  ( 0.1139756605157203895, -17.49650554526767365, 40.50712916758530469 ) ) ;
#23847 = VERTEX_POINT ( 'NONE', #38071 ) ;
#23848 = CARTESIAN_POINT ( 'NONE',  ( 5.974727161628367256, -16.27409205901383871, 12.50710176109980409 ) ) ;
#23849 = VERTEX_POINT ( 'NONE', #9520 ) ;
#23850 = DIRECTION ( 'NONE',  ( -1.000000000000000000, -1.836909530733573776E-16, 2.465190328815682145E-32 ) ) ;
#23851 = CARTESIAN_POINT ( 'NONE',  ( 0.5786265663353196143, -23.32245830378999329, -41.83999636203343186 ) ) ;
#23852 = EDGE_LOOP ( 'NONE', ( #59416, #39881, #37194, #9912 ) ) ;
#23853 = CARTESIAN_POINT ( 'NONE',  ( 3.407937589446178528, 0.4592810312471982126, 13.69123696618924590 ) ) ;
#23854 = LINE ( 'NONE', #38285, #50293 ) ;
#23855 = CARTESIAN_POINT ( 'NONE',  ( -90.00000000000000000, 0.000000000000000000, 0.000000000000000000 ) ) ;
#23856 = CARTESIAN_POINT ( 'NONE',  ( -6.063463321072278589, 15.44190279603010119, -11.50513322467096344 ) ) ;
#23857 = VECTOR ( 'NONE', #28796, 1000.000000000000114 ) ;
#23858 = EDGE_CURVE ( 'NONE', #58674, #12140, #14070, .T. ) ;
#23859 = EDGE_LOOP ( 'NONE', ( #25749, #26790 ) ) ;
#23860 = CARTESIAN_POINT ( 'NONE',  ( 0.3622758884714730732, -26.89560658783362612, -33.69533458712334806 ) ) ;
#23861 = CARTESIAN_POINT ( 'NONE',  ( 5.880360259849739535, -21.17507050419543191, 43.04573319267409204 ) ) ;
#23862 = ADVANCED_FACE ( 'NONE', ( #29552 ), #48662, .F. ) ;
#23863 = CARTESIAN_POINT ( 'NONE',  ( 4.303969348037246512, 25.89994482339426440, -40.54345935592751715 ) ) ;
#23864 = B_SPLINE_CURVE_WITH_KNOTS ( 'NONE', 3,
 ( #17792, #2433, #11557, #6812 ),
 .UNSPECIFIED., .F., .F.,
 ( 4, 4 ),
 ( 0.000000000000000000, 0.005013413432710140706 ),
 .UNSPECIFIED. ) ;
#23865 = CARTESIAN_POINT ( 'NONE',  ( 5.896782393890504181, 20.06749419425504399, -1.349727247095607430 ) ) ;
#23866 = CARTESIAN_POINT ( 'NONE',  ( 5.959547316686252039, -16.28190225198627061, 12.49803383497722642 ) ) ;
#23867 = CARTESIAN_POINT ( 'NONE',  ( 0.8560838555295223751, 23.34035564869547841, 40.68907263964295851 ) ) ;
#23868 = VECTOR ( 'NONE', #34455, 1000.000000000000000 ) ;
#23869 = CARTESIAN_POINT ( 'NONE',  ( -6.015611763856276717, -2.453375430803944823, -18.68284711750060723 ) ) ;
#23870 = AXIS2_PLACEMENT_3D ( 'NONE', #20155, #19541, #57709 ) ;
#23871 = CARTESIAN_POINT ( 'NONE',  ( 0.5817217712918331118, 40.57952311434399206, -23.50611107394829702 ) ) ;
#23872 = DIRECTION ( 'NONE',  ( 0.9848077530122080203, 0.1736481776669314692, -5.551115123125783935E-17 ) ) ;
#23873 = CARTESIAN_POINT ( 'NONE',  ( 0.9758171775293915662, 30.33669560438110935, -30.34506652060211351 ) ) ;
#23874 = CARTESIAN_POINT ( 'NONE',  ( 0.1152809850208375286, -43.73310776251593524, -5.861788798815898538 ) ) ;
#23875 = CARTESIAN_POINT ( 'NONE',  ( 0.9722240741986376555, -34.39263045016073761, 25.65687427836892454 ) ) ;
#23876 = CARTESIAN_POINT ( 'NONE',  ( 0.9730545539215883499, -41.57420493492377744, -10.61654491617608009 ) ) ;
#23877 = CARTESIAN_POINT ( 'NONE',  ( 3.376099380956842921, -12.80728341440181595, -3.960034744197991508 ) ) ;
#23878 =( BOUNDED_SURFACE ( )  B_SPLINE_SURFACE ( 3, 1, ( 
 ( #28484, #51361 ),
 ( #28183, #4347 ),
 ( #32282, #8446 ),
 ( #22879, #47611 ) ),
 .UNSPECIFIED., .F., .F., .F. ) 
 B_SPLINE_SURFACE_WITH_KNOTS ( ( 4, 4 ),
 ( 2, 2 ),
 ( 0.000000000000000000, 1.000000000000000000 ),
 ( 0.000000000000000000, 1.000000000000000000 ),
 .UNSPECIFIED. ) 
 GEOMETRIC_REPRESENTATION_ITEM ( )  RATIONAL_B_SPLINE_SURFACE ( (
 ( 1.000000000000000000, 1.000000000000000000),
 ( 0.9953485035131437453, 0.8621029689291523912),
 ( 0.9953485035131437453, 0.8621029689291523912),
 ( 1.000000000000000000, 1.000000000000000000) ) ) 
 REPRESENTATION_ITEM ( '' )  SURFACE ( )  );
#23879 = CARTESIAN_POINT ( 'NONE',  ( 0.8557997880470599172, -46.03118133706016835, -13.27832040216687304 ) ) ;
#23880 = EDGE_CURVE ( 'NONE', #44114, #15737, #53642, .T. ) ;
#23881 = DIRECTION ( 'NONE',  ( -0.1024043820194934368, -0.9844298967354715435, -0.1428674944016109227 ) ) ;
#23882 = CARTESIAN_POINT ( 'NONE',  ( -6.001507490154110336, -18.68062548815627721, 2.475062734132372100 ) ) ;
#23883 = ORIENTED_EDGE ( 'NONE', *, *, #57457, .F. ) ;
#23884 = VECTOR ( 'NONE', #47220, 999.9999999999997726 ) ;
#23885 = CARTESIAN_POINT ( 'NONE',  ( 1.500000000000001332, 0.000000000000000000, 0.000000000000000000 ) ) ;
#23886 = CARTESIAN_POINT ( 'NONE',  ( 0.7056759521544966329, -18.97452373679281479, -42.89191390086098465 ) ) ;
#23887 = CARTESIAN_POINT ( 'NONE',  ( 4.956445790443988031, 0.000000000000000000, 0.000000000000000000 ) ) ;
#23888 = EDGE_LOOP ( 'NONE', ( #30800, #45118 ) ) ;
#23889 = DIRECTION ( 'NONE',  ( 0.000000000000000000, 0.000000000000000000, 1.000000000000000000 ) ) ;
#23890 = LINE ( 'NONE', #52687, #38958 ) ;
#23891 = CARTESIAN_POINT ( 'NONE',  ( 0.7762783648524402835, 34.49689442177346876, 33.23866576554850383 ) ) ;
#23892 =( BOUNDED_SURFACE ( )  B_SPLINE_SURFACE ( 3, 1, ( 
 ( #10408, #39242 ),
 ( #5056, #48008 ),
 ( #5971, #38937 ),
 ( #29192, #39869 ) ),
 .UNSPECIFIED., .F., .F., .F. ) 
 B_SPLINE_SURFACE_WITH_KNOTS ( ( 4, 4 ),
 ( 2, 2 ),
 ( 0.000000000000000000, 1.000000000000000000 ),
 ( 0.000000000000000000, 1.000000000000000000 ),
 .UNSPECIFIED. ) 
 GEOMETRIC_REPRESENTATION_ITEM ( )  RATIONAL_B_SPLINE_SURFACE ( (
 ( 1.000000000000000000, 1.000000000000000000),
 ( 0.9953040768229013402, 0.8617119497784988535),
 ( 0.9953040768229013402, 0.8617119497784988535),
 ( 1.000000000000000000, 1.000000000000000000) ) ) 
 REPRESENTATION_ITEM ( '' )  SURFACE ( )  );
#23893 = ORIENTED_EDGE ( 'NONE', *, *, #1913, .T. ) ;
#23894 = ORIENTED_EDGE ( 'NONE', *, *, #26239, .T. ) ;
#23895 = CARTESIAN_POINT ( 'NONE',  ( 0.9730545539215883499, -11.59290486963477562, -41.31259007387244253 ) ) ;
#23896 = ORIENTED_EDGE ( 'NONE', *, *, #44390, .T. ) ;
#23897 = CARTESIAN_POINT ( 'NONE',  ( 4.694002226626921015, -21.39119943673082247, 40.25793534328533241 ) ) ;
#23898 = CARTESIAN_POINT ( 'NONE',  ( -6.016489644550736315, -9.417787539062361546, 16.32089497094057862 ) ) ;
#23899 = ORIENTED_EDGE ( 'NONE', *, *, #35886, .F. ) ;
#23900 = ORIENTED_EDGE ( 'NONE', *, *, #9533, .F. ) ;
#23901 = DIRECTION ( 'NONE',  ( 0.000000000000000000, 0.000000000000000000, 1.000000000000000000 ) ) ;
#23902 = VERTEX_POINT ( 'NONE', #36370 ) ;
#23903 = CARTESIAN_POINT ( 'NONE',  ( -6.078075953587585900, -12.94192373113803463, 14.25839347137474888 ) ) ;
#23904 = CARTESIAN_POINT ( 'NONE',  ( 0.9730545539215883499, -29.98130006528883129, 30.69604515769640329 ) ) ;
#23905 = CARTESIAN_POINT ( 'NONE',  ( 5.719999999999994422, 15.72000000000000064, 0.000000000000000000 ) ) ;
#23906 = ORIENTED_EDGE ( 'NONE', *, *, #8550, .F. ) ;
#23907 = DIRECTION ( 'NONE',  ( -0.1024043820194934507, -0.7971196296869339504, 0.5950744814819157735 ) ) ;
#23908 = CARTESIAN_POINT ( 'NONE',  ( 0.9730545539215883499, -33.73144377768539215, -26.52009130076805832 ) ) ;
#23909 = ORIENTED_EDGE ( 'NONE', *, *, #40293, .T. ) ;
#23910 = ADVANCED_FACE ( 'NONE', ( #16953 ), #36161, .F. ) ;
#23911 = VERTEX_POINT ( 'NONE', #31965 ) ;
#23912 = FACE_OUTER_BOUND ( 'NONE', #44375, .T. ) ;
#23913 = CIRCLE ( 'NONE', #58910, 6.887500000000022382 ) ;
#23914 = ORIENTED_EDGE ( 'NONE', *, *, #50625, .F. ) ;
#23915 = CARTESIAN_POINT ( 'NONE',  ( 3.050102900204245682, 34.64366268476908317, 27.11534408710312505 ) ) ;
#23916 = DIRECTION ( 'NONE',  ( 0.07500201931887538753, -0.1132404149163173945, 0.9907327114452572081 ) ) ;
#23917 = DIRECTION ( 'NONE',  ( 0.000000000000000000, 0.000000000000000000, 1.000000000000000000 ) ) ;
#23918 = CARTESIAN_POINT ( 'NONE',  ( 3.783278058412226752, -14.86148287637761634, 40.39104487792936737 ) ) ;
#23919 = EDGE_CURVE ( 'NONE', #20243, #1725, #12017, .T. ) ;
#23920 = ORIENTED_EDGE ( 'NONE', *, *, #7029, .F. ) ;
#23921 = DIRECTION ( 'NONE',  ( 0.07836865515943411409, -0.9893941468723573829, 0.1223011693452750320 ) ) ;
#23922 = DIRECTION ( 'NONE',  ( 1.000000000000000000, 0.000000000000000000, 0.000000000000000000 ) ) ;
#23923 = ADVANCED_FACE ( 'NONE', ( #59838 ), #48945, .F. ) ;
#23924 = CARTESIAN_POINT ( 'NONE',  ( 4.999999999999983125, 80.00000000000001421, -2.649999999999992806 ) ) ;
#23925 = AXIS2_PLACEMENT_3D ( 'NONE', #4874, #14937, #42517 ) ;
#23926 = ORIENTED_EDGE ( 'NONE', *, *, #21888, .F. ) ;
#23927 = CARTESIAN_POINT ( 'NONE',  ( 0.7948878604505656975, 41.61600051860138194, 26.05392769112145857 ) ) ;
#23928 = CARTESIAN_POINT ( 'NONE',  ( 0.5980271706414734822, -24.85837266090920394, 42.35694218771019592 ) ) ;
#23929 = CARTESIAN_POINT ( 'NONE',  ( 4.956653778116960396, -3.690426056930336429, 47.94889704119049867 ) ) ;
#23930 = VECTOR ( 'NONE', #43612, 1000.000000000000000 ) ;
#23931 = EDGE_LOOP ( 'NONE', ( #49947, #34729, #7480, #20377 ) ) ;
#23932 = VERTEX_POINT ( 'NONE', #58655 ) ;
#23933 = DIRECTION ( 'NONE',  ( 0.000000000000000000, 0.000000000000000000, -1.000000000000000000 ) ) ;
#23934 = CARTESIAN_POINT ( 'NONE',  ( -6.015611763856276717, 13.31979030221817695, -13.32857883366819429 ) ) ;
#23935 = CARTESIAN_POINT ( 'NONE',  ( 1.088908134280557327, -17.14055988408889064, -39.34174992079771016 ) ) ;
#23936 = ADVANCED_FACE ( 'NONE', ( #50140 ), #55329, .F. ) ;
#23937 = CARTESIAN_POINT ( 'NONE',  ( 4.975610109902397937, -48.77192499014914517, 3.707929326866768349 ) ) ;
#23938 = CARTESIAN_POINT ( 'NONE',  ( -6.017396004339686577, -11.47005965438149033, 14.95000090562877482 ) ) ;
#23939 = CARTESIAN_POINT ( 'NONE',  ( 0.9756950546413921677, -42.52863374229713855, 5.696573146291832757 ) ) ;
#23940 = CARTESIAN_POINT ( 'NONE',  ( 0.6029443449137436017, -42.80956090170459305, 24.05994666217235078 ) ) ;
#23941 = CARTESIAN_POINT ( 'NONE',  ( 0.6067375320500716374, 0.7090021732340618943, -47.89177856776003495 ) ) ;
#23942 = DIRECTION ( 'NONE',  ( -1.000000000000000000, -0.000000000000000000, -0.000000000000000000 ) ) ;
#23943 = CARTESIAN_POINT ( 'NONE',  ( 5.895596859100789899, 12.98270243688412329, 15.36156309259609642 ) ) ;
#23944 = CARTESIAN_POINT ( 'NONE',  ( -5.272380000000000067, 0.000000000000000000, 12.55882000000000076 ) ) ;
#23945 = B_SPLINE_CURVE_WITH_KNOTS ( 'NONE', 3,
 ( #44004, #30781, #20468, #35509 ),
 .UNSPECIFIED., .F., .F.,
 ( 4, 4 ),
 ( 1.084202172485504434E-19, 0.004444878191957687789 ),
 .UNSPECIFIED. ) ;
#23946 = CARTESIAN_POINT ( 'NONE',  ( -2.739355103387248747, -13.73625580088958920, 5.844898931850249113 ) ) ;
#23947 = ORIENTED_EDGE ( 'NONE', *, *, #26769, .T. ) ;
#23948 = CARTESIAN_POINT ( 'NONE',  ( 5.959547316686252039, -10.26589671991375674, 17.77392908783916070 ) ) ;
#23949 = CARTESIAN_POINT ( 'NONE',  ( 0.1084644655670284341, -34.45367667780550391, -25.93599432281485662 ) ) ;
#23950 = CARTESIAN_POINT ( 'NONE',  ( 0.7764139734771269286, -45.77880932777608791, -10.21474852544046463 ) ) ;
#23951 = CARTESIAN_POINT ( 'NONE',  ( 2.299746137290199499, -47.74024417197872339, -11.18706503449364575 ) ) ;
#23952 = DIRECTION ( 'NONE',  ( 1.000000000000000000, 0.000000000000000000, 0.000000000000000000 ) ) ;
#23953 = CARTESIAN_POINT ( 'NONE',  ( -6.016489644550736315, -17.41053539857194465, -7.206912786933474813 ) ) ;
#23954 = ITEM_DEFINED_TRANSFORMATION ( 'NONE', 'NONE', #26894,  #14677 ) ;
#23955 = CARTESIAN_POINT ( 'NONE',  ( 4.975801465491695552, -45.55012473237743365, -14.85979367497158599 ) ) ;
#23956 = VECTOR ( 'NONE', #31993, 1000.000000000000000 ) ;
#23957 = CARTESIAN_POINT ( 'NONE',  ( 0.6021448801613057400, 48.25111984599001858, -9.130748722577767040 ) ) ;
#23958 = CARTESIAN_POINT ( 'NONE',  ( 0.5797568665920713737, 10.25842449096921172, -45.76013587791182857 ) ) ;
#23959 = CARTESIAN_POINT ( 'NONE',  ( 5.981074661064941900, 0.008585178657332563981, 20.52466374824937034 ) ) ;
#23961 = ORIENTED_EDGE ( 'NONE', *, *, #35863, .F. ) ;
#23960 = CARTESIAN_POINT ( 'NONE',  ( 0.9972139404380295780, -36.82725283858625431, 22.02214929131128329 ) ) ;
#23962 = ORIENTED_EDGE ( 'NONE', *, *, #58050, .T. ) ;
#23963 = AXIS2_PLACEMENT_3D ( 'NONE', #42563, #22821, #18751 ) ;
#23964 = CARTESIAN_POINT ( 'NONE',  ( 0.1073791018717483448, -43.12183934961191056, 0.4849339620931858996 ) ) ;
#23965 = CARTESIAN_POINT ( 'NONE',  ( 0.1092355843206037486, 39.72582785521893101, 16.78033551728677963 ) ) ;
#23966 = CARTESIAN_POINT ( 'NONE',  ( 0.8760168074887090262, 37.61398439004534566, -29.98565522133306871 ) ) ;
#23967 = EDGE_CURVE ( 'NONE', #16223, #34962, #29035, .T. ) ;
#23968 = ORIENTED_EDGE ( 'NONE', *, *, #36222, .F. ) ;
#23969 = CARTESIAN_POINT ( 'NONE',  ( 4.549368137175248350, 32.41327393324141326, -28.14399996863463116 ) ) ;
#23970 = CARTESIAN_POINT ( 'NONE',  ( 0.5835226383429304997, -45.91973687464727050, 9.519466366825529491 ) ) ;
#23971 = CARTESIAN_POINT ( 'NONE',  ( 5.896782393890504181, -19.39652907507979052, 5.319844614046219000 ) ) ;
#23972 = EDGE_CURVE ( 'NONE', #48721, #7149, #39479, .T. ) ;
#23973 = VERTEX_POINT ( 'NONE', #61358 ) ;
#23974 = ORIENTED_EDGE ( 'NONE', *, *, #38427, .T. ) ;
#23975 = EDGE_CURVE ( 'NONE', #14042, #60263, #32272, .T. ) ;
#23976 = VECTOR ( 'NONE', #21936, 1000.000000000000114 ) ;
#23977 = CARTESIAN_POINT ( 'NONE',  ( -6.016489644550737204, 13.32104266208099475, 13.32727118274442546 ) ) ;
#23978 = CARTESIAN_POINT ( 'NONE',  ( 0.1073791018717483448, 10.69234304550053949, -41.77800844988504991 ) ) ;
#23979 = CYLINDRICAL_SURFACE ( 'NONE', #27979, 9.500000000000000000 ) ;
#23980 = EDGE_LOOP ( 'NONE', ( #20815, #43098, #19775, #21377 ) ) ;
#23981 = EDGE_CURVE ( 'NONE', #35321, #8818, #23054, .T. ) ;
#23982 = CARTESIAN_POINT ( 'NONE',  ( 0.7056555295713303755, -11.58338207350432825, 46.47980662829228748 ) ) ;
#23983 = CARTESIAN_POINT ( 'NONE',  ( 4.226256110419178924, 43.93923658072332472, 0.4132053852653991832 ) ) ;
#23984 = ORIENTED_EDGE ( 'NONE', *, *, #20400, .T. ) ;
#23985 = CARTESIAN_POINT ( 'NONE',  ( 0.9972139404380286898, -37.48536715150211052, -20.88226186415268870 ) ) ;
#23986 = EDGE_CURVE ( 'NONE', #7311, #37701, #13478, .T. ) ;
#23987 = CARTESIAN_POINT ( 'NONE',  ( 0.5797568599927143129, 5.319646101103417735, -46.59320416144418431 ) ) ;
#23988 = FACE_OUTER_BOUND ( 'NONE', #3604, .T. ) ;
#23989 = DIRECTION ( 'NONE',  ( 0.000000000000000000, 0.000000000000000000, 1.000000000000000000 ) ) ;
#23990 = VERTEX_POINT ( 'NONE', #57270 ) ;
#23991 = VERTEX_POINT ( 'NONE', #27562 ) ;
#23992 = CARTESIAN_POINT ( 'NONE',  ( -6.016104459813374383, -11.47525878590926673, 14.94608397322080506 ) ) ;
#23993 = CARTESIAN_POINT ( 'NONE',  ( 0.9722240750034587542, 10.54237121715143388, -41.59310803641446341 ) ) ;
#23994 = EDGE_CURVE ( 'NONE', #44906, #8488, #33205, .T. ) ;
#23995 = CARTESIAN_POINT ( 'NONE',  ( 5.958863334805807099, 2.677925489610637921, -20.35021240744032411 ) ) ;
#23996 =( BOUNDED_SURFACE ( )  B_SPLINE_SURFACE ( 3, 1, ( 
 ( #34517, #52984 ),
 ( #48600, #5656 ),
 ( #29182, #29490 ),
 ( #24800, #15103 ) ),
 .UNSPECIFIED., .F., .F., .F. ) 
 B_SPLINE_SURFACE_WITH_KNOTS ( ( 4, 4 ),
 ( 2, 2 ),
 ( 0.000000000000000000, 1.000000000000000000 ),
 ( 0.000000000000000000, 1.000000000000000000 ),
 .UNSPECIFIED. ) 
 GEOMETRIC_REPRESENTATION_ITEM ( )  RATIONAL_B_SPLINE_SURFACE ( (
 ( 1.000000000000000000, 1.000000000000000000),
 ( 0.9751682680413298332, 0.9999560080971552356),
 ( 0.9751682680413298332, 0.9999560080971552356),
 ( 1.000000000000000000, 1.000000000000000000) ) ) 
 REPRESENTATION_ITEM ( '' )  SURFACE ( )  );
#23997 = CARTESIAN_POINT ( 'NONE',  ( 0.8560838555295223751, 11.76118766017263972, 45.40977096290989579 ) ) ;
#23998 = EDGE_LOOP ( 'NONE', ( #10968, #34328, #7459, #2959 ) ) ;
#23999 = CARTESIAN_POINT ( 'NONE',  ( -6.016761891674565099, 18.20201388312102253, -4.873659902332176053 ) ) ;
#24000 = ORIENTED_EDGE ( 'NONE', *, *, #1934, .F. ) ;
#24001 = CARTESIAN_POINT ( 'NONE',  ( 2.643462169533600914, -22.81120928486466326, -42.27470921730932218 ) ) ;
#24002 = FACE_OUTER_BOUND ( 'NONE', #30498, .T. ) ;
#24003 = CIRCLE ( 'NONE', #58999, 10.00000000000000000 ) ;
#24004 = VERTEX_POINT ( 'NONE', #4337 ) ;
#24005 = CARTESIAN_POINT ( 'NONE',  ( 0.8751705887134553219, -33.37254303619578621, 34.63284514348527665 ) ) ;
#24006 = CARTESIAN_POINT ( 'NONE',  ( 5.901463166500146684, 0.6576072425842132141, -20.10187610784469570 ) ) ;
#24007 = CARTESIAN_POINT ( 'NONE',  ( 4.975610109902397937, 0.000000000000000000, 0.000000000000000000 ) ) ;
#24008 = EDGE_CURVE ( 'NONE', #27345, #18903, #9370, .T. ) ;
#24009 = ORIENTED_EDGE ( 'NONE', *, *, #17548, .T. ) ;
#24010 = CARTESIAN_POINT ( 'NONE',  ( 0.8557997880470697982, 29.88293891557470516, 37.44587306708108088 ) ) ;
#24011 = CARTESIAN_POINT ( 'NONE',  ( 0.9730545539215883499, 15.95224156741828914, 39.83279466599044838 ) ) ;
#24012 = CARTESIAN_POINT ( 'NONE',  ( 4.967162193818130511, -36.06913038482816347, 23.56777426397165698 ) ) ;
#24013 = B_SPLINE_CURVE_WITH_KNOTS ( 'NONE', 3,
 ( #24651, #48154, #48757, #19654, #5211, #19343 ),
 .UNSPECIFIED., .F., .F.,
 ( 4, 2, 4 ),
 ( 3.476216610979977084E-18, 0.0002291459268755711835, 0.0004582918537511388975 ),
 .UNSPECIFIED. ) ;
#24014 = CARTESIAN_POINT ( 'NONE',  ( -6.072942160501519915, 13.82262479916552778, -13.40668512162922532 ) ) ;
#24015 = CARTESIAN_POINT ( 'NONE',  ( 0.1087620492084205304, 16.83695155255833598, -39.70193592734187860 ) ) ;
#24016 = ORIENTED_EDGE ( 'NONE', *, *, #60873, .F. ) ;
#24017 = CARTESIAN_POINT ( 'NONE',  ( 0.6039202388192953519, -13.80541670804789511, 47.12721275830073608 ) ) ;
#24018 = CARTESIAN_POINT ( 'NONE',  ( 0.7413678028165011646, -16.99214960714165912, 40.69094424437406587 ) ) ;
#24019 = VECTOR ( 'NONE', #8914, 999.9999999999998863 ) ;
#24020 = ORIENTED_EDGE ( 'NONE', *, *, #53999, .T. ) ;
#24021 = LINE ( 'NONE', #57818, #7914 ) ;
#24022 = CARTESIAN_POINT ( 'NONE',  ( 0.5839879882104923592, 0.04539914087015842203, -47.89596766822081264 ) ) ;
#24023 = CARTESIAN_POINT ( 'NONE',  ( 0.3622758884714730732, 4.808133778521878732, -42.84426538328727219 ) ) ;
#24024 = CARTESIAN_POINT ( 'NONE',  ( 5.974727161628367256, 2.694421823322646237, 20.34732802718248479 ) ) ;
#24025 = CARTESIAN_POINT ( 'NONE',  ( 0.9754292589017201642, -6.395579240694774015, 41.41767778462806149 ) ) ;
#24026 = FACE_BOUND ( 'NONE', #1220, .T. ) ;
#24027 = CARTESIAN_POINT ( 'NONE',  ( 53.14999999999999147, 15.50000000000000711, 0.1731622330692809963 ) ) ;
#24028 = PRESENTATION_STYLE_ASSIGNMENT (( #509 ) ) ;
#24029 = CARTESIAN_POINT ( 'NONE',  ( 0.5824935313925952984, 11.22545165556063651, 45.53270705967863563 ) ) ;
#24030 = CARTESIAN_POINT ( 'NONE',  ( -6.010958268070873523, 18.19761767765837135, -4.891065400978194866 ) ) ;
#24031 = CARTESIAN_POINT ( 'NONE',  ( 0.3622758884714600280, -25.58609868863743841, -34.70015533914819628 ) ) ;
#24033 = EDGE_LOOP ( 'NONE', ( #17933, #27290, #6395, #3686 ) ) ;
#24032 = CARTESIAN_POINT ( 'NONE',  ( 4.694002226626921015, 42.38457918174925254, -16.78785927484989671 ) ) ;
#24034 = VERTEX_POINT ( 'NONE', #23791 ) ;
#24035 = B_SPLINE_CURVE_WITH_KNOTS ( 'NONE', 3,
 ( #11760, #6696, #11138, #40587, #54945, #12378, #59648, #12079, #21760, #31464, #26451, #31152, #50261, #6383, #2636, #40900 ),
 .UNSPECIFIED., .F., .F.,
 ( 4, 3, 3, 3, 3, 4 ),
 ( 1.868480190406682863E-17, 0.0002618515315864384531, 0.0003927756766341935460, 0.0005236998216950533363, 0.0007855159896329884893, 0.001047349442285926352 ),
 .UNSPECIFIED. ) ;
#24036 = CARTESIAN_POINT ( 'NONE',  ( 3.783198216974391404, -33.06596988314780106, -27.54889409286111857 ) ) ;
#24037 = CARTESIAN_POINT ( 'NONE',  ( -2.601141883200665639, 1.878577531912080545, -14.80764579283228777 ) ) ;
#24038 = EDGE_CURVE ( 'NONE', #45127, #34420, #55977, .T. ) ;
#24039 = CARTESIAN_POINT ( 'NONE',  ( 0.8753041380234524160, -6.957149426674410719, 48.60798699522440813 ) ) ;
#24040 = CARTESIAN_POINT ( 'NONE',  ( 0.9754642270333688803, 42.56393738774957569, -5.426415525315391619 ) ) ;
#24041 = CARTESIAN_POINT ( 'NONE',  ( 0.5800708057587381505, -11.78915002112689692, -46.42229836006548283 ) ) ;
#24042 = EDGE_CURVE ( 'NONE', #45559, #55532, #52978, .T. ) ;
#24043 = EDGE_LOOP ( 'NONE', ( #29008, #16987, #5066, #30194 ) ) ;
#24044 = CARTESIAN_POINT ( 'NONE',  ( 0.1310142868023693452, -4.996535778099055136, -42.83311553787491732 ) ) ;
#24045 = ADVANCED_FACE ( 'NONE', ( #46684 ), #41998, .T. ) ;
#24046 = EDGE_CURVE ( 'NONE', #15772, #38898, #58853, .T. ) ;
#24047 = B_SPLINE_CURVE_WITH_KNOTS ( 'NONE', 3,
 ( #46542, #23958, #28341, #18971, #52444, #47771 ),
 .UNSPECIFIED., .F., .F.,
 ( 4, 2, 4 ),
 ( 8.805430561888389713E-18, 0.0002448709889506572109, 0.0004897419779013056397 ),
 .UNSPECIFIED. ) ;
#24048 = FACE_OUTER_BOUND ( 'NONE', #55873, .T. ) ;
#24049 = EDGE_CURVE ( 'NONE', #33545, #60706, #5881, .T. ) ;
#24050 = CARTESIAN_POINT ( 'NONE',  ( 0.8560838555295223751, 42.82099363437819051, -19.15033519931896322 ) ) ;
#24051 = EDGE_LOOP ( 'NONE', ( #29854, #25925, #9170, #3002 ) ) ;
#24052 = B_SPLINE_CURVE_WITH_KNOTS ( 'NONE', 3,
 ( #139, #28667, #52776, #9880 ),
 .UNSPECIFIED., .F., .F.,
 ( 4, 4 ),
 ( 7.790820618110713323E-17, 0.005004741218457486526 ),
 .UNSPECIFIED. ) ;
#24053 = CARTESIAN_POINT ( 'NONE',  ( 0.5824935313925941882, 43.31572943909446138, 17.97180458977351236 ) ) ;
#24054 = FACE_OUTER_BOUND ( 'NONE', #41942, .T. ) ;
#24055 = ORIENTED_EDGE ( 'NONE', *, *, #33765, .F. ) ;
#24056 = ADVANCED_FACE ( 'NONE', ( #19714 ), #32033, .F. ) ;
#24057 = CARTESIAN_POINT ( 'NONE',  ( -5.283180000000052168, 0.000000000000000000, 0.000000000000000000 ) ) ;
#24058 = ORIENTED_EDGE ( 'NONE', *, *, #31213, .F. ) ;
#24059 = EDGE_CURVE ( 'NONE', #44566, #61266, #10280, .T. ) ;
#24060 = B_SPLINE_CURVE_WITH_KNOTS ( 'NONE', 3,
 ( #27251, #26016, #22555, #45151 ),
 .UNSPECIFIED., .F., .F.,
 ( 4, 4 ),
 ( 2.602085213965210642E-18, 0.004042984057420973693 ),
 .UNSPECIFIED. ) ;
#24061 = CARTESIAN_POINT ( 'NONE',  ( 53.06512528815419927, 15.48567863024351432, -0.6878158681035048128 ) ) ;
#24062 = VECTOR ( 'NONE', #60521, 1000.000000000000114 ) ;
#24063 = CARTESIAN_POINT ( 'NONE',  ( -6.015611763856276717, 7.205255340944849429, -17.41126425312530301 ) ) ;
#24064 = ORIENTED_EDGE ( 'NONE', *, *, #8546, .T. ) ;
#24065 = CARTESIAN_POINT ( 'NONE',  ( 0.6845945791218023269, -44.58955076018944652, -14.56634764511800562 ) ) ;
#24066 = CARTESIAN_POINT ( 'NONE',  ( 0.9789889208857693870, 40.44490217462196568, 10.97928896275300659 ) ) ;
#24067 = CARTESIAN_POINT ( 'NONE',  ( 0.3622758884714600280, -15.73321244754826509, -40.13994584881776007 ) ) ;
#24068 = ORIENTED_EDGE ( 'NONE', *, *, #36759, .T. ) ;
#24069 = CARTESIAN_POINT ( 'NONE',  ( 4.975801465491695552, 32.01766832630263337, 35.64402118370968964 ) ) ;
#24070 = ORIENTED_EDGE ( 'NONE', *, *, #42155, .T. ) ;
#24071 = CARTESIAN_POINT ( 'NONE',  ( 0.5997462898726536595, -14.47257175146309649, 46.92649887902422279 ) ) ;
#24072 =( BOUNDED_SURFACE ( )  B_SPLINE_SURFACE ( 3, 1, ( 
 ( #20333, #34743 ),
 ( #58206, #898 ),
 ( #34435, #20634 ),
 ( #48219, #24402 ) ),
 .UNSPECIFIED., .F., .F., .F. ) 
 B_SPLINE_SURFACE_WITH_KNOTS ( ( 4, 4 ),
 ( 2, 2 ),
 ( 0.000000000000000000, 1.000000000000000000 ),
 ( 0.000000000000000000, 1.000000000000000000 ),
 .UNSPECIFIED. ) 
 GEOMETRIC_REPRESENTATION_ITEM ( )  RATIONAL_B_SPLINE_SURFACE ( (
 ( 1.000000000000000000, 1.000000000000000000),
 ( 0.7223157951917480446, 0.9931996967497186413),
 ( 0.7223157951917480446, 0.9931996967497186413),
 ( 1.000000000000000000, 1.000000000000000000) ) ) 
 REPRESENTATION_ITEM ( '' )  SURFACE ( )  );
#24073 = ORIENTED_EDGE ( 'NONE', *, *, #12006, .T. ) ;
#24074 = VERTEX_POINT ( 'NONE', #1501 ) ;
#24075 = CARTESIAN_POINT ( 'NONE',  ( 5.901463166500146684, 8.452982876530629852, -18.25006714589610723 ) ) ;
#24076 = CARTESIAN_POINT ( 'NONE',  ( 0.6027935024548037868, -34.14031893787248606, 33.89348162668918008 ) ) ;
#24077 = DIRECTION ( 'NONE',  ( 0.000000000000000000, 0.000000000000000000, 1.000000000000000000 ) ) ;
#24078 = CARTESIAN_POINT ( 'NONE',  ( 0.1365634738349412458, -43.67502418020411881, -6.273346991983733467 ) ) ;
#24079 = VERTEX_POINT ( 'NONE', #15330 ) ;
#24080 = CARTESIAN_POINT ( 'NONE',  ( 5.880360259849752858, 21.17507050419453662, 43.04573319267453968 ) ) ;
#24081 = CARTESIAN_POINT ( 'NONE',  ( 2.618530812446111078, -31.41152511854616947, 34.97202995145038074 ) ) ;
#24082 = DIRECTION ( 'NONE',  ( 0.07906939808003034253, -0.09174470402933210256, -0.9926383730089382018 ) ) ;
#24084 = ORIENTED_EDGE ( 'NONE', *, *, #22258, .T. ) ;
#24083 = ADVANCED_FACE ( 'NONE', ( #4965 ), #15002, .T. ) ;
#24085 = ORIENTED_EDGE ( 'NONE', *, *, #50559, .T. ) ;
#24086 = CARTESIAN_POINT ( 'NONE',  ( 0.9730545539215883499, 16.88610103448612065, -39.44597740938043273 ) ) ;
#24088 = ADVANCED_FACE ( 'NONE', ( #5577 ), #24072, .F. ) ;
#24087 = CARTESIAN_POINT ( 'NONE',  ( 3.376099380956838925, 8.983142335927780664, 9.950454130567566224 ) ) ;
#24089 = DIRECTION ( 'NONE',  ( -0.1024043820194934368, -0.3684880688409071237, -0.9239750460186164638 ) ) ;
#24090 = CARTESIAN_POINT ( 'NONE',  ( 3.678834586032787346, 6.540082731167337293, -48.53699297955983383 ) ) ;
#24091 = CARTESIAN_POINT ( 'NONE',  ( 1.830465331921976579, -37.76032919508905650, -22.68333297725216013 ) ) ;
#24092 = VERTEX_POINT ( 'NONE', #25327 ) ;
#24093 = EDGE_LOOP ( 'NONE', ( #43724, #24770, #565, #57935 ) ) ;
#24094 = CARTESIAN_POINT ( 'NONE',  ( 0.2940133293163014194, -42.87040773915203573, 10.41002833122450433 ) ) ;
#24095 = CARTESIAN_POINT ( 'NONE',  ( -6.016489644550736315, -14.95199950534940037, -11.46752133529400375 ) ) ;
#24096 = LINE ( 'NONE', #43225, #25008 ) ;
#24097 = CARTESIAN_POINT ( 'NONE',  ( 0.6846871229502899947, 5.395516691087876460, -47.60345020167345353 ) ) ;
#24098 = CARTESIAN_POINT ( 'NONE',  ( 3.660176727303401378, 10.60619300811871746, 46.85282580473582215 ) ) ;
#24099 = CARTESIAN_POINT ( 'NONE',  ( 0.08486401232817714080, 5.403818426594913263E-15, -44.12552607296456131 ) ) ;
#24100 = AXIS2_PLACEMENT_3D ( 'NONE', #9683, #28795, #17948 ) ;
#24101 = VERTEX_POINT ( 'NONE', #5271 ) ;
#24102 = CARTESIAN_POINT ( 'NONE',  ( 3.678834586032787346, -31.95978921216147128, 37.11043307673141101 ) ) ;
#24103 = CARTESIAN_POINT ( 'NONE',  ( 0.8744876279028263033, 48.92939099258497038, 4.032957658374010101 ) ) ;
#24104 = CARTESIAN_POINT ( 'NONE',  ( -6.078726893082806448, 3.076629396955338436, -19.00863995194055178 ) ) ;
#24105 = LINE ( 'NONE', #23183, #3816 ) ;
#24106 = DIRECTION ( 'NONE',  ( -1.000000000000000000, -0.000000000000000000, -0.000000000000000000 ) ) ;
#24107 = LINE ( 'NONE', #909, #41158 ) ;
#24108 = FACE_OUTER_BOUND ( 'NONE', #26124, .T. ) ;
#24109 = ADVANCED_FACE ( 'NONE', ( #20036 ), #30449, .F. ) ;
#24110 = ORIENTED_EDGE ( 'NONE', *, *, #13225, .T. ) ;
#24111 = CARTESIAN_POINT ( 'NONE',  ( 0.8560838555295223751, 46.35895890951135812, -7.156798369939577853 ) ) ;
#24112 = EDGE_CURVE ( 'NONE', #48331, #51387, #9988, .T. ) ;
#24113 = CARTESIAN_POINT ( 'NONE',  ( 0.1104177457020373149, 37.34931850022140054, 21.55798761925400697 ) ) ;
#24114 = CARTESIAN_POINT ( 'NONE',  ( 1.834102595619085507, 40.23352532279152882, 17.92933866482468730 ) ) ;
#24115 = CARTESIAN_POINT ( 'NONE',  ( 4.553261556744875094, 17.98701270972463817, -40.07501640179128799 ) ) ;
#24116 = EDGE_CURVE ( 'NONE', #49729, #21388, #24096, .T. ) ;
#24117 = EDGE_LOOP ( 'NONE', ( #46423, #38946 ) ) ;
#24118 = CARTESIAN_POINT ( 'NONE',  ( -2.569797478183783568, 14.24379821351252495, 3.352038560005965451 ) ) ;
#24119 = PLANE ( 'NONE',  #40979 ) ;
#24120 = B_SPLINE_CURVE_WITH_KNOTS ( 'NONE', 3,
 ( #28410, #57204, #193, #48152, #47850, #4275 ),
 .UNSPECIFIED., .F., .F.,
 ( 4, 2, 4 ),
 ( 3.252606517456513302E-18, 0.0002447193893791697623, 0.0004894387787583362719 ),
 .UNSPECIFIED. ) ;
#24121 = ORIENTED_EDGE ( 'NONE', *, *, #48130, .T. ) ;
#24122 = DIRECTION ( 'NONE',  ( -1.000000000000000000, -0.000000000000000000, -0.000000000000000000 ) ) ;
#24123 = CARTESIAN_POINT ( 'NONE',  ( 0.9754292580325133466, 25.32584952646948651, -33.39054975088954080 ) ) ;
#24124 = VERTEX_POINT ( 'NONE', #53206 ) ;
#24125 = CARTESIAN_POINT ( 'NONE',  ( 0.9722240750034566448, -6.177112354444842524, -42.46141201102052776 ) ) ;
#24126 = EDGE_LOOP ( 'NONE', ( #41624, #25741, #15284, #16749 ) ) ;
#24127 = CARTESIAN_POINT ( 'NONE',  ( -6.001507490154111224, 17.41542759839274268, -7.196845540358981275 ) ) ;
#24128 = ORIENTED_EDGE ( 'NONE', *, *, #36222, .T. ) ;
#24129 = CARTESIAN_POINT ( 'NONE',  ( -6.057079549204054558, -8.899553672604941568, 17.07715361318045666 ) ) ;
#24130 = DIRECTION ( 'NONE',  ( -1.000000000000000000, 0.000000000000000000, 0.000000000000000000 ) ) ;
#24131 = ORIENTED_EDGE ( 'NONE', *, *, #49956, .T. ) ;
#24132 = CARTESIAN_POINT ( 'NONE',  ( 4.975801465491694664, -45.55012473237763260, 14.85979367497093762 ) ) ;
#24133 = VERTEX_POINT ( 'NONE', #19408 ) ;
#24134 = CARTESIAN_POINT ( 'NONE',  ( 0.3676999524040323597, -43.84864779214683495, 4.821480075982420566 ) ) ;
#24135 = CIRCLE ( 'NONE', #40184, 13.00000000000000178 ) ;
#24136 = CARTESIAN_POINT ( 'NONE',  ( 0.5817217712918331118, 40.11546086164733538, 24.28960176425324846 ) ) ;
#24137 =( BOUNDED_SURFACE ( )  B_SPLINE_SURFACE ( 3, 1, ( 
 ( #8029, #27141 ),
 ( #46268, #22442 ),
 ( #41567, #17746 ),
 ( #36873, #8635 ) ),
 .UNSPECIFIED., .F., .F., .F. ) 
 B_SPLINE_SURFACE_WITH_KNOTS ( ( 4, 4 ),
 ( 2, 2 ),
 ( 0.000000000000000000, 1.000000000000000000 ),
 ( 0.000000000000000000, 1.000000000000000000 ),
 .UNSPECIFIED. ) 
 GEOMETRIC_REPRESENTATION_ITEM ( )  RATIONAL_B_SPLINE_SURFACE ( (
 ( 1.000000000000000000, 1.000000000000000000),
 ( 0.9953390228620291325, 0.8624445117761032620),
 ( 0.9953390228620291325, 0.8624445117761032620),
 ( 1.000000000000000000, 1.000000000000000000) ) ) 
 REPRESENTATION_ITEM ( '' )  SURFACE ( )  );
#24138 = ORIENTED_EDGE ( 'NONE', *, *, #29594, .T. ) ;
#24139 = CARTESIAN_POINT ( 'NONE',  ( 1.399999999999998579, 0.000000000000000000, -5.000000000000000888 ) ) ;
#24140 = B_SPLINE_CURVE_WITH_KNOTS ( 'NONE', 3,
 ( #46189, #12675, #31774, #7953, #47111, #40886, #8558, #41492, #12991, #59952, #17060, #37407, #3853 ),
 .UNSPECIFIED., .F., .F.,
 ( 4, 3, 3, 3, 4 ),
 ( 0.0004849530346207898404, 0.0005237000248299429964, 0.0006546240681324979336, 0.0007855481115631321671, 0.0009699050456655107250 ),
 .UNSPECIFIED. ) ;
#24141 = CARTESIAN_POINT ( 'NONE',  ( 1.227938101723756947, 36.73927144310543014, -22.18841447410681411 ) ) ;
#24142 = ORIENTED_EDGE ( 'NONE', *, *, #38097, .T. ) ;
#24143 = CARTESIAN_POINT ( 'NONE',  ( 0.5839879327111928697, -33.93179405280464778, -33.80333292213293106 ) ) ;
#24144 = CARTESIAN_POINT ( 'NONE',  ( 0.1158403557922069033, -17.89533752146796530, 40.33233444987482841 ) ) ;
#24145 = ORIENTED_EDGE ( 'NONE', *, *, #33567, .T. ) ;
#24146 = CARTESIAN_POINT ( 'NONE',  ( 0.5806925824938511393, 42.95845041307772050, -18.80940989108128747 ) ) ;
#24147 = ORIENTED_EDGE ( 'NONE', *, *, #12575, .T. ) ;
#24148 = DIRECTION ( 'NONE',  ( 0.07500201931887538753, 0.4074616462826469721, 0.9101371896075481915 ) ) ;
#24150 = EDGE_CURVE ( 'NONE', #58621, #4984, #2987, .T. ) ;
#24149 = B_SPLINE_CURVE_WITH_KNOTS ( 'NONE', 3,
 ( #54572, #60211, #40530, #6639, #54262, #59287 ),
 .UNSPECIFIED., .F., .F.,
 ( 4, 2, 4 ),
 ( 1.137877798855602457E-16, 0.0002448718616795915784, 0.0004897437233590694241 ),
 .UNSPECIFIED. ) ;
#24151 = CARTESIAN_POINT ( 'NONE',  ( 0.1152809850208375703, 25.06245401136728290, 36.31554324828218938 ) ) ;
#24152 = EDGE_LOOP ( 'NONE', ( #2608, #5005, #1230, #46366 ) ) ;
#24153 = CARTESIAN_POINT ( 'NONE',  ( 0.3622758884714730732, -37.74294673546571488, -20.83792692158958815 ) ) ;
#24154 = CARTESIAN_POINT ( 'NONE',  ( 0.1155031312995260795, 25.38218459480881961, -36.09274633117931330 ) ) ;
#24155 = CARTESIAN_POINT ( 'NONE',  ( 3.661933894777871679, -42.79842724482195138, 19.51732026486564564 ) ) ;
#24156 = CARTESIAN_POINT ( 'NONE',  ( 0.5998501479064708430, 12.95623334615502387, -46.33007877220726556 ) ) ;
#24157 =( BOUNDED_SURFACE ( )  B_SPLINE_SURFACE ( 3, 1, ( 
 ( #29573, #48683 ),
 ( #59302, #35219 ),
 ( #40862, #50528 ),
 ( #12651, #3213 ) ),
 .UNSPECIFIED., .F., .F., .F. ) 
 B_SPLINE_SURFACE_WITH_KNOTS ( ( 4, 4 ),
 ( 2, 2 ),
 ( 0.000000000000000000, 1.000000000000000000 ),
 ( 0.000000000000000000, 1.000000000000000000 ),
 .UNSPECIFIED. ) 
 GEOMETRIC_REPRESENTATION_ITEM ( )  RATIONAL_B_SPLINE_SURFACE ( (
 ( 1.000000000000000000, 1.000000000000000000),
 ( 0.7269869731126817891, 0.9931720237060910339),
 ( 0.7269869731126817891, 0.9931720237060910339),
 ( 1.000000000000000000, 1.000000000000000000) ) ) 
 REPRESENTATION_ITEM ( '' )  SURFACE ( )  );
#24158 = ORIENTED_EDGE ( 'NONE', *, *, #14675, .F. ) ;
#24159 = CARTESIAN_POINT ( 'NONE',  ( -6.016489644550736315, -18.68257207665194741, -2.455165042129931141 ) ) ;
#24160 =( BOUNDED_SURFACE ( )  B_SPLINE_SURFACE ( 3, 1, ( 
 ( #33194, #47282 ),
 ( #4329, #23464 ),
 ( #18786, #37912 ),
 ( #9363, #28465 ) ),
 .UNSPECIFIED., .F., .F., .F. ) 
 B_SPLINE_SURFACE_WITH_KNOTS ( ( 4, 4 ),
 ( 2, 2 ),
 ( 0.000000000000000000, 1.000000000000000000 ),
 ( 0.000000000000000000, 1.000000000000000000 ),
 .UNSPECIFIED. ) 
 GEOMETRIC_REPRESENTATION_ITEM ( )  RATIONAL_B_SPLINE_SURFACE ( (
 ( 1.000000000000000000, 1.000000000000000000),
 ( 0.7269869731126821222, 0.9931720237060910339),
 ( 0.7269869731126821222, 0.9931720237060910339),
 ( 1.000000000000000000, 1.000000000000000000) ) ) 
 REPRESENTATION_ITEM ( '' )  SURFACE ( )  );
#24161 = CARTESIAN_POINT ( 'NONE',  ( 4.975610109902397937, 0.9924324126411095959, -48.90260202733707473 ) ) ;
#24162 = B_SPLINE_CURVE_WITH_KNOTS ( 'NONE', 3,
 ( #31809, #13024, #41222, #42159 ),
 .UNSPECIFIED., .F., .F.,
 ( 4, 4 ),
 ( 0.000000000000000000, 0.005014147105413705591 ),
 .UNSPECIFIED. ) ;
#24163 = CARTESIAN_POINT ( 'NONE',  ( 0.5786265663353153954, 41.83999636203319028, 23.32245830379044094 ) ) ;
#24164 = CARTESIAN_POINT ( 'NONE',  ( -6.015611763856276717, -16.32183393015603556, 9.416239407363246272 ) ) ;
#24165 = B_SPLINE_CURVE_WITH_KNOTS ( 'NONE', 3,
 ( #15142, #61791, #24524, #10438, #34249, #53325 ),
 .UNSPECIFIED., .F., .F.,
 ( 4, 2, 4 ),
 ( 1.196073045797343302E-16, 0.0002448718616795927711, 0.0004897437233590659546 ),
 .UNSPECIFIED. ) ;
#24166 = LINE ( 'NONE', #34826, #49628 ) ;
#24167 = CARTESIAN_POINT ( 'NONE',  ( 3.270143674763207553, 9.870732238228656641, -9.482922169187856909 ) ) ;
#24168 = CARTESIAN_POINT ( 'NONE',  ( 0.7056313189692711152, 46.58785579558880841, 5.414825604484328814 ) ) ;
#24169 = CARTESIAN_POINT ( 'NONE',  ( 4.549368137175248350, 0.000000000000000000, 0.000000000000000000 ) ) ;
#24170 = CARTESIAN_POINT ( 'NONE',  ( 0.9740398440564311811, 30.04629765303432620, -30.63262235044597759 ) ) ;
#24171 = CARTESIAN_POINT ( 'NONE',  ( -1.129531546211690163, 0.000000000000000000, 0.000000000000000000 ) ) ;
#24172 = CARTESIAN_POINT ( 'NONE',  ( 5.901463166500146684, -13.97174733644476419, 14.46748584610281263 ) ) ;
#24173 = CONICAL_SURFACE ( 'NONE', #23200, 42.08604991992415023, 1.569615340895231137 ) ;
#24174 = CARTESIAN_POINT ( 'NONE',  ( 0.5806925824938499181, -2.112975627976999782, 46.84824112321762613 ) ) ;
#24175 = CARTESIAN_POINT ( 'NONE',  ( 0.5832367798473389042, -23.71165515427687609, -41.61463593465329325 ) ) ;
#24176 = EDGE_CURVE ( 'NONE', #18514, #2406, #57397, .T. ) ;
#24177 = CARTESIAN_POINT ( 'NONE',  ( 0.5987334308729317378, -45.74238939486933475, -17.86607732597938991 ) ) ;
#24178 = EDGE_CURVE ( 'NONE', #41399, #46288, #32041, .T. ) ;
#24179 = CARTESIAN_POINT ( 'NONE',  ( 0.6064782688330856431, -13.21402945353875857, -44.99693180673298087 ) ) ;
#24180 = DIRECTION ( 'NONE',  ( -1.000000000000000000, -0.000000000000000000, -0.000000000000000000 ) ) ;
#24181 = ORIENTED_EDGE ( 'NONE', *, *, #27341, .T. ) ;
#24182 = CARTESIAN_POINT ( 'NONE',  ( -2.739355103387247858, -9.511660422587072006, 11.50547187021930640 ) ) ;
#24183 = CARTESIAN_POINT ( 'NONE',  ( 4.226256110419179812, 18.16371129757565939, -40.01133391784768634 ) ) ;
#24184 = CARTESIAN_POINT ( 'NONE',  ( 0.6041374136657475802, 24.20487816031520723, -41.57494627055121583 ) ) ;
#24185 = EDGE_CURVE ( 'NONE', #55289, #30839, #47670, .T. ) ;
#24186 = ORIENTED_EDGE ( 'NONE', *, *, #29414, .F. ) ;
#24187 = CARTESIAN_POINT ( 'NONE',  ( 0.9745511491811765792, 5.262846425219600555, 42.58443036172445773 ) ) ;
#24189 = DIRECTION ( 'NONE',  ( -0.000000000000000000, 1.000000000000000000, 1.224646799147353207E-16 ) ) ;
#24188 = B_SPLINE_CURVE_WITH_KNOTS ( 'NONE', 3,
 ( #53236, #6218, #57299, #931 ),
 .UNSPECIFIED., .F., .F.,
 ( 4, 4 ),
 ( 2.168573744943531741E-17, 0.004559932413162186803 ),
 .UNSPECIFIED. ) ;
#24190 = UNCERTAINTY_MEASURE_WITH_UNIT (LENGTH_MEASURE( 1.000000000000000082E-05 ), #51284, 'distance_accuracy_value', 'NONE');
#24191 = B_SPLINE_CURVE_WITH_KNOTS ( 'NONE', 3,
 ( #39566, #44576, #58945, #53313 ),
 .UNSPECIFIED., .F., .F.,
 ( 4, 4 ),
 ( 2.602085213965210642E-18, 0.004050076154992997279 ),
 .UNSPECIFIED. ) ;
#24192 = VERTEX_POINT ( 'NONE', #40694 ) ;
#24193 = EDGE_LOOP ( 'NONE', ( #46728, #27314, #5451, #9053 ) ) ;
#24194 = CARTESIAN_POINT ( 'NONE',  ( 0.7242486021783879346, -31.25073749153447977, 37.87351143753605953 ) ) ;
#24195 = VERTEX_POINT ( 'NONE', #49438 ) ;
#24196 = ADVANCED_FACE ( 'NONE', ( #7120 ), #36528, .F. ) ;
#24197 = CARTESIAN_POINT ( 'NONE',  ( 3.678748215320120529, 47.68472573843015994, -11.17048546618184446 ) ) ;
#24198 = ORIENTED_EDGE ( 'NONE', *, *, #40897, .T. ) ;
#24199 = VERTEX_POINT ( 'NONE', #12179 ) ;
#24200 = CARTESIAN_POINT ( 'NONE',  ( 0.000000000000000000, 0.000000000000000000, -0.2800830152838832965 ) ) ;
#24202 = ORIENTED_EDGE ( 'NONE', *, *, #4088, .T. ) ;
#24201 = EDGE_CURVE ( 'NONE', #14207, #44808, #55358, .T. ) ;
#24203 = CARTESIAN_POINT ( 'NONE',  ( 1.088313998177382391, 11.85828975620065684, -41.24258460930624892 ) ) ;
#24204 = CARTESIAN_POINT ( 'NONE',  ( -6.057079549204054558, -8.914624657271952302, -17.06929109013310608 ) ) ;
#24205 = CARTESIAN_POINT ( 'NONE',  ( 0.000000000000000000, 0.000000000000000000, -5.600000000000000533 ) ) ;
#24206 = ORIENTED_EDGE ( 'NONE', *, *, #50072, .T. ) ;
#24207 = CARTESIAN_POINT ( 'NONE',  ( 4.956653778116971054, 47.05699031914949160, 9.917440902361329691 ) ) ;
#24208 = CARTESIAN_POINT ( 'NONE',  ( 4.975801465491694664, 47.10002938642141856, -8.787181743659651545 ) ) ;
#24209 = ORIENTED_EDGE ( 'NONE', *, *, #41898, .F. ) ;
#24210 = EDGE_LOOP ( 'NONE', ( #19065, #44534, #32440 ) ) ;
#24211 = CARTESIAN_POINT ( 'NONE',  ( -6.079354080745853928, -16.13757513887036410, -10.50579001719886030 ) ) ;
#24212 = VERTEX_POINT ( 'NONE', #60361 ) ;
#24213 = CARTESIAN_POINT ( 'NONE',  ( 4.060580049360325461, 34.91776364945923206, 26.68740294745280295 ) ) ;
#24214 = CARTESIAN_POINT ( 'NONE',  ( 0.8753041380234465318, 36.80657072176691003, 32.50253343320412114 ) ) ;
#24215 = CARTESIAN_POINT ( 'NONE',  ( 4.960156602257182357, 15.40604254112701810, -43.79161740034457750 ) ) ;
#24216 = CARTESIAN_POINT ( 'NONE',  ( -1.200000000000006617, 0.000000000000000000, 0.000000000000000000 ) ) ;
#24217 = ORIENTED_EDGE ( 'NONE', *, *, #44542, .T. ) ;
#24218 = CARTESIAN_POINT ( 'NONE',  ( 0.6028618097248863439, -12.28244208173093099, 46.51318640245693103 ) ) ;
#24219 = VECTOR ( 'NONE', #43002, 1000.000000000000114 ) ;
#24220 = FACE_OUTER_BOUND ( 'NONE', #40453, .T. ) ;
#24221 = AXIS2_PLACEMENT_3D ( 'NONE', #59702, #35931, #30582 ) ;
#24222 = CARTESIAN_POINT ( 'NONE',  ( 0.5824935313925962976, 36.57712202577805272, -29.34880442820758972 ) ) ;
#24223 = EDGE_CURVE ( 'NONE', #60467, #18665, #45086, .T. ) ;
#24224 = CARTESIAN_POINT ( 'NONE',  ( 0.6041374136657476912, 6.106202762793474292, -47.71861871402583688 ) ) ;
#24225 = ORIENTED_EDGE ( 'NONE', *, *, #51244, .F. ) ;
#24226 = CARTESIAN_POINT ( 'NONE',  ( 1.000433927950263646, -34.92054925016447697, -23.17269767894281074 ) ) ;
#24227 = CARTESIAN_POINT ( 'NONE',  ( 0.6028777368367059797, -13.88892840780163063, -47.10241498048729625 ) ) ;
#24228 = CARTESIAN_POINT ( 'NONE',  ( 3.782542959838394392, 41.85823152591767382, -3.889255316797903372 ) ) ;
#24229 = CARTESIAN_POINT ( 'NONE',  ( 1.157643937452368155, 41.90847803242347425, -0.8256776614597129971 ) ) ;
#24230 = ORIENTED_EDGE ( 'NONE', *, *, #39177, .T. ) ;
#24231 = ORIENTED_EDGE ( 'NONE', *, *, #24589, .F. ) ;
#24232 = CARTESIAN_POINT ( 'NONE',  ( 1.231276596079887264, 33.41651732065550817, 25.31033664684050777 ) ) ;
#24233 = CARTESIAN_POINT ( 'NONE',  ( 0.6067375320500731917, -13.08014790719059128, 46.07640252006475379 ) ) ;
#24234 = FACE_OUTER_BOUND ( 'NONE', #35438, .T. ) ;
#24235 = CARTESIAN_POINT ( 'NONE',  ( 0.8560838555295223751, -41.44626783305086093, 21.96769712083507287 ) ) ;
#24236 = CARTESIAN_POINT ( 'NONE',  ( 0.7056313189692705601, -20.50398842223628648, -42.18216569521248971 ) ) ;
#24237 = B_SPLINE_CURVE_WITH_KNOTS ( 'NONE', 3,
 ( #47891, #15000, #24692, #43834, #57554, #876 ),
 .UNSPECIFIED., .F., .F.,
 ( 4, 2, 4 ),
 ( 1.010636948379330479E-17, 0.0002448709889506569398, 0.0004897419779013037966 ),
 .UNSPECIFIED. ) ;
#24238 =( BOUNDED_SURFACE ( )  B_SPLINE_SURFACE ( 3, 1, ( 
 ( #14564, #32742 ),
 ( #33059, #43073 ),
 ( #42459, #5117 ),
 ( #8595, #56826 ) ),
 .UNSPECIFIED., .F., .F., .F. ) 
 B_SPLINE_SURFACE_WITH_KNOTS ( ( 4, 4 ),
 ( 2, 2 ),
 ( 0.000000000000000000, 1.000000000000000000 ),
 ( 0.000000000000000000, 1.000000000000000000 ),
 .UNSPECIFIED. ) 
 GEOMETRIC_REPRESENTATION_ITEM ( )  RATIONAL_B_SPLINE_SURFACE ( (
 ( 1.000000000000000000, 1.000000000000000000),
 ( 0.9953040768229013402, 0.8617119497784988535),
 ( 0.9953040768229013402, 0.8617119497784988535),
 ( 1.000000000000000000, 1.000000000000000000) ) ) 
 REPRESENTATION_ITEM ( '' )  SURFACE ( )  );
#24239 = CARTESIAN_POINT ( 'NONE',  ( 4.549368137175248350, -32.41327393324121431, -28.14399996863486209 ) ) ;
#24240 = CARTESIAN_POINT ( 'NONE',  ( 5.896782393890504181, 12.99025607003297722, 15.35510775321956345 ) ) ;
#24241 = CARTESIAN_POINT ( 'NONE',  ( 0.5980271706414711508, 16.30306832862478217, 46.32773689609556556 ) ) ;
#24242 = CARTESIAN_POINT ( 'NONE',  ( 4.335381028904216727, -48.26758661664255357, 8.366416787923856901 ) ) ;
#24243 = CARTESIAN_POINT ( 'NONE',  ( 0.1073791018717483448, 30.14884492832389284, -30.83464511437107447 ) ) ;
#24244 = CARTESIAN_POINT ( 'NONE',  ( -6.015611763856276717, 17.41126425312538117, 7.205255340944677123 ) ) ;
#24245 = ORIENTED_EDGE ( 'NONE', *, *, #15753, .T. ) ;
#24246 = CARTESIAN_POINT ( 'NONE',  ( 4.975610109902397937, -47.89734868211972696, -9.914302615979444511 ) ) ;
#24247 = CARTESIAN_POINT ( 'NONE',  ( 0.1097557419366048670, -34.34829179474817806, -26.07515889977806367 ) ) ;
#24248 = CARTESIAN_POINT ( 'NONE',  ( 0.7044674535452954967, 23.45856740197708845, -43.14508475200626947 ) ) ;
#24249 = CARTESIAN_POINT ( 'NONE',  ( -6.016104459813371719, -14.94608397322092586, 11.47525878590911041 ) ) ;
#24250 = CARTESIAN_POINT ( 'NONE',  ( -5.995132425357893702, 7.219211173946727733, -17.40647075750109352 ) ) ;
#24251 = LINE ( 'NONE', #38688, #60610 ) ;
#24252 = DIRECTION ( 'NONE',  ( 0.1024043820194936449, 0.5950744814819241002, -0.7971196296869277331 ) ) ;
#24253 = ITEM_DEFINED_TRANSFORMATION ( 'NONE', 'NONE', #53874,  #14677 ) ;
#24254 = LINE ( 'NONE', #34911, #25862 ) ;
#24255 =( BOUNDED_SURFACE ( )  B_SPLINE_SURFACE ( 3, 1, ( 
 ( #9008, #57211 ),
 ( #47237, #33766 ),
 ( #4587, #3979 ),
 ( #23119, #4283 ) ),
 .UNSPECIFIED., .F., .F., .F. ) 
 B_SPLINE_SURFACE_WITH_KNOTS ( ( 4, 4 ),
 ( 2, 2 ),
 ( 0.000000000000000000, 1.000000000000000000 ),
 ( 0.000000000000000000, 1.000000000000000000 ),
 .UNSPECIFIED. ) 
 GEOMETRIC_REPRESENTATION_ITEM ( )  RATIONAL_B_SPLINE_SURFACE ( (
 ( 1.000000000000000000, 1.000000000000000000),
 ( 0.7269869731126821222, 0.9931720237060910339),
 ( 0.7269869731126821222, 0.9931720237060910339),
 ( 1.000000000000000000, 1.000000000000000000) ) ) 
 REPRESENTATION_ITEM ( '' )  SURFACE ( )  );
#24256 = CARTESIAN_POINT ( 'NONE',  ( 0.5998501479064708430, -5.759754759340450114, -47.76154736470756745 ) ) ;
#24257 = CARTESIAN_POINT ( 'NONE',  ( 0.8557997880470690211, 33.22501220301949587, -34.51495345639514767 ) ) ;
#24258 = EDGE_CURVE ( 'NONE', #48887, #26359, #9606, .T. ) ;
#24259 = DIRECTION ( 'NONE',  ( 1.000000000000000000, 0.000000000000000000, 0.000000000000000000 ) ) ;
#24260 = CARTESIAN_POINT ( 'NONE',  ( -6.078075953587585900, 3.068021059656765193, -19.01006104736748625 ) ) ;
#24262 = ORIENTED_EDGE ( 'NONE', *, *, #50786, .T. ) ;
#24261 = LINE ( 'NONE', #1355, #24332 ) ;
#24263 = VERTEX_POINT ( 'NONE', #54741 ) ;
#24264 = LINE ( 'NONE', #15804, #11910 ) ;
#24265 = CARTESIAN_POINT ( 'NONE',  ( 3.661921753702001237, -43.78265665639738558, 17.19622342091600231 ) ) ;
#24266 = CARTESIAN_POINT ( 'NONE',  ( -6.015611763856276717, -14.95313250337437871, 11.46610900684717471 ) ) ;
#24267 = ADVANCED_FACE ( 'NONE', ( #16875 ), #43302, .F. ) ;
#24268 = ORIENTED_EDGE ( 'NONE', *, *, #48237, .T. ) ;
#24269 = CARTESIAN_POINT ( 'NONE',  ( 0.1097557419366048670, -10.94578341459299509, 41.71221507312528587 ) ) ;
#24270 = CARTESIAN_POINT ( 'NONE',  ( 2.891212509700765487, 5.349982771599759140E-15, 41.99381090189422139 ) ) ;
#24271 = CARTESIAN_POINT ( 'NONE',  ( 0.3676999524040323597, -43.63756228305270213, -6.458617600968101335 ) ) ;
#24272 =( GEOMETRIC_REPRESENTATION_CONTEXT ( 3 ) GLOBAL_UNCERTAINTY_ASSIGNED_CONTEXT ( ( #59938 ) ) GLOBAL_UNIT_ASSIGNED_CONTEXT ( ( #42091, #51753, #38613 ) ) REPRESENTATION_CONTEXT ( 'NONE', 'WORKASPACE' ) );
#24273 = ADVANCED_BREP_SHAPE_REPRESENTATION ( '', ( #32179, #14677 ), #31864 ) ;
#24274 = ORIENTED_EDGE ( 'NONE', *, *, #26976, .F. ) ;
#24275 = EDGE_LOOP ( 'NONE', ( #21866, #22550, #31297, #19097 ) ) ;
#24276 = B_SPLINE_CURVE_WITH_KNOTS ( 'NONE', 3,
 ( #10960, #15349, #53224, #49154 ),
 .UNSPECIFIED., .F., .F.,
 ( 4, 4 ),
 ( 1.301042606982605321E-18, 0.004444878191957692126 ),
 .UNSPECIFIED. ) ;
#24277 = CARTESIAN_POINT ( 'NONE',  ( 0.9749527285493319040, -39.53206838353031571, -16.68386601451079443 ) ) ;
#24278 = CARTESIAN_POINT ( 'NONE',  ( 0.2885697896453107147, 17.24062360132716165, -39.51953439758091946 ) ) ;
#24279 = CARTESIAN_POINT ( 'NONE',  ( 3.678834586032788234, 24.27644425923901039, -42.53547488575171798 ) ) ;
#24280 = B_SPLINE_CURVE_WITH_KNOTS ( 'NONE', 3,
 ( #61668, #10313, #53207, #47917, #19715, #43536 ),
 .UNSPECIFIED., .F., .F.,
 ( 4, 2, 4 ),
 ( 2.224240575184740080E-17, 0.0002293755540694317251, 0.0004587511081388411698 ),
 .UNSPECIFIED. ) ;
#24281 = CARTESIAN_POINT ( 'NONE',  ( -6.057079549204054558, -16.13440658954566587, -10.51247616420431541 ) ) ;
#24282 = EDGE_CURVE ( 'NONE', #60198, #46592, #31247, .T. ) ;
#24283 = CARTESIAN_POINT ( 'NONE',  ( 0.8554163680231720024, -35.40260165760457767, -30.78735566729940132 ) ) ;
#24284 = B_SPLINE_CURVE_WITH_KNOTS ( 'NONE', 3,
 ( #19020, #29017, #10220, #52811 ),
 .UNSPECIFIED., .F., .F.,
 ( 4, 4 ),
 ( 0.000000000000000000, 0.005014147105413696917 ),
 .UNSPECIFIED. ) ;
#24285 = CARTESIAN_POINT ( 'NONE',  ( 0.6252788684277230669, 48.06490558434089877, -10.06027744856285722 ) ) ;
#24286 = VECTOR ( 'NONE', #3221, 1000.000000000000000 ) ;
#24287 = B_SPLINE_CURVE_WITH_KNOTS ( 'NONE', 3,
 ( #9541, #42777, #13647, #57437, #14270, #47463, #3590, #46864, #18651, #38090, #41858, #27735, #60926, #42472, #22726, #32439 ),
 .UNSPECIFIED., .F., .F.,
 ( 4, 3, 3, 3, 3, 4 ),
 ( 2.194378057379452319E-17, 0.0002618515315864434947, 0.0003927756766341995633, 0.0005236998216950572394, 0.0007855159896329905493, 0.001047349442285928087 ),
 .UNSPECIFIED. ) ;
#24288 = VERTEX_POINT ( 'NONE', #28405 ) ;
#24289 = VERTEX_POINT ( 'NONE', #42845 ) ;
#24290 = CARTESIAN_POINT ( 'NONE',  ( 0.3622758884714600280, 10.35929834645864389, 41.85013935980105515 ) ) ;
#24291 = CARTESIAN_POINT ( 'NONE',  ( 1.296416391601052487, 44.03828134713403841, 1.713811561060474942 ) ) ;
#24292 = VERTEX_POINT ( 'NONE', #27798 ) ;
#24293 = CARTESIAN_POINT ( 'NONE',  ( 0.1157506346131639274, 41.84695283361572393, -13.99189759625102703 ) ) ;
#24294 = CARTESIAN_POINT ( 'NONE',  ( 0.3622758884714730732, 37.74294673546557988, 20.83792692158985460 ) ) ;
#24295 = CARTESIAN_POINT ( 'NONE',  ( 0.6027935024548037868, 46.42277558035024754, 12.61964268015572976 ) ) ;
#24296 = CARTESIAN_POINT ( 'NONE',  ( 5.896782393890504181, 3.339090646272624419, 19.83372281075811827 ) ) ;
#24297 = ORIENTED_EDGE ( 'NONE', *, *, #20041, .F. ) ;
#24298 = VERTEX_POINT ( 'NONE', #23106 ) ;
#24299 = CARTESIAN_POINT ( 'NONE',  ( 0.1310142868023686513, 4.996535778098778025, 42.83311553787493864 ) ) ;
#24300 = CARTESIAN_POINT ( 'NONE',  ( 0.9747592971366240144, -42.58247319705098022, -5.279515277919826666 ) ) ;
#24301 = CARTESIAN_POINT ( 'NONE',  ( 0.5850706913938533704, -6.431767090163146960, 47.46255051844951822 ) ) ;
#24302 = CARTESIAN_POINT ( 'NONE',  ( 0.5804410086790514622, 28.25755288515122743, -37.43034272883802771 ) ) ;
#24303 = ORIENTED_EDGE ( 'NONE', *, *, #35163, .F. ) ;
#24304 = CARTESIAN_POINT ( 'NONE',  ( 4.963659409799329403, 33.96111158240244521, 29.14784479683121887 ) ) ;
#24305 = ORIENTED_EDGE ( 'NONE', *, *, #50141, .T. ) ;
#24306 = CARTESIAN_POINT ( 'NONE',  ( -6.016489644550737204, 16.31649074174277203, 9.425415887801145587 ) ) ;
#24307 = ORIENTED_EDGE ( 'NONE', *, *, #10559, .T. ) ;
#24308 = CARTESIAN_POINT ( 'NONE',  ( 0.6845945791218034371, 40.79463988471336933, -23.15607646797048247 ) ) ;
#24309 = EDGE_CURVE ( 'NONE', #56342, #32449, #52873, .T. ) ;
#24310 = DIRECTION ( 'NONE',  ( -0.07906939808003035641, -0.3030506235706508233, -0.9496885541274577847 ) ) ;
#24311 = DIRECTION ( 'NONE',  ( -1.000000000000000000, -0.000000000000000000, -0.000000000000000000 ) ) ;
#24312 = B_SPLINE_CURVE_WITH_KNOTS ( 'NONE', 3,
 ( #46680, #46079, #23172, #55738, #3728, #56355, #56050, #13473, #61059, #60429, #22557, #22862, #41994, #32268, #41680, #51659 ),
 .UNSPECIFIED., .F., .F.,
 ( 4, 3, 3, 3, 3, 4 ),
 ( 9.541595121948225732E-18, 0.0002724568934985560349, 0.0004086836638483799301, 0.0005449104342063581640, 0.0008173270854453656975, 0.001089761613562689226 ),
 .UNSPECIFIED. ) ;
#24313 = CIRCLE ( 'NONE', #9284, 2.500000000000000444 ) ;
#24315 = ORIENTED_EDGE ( 'NONE', *, *, #42871, .T. ) ;
#24314 = EDGE_CURVE ( 'NONE', #55332, #56636, #17058, .T. ) ;
#24316 = B_SPLINE_CURVE_WITH_KNOTS ( 'NONE', 3,
 ( #55410, #12536, #56033, #45437 ),
 .UNSPECIFIED., .F., .F.,
 ( 4, 4 ),
 ( 2.054184040232706591E-17, 0.004444306975806115896 ),
 .UNSPECIFIED. ) ;
#24317 = CARTESIAN_POINT ( 'NONE',  ( 2.099999999999999645, 0.000000000000000000, -5.294516984716111097 ) ) ;
#24318 = DIRECTION ( 'NONE',  ( 0.000000000000000000, 0.000000000000000000, 1.000000000000000000 ) ) ;
#24319 = CARTESIAN_POINT ( 'NONE',  ( 0.1310142868023677631, 10.54463319394675658, 41.81449350725031167 ) ) ;
#24320 = CARTESIAN_POINT ( 'NONE',  ( 4.549368137175248350, 19.17571786012324608, -38.40568845698256695 ) ) ;
#24321 = DIRECTION ( 'NONE',  ( -0.1024043820194934229, 0.9139094329506604053, 0.3927886084231669295 ) ) ;
#24322 = EDGE_LOOP ( 'NONE', ( #58411, #54210, #61151, #10896 ) ) ;
#24323 = ADVANCED_FACE ( 'NONE', ( #28105 ), #30095, .F. ) ;
#24324 = CARTESIAN_POINT ( 'NONE',  ( 0.5839254288179572816, -24.02657516616534750, 41.43367229384574557 ) ) ;
#24325 = CARTESIAN_POINT ( 'NONE',  ( 3.407937589446174087, -13.34359005742691373, 3.099921468254956736 ) ) ;
#24326 = CARTESIAN_POINT ( 'NONE',  ( 0.7056759521544998526, 3.855032142332291301, 46.74278079338640879 ) ) ;
#24327 = ORIENTED_EDGE ( 'NONE', *, *, #24538, .F. ) ;
#24328 = CARTESIAN_POINT ( 'NONE',  ( 0.9730545539215883499, -30.69604515769671949, 29.98130006528850444 ) ) ;
#24329 = CARTESIAN_POINT ( 'NONE',  ( 4.549368137175248350, 28.46244473166628097, 32.13400537129935230 ) ) ;
#24330 = CARTESIAN_POINT ( 'NONE',  ( 58.00000000000000000, -15.49999999999999112, -2.995852231480067093E-16 ) ) ;
#24331 = DIRECTION ( 'NONE',  ( 0.07836865515943411409, 0.6993330359244814831, 0.7104869166657112878 ) ) ;
#24332 = VECTOR ( 'NONE', #43398, 1000.000000000000000 ) ;
#24333 = CARTESIAN_POINT ( 'NONE',  ( 5.880360259849752858, -26.61251048557221210, -39.91356965504138543 ) ) ;
#24334 = CARTESIAN_POINT ( 'NONE',  ( 0.000000000000000000, 0.000000000000000000, -5.294516984716111097 ) ) ;
#24335 = CARTESIAN_POINT ( 'NONE',  ( -1.400000000000000799, 0.000000000000000000, 0.000000000000000000 ) ) ;
#24336 = DIRECTION ( 'NONE',  ( 9.298117831235686026E-16, -0.8294993580478402517, 0.5585076678061106081 ) ) ;
#24337 = CARTESIAN_POINT ( 'NONE',  ( 0.1368894036331283204, 39.47291701970388544, -19.71674790321427295 ) ) ;
#24338 = DIRECTION ( 'NONE',  ( -1.000000000000000000, -0.000000000000000000, -0.000000000000000000 ) ) ;
#24339 = EDGE_CURVE ( 'NONE', #26618, #51034, #43254, .T. ) ;
#24340 = CARTESIAN_POINT ( 'NONE',  ( 0.1073791018717578927, -26.63563652260192427, 33.91564619577761874 ) ) ;
#24342 = ORIENTED_EDGE ( 'NONE', *, *, #7261, .T. ) ;
#24341 = DIRECTION ( 'NONE',  ( 0.000000000000000000, 0.000000000000000000, 1.000000000000000000 ) ) ;
#24343 = ORIENTED_EDGE ( 'NONE', *, *, #57768, .F. ) ;
#24344 = CARTESIAN_POINT ( 'NONE',  ( 0.5834872094924177244, -12.61552836343323314, 46.20467604622297131 ) ) ;
#24345 = CARTESIAN_POINT ( 'NONE',  ( -2.569797478183783568, -13.34095667500609217, 6.011723966603914171 ) ) ;
#24346 = CARTESIAN_POINT ( 'NONE',  ( 48.86911069238522742, 15.35671945348452638, -2.116951128576620711 ) ) ;
#24347 = EDGE_CURVE ( 'NONE', #31565, #37013, #49999, .T. ) ;
#24348 = PRODUCT_DEFINITION_SHAPE ( 'NONE', 'NONE',  #61989 ) ;
#24349 = CARTESIAN_POINT ( 'NONE',  ( 1.227938101723756947, 30.94118573761312874, 29.74462687941236538 ) ) ;
#24350 = CARTESIAN_POINT ( 'NONE',  ( 0.8744876279028306332, -35.88078294188929362, -33.50999053799506555 ) ) ;
#24351 = CARTESIAN_POINT ( 'NONE',  ( 0.5848930533535030563, 27.67115520191777733, -37.86264983039271215 ) ) ;
#24352 = EDGE_CURVE ( 'NONE', #12149, #884, #44694, .T. ) ;
#24353 = EDGE_LOOP ( 'NONE', ( #52789, #16513, #9492, #3224 ) ) ;
#24354 = CARTESIAN_POINT ( 'NONE',  ( 4.956653778116994147, 35.79382859084161339, -32.11725092155005967 ) ) ;
#24355 = CARTESIAN_POINT ( 'NONE',  ( 0.8760168074887090262, -28.57146030082009602, 38.69913431881773391 ) ) ;
#24356 = CARTESIAN_POINT ( 'NONE',  ( -6.063463321072278589, 0.6016212027209763002, 19.24729862624639765 ) ) ;
#24357 = ORIENTED_EDGE ( 'NONE', *, *, #40061, .F. ) ;
#24358 = EDGE_CURVE ( 'NONE', #18458, #32580, #60990, .T. ) ;
#24359 = B_SPLINE_CURVE_WITH_KNOTS ( 'NONE', 3,
 ( #11177, #2052, #25882, #21184, #40626, #21807 ),
 .UNSPECIFIED., .F., .F.,
 ( 4, 2, 4 ),
 ( 8.434507579685065902E-18, 0.0002291978881530156180, 0.0004583957763060228334 ),
 .UNSPECIFIED. ) ;
#24360 = CONICAL_SURFACE ( 'NONE', #4339, 42.92674063221959813, 1.485477209440487556 ) ;
#24361 = CARTESIAN_POINT ( 'NONE',  ( 4.967162193818130511, 0.000000000000000000, 0.000000000000000000 ) ) ;
#24362 = CARTESIAN_POINT ( 'NONE',  ( 0.5832366564991511293, 47.44984844891997255, -6.521686574605630504 ) ) ;
#24363 = ORIENTED_EDGE ( 'NONE', *, *, #41715, .T. ) ;
#24364 =( BOUNDED_SURFACE ( )  B_SPLINE_SURFACE ( 3, 1, ( 
 ( #22959, #32668 ),
 ( #47082, #4120 ),
 ( #47685, #37687 ),
 ( #18885, #56752 ) ),
 .UNSPECIFIED., .F., .F., .F. ) 
 B_SPLINE_SURFACE_WITH_KNOTS ( ( 4, 4 ),
 ( 2, 2 ),
 ( 0.000000000000000000, 1.000000000000000000 ),
 ( 0.000000000000000000, 1.000000000000000000 ),
 .UNSPECIFIED. ) 
 GEOMETRIC_REPRESENTATION_ITEM ( )  RATIONAL_B_SPLINE_SURFACE ( (
 ( 1.000000000000000000, 1.000000000000000000),
 ( 0.9751682680413298332, 0.9999560080971552356),
 ( 0.9751682680413298332, 0.9999560080971552356),
 ( 1.000000000000000000, 1.000000000000000000) ) ) 
 REPRESENTATION_ITEM ( '' )  SURFACE ( )  );
#24365 = B_SPLINE_CURVE_WITH_KNOTS ( 'NONE', 3,
 ( #6566, #45766, #45162, #21630, #2812, #58902 ),
 .UNSPECIFIED., .F., .F.,
 ( 4, 2, 4 ),
 ( 1.870693080156664505E-17, 0.0002293755540694311559, 0.0004587511081388436092 ),
 .UNSPECIFIED. ) ;
#24366 = CARTESIAN_POINT ( 'NONE',  ( 4.553261556744873317, -4.442710778081946366, -43.70128015019640344 ) ) ;
#24367 = ORIENTED_EDGE ( 'NONE', *, *, #39849, .T. ) ;
#24368 = CARTESIAN_POINT ( 'NONE',  ( 0.6001305935487315502, 33.64689939321893775, 34.38748867424725830 ) ) ;
#24369 = CARTESIAN_POINT ( 'NONE',  ( 0.8557997880470599172, 0.9121262075952832893, -47.89938907511592703 ) ) ;
#24370 = ORIENTED_EDGE ( 'NONE', *, *, #38008, .F. ) ;
#24371 = FACE_OUTER_BOUND ( 'NONE', #61453, .T. ) ;
#24372 = CARTESIAN_POINT ( 'NONE',  ( 0.9762797500689124330, 40.55021165774351743, 10.58324712448433580 ) ) ;
#24373 = CARTESIAN_POINT ( 'NONE',  ( 0.7948878604505652534, 28.79738884442139124, 39.76693404125605724 ) ) ;
#24374 = AXIS2_PLACEMENT_3D ( 'NONE', #44136, #20003, #1164 ) ;
#24375 = VERTEX_POINT ( 'NONE', #48147 ) ;
#24376 = ORIENTED_EDGE ( 'NONE', *, *, #23432, .F. ) ;
#24377 = CARTESIAN_POINT ( 'NONE',  ( 1.157644175074336923, 40.63757550383299844, -10.27568648069094337 ) ) ;
#24378 = ORIENTED_EDGE ( 'NONE', *, *, #48316, .T. ) ;
#24379 = ORIENTED_EDGE ( 'NONE', *, *, #45775, .F. ) ;
#24380 = CARTESIAN_POINT ( 'NONE',  ( 0.2285344041767080614, 36.55576111592239386, -24.70177118206449762 ) ) ;
#24381 = CARTESIAN_POINT ( 'NONE',  ( 0.9762797500689124330, 35.79768877047989406, -21.79105926469756938 ) ) ;
#24382 = ADVANCED_FACE ( 'NONE', ( #5199 ), #15303, .F. ) ;
#24383 = CARTESIAN_POINT ( 'NONE',  ( 4.956445790443988031, 46.94638516972315756, 3.684422564749393558 ) ) ;
#24384 = ORIENTED_EDGE ( 'NONE', *, *, #38247, .T. ) ;
#24385 = CARTESIAN_POINT ( 'NONE',  ( 0.5804410086790514622, 11.40290849443472787, 45.49168638029309619 ) ) ;
#24386 = EDGE_CURVE ( 'NONE', #36850, #36264, #14643, .T. ) ;
#24387 = CARTESIAN_POINT ( 'NONE',  ( 4.549368137175248350, -13.99871866169335810, -40.58005590356685843 ) ) ;
#24388 = FACE_OUTER_BOUND ( 'NONE', #2862, .T. ) ;
#24389 = EDGE_LOOP ( 'NONE', ( #13136, #39410 ) ) ;
#24390 = ADVANCED_FACE ( 'NONE', ( #48750 ), #49012, .F. ) ;
#24391 = ORIENTED_EDGE ( 'NONE', *, *, #23771, .T. ) ;
#24392 = CARTESIAN_POINT ( 'NONE',  ( 0.1095718737110178143, -21.33933464366394261, -37.47471772507211796 ) ) ;
#24393 = CARTESIAN_POINT ( 'NONE',  ( -2.601141883200662974, -8.951945844433506494, 11.94395634066527734 ) ) ;
#24394 = CARTESIAN_POINT ( 'NONE',  ( 0.8554163680231816613, 16.00619315955244204, -44.10223637924629259 ) ) ;
#24395 = CARTESIAN_POINT ( 'NONE',  ( -2.569797478183790229, 3.352038560005718981, 14.24379821351258535 ) ) ;
#24396 = VERTEX_POINT ( 'NONE', #39079 ) ;
#24397 = EDGE_CURVE ( 'NONE', #47270, #27605, #44045, .T. ) ;
#24398 = EDGE_CURVE ( 'NONE', #988, #1157, #41701, .T. ) ;
#24399 = ORIENTED_EDGE ( 'NONE', *, *, #43944, .F. ) ;
#24400 = DIRECTION ( 'NONE',  ( 1.000000000000000000, 0.000000000000000000, 0.000000000000000000 ) ) ;
#24401 = CARTESIAN_POINT ( 'NONE',  ( 5.895881250540457863, 0.6766202122108295747, 20.10148916614708270 ) ) ;
#24402 = CARTESIAN_POINT ( 'NONE',  ( 5.880360259849739535, 43.04573319267415599, 21.17507050419530401 ) ) ;
#24403 = CARTESIAN_POINT ( 'NONE',  ( 0.9757787079277461251, -21.48842038179459735, 37.14005577278813064 ) ) ;
#24404 =( NAMED_UNIT ( * ) PLANE_ANGLE_UNIT ( ) SI_UNIT ( $, .RADIAN. ) );
#24405 = DIRECTION ( 'NONE',  ( -0.07906939808003035641, 0.9890184005629925057, 0.1248624588700777416 ) ) ;
#24406 = ORIENTED_EDGE ( 'NONE', *, *, #58180, .F. ) ;
#24407 = CARTESIAN_POINT ( 'NONE',  ( 0.2224561200757651791, 34.66601556960352326, -25.64288022150844526 ) ) ;
#24408 = CARTESIAN_POINT ( 'NONE',  ( 4.975610109902397937, -46.23629923292363486, -15.95788333023269878 ) ) ;
#24409 = ADVANCED_FACE ( 'NONE', ( #38766 ), #32493, .F. ) ;
#24410 = CARTESIAN_POINT ( 'NONE',  ( 0.6253024248130496510, -47.66998618349910544, 11.79053199319904977 ) ) ;
#24411 = CARTESIAN_POINT ( 'NONE',  ( 0.8751705887134423323, 23.27176129838367302, 42.09020928323383259 ) ) ;
#24412 = CARTESIAN_POINT ( 'NONE',  ( 0.8744876279028263033, -6.955970791787605911, -48.60004650947661275 ) ) ;
#24413 = FACE_OUTER_BOUND ( 'NONE', #6523, .T. ) ;
#24414 = CARTESIAN_POINT ( 'NONE',  ( 2.282816707992318950, 9.607080803701229854, -45.98044111183712346 ) ) ;
#24415 = EDGE_CURVE ( 'NONE', #53799, #36392, #13280, .T. ) ;
#24416 = ORIENTED_EDGE ( 'NONE', *, *, #24775, .T. ) ;
#24417 = CARTESIAN_POINT ( 'NONE',  ( 3.240649175237394708, 23.64729060054057896, 37.09542511754295191 ) ) ;
#24418 = DIRECTION ( 'NONE',  ( 0.000000000000000000, -0.7071067811865487940, 0.7071067811865461294 ) ) ;
#24419 = CARTESIAN_POINT ( 'NONE',  ( 0.7762777257811881437, 47.37038525518534726, 7.133808567472427420 ) ) ;
#24420 = CARTESIAN_POINT ( 'NONE',  ( 3.782625744892853525, -29.99484860343034498, 29.45415355009026115 ) ) ;
#24421 = CARTESIAN_POINT ( 'NONE',  ( 0.7954190325252775695, -23.29293489839764320, 42.08256085583533945 ) ) ;
#24422 = VERTEX_POINT ( 'NONE', #5505 ) ;
#24423 = CARTESIAN_POINT ( 'NONE',  ( 0.7948884756798489937, 32.36187196966092472, 36.92435357889731051 ) ) ;
#24424 = CARTESIAN_POINT ( 'NONE',  ( 5.200000000000002842, 3.061616997868383634E-16, -2.500000000000000444 ) ) ;
#24425 = ADVANCED_FACE ( 'NONE', ( #10863 ), #49673, .F. ) ;
#24426 = B_SPLINE_CURVE_WITH_KNOTS ( 'NONE', 3,
 ( #46759, #22945, #37057, #28542, #42992, #23543 ),
 .UNSPECIFIED., .F., .F.,
 ( 4, 2, 4 ),
 ( 1.056081928668503685E-17, 0.0002291978881530176780, 0.0004583957763060247850 ),
 .UNSPECIFIED. ) ;
#24427 = CARTESIAN_POINT ( 'NONE',  ( 5.910764540655177868, 10.83508461757094565, -16.94408981914462586 ) ) ;
#24428 =( BOUNDED_SURFACE ( )  B_SPLINE_SURFACE ( 3, 1, ( 
 ( #31266, #31576 ),
 ( #27182, #36293 ),
 ( #41608, #55054 ),
 ( #13406, #12799 ) ),
 .UNSPECIFIED., .F., .F., .F. ) 
 B_SPLINE_SURFACE_WITH_KNOTS ( ( 4, 4 ),
 ( 2, 2 ),
 ( 0.000000000000000000, 1.000000000000000000 ),
 ( 0.000000000000000000, 1.000000000000000000 ),
 .UNSPECIFIED. ) 
 GEOMETRIC_REPRESENTATION_ITEM ( )  RATIONAL_B_SPLINE_SURFACE ( (
 ( 1.000000000000000000, 1.000000000000000000),
 ( 0.9953040768229013402, 0.8617119497784988535),
 ( 0.9953040768229013402, 0.8617119497784988535),
 ( 1.000000000000000000, 1.000000000000000000) ) ) 
 REPRESENTATION_ITEM ( '' )  SURFACE ( )  );
#24429 = ORIENTED_EDGE ( 'NONE', *, *, #36238, .T. ) ;
#24430 = CARTESIAN_POINT ( 'NONE',  ( 5.895596859100789899, 12.98817590332804883, 15.35693556399505155 ) ) ;
#24431 = EDGE_CURVE ( 'NONE', #37022, #23510, #51420, .T. ) ;
#24432 = CARTESIAN_POINT ( 'NONE',  ( 0.5800708057587384836, 23.40241940841957202, 41.78924035064532205 ) ) ;
#24433 = VERTEX_POINT ( 'NONE', #24957 ) ;
#24434 = CARTESIAN_POINT ( 'NONE',  ( 0.7948878604505683620, -31.28609773251230664, -37.84017357214558075 ) ) ;
#24435 = ORIENTED_EDGE ( 'NONE', *, *, #35797, .F. ) ;
#24436 = CARTESIAN_POINT ( 'NONE',  ( 0.6254087463353893428, 33.52637152047081059, -34.49952850220934408 ) ) ;
#24437 = ORIENTED_EDGE ( 'NONE', *, *, #9538, .F. ) ;
#24438 = CARTESIAN_POINT ( 'NONE',  ( 0.1140933569871965259, 29.94445442560179771, -32.40801751475956394 ) ) ;
#24439 = LINE ( 'NONE', #6530, #23356 ) ;
#24440 = VERTEX_POINT ( 'NONE', #19039 ) ;
#24441 = CARTESIAN_POINT ( 'NONE',  ( 2.301529144917015213, -46.04684498357990918, 13.67115311793984311 ) ) ;
#24442 = B_SPLINE_CURVE_WITH_KNOTS ( 'NONE', 3,
 ( #41902, #24852, #60971, #23086 ),
 .UNSPECIFIED., .F., .F.,
 ( 4, 4 ),
 ( 0.000000000000000000, 0.005014147105413696917 ),
 .UNSPECIFIED. ) ;
#24443 = ORIENTED_EDGE ( 'NONE', *, *, #59241, .F. ) ;
#24444 = CARTESIAN_POINT ( 'NONE',  ( 4.962356264823608143, 0.000000000000000000, 0.000000000000000000 ) ) ;
#24445 = CARTESIAN_POINT ( 'NONE',  ( 4.962356264823608143, -10.17958088187436871, 40.83640203215416165 ) ) ;
#24446 = CARTESIAN_POINT ( 'NONE',  ( 0.6023143664670691511, -38.32505149877531636, 29.07782746490689973 ) ) ;
#24447 = AXIS2_PLACEMENT_3D ( 'NONE', #13843, #57318, #18225 ) ;
#24448 = ORIENTED_EDGE ( 'NONE', *, *, #15305, .F. ) ;
#24449 = CARTESIAN_POINT ( 'NONE',  ( 2.009741617377216460, -36.09682931428869779, -25.22940726767382813 ) ) ;
#24450 = CARTESIAN_POINT ( 'NONE',  ( 14.84250595937556483, 5.000000000000012434, -2.300655493813809945E-30 ) ) ;
#24451 = CARTESIAN_POINT ( 'NONE',  ( 0.8557997880470599172, -29.88293891557496096, 37.44587306708088192 ) ) ;
#24452 = ORIENTED_EDGE ( 'NONE', *, *, #20237, .F. ) ;
#24453 = B_SPLINE_CURVE_WITH_KNOTS ( 'NONE', 3,
 ( #8578, #18939, #57107, #14239, #60577, #27705 ),
 .UNSPECIFIED., .F., .F.,
 ( 4, 2, 4 ),
 ( 0.000000000000000000, 0.0002450742804987333630, 0.0004901485609974667260 ),
 .UNSPECIFIED. ) ;
#24454 = EDGE_CURVE ( 'NONE', #19345, #11856, #52516, .T. ) ;
#24455 = CARTESIAN_POINT ( 'NONE',  ( 0.5837374860065638327, -33.99581326751410870, -33.73893264285585047 ) ) ;
#24456 = CARTESIAN_POINT ( 'NONE',  ( 3.660087539127326206, -40.62968541507459719, 25.63019641081313438 ) ) ;
#24457 = AXIS2_PLACEMENT_3D ( 'NONE', #12092, #2028, #31801 ) ;
#24458 = ORIENTED_EDGE ( 'NONE', *, *, #11747, .T. ) ;
#24459 = CARTESIAN_POINT ( 'NONE',  ( 3.680974057930774812, 39.15945827951711067, -27.71659654258255046 ) ) ;
#24460 = ADVANCED_FACE ( 'NONE', ( #47845 ), #21794, .F. ) ;
#24461 = ORIENTED_EDGE ( 'NONE', *, *, #4934, .F. ) ;
#24462 = CARTESIAN_POINT ( 'NONE',  ( 0.9741495583595161101, 25.80610403442907952, 34.28086552274301368 ) ) ;
#24463 = CARTESIAN_POINT ( 'NONE',  ( 4.963659409799332067, 29.14784479683110163, 33.96111158240255889 ) ) ;
#24464 = ORIENTED_EDGE ( 'NONE', *, *, #46010, .T. ) ;
#24465 = CARTESIAN_POINT ( 'NONE',  ( 0.5806925824938502512, -14.41498975133575300, -44.62544602368080859 ) ) ;
#24466 = CARTESIAN_POINT ( 'NONE',  ( 6.999999999999992895, 72.00000000000002842, -4.718528363748726964E-31 ) ) ;
#24467 = CARTESIAN_POINT ( 'NONE',  ( 0.1368894036331274877, -0.7768805341913491702, 44.11641171445076282 ) ) ;
#24468 = CARTESIAN_POINT ( 'NONE',  ( 5.901764892641307547, -37.31543133725939043, 31.71040919877821906 ) ) ;
#24469 = ADVANCED_FACE ( 'NONE', ( #11167 ), #10910, .F. ) ;
#24470 = EDGE_CURVE ( 'NONE', #58260, #23595, #17833, .T. ) ;
#24471 = EDGE_LOOP ( 'NONE', ( #34530, #32846, #60176, #57408 ) ) ;
#24472 = CARTESIAN_POINT ( 'NONE',  ( 0.1157991065609915854, -40.92991374543836969, 16.48285552714316893 ) ) ;
#24473 = EDGE_CURVE ( 'NONE', #50534, #54562, #604, .T. ) ;
#24474 = CARTESIAN_POINT ( 'NONE',  ( 3.678949249685231848, 0.000000000000000000, 0.000000000000000000 ) ) ;
#24475 = CARTESIAN_POINT ( 'NONE',  ( 0.5839880159502333079, -44.23273844814451650, -18.37091806000283967 ) ) ;
#24476 = CARTESIAN_POINT ( 'NONE',  ( 0.8557997880470599172, 0.9121262075952832893, -47.89938907511592703 ) ) ;
#24477 = CARTESIAN_POINT ( 'NONE',  ( 0.3622758884714730732, 20.83792692158972670, -37.74294673546565804 ) ) ;
#24478 = CIRCLE ( 'NONE', #59475, 47.09074272231896430 ) ;
#24479 = EDGE_CURVE ( 'NONE', #58937, #27859, #37258, .T. ) ;
#24480 = DIRECTION ( 'NONE',  ( 0.000000000000000000, 0.000000000000000000, 1.000000000000000000 ) ) ;
#24481 = CARTESIAN_POINT ( 'NONE',  ( 3.660176727303401378, -25.63023984566673974, 40.62966184289481220 ) ) ;
#24482 = CARTESIAN_POINT ( 'NONE',  ( 0.8560838555295223751, 46.60258007729417784, 5.345312359546021241 ) ) ;
#24483 = DIRECTION ( 'NONE',  ( 0.1011922191286468153, 0.8906890386588646180, -0.4432078194264711390 ) ) ;
#24484 = CARTESIAN_POINT ( 'NONE',  ( 0.2940133293162988104, 34.10816071058727772, -27.97988424777333449 ) ) ;
#24485 = CARTESIAN_POINT ( 'NONE',  ( 7.000000000000019540, -72.00000000000002842, 8.817456953860946444E-15 ) ) ;
#24486 = CARTESIAN_POINT ( 'NONE',  ( 0.1156495703730067853, 39.81346568422283383, 19.02185331250035460 ) ) ;
#24487 = CARTESIAN_POINT ( 'NONE',  ( -6.016761891674564211, 4.880293656734964181, 18.20023637398600869 ) ) ;
#24488 = FACE_OUTER_BOUND ( 'NONE', #47964, .T. ) ;
#24489 = CARTESIAN_POINT ( 'NONE',  ( 0.5997462898726536595, -39.66574928371259290, 28.95133786038155321 ) ) ;
#24490 = ORIENTED_EDGE ( 'NONE', *, *, #4012, .T. ) ;
#24491 = CARTESIAN_POINT ( 'NONE',  ( 4.553261556744875094, -3.993093339916522488, -43.74465420371214464 ) ) ;
#24492 = AXIS2_PLACEMENT_3D ( 'NONE', #17114, #45326, #46549 ) ;
#24493 = CARTESIAN_POINT ( 'NONE',  ( 0.9788927965476029724, -1.258742425780537078, 41.88976223538774235 ) ) ;
#24494 = CARTESIAN_POINT ( 'NONE',  ( 1.157643937452370597, 38.26069984755655184, -17.12078040773669230 ) ) ;
#24495 = VERTEX_POINT ( 'NONE', #35905 ) ;
#24496 = CARTESIAN_POINT ( 'NONE',  ( 5.960721111146673579, -20.35079619394247885, 2.672857320902960243 ) ) ;
#24497 = LINE ( 'NONE', #4436, #7940 ) ;
#24498 = EDGE_LOOP ( 'NONE', ( #44673, #51140, #22224, #1197 ) ) ;
#24499 = ORIENTED_EDGE ( 'NONE', *, *, #42718, .T. ) ;
#24500 = EDGE_CURVE ( 'NONE', #15229, #19843, #30003, .T. ) ;
#24502 = ORIENTED_EDGE ( 'NONE', *, *, #18245, .T. ) ;
#24501 =( BOUNDED_SURFACE ( )  B_SPLINE_SURFACE ( 3, 1, ( 
 ( #44860, #40787 ),
 ( #58589, #30722 ),
 ( #12266, #35451 ),
 ( #54509, #11022 ) ),
 .UNSPECIFIED., .F., .F., .F. ) 
 B_SPLINE_SURFACE_WITH_KNOTS ( ( 4, 4 ),
 ( 2, 2 ),
 ( 0.000000000000000000, 1.000000000000000000 ),
 ( 0.000000000000000000, 1.000000000000000000 ),
 .UNSPECIFIED. ) 
 GEOMETRIC_REPRESENTATION_ITEM ( )  RATIONAL_B_SPLINE_SURFACE ( (
 ( 1.000000000000000000, 1.000000000000000000),
 ( 0.7269869731126817891, 0.9931720237060910339),
 ( 0.7269869731126817891, 0.9931720237060910339),
 ( 1.000000000000000000, 1.000000000000000000) ) ) 
 REPRESENTATION_ITEM ( '' )  SURFACE ( )  );
#24503 = CARTESIAN_POINT ( 'NONE',  ( 0.8560838555295223751, 28.55542365806889293, 37.21505896528891810 ) ) ;
#24504 = VERTEX_POINT ( 'NONE', #1731 ) ;
#24505 = ORIENTED_EDGE ( 'NONE', *, *, #7228, .T. ) ;
#24506 = CARTESIAN_POINT ( 'NONE',  ( 0.1104177457020373426, 11.16615714989251096, 41.65375561851289632 ) ) ;
#24507 = ORIENTED_EDGE ( 'NONE', *, *, #37068, .T. ) ;
#24508 = DIRECTION ( 'NONE',  ( 0.000000000000000000, 0.000000000000000000, 1.000000000000000000 ) ) ;
#24509 = DIRECTION ( 'NONE',  ( 0.000000000000000000, 0.000000000000000000, 1.000000000000000000 ) ) ;
#24510 = CARTESIAN_POINT ( 'NONE',  ( 0.1097557419366048670, -30.65094619415046751, -30.33543403792227267 ) ) ;
#24511 = ORIENTED_EDGE ( 'NONE', *, *, #60317, .T. ) ;
#24512 = CARTESIAN_POINT ( 'NONE',  ( 0.8744876279028306332, -13.11369837310865805, 47.31153099782990523 ) ) ;
#24513 = AXIS2_PLACEMENT_3D ( 'NONE', #14969, #5523, #34079 ) ;
#24514 = CARTESIAN_POINT ( 'NONE',  ( 0.9757892942422830007, -34.07281211842306590, -26.08029006934572180 ) ) ;
#24515 = ORIENTED_EDGE ( 'NONE', *, *, #4864, .F. ) ;
#24516 = ORIENTED_EDGE ( 'NONE', *, *, #49157, .T. ) ;
#24517 =( BOUNDED_SURFACE ( )  B_SPLINE_SURFACE ( 3, 1, ( 
 ( #12567, #56370 ),
 ( #46387, #2515 ),
 ( #17566, #56064 ),
 ( #26641, #40782 ) ),
 .UNSPECIFIED., .F., .F., .F. ) 
 B_SPLINE_SURFACE_WITH_KNOTS ( ( 4, 4 ),
 ( 2, 2 ),
 ( 0.000000000000000000, 1.000000000000000000 ),
 ( 0.000000000000000000, 1.000000000000000000 ),
 .UNSPECIFIED. ) 
 GEOMETRIC_REPRESENTATION_ITEM ( )  RATIONAL_B_SPLINE_SURFACE ( (
 ( 1.000000000000000000, 1.000000000000000000),
 ( 0.9953485035131437453, 0.8621029689291523912),
 ( 0.9953485035131437453, 0.8621029689291523912),
 ( 1.000000000000000000, 1.000000000000000000) ) ) 
 REPRESENTATION_ITEM ( '' )  SURFACE ( )  );
#24518 = CARTESIAN_POINT ( 'NONE',  ( -6.016104459813371719, 14.94608397322100224, -11.47525878590901094 ) ) ;
#24519 = B_SPLINE_CURVE_WITH_KNOTS ( 'NONE', 3,
 ( #11854, #55029, #56881, #42823, #19312, #61877, #19015, #47507, #41901, #52493, #46909, #14007, #32802, #51560, #27462, #13382 ),
 .UNSPECIFIED., .F., .F.,
 ( 4, 3, 3, 3, 3, 4 ),
 ( 2.221635811791082109E-17, 0.0002612764279487786922, 0.0003919131003184823893, 0.0005225497727000684000, 0.0007837925190632490406, 0.001045051706266717385 ),
 .UNSPECIFIED. ) ;
#24520 = ORIENTED_EDGE ( 'NONE', *, *, #23185, .T. ) ;
#24521 = CARTESIAN_POINT ( 'NONE',  ( 48.50503732531682033, 12.37710729184128944, 1.752842796636026490 ) ) ;
#24522 = CARTESIAN_POINT ( 'NONE',  ( 0.1073791018717578927, -41.52698815987159264, -11.62916352156135780 ) ) ;
#24523 = CARTESIAN_POINT ( 'NONE',  ( 3.782625744892851305, 27.96054597547522391, -31.39181378716972404 ) ) ;
#24524 = CARTESIAN_POINT ( 'NONE',  ( 0.7056759521544994085, -0.7243499498853074314, -46.89588624034189479 ) ) ;
#24525 =( BOUNDED_SURFACE ( )  B_SPLINE_SURFACE ( 3, 1, ( 
 ( #49896, #60204 ),
 ( #59903, #50812 ),
 ( #22016, #45523 ),
 ( #21080, #7903 ) ),
 .UNSPECIFIED., .F., .F., .F. ) 
 B_SPLINE_SURFACE_WITH_KNOTS ( ( 4, 4 ),
 ( 2, 2 ),
 ( 0.000000000000000000, 1.000000000000000000 ),
 ( 0.000000000000000000, 1.000000000000000000 ),
 .UNSPECIFIED. ) 
 GEOMETRIC_REPRESENTATION_ITEM ( )  RATIONAL_B_SPLINE_SURFACE ( (
 ( 1.000000000000000000, 1.000000000000000000),
 ( 0.9952954269826590483, 0.8620686068821307169),
 ( 0.9952954269826590483, 0.8620686068821307169),
 ( 1.000000000000000000, 1.000000000000000000) ) ) 
 REPRESENTATION_ITEM ( '' )  SURFACE ( )  );
#24526 = EDGE_CURVE ( 'NONE', #20520, #1247, #7247, .T. ) ;
#24527 = B_SPLINE_CURVE_WITH_KNOTS ( 'NONE', 3,
 ( #7844, #11322, #2204, #35141, #17263, #55139 ),
 .UNSPECIFIED., .F., .F.,
 ( 4, 2, 4 ),
 ( 7.913933220075304459E-18, 0.0002448709889506558556, 0.0004897419779013037966 ),
 .UNSPECIFIED. ) ;
#24528 = EDGE_LOOP ( 'NONE', ( #2676, #55037 ) ) ;
#24529 = CARTESIAN_POINT ( 'NONE',  ( 0.1152339509894530906, -1.637524258439203573, -44.09377739271456420 ) ) ;
#24530 = CARTESIAN_POINT ( 'NONE',  ( 0.9762797500689124330, 41.46413394121034912, 6.086902470967687329 ) ) ;
#24531 = ADVANCED_FACE ( 'NONE', ( #50587 ), #3962, .T. ) ;
#24532 = CARTESIAN_POINT ( 'NONE',  ( 0.5797568665920715958, -30.75502540147657271, -35.40273606878996304 ) ) ;
#24533 = CARTESIAN_POINT ( 'NONE',  ( 4.549368137175248350, -8.166781970326043805, 42.14271863032818999 ) ) ;
#24534 = CIRCLE ( 'NONE', #57551, 10.00000000000000000 ) ;
#24535 = ORIENTED_EDGE ( 'NONE', *, *, #36764, .F. ) ;
#24536 = CARTESIAN_POINT ( 'NONE',  ( 0.7044674535452954967, -29.95677278048739467, -38.91522179545113858 ) ) ;
#24537 = CARTESIAN_POINT ( 'NONE',  ( 0.1158403557922069033, 37.00056559947007173, -24.03951855805625115 ) ) ;
#24538 = EDGE_CURVE ( 'NONE', #44946, #3395, #28980, .T. ) ;
#24539 = CARTESIAN_POINT ( 'NONE',  ( 1.231276596079881935, 41.65019306089989470, -4.747440258479600494 ) ) ;
#24540 = CARTESIAN_POINT ( 'NONE',  ( 0.6021447746440204973, -35.45755941940524281, -33.97502934668098362 ) ) ;
#24541 = EDGE_CURVE ( 'NONE', #29203, #57580, #26690, .T. ) ;
#24543 = ORIENTED_EDGE ( 'NONE', *, *, #34693, .F. ) ;
#24542 = CIRCLE ( 'NONE', #29540, 43.08621763946400307 ) ;
#24544 = EDGE_LOOP ( 'NONE', ( #9962, #30973 ) ) ;
#24545 = FACE_BOUND ( 'NONE', #8725, .T. ) ;
#24546 = EDGE_CURVE ( 'NONE', #11211, #54760, #53521, .T. ) ;
#24547 = CARTESIAN_POINT ( 'NONE',  ( 0.9730545539215883499, -21.01499094264522682, -37.40983423658496321 ) ) ;
#24548 = CARTESIAN_POINT ( 'NONE',  ( 1.154321485836933059, -17.18284940416421591, -39.32643515542051915 ) ) ;
#24549 = CIRCLE ( 'NONE', #37589, 10.00000000000000711 ) ;
#24550 = CARTESIAN_POINT ( 'NONE',  ( 5.896782393890504181, -11.93563916323493146, 16.18847134979287361 ) ) ;
#24551 = B_SPLINE_CURVE_WITH_KNOTS ( 'NONE', 3,
 ( #12377, #46202, #54316, #7639, #31786, #11439, #30521, #49958, #49638, #7011, #45281, #7321, #26145, #2323, #35874, #42734, #8895, #51796, #37120 ),
 .UNSPECIFIED., .F., .F.,
 ( 4, 3, 3, 3, 3, 3, 4 ),
 ( 0.000000000000000000, 0.0002724573126191774902, 0.0004086839781548475556, 0.0005449106435901796431, 0.0006811373090491484221, 0.0008459866663933725186, 0.001010840725717214450 ),
 .UNSPECIFIED. ) ;
#24552 = DIRECTION ( 'NONE',  ( 0.1736481776669314137, -0.9848077530122077983, 5.551115123125779004E-17 ) ) ;
#24553 = B_SPLINE_CURVE_WITH_KNOTS ( 'NONE', 3,
 ( #33398, #13674, #9888, #48105 ),
 .UNSPECIFIED., .F., .F.,
 ( 4, 4 ),
 ( 2.010076909634645264E-17, 0.004444306975806113294 ),
 .UNSPECIFIED. ) ;
#24554 = CARTESIAN_POINT ( 'NONE',  ( 0.1158516988532803799, -31.66230134112594286, 30.73175609392555430 ) ) ;
#24555 = FACE_OUTER_BOUND ( 'NONE', #11289, .T. ) ;
#24556 = CARTESIAN_POINT ( 'NONE',  ( -2.601141883200665639, 14.73012113219610342, -2.412251831840622973 ) ) ;
#24557 = CARTESIAN_POINT ( 'NONE',  ( 5.895596859100789899, 19.00119700155552493, 6.594141014610245932 ) ) ;
#24558 = CARTESIAN_POINT ( 'NONE',  ( 2.643462169533613793, 32.97543604874675083, -34.93025802711691341 ) ) ;
#24559 = CARTESIAN_POINT ( 'NONE',  ( 1.227938101723756947, 11.92353943227949387, 41.23019537246713639 ) ) ;
#24561 = ORIENTED_EDGE ( 'NONE', *, *, #53581, .T. ) ;
#24560 = ADVANCED_FACE ( 'NONE', ( #32745 ), #446, .F. ) ;
#24562 = CARTESIAN_POINT ( 'NONE',  ( 0.9722240750034567558, -42.46141201102050644, 6.177112354444973086 ) ) ;
#24563 = CARTESIAN_POINT ( 'NONE',  ( 0.1103310638050662290, -34.16271402810851043, -26.31782144882228636 ) ) ;
#24565 = EDGE_CURVE ( 'NONE', #39339, #7638, #60287, .T. ) ;
#24564 = CARTESIAN_POINT ( 'NONE',  ( 0.1135584504625008206, -35.61847315347595355, 26.04374055988050074 ) ) ;
#24566 = CARTESIAN_POINT ( 'NONE',  ( 0.8554163680231720024, 37.37991192211390512, 28.35397075908108988 ) ) ;
#24567 = B_SPLINE_CURVE_WITH_KNOTS ( 'NONE', 3,
 ( #36780, #49607, #6667, #1989, #44948, #40256 ),
 .UNSPECIFIED., .F., .F.,
 ( 4, 2, 4 ),
 ( 6.992893892674702526E-18, 0.0002291472222819966218, 0.0004582944445639862505 ),
 .UNSPECIFIED. ) ;
#24568 = CARTESIAN_POINT ( 'NONE',  ( 0.6023143664670691511, -24.28012784216906894, 41.53077189784221446 ) ) ;
#24569 = CARTESIAN_POINT ( 'NONE',  ( 0.6027935024548037868, -46.51312430684514254, 12.28245664247765490 ) ) ;
#24570 = CARTESIAN_POINT ( 'NONE',  ( 0.5806925824938499181, 45.37089516811292356, -11.86188155343291584 ) ) ;
#24571 = ITEM_DEFINED_TRANSFORMATION ( 'NONE', 'NONE', #43919,  #14677 ) ;
#24572 = CARTESIAN_POINT ( 'NONE',  ( 0.9754642270333674370, -26.26019354539063144, 33.93430397636404905 ) ) ;
#24573 = CARTESIAN_POINT ( 'NONE',  ( 5.958863334805807099, 12.49425770716465678, 16.28483817244743292 ) ) ;
#24574 = CARTESIAN_POINT ( 'NONE',  ( 0.9745511491811743587, -11.43411988112632471, 41.35688774886285302 ) ) ;
#24575 = CARTESIAN_POINT ( 'NONE',  ( 4.549368137175248350, -23.67244292351614376, -35.80950303116092925 ) ) ;
#24576 = CARTESIAN_POINT ( 'NONE',  ( 0.6041374136657475802, -12.28249295042015277, -46.51335992032614541 ) ) ;
#24578 = ORIENTED_EDGE ( 'NONE', *, *, #10779, .T. ) ;
#24577 = DIRECTION ( 'NONE',  ( 0.000000000000000000, -0.000000000000000000, 1.000000000000000000 ) ) ;
#24579 = ORIENTED_EDGE ( 'NONE', *, *, #53087, .T. ) ;
#24580 = CARTESIAN_POINT ( 'NONE',  ( 0.1064266379913943183, -33.86837498006642733, 26.69589650908227796 ) ) ;
#24581 = CARTESIAN_POINT ( 'NONE',  ( 2.009741617377216460, 43.84020297899651553, -4.188159546081140938 ) ) ;
#24582 = CARTESIAN_POINT ( 'NONE',  ( 0.7948884756798493267, -34.66113248934519220, -34.77505627826086965 ) ) ;
#24583 = ORIENTED_EDGE ( 'NONE', *, *, #12113, .T. ) ;
#24584 = DIRECTION ( 'NONE',  ( 0.07906939808003032866, 0.8172634100797984136, 0.5708139353870058663 ) ) ;
#24585 = LINE ( 'NONE', #61841, #37174 ) ;
#24586 = CARTESIAN_POINT ( 'NONE',  ( 0.5838002273316443835, -41.41085122398235541, -24.06583301632245409 ) ) ;
#24587 = ORIENTED_EDGE ( 'NONE', *, *, #6820, .T. ) ;
#24588 = EDGE_LOOP ( 'NONE', ( #35784, #368, #35265, #7320 ) ) ;
#24589 = EDGE_CURVE ( 'NONE', #29266, #6519, #8709, .T. ) ;
#24590 = CARTESIAN_POINT ( 'NONE',  ( 0.6017667736363750963, -23.75082673020834534, -41.83584368312182988 ) ) ;
#24591 = LINE ( 'NONE', #38105, #18343 ) ;
#24592 = CARTESIAN_POINT ( 'NONE',  ( 0.8557997880470697982, -41.02602466100796619, 24.73961900479237386 ) ) ;
#24593 = AXIS2_PLACEMENT_3D ( 'NONE', #27367, #45568, #31772 ) ;
#24594 = CARTESIAN_POINT ( 'NONE',  ( 0.5837157313716048179, 46.89593559896864861, 0.09103779108274359655 ) ) ;
#24596 = CARTESIAN_POINT ( 'NONE',  ( 0.9785694773339255192, -41.02396546051519266, -8.565609354221619398 ) ) ;
#24595 = CIRCLE ( 'NONE', #39639, 43.92652462719577500 ) ;
#24597 = B_SPLINE_CURVE_WITH_KNOTS ( 'NONE', 3,
 ( #30858, #7034, #35894, #26162, #2343, #45299, #42154, #13628, #3262, #36511, #60277, #56204, #32733, #32113, #22392, #37442, #8588, #46222, #61209 ),
 .UNSPECIFIED., .F., .F.,
 ( 4, 3, 3, 3, 3, 3, 4 ),
 ( 4.878909776184769953E-18, 0.0002724573126191761892, 0.0004086839781548490735, 0.0005449106435901837631, 0.0006811373090491487474, 0.0008459866663933690491, 0.001010840725717212715 ),
 .UNSPECIFIED. ) ;
#24598 = DIRECTION ( 'NONE',  ( -1.000000000000000000, -0.000000000000000000, -0.000000000000000000 ) ) ;
#24599 = B_SPLINE_CURVE_WITH_KNOTS ( 'NONE', 3,
 ( #43395, #60685, #17493, #61002 ),
 .UNSPECIFIED., .F., .F.,
 ( 4, 4 ),
 ( 3.878959614448863476E-18, 0.004042984057420973693 ),
 .UNSPECIFIED. ) ;
#24600 = CARTESIAN_POINT ( 'NONE',  ( 5.959828726073459926, 2.674641840415901139, 20.35060134307035540 ) ) ;
#24601 = ORIENTED_EDGE ( 'NONE', *, *, #47344, .F. ) ;
#24602 = CIRCLE ( 'NONE', #32615, 8.000000000000000000 ) ;
#24603 = EDGE_LOOP ( 'NONE', ( #30864, #61517, #1367, #4523 ) ) ;
#24604 = LINE ( 'NONE', #43740, #34836 ) ;
#24605 = CARTESIAN_POINT ( 'NONE',  ( 0.5549461598389365813, 44.06152503503679441, 1.949283728355195811 ) ) ;
#24606 = VERTEX_POINT ( 'NONE', #46854 ) ;
#24607 = CARTESIAN_POINT ( 'NONE',  ( 0.9789889208857711633, -37.44753480729469430, -18.81534041410943559 ) ) ;
#24608 = CARTESIAN_POINT ( 'NONE',  ( 4.335381028904216727, -46.16199858719131299, -16.39593651184625500 ) ) ;
#24609 = FACE_OUTER_BOUND ( 'NONE', #23819, .T. ) ;
#24610 = CARTESIAN_POINT ( 'NONE',  ( 0.5806925824938499181, 28.25565086187788921, -37.42780459384738379 ) ) ;
#24611 = ORIENTED_EDGE ( 'NONE', *, *, #40922, .F. ) ;
#24612 = CARTESIAN_POINT ( 'NONE',  ( 0.3622758884714600280, 4.808133778521302304, 42.84426538328732903 ) ) ;
#24613 = CARTESIAN_POINT ( 'NONE',  ( 0.6001305935487422083, -44.64600790884043846, -17.92615948558524863 ) ) ;
#24614 = CARTESIAN_POINT ( 'NONE',  ( 0.6253024248130462093, 28.65516068116093606, -39.87889158131772405 ) ) ;
#24615 =( BOUNDED_SURFACE ( )  B_SPLINE_SURFACE ( 3, 1, ( 
 ( #58831, #30335 ),
 ( #54124, #44782 ),
 ( #40094, #38849 ),
 ( #35067, #15338 ) ),
 .UNSPECIFIED., .F., .F., .F. ) 
 B_SPLINE_SURFACE_WITH_KNOTS ( ( 4, 4 ),
 ( 2, 2 ),
 ( 0.000000000000000000, 1.000000000000000000 ),
 ( 0.000000000000000000, 1.000000000000000000 ),
 .UNSPECIFIED. ) 
 GEOMETRIC_REPRESENTATION_ITEM ( )  RATIONAL_B_SPLINE_SURFACE ( (
 ( 1.000000000000000000, 1.000000000000000000),
 ( 0.9953390228620291325, 0.8624445117761032620),
 ( 0.9953390228620291325, 0.8624445117761032620),
 ( 1.000000000000000000, 1.000000000000000000) ) ) 
 REPRESENTATION_ITEM ( '' )  SURFACE ( )  );
#24616 = CARTESIAN_POINT ( 'NONE',  ( 0.5819845901640484653, 28.79568196372268574, 38.27312528999442520 ) ) ;
#24617 = ORIENTED_EDGE ( 'NONE', *, *, #53045, .T. ) ;
#24618 = CARTESIAN_POINT ( 'NONE',  ( -6.016761891674564211, 13.32172022638610365, -13.32657647165341253 ) ) ;
#24619 = EDGE_CURVE ( 'NONE', #2619, #51439, #4196, .T. ) ;
#24620 = ORIENTED_EDGE ( 'NONE', *, *, #17706, .F. ) ;
#24621 = CARTESIAN_POINT ( 'NONE',  ( 3.661933894777869902, -3.452430679485475107, 46.91174572913485008 ) ) ;
#24622 = CARTESIAN_POINT ( 'NONE',  ( 0.5839879882012682932, 23.94795769224444726, -41.47913983251925885 ) ) ;
#24623 =( BOUNDED_SURFACE ( )  B_SPLINE_SURFACE ( 3, 1, ( 
 ( #7083, #40346 ),
 ( #59407, #15599 ),
 ( #49100, #1161 ),
 ( #11837, #59721 ) ),
 .UNSPECIFIED., .F., .F., .F. ) 
 B_SPLINE_SURFACE_WITH_KNOTS ( ( 4, 4 ),
 ( 2, 2 ),
 ( 0.000000000000000000, 1.000000000000000000 ),
 ( 0.000000000000000000, 1.000000000000000000 ),
 .UNSPECIFIED. ) 
 GEOMETRIC_REPRESENTATION_ITEM ( )  RATIONAL_B_SPLINE_SURFACE ( (
 ( 1.000000000000000000, 1.000000000000000000),
 ( 0.7211978278499968642, 0.9934217856018975334),
 ( 0.7211978278499968642, 0.9934217856018975334),
 ( 1.000000000000000000, 1.000000000000000000) ) ) 
 REPRESENTATION_ITEM ( '' )  SURFACE ( )  );
#24624 = VERTEX_POINT ( 'NONE', #31815 ) ;
#24625 = CARTESIAN_POINT ( 'NONE',  ( 1.827119703190779321, -25.21842556008211389, 34.89020442382214782 ) ) ;
#24626 = EDGE_CURVE ( 'NONE', #20133, #19445, #52087, .T. ) ;
#24627 = FACE_OUTER_BOUND ( 'NONE', #49476, .T. ) ;
#24628 = FACE_OUTER_BOUND ( 'NONE', #20319, .T. ) ;
#24629 = CARTESIAN_POINT ( 'NONE',  ( 4.322998006666179727, -47.94177812210863010, 2.120302895116117803 ) ) ;
#24630 = CARTESIAN_POINT ( 'NONE',  ( 0.1140933569871964842, 33.84285616430637589, -28.31273629881038190 ) ) ;
#24631 = CARTESIAN_POINT ( 'NONE',  ( 1.139999999999998570, 0.000000000000000000, 0.000000000000000000 ) ) ;
#24632 = CARTESIAN_POINT ( 'NONE',  ( 3.660176727303419586, 47.83637937224830949, -4.399934609596090951 ) ) ;
#24633 = CARTESIAN_POINT ( 'NONE',  ( 0.6067375320500718594, 47.89177856776005626, 0.7090021732335601845 ) ) ;
#24634 = ORIENTED_EDGE ( 'NONE', *, *, #12109, .T. ) ;
#24635 = CARTESIAN_POINT ( 'NONE',  ( 0.9745511491811736926, 39.77127619790164914, -16.10518088436863238 ) ) ;
#24636 = DIRECTION ( 'NONE',  ( -1.000000000000000000, -0.000000000000000000, -0.000000000000000000 ) ) ;
#24637 = CARTESIAN_POINT ( 'NONE',  ( 5.895596859100789899, -15.78680134203122165, 12.46214614742294913 ) ) ;
#24638 = VERTEX_POINT ( 'NONE', #36840 ) ;
#24639 = CIRCLE ( 'NONE', #42669, 15.71999999999999353 ) ;
#24640 = CONICAL_SURFACE ( 'NONE', #52656, 42.92674063221959813, 1.485477209440487556 ) ;
#24641 = CARTESIAN_POINT ( 'NONE',  ( 5.959547316686252039, 2.682663672454912440, -20.34955788964373724 ) ) ;
#24642 = CARTESIAN_POINT ( 'NONE',  ( -5.995132425357893702, -11.47834865841106300, 14.94489030678147401 ) ) ;
#24644 = EDGE_CURVE ( 'NONE', #14065, #54546, #46132, .T. ) ;
#24643 = CARTESIAN_POINT ( 'NONE',  ( 0.5987334308729321819, 10.33658553128385016, -48.00747760634984473 ) ) ;
#24645 = CARTESIAN_POINT ( 'NONE',  ( 0.8551540677456739292, -5.348818140990592163, -47.61725548905996419 ) ) ;
#24646 = CARTESIAN_POINT ( 'NONE',  ( -6.015611763856276717, -17.40650793417838571, -7.216738110653465377 ) ) ;
#24647 = CARTESIAN_POINT ( 'NONE',  ( 3.661921753702016780, -15.72362396054653999, -44.33281824316339481 ) ) ;
#24648 =( LENGTH_UNIT ( ) NAMED_UNIT ( * ) SI_UNIT ( .MILLI., .METRE. ) );
#24649 = FACE_OUTER_BOUND ( 'NONE', #36404, .T. ) ;
#24650 = DIRECTION ( 'NONE',  ( -1.000000000000000000, -0.000000000000000000, -0.000000000000000000 ) ) ;
#24651 = CARTESIAN_POINT ( 'NONE',  ( 0.9762797500689124330, -11.93232144563776487, -40.17392798947692256 ) ) ;
#24653 = EDGE_LOOP ( 'NONE', ( #57373, #58229, #6628, #14779 ) ) ;
#24652 = LINE ( 'NONE', #6124, #45372 ) ;
#24654 = ORIENTED_EDGE ( 'NONE', *, *, #35934, .F. ) ;
#24655 = CARTESIAN_POINT ( 'NONE',  ( 0.8560838555295223751, -6.899551485032601406, 46.39794201672221163 ) ) ;
#24656 = FACE_BOUND ( 'NONE', #8883, .T. ) ;
#24657 = CARTESIAN_POINT ( 'NONE',  ( 0.1103878639767399417, 16.54784522866413354, 39.82320122342710533 ) ) ;
#24658 = CARTESIAN_POINT ( 'NONE',  ( 0.9730545539215883499, 0.5054011016612682816, 42.90536227157002003 ) ) ;
#24659 = ORIENTED_EDGE ( 'NONE', *, *, #60237, .T. ) ;
#24660 = ADVANCED_FACE ( 'NONE', ( #45933 ), #41848, .F. ) ;
#24661 = CARTESIAN_POINT ( 'NONE',  ( 2.282803330402959130, 44.93953277324986573, 13.67242851796949665 ) ) ;
#24662 = CARTESIAN_POINT ( 'NONE',  ( -17.97369999999976642, -7.719455939378113030, 2.099999999999994760 ) ) ;
#24663 = CARTESIAN_POINT ( 'NONE',  ( 0.000000000000000000, 0.000000000000000000, -5.599999999999999645 ) ) ;
#24664 = ORIENTED_EDGE ( 'NONE', *, *, #56579, .F. ) ;
#24665 = B_SPLINE_CURVE_WITH_KNOTS ( 'NONE', 3,
 ( #7797, #36037, #22225, #27225 ),
 .UNSPECIFIED., .F., .F.,
 ( 4, 4 ),
 ( 6.505213034913026604E-19, 0.004041751736741000349 ),
 .UNSPECIFIED. ) ;
#24666 = ADVANCED_FACE ( 'NONE', ( #13328 ), #26077, .F. ) ;
#24667 = B_SPLINE_CURVE_WITH_KNOTS ( 'NONE', 3,
 ( #9334, #14986, #13756, #10274, #9643, #33473 ),
 .UNSPECIFIED., .F., .F.,
 ( 4, 2, 4 ),
 ( 3.511543213478341086E-18, 0.0002445244328975359387, 0.0004890488657950682995 ),
 .UNSPECIFIED. ) ;
#24668 = CARTESIAN_POINT ( 'NONE',  ( 5.960721111146673579, -12.49016043756459915, -16.28787783074223228 ) ) ;
#24669 = CARTESIAN_POINT ( 'NONE',  ( 0.5837374860065647209, 47.46223477511620814, -6.431731162805296442 ) ) ;
#24670 = VERTEX_POINT ( 'NONE', #5120 ) ;
#24671 = ADVANCED_FACE ( 'NONE', ( #39299 ), #38920, .F. ) ;
#24672 = CARTESIAN_POINT ( 'NONE',  ( 0.8744876279028263033, -47.25615711918255357, -13.31186180466976587 ) ) ;
#24673 = VECTOR ( 'NONE', #43456, 1000.000000000000227 ) ;
#24674 = ORIENTED_EDGE ( 'NONE', *, *, #51052, .F. ) ;
#24675 = CARTESIAN_POINT ( 'NONE',  ( -2.569797478183790229, 4.218948559326250347, -14.01151037928418930 ) ) ;
#24676 = CARTESIAN_POINT ( 'NONE',  ( 2.299652685299200972, -15.18162634922640564, 46.62402756359244904 ) ) ;
#24677 =( GEOMETRIC_REPRESENTATION_CONTEXT ( 3 ) GLOBAL_UNCERTAINTY_ASSIGNED_CONTEXT ( ( #52377 ) ) GLOBAL_UNIT_ASSIGNED_CONTEXT ( ( #27903, #22900, #41409 ) ) REPRESENTATION_CONTEXT ( 'NONE', 'WORKASPACE' ) );
#24678 = VERTEX_POINT ( 'NONE', #42767 ) ;
#24679 = CARTESIAN_POINT ( 'NONE',  ( 5.896782393890504181, 19.00205529748287248, 6.591508275760228130 ) ) ;
#24680 = CARTESIAN_POINT ( 'NONE',  ( 0.5782707292762423457, -44.53844888462747775, -14.69907904118641007 ) ) ;
#24681 = CARTESIAN_POINT ( 'NONE',  ( 0.9783242366443547500, 40.34793699461262406, 11.33042234364170397 ) ) ;
#24682 = DIRECTION ( 'NONE',  ( 0.000000000000000000, 0.000000000000000000, 1.000000000000000000 ) ) ;
#24683 = EDGE_LOOP ( 'NONE', ( #2424, #15067, #18337, #43324 ) ) ;
#24684 = CARTESIAN_POINT ( 'NONE',  ( 2.618530812446115519, -37.94055228201274588, 27.75322110555919508 ) ) ;
#24685 = CARTESIAN_POINT ( 'NONE',  ( 5.981074661064941900, 16.28853686865582517, 12.48781255314294469 ) ) ;
#24686 = ORIENTED_EDGE ( 'NONE', *, *, #43239, .T. ) ;
#24687 = LINE ( 'NONE', #872, #15206 ) ;
#24688 = ORIENTED_EDGE ( 'NONE', *, *, #37467, .T. ) ;
#24689 = CARTESIAN_POINT ( 'NONE',  ( 5.901764892641288895, 30.49809846213706521, -38.31262791343699092 ) ) ;
#24690 = EDGE_CURVE ( 'NONE', #18401, #15970, #14262, .T. ) ;
#24691 = EDGE_LOOP ( 'NONE', ( #43406, #4778, #29598, #60791 ) ) ;
#24692 = CARTESIAN_POINT ( 'NONE',  ( 0.6064515330803592619, -46.83442941052457087, -2.422923405243606609 ) ) ;
#24694 = VECTOR ( 'NONE', #52601, 1000.000000000000114 ) ;
#24693 = CARTESIAN_POINT ( 'NONE',  ( 5.981074661064941900, 17.77917279944618301, 10.25489689131136650 ) ) ;
#24695 = CARTESIAN_POINT ( 'NONE',  ( 0.2279481005628801182, 10.55626456711305217, -42.83770261652724543 ) ) ;
#24696 = VERTEX_POINT ( 'NONE', #4503 ) ;
#24697 = DIRECTION ( 'NONE',  ( 0.000000000000000000, 0.000000000000000000, 1.000000000000000000 ) ) ;
#24698 = EDGE_CURVE ( 'NONE', #21667, #8183, #59520, .T. ) ;
#24699 = CARTESIAN_POINT ( 'NONE',  ( 0.6067375320500733027, 11.71046088714751399, 46.44340905096866834 ) ) ;
#24700 = B_SPLINE_CURVE_WITH_KNOTS ( 'NONE', 3,
 ( #55707, #31614, #12220, #12523, #7793, #31304 ),
 .UNSPECIFIED., .F., .F.,
 ( 4, 2, 4 ),
 ( 1.738108305489988542E-18, 0.0002291459268755720237, 0.0004582918537511423127 ),
 .UNSPECIFIED. ) ;
#24701 = CARTESIAN_POINT ( 'NONE',  ( 0.8753041380234524160, -49.09527960836077654, 0.8898584437169385630 ) ) ;
#24702 = EDGE_LOOP ( 'NONE', ( #1674, #26029, #13587, #49040 ) ) ;
#24703 = CIRCLE ( 'NONE', #4669, 43.08621763946400307 ) ;
#24704 = ADVANCED_FACE ( 'NONE', ( #29563 ), #45318, .F. ) ;
#24705 = ORIENTED_EDGE ( 'NONE', *, *, #51226, .F. ) ;
#24706 = CARTESIAN_POINT ( 'NONE',  ( 0.9788927965476029724, -31.17652977587658825, -28.00643861267721846 ) ) ;
#24707 = LINE ( 'NONE', #53796, #17951 ) ;
#24708 = CARTESIAN_POINT ( 'NONE',  ( 0.6252788684277210685, -13.31242424175264460, 47.26757548236700757 ) ) ;
#24709 = CARTESIAN_POINT ( 'NONE',  ( 0.7242486021783849370, -45.81454891244490568, 17.66461350619272963 ) ) ;
#24710 = ORIENTED_EDGE ( 'NONE', *, *, #52298, .T. ) ;
#24711 = ORIENTED_EDGE ( 'NONE', *, *, #2527, .F. ) ;
#24712 = CARTESIAN_POINT ( 'NONE',  ( -6.057079549204054558, 18.62933071312879818, -4.876399110062101805 ) ) ;
#24714 = EDGE_CURVE ( 'NONE', #40578, #18068, #28335, .T. ) ;
#24713 = CARTESIAN_POINT ( 'NONE',  ( 0.5809828226811617480, -38.32755012159166341, 28.72298383114474518 ) ) ;
#24715 = CARTESIAN_POINT ( 'NONE',  ( 0.3622758884714730732, -11.95365414648468594, -41.42293301073622303 ) ) ;
#24716 = B_SPLINE_CURVE_WITH_KNOTS ( 'NONE', 3,
 ( #17544, #12863, #27249, #36662, #41672, #27862 ),
 .UNSPECIFIED., .F., .F.,
 ( 4, 2, 4 ),
 ( 8.484948815274053452E-17, 0.0002293366620881442529, 0.0004586733241762036670 ),
 .UNSPECIFIED. ) ;
#24717 = DIRECTION ( 'NONE',  ( 0.000000000000000000, 0.000000000000000000, -1.000000000000000000 ) ) ;
#24718 = CARTESIAN_POINT ( 'NONE',  ( 0.6000166863083090663, -48.63754814943176541, -6.797969676319537413 ) ) ;
#24719 =( NAMED_UNIT ( * ) SI_UNIT ( $, .STERADIAN. ) SOLID_ANGLE_UNIT ( ) );
#24720 = CARTESIAN_POINT ( 'NONE',  ( 4.956445790443998689, -11.44166143952028314, 45.67960632101629415 ) ) ;
#24721 = B_SPLINE_CURVE_WITH_KNOTS ( 'NONE', 3,
 ( #40237, #26098, #2270, #40533 ),
 .UNSPECIFIED., .F., .F.,
 ( 4, 4 ),
 ( 2.043828937333572736E-17, 0.004444306975806114161 ),
 .UNSPECIFIED. ) ;
#24722 = CIRCLE ( 'NONE', #59714, 48.91267123290010943 ) ;
#24723 = CARTESIAN_POINT ( 'NONE',  ( 0.1157991065609915715, 29.60440130558512450, 32.71882927116385531 ) ) ;
#24724 = CARTESIAN_POINT ( 'NONE',  ( 0.1119898979215349505, -1.975119484476948628, -44.08015666117655229 ) ) ;
#24725 = VECTOR ( 'NONE', #20006, 1000.000000000000114 ) ;
#24726 = CARTESIAN_POINT ( 'NONE',  ( 0.8560838555295158248, 40.81790744942473737, -23.11430867518922128 ) ) ;
#24727 = CARTESIAN_POINT ( 'NONE',  ( 0.9791128995231621612, -34.54836961549908381, 23.72230155691098474 ) ) ;
#24728 = DIRECTION ( 'NONE',  ( 0.000000000000000000, 0.000000000000000000, 1.000000000000000000 ) ) ;
#24729 =( BOUNDED_SURFACE ( )  B_SPLINE_SURFACE ( 3, 1, ( 
 ( #19557, #23324 ),
 ( #57415, #14554 ),
 ( #56815, #10145 ),
 ( #33655, #52734 ) ),
 .UNSPECIFIED., .F., .F., .F. ) 
 B_SPLINE_SURFACE_WITH_KNOTS ( ( 4, 4 ),
 ( 2, 2 ),
 ( 0.000000000000000000, 1.000000000000000000 ),
 ( 0.000000000000000000, 1.000000000000000000 ),
 .UNSPECIFIED. ) 
 GEOMETRIC_REPRESENTATION_ITEM ( )  RATIONAL_B_SPLINE_SURFACE ( (
 ( 1.000000000000000000, 1.000000000000000000),
 ( 0.9729067724841187204, 0.9999501103223794596),
 ( 0.9729067724841187204, 0.9999501103223794596),
 ( 1.000000000000000000, 1.000000000000000000) ) ) 
 REPRESENTATION_ITEM ( '' )  SURFACE ( )  );
#24730 = EDGE_LOOP ( 'NONE', ( #22319, #42706, #3942, #44333 ) ) ;
#24731 = DIRECTION ( 'NONE',  ( 0.07906939808003037029, 0.6374189498684894595, 0.7664496804329778978 ) ) ;
#24732 = VECTOR ( 'NONE', #38315, 1000.000000000000000 ) ;
#24733 = CARTESIAN_POINT ( 'NONE',  ( 5.896782393890504181, 16.57826022845101122, -11.38803647148056797 ) ) ;
#24734 = CARTESIAN_POINT ( 'NONE',  ( 0.6029443449137434907, -47.49030531303264269, -12.49841747015503834 ) ) ;
#24735 = CARTESIAN_POINT ( 'NONE',  ( 4.549368137175248350, 42.84816078363930814, -2.596185425821480930 ) ) ;
#24736 = CARTESIAN_POINT ( 'NONE',  ( 2.526552050251863246, 39.22765360404650181, 17.56110221699841745 ) ) ;
#24737 = ORIENTED_EDGE ( 'NONE', *, *, #7874, .T. ) ;
#24738 = EDGE_CURVE ( 'NONE', #6825, #23990, #53993, .T. ) ;
#24739 = CARTESIAN_POINT ( 'NONE',  ( 0.9749527285493305717, -37.30179927241191251, 21.20640438431177444 ) ) ;
#24740 = CARTESIAN_POINT ( 'NONE',  ( 0.8557997880470599172, 46.03118133706026072, 13.27832040216655507 ) ) ;
#24741 = EDGE_CURVE ( 'NONE', #42439, #27088, #28128, .T. ) ;
#24742 = FACE_OUTER_BOUND ( 'NONE', #56323, .T. ) ;
#24743 = ORIENTED_EDGE ( 'NONE', *, *, #45679, .T. ) ;
#24744 = FACE_OUTER_BOUND ( 'NONE', #61460, .T. ) ;
#24745 = EDGE_CURVE ( 'NONE', #11136, #462, #47764, .T. ) ;
#24746 = CARTESIAN_POINT ( 'NONE',  ( 0.8551540677456715978, 7.157691013574362771, 47.37911285756622704 ) ) ;
#24747 = ORIENTED_EDGE ( 'NONE', *, *, #59279, .T. ) ;
#24748 = CARTESIAN_POINT ( 'NONE',  ( -6.017396004339687465, 14.94857180791993123, 11.47192209077592295 ) ) ;
#24749 = EDGE_LOOP ( 'NONE', ( #51326, #61157, #59729, #39620 ) ) ;
#24750 = CARTESIAN_POINT ( 'NONE',  ( 0.5809828226811617480, 37.66417181417551774, 29.58751527316192664 ) ) ;
#24751 = ORIENTED_EDGE ( 'NONE', *, *, #57664, .T. ) ;
#24752 = CARTESIAN_POINT ( 'NONE',  ( 5.901764892641288895, 25.34839938110072666, -41.89809203598525045 ) ) ;
#24753 = CARTESIAN_POINT ( 'NONE',  ( 0.5809828226811617480, 23.47450554821709900, 41.74875432577658074 ) ) ;
#24754 = EDGE_LOOP ( 'NONE', ( #41065, #16009, #28994, #3591 ) ) ;
#24755 = CARTESIAN_POINT ( 'NONE',  ( 3.783278058412226308, -39.06943705276843559, 18.05212641201958590 ) ) ;
#24756 = B_SPLINE_CURVE_WITH_KNOTS ( 'NONE', 3,
 ( #22326, #47918, #55824, #38225, #51423, #46768 ),
 .UNSPECIFIED., .F., .F.,
 ( 4, 2, 4 ),
 ( 0.000000000000000000, 0.0002291459268755702077, 0.0004582918537511404154 ),
 .UNSPECIFIED. ) ;
#24757 = ORIENTED_EDGE ( 'NONE', *, *, #30008, .F. ) ;
#24758 = CARTESIAN_POINT ( 'NONE',  ( 4.956653778116991482, -14.93973939759855263, -45.71126949320266419 ) ) ;
#24759 = CARTESIAN_POINT ( 'NONE',  ( 0.6000166863083106206, -45.71468846346260761, 17.94410043432138480 ) ) ;
#24760 = CARTESIAN_POINT ( 'NONE',  ( -6.016761891674564211, -18.20201388312091950, -4.873659902332557081 ) ) ;
#24761 = AXIS2_PLACEMENT_3D ( 'NONE', #35329, #49714, #21212 ) ;
#24762 = EDGE_CURVE ( 'NONE', #51041, #42003, #16064, .T. ) ;
#24763 = ORIENTED_EDGE ( 'NONE', *, *, #3376, .F. ) ;
#24764 = CARTESIAN_POINT ( 'NONE',  ( 5.895881250540457863, 16.57931246612933407, 11.38657454016568416 ) ) ;
#24765 = CARTESIAN_POINT ( 'NONE',  ( 3.727782113643637096, -36.46987195321302977, -24.55048300181119814 ) ) ;
#24766 = B_SPLINE_CURVE_WITH_KNOTS ( 'NONE', 3,
 ( #49142, #6194, #25336, #55674, #3061, #3357 ),
 .UNSPECIFIED., .F., .F.,
 ( 4, 2, 4 ),
 ( 1.738108305489988542E-18, 0.0002291459268755712377, 0.0004582918537511407406 ),
 .UNSPECIFIED. ) ;
#24767 = CARTESIAN_POINT ( 'NONE',  ( 0.5817217712918332229, 32.92749272057849907, -33.39184297316671746 ) ) ;
#24768 = CONICAL_SURFACE ( 'NONE', #37769, 43.92652462719577500, 1.486293639869522343 ) ;
#24769 = CARTESIAN_POINT ( 'NONE',  ( 1.092182651088182688, -18.34815906953977560, -37.68429703737552217 ) ) ;
#24770 = ORIENTED_EDGE ( 'NONE', *, *, #20954, .F. ) ;
#24771 = EDGE_CURVE ( 'NONE', #29203, #37717, #10158, .T. ) ;
#24772 = CARTESIAN_POINT ( 'NONE',  ( 0.6254311100348650676, -13.11433105842173852, 46.28443883864371600 ) ) ;
#24773 = VERTEX_POINT ( 'NONE', #29253 ) ;
#24774 = LINE ( 'NONE', #58885, #36773 ) ;
#24775 = EDGE_CURVE ( 'NONE', #36320, #9573, #12509, .T. ) ;
#24776 = ORIENTED_EDGE ( 'NONE', *, *, #46503, .T. ) ;
#24777 = FACE_OUTER_BOUND ( 'NONE', #30232, .T. ) ;
#24778 = CARTESIAN_POINT ( 'NONE',  ( 0.9789889208857698311, 40.39408608331138595, -11.16479769348274331 ) ) ;
#24779 = ORIENTED_EDGE ( 'NONE', *, *, #37519, .T. ) ;
#24780 = CARTESIAN_POINT ( 'NONE',  ( 0.9762797500689124330, -11.93232144563776487, -40.17392798947692256 ) ) ;
#24781 = CARTESIAN_POINT ( 'NONE',  ( 4.960386119450144626, -40.09630699761674322, 17.51349850330343472 ) ) ;
#24782 = CARTESIAN_POINT ( 'NONE',  ( 0.5809828226811544205, -28.72298383114515374, 38.32755012159135077 ) ) ;
#24783 = DIRECTION ( 'NONE',  ( 0.000000000000000000, 0.000000000000000000, -1.000000000000000000 ) ) ;
#24784 = ORIENTED_EDGE ( 'NONE', *, *, #51062, .T. ) ;
#24785 = CARTESIAN_POINT ( 'NONE',  ( 4.694002226626921015, 42.12595566887518572, 17.42666435179430096 ) ) ;
#24787 = ADVANCED_FACE ( 'NONE', ( #28953 ), #25715, .F. ) ;
#24786 = CARTESIAN_POINT ( 'NONE',  ( 0.9722240741986389878, 33.68410525900284114, 26.58024228478306483 ) ) ;
#24788 = AXIS2_PLACEMENT_3D ( 'NONE', #51500, #4492, #56820 ) ;
#24789 = B_SPLINE_CURVE_WITH_KNOTS ( 'NONE', 3,
 ( #15897, #50315, #21508, #7383 ),
 .UNSPECIFIED., .F., .F.,
 ( 4, 4 ),
 ( 6.254634441385501517E-18, 0.004050076154993002484 ),
 .UNSPECIFIED. ) ;
#24791 = CARTESIAN_POINT ( 'NONE',  ( 0.5832366564991509073, -44.14509737861659033, 18.58038995918336767 ) ) ;
#24790 =( BOUNDED_SURFACE ( )  B_SPLINE_SURFACE ( 3, 1, ( 
 ( #13692, #52184 ),
 ( #14006, #46589 ),
 ( #42822, #3943 ),
 ( #18076, #3631 ) ),
 .UNSPECIFIED., .F., .F., .F. ) 
 B_SPLINE_SURFACE_WITH_KNOTS ( ( 4, 4 ),
 ( 2, 2 ),
 ( 0.000000000000000000, 1.000000000000000000 ),
 ( 0.000000000000000000, 1.000000000000000000 ),
 .UNSPECIFIED. ) 
 GEOMETRIC_REPRESENTATION_ITEM ( )  RATIONAL_B_SPLINE_SURFACE ( (
 ( 1.000000000000000000, 1.000000000000000000),
 ( 0.9751682680413298332, 0.9999560080971552356),
 ( 0.9751682680413298332, 0.9999560080971552356),
 ( 1.000000000000000000, 1.000000000000000000) ) ) 
 REPRESENTATION_ITEM ( '' )  SURFACE ( )  );
#24792 = CARTESIAN_POINT ( 'NONE',  ( 0.8557997880470599172, 46.03118133706026072, 13.27832040216655507 ) ) ;
#24793 = CARTESIAN_POINT ( 'NONE',  ( 3.894904216938898323, -9.202360858324848181, -42.98186695700143645 ) ) ;
#24794 = VECTOR ( 'NONE', #14656, 1000.000000000000114 ) ;
#24795 = CARTESIAN_POINT ( 'NONE',  ( 0.8557997880470690211, 33.22501220301949587, -34.51495345639514767 ) ) ;
#24796 = DIRECTION ( 'NONE',  ( 0.000000000000000000, 0.000000000000000000, 1.000000000000000000 ) ) ;
#24797 = CARTESIAN_POINT ( 'NONE',  ( 0.5807400328401637335, -46.12278621143506285, 12.92266817605998952 ) ) ;
#24798 = CARTESIAN_POINT ( 'NONE',  ( 5.901463166500145796, -4.648441909663419302, -19.56808263865219288 ) ) ;
#24799 = DIRECTION ( 'NONE',  ( 0.000000000000000000, 0.4999999999999990008, -0.8660254037844391517 ) ) ;
#24800 = CARTESIAN_POINT ( 'NONE',  ( -6.016761891674564211, -17.41015286184797262, -7.207804629151495668 ) ) ;
#24801 = CARTESIAN_POINT ( 'NONE',  ( 0.5837799406558246140, -1.475992047555320541, 46.87285991970995980 ) ) ;
#24802 =( BOUNDED_SURFACE ( )  B_SPLINE_SURFACE ( 3, 1, ( 
 ( #17177, #41012 ),
 ( #46015, #50365 ),
 ( #13100, #60674 ),
 ( #27485, #55360 ) ),
 .UNSPECIFIED., .F., .F., .F. ) 
 B_SPLINE_SURFACE_WITH_KNOTS ( ( 4, 4 ),
 ( 2, 2 ),
 ( 0.000000000000000000, 1.000000000000000000 ),
 ( 0.000000000000000000, 1.000000000000000000 ),
 .UNSPECIFIED. ) 
 GEOMETRIC_REPRESENTATION_ITEM ( )  RATIONAL_B_SPLINE_SURFACE ( (
 ( 1.000000000000000000, 1.000000000000000000),
 ( 0.9732289882329797637, 0.9999525324661233672),
 ( 0.9732289882329797637, 0.9999525324661233672),
 ( 1.000000000000000000, 1.000000000000000000) ) ) 
 REPRESENTATION_ITEM ( '' )  SURFACE ( )  );
#24803 = CARTESIAN_POINT ( 'NONE',  ( 0.5806925824938499181, -1.020860314012482561, -46.88475452172953339 ) ) ;
#24804 = CARTESIAN_POINT ( 'NONE',  ( 4.956445790444004018, -47.08764048036452721, 0.5405220916596411573 ) ) ;
#24805 = VERTEX_POINT ( 'NONE', #29871 ) ;
#24806 = CIRCLE ( 'NONE', #22802, 10.00000000000000000 ) ;
#24807 = CARTESIAN_POINT ( 'NONE',  ( 4.549368137175248350, 40.71620287708324781, 13.59764261105765826 ) ) ;
#24808 = CARTESIAN_POINT ( 'NONE',  ( 2.359973842542475442, 19.01300918997274891, -39.70694367707632466 ) ) ;
#24809 = CARTESIAN_POINT ( 'NONE',  ( -6.017396004339686577, -9.420565012089543444, 16.31924478664272371 ) ) ;
#24810 = ORIENTED_EDGE ( 'NONE', *, *, #33673, .T. ) ;
#24811 = EDGE_CURVE ( 'NONE', #58761, #38098, #54578, .T. ) ;
#24812 = LINE ( 'NONE', #43326, #44349 ) ;
#24813 = CARTESIAN_POINT ( 'NONE',  ( 3.727782113643636652, 26.87588261961982994, 34.79173334748344359 ) ) ;
#24814 = ADVANCED_FACE ( 'NONE', ( #40853 ), #8880, .F. ) ;
#24815 = PRODUCT_DEFINITION_CONTEXT ( 'detailed design', #50787, 'design' ) ;
#24816 = EDGE_LOOP ( 'NONE', ( #40498, #1092, #25002, #27736 ) ) ;
#24817 = ORIENTED_EDGE ( 'NONE', *, *, #57754, .T. ) ;
#24818 = CARTESIAN_POINT ( 'NONE',  ( -6.015611763856276717, -13.31979030221789984, -13.32857883366847318 ) ) ;
#24819 = EDGE_CURVE ( 'NONE', #19445, #52485, #53967, .T. ) ;
#24820 = ORIENTED_EDGE ( 'NONE', *, *, #58726, .T. ) ;
#24821 = EDGE_CURVE ( 'NONE', #25537, #15737, #43137, .T. ) ;
#24822 = CARTESIAN_POINT ( 'NONE',  ( 4.549368137175248350, -28.14399996863522446, 32.41327393324091588 ) ) ;
#24823 = AXIS2_PLACEMENT_3D ( 'NONE', #2972, #45926, #17705 ) ;
#24824 = EDGE_CURVE ( 'NONE', #61266, #12288, #17714, .T. ) ;
#24825 = ORIENTED_EDGE ( 'NONE', *, *, #6901, .T. ) ;
#24826 = VERTEX_POINT ( 'NONE', #26100 ) ;
#24827 = CARTESIAN_POINT ( 'NONE',  ( 0.5997462898726536595, -48.76843890605309184, 5.761162800240605897 ) ) ;
#24828 = VERTEX_POINT ( 'NONE', #10785 ) ;
#24829 = CARTESIAN_POINT ( 'NONE',  ( 0.6031357023905875581, -29.32055886552351254, 38.13964912630282811 ) ) ;
#24830 = CARTESIAN_POINT ( 'NONE',  ( 4.999999999999996447, 2.649999999999714362, 80.00000000000002842 ) ) ;
#24831 = B_SPLINE_CURVE_WITH_KNOTS ( 'NONE', 3,
 ( #19596, #33086, #37476, #28058, #38716, #4526, #23363, #42486, #52158, #9248, #12507, #31599, #23667, #42794, #50687, #7779, #3077, #13667, #22205, #41333, #61244, #59012, #16122, #20818, #58690 ),
 .UNSPECIFIED., .F., .F.,
 ( 4, 3, 3, 3, 3, 3, 3, 3, 4 ),
 ( 4.906538933386797396E-18, 0.0005656085177311379053, 0.001131215744874498538, 0.001696821861372765699, 0.002262427090022497284, 0.002828031679238745492, 0.003393635864401604429, 0.003977030878808131623, 0.004561030005651156398 ),
 .UNSPECIFIED. ) ;
#24832 = CARTESIAN_POINT ( 'NONE',  ( -6.017396004339687465, 16.31807101179370179, 9.422598049764681960 ) ) ;
#24833 = VERTEX_POINT ( 'NONE', #50215 ) ;
#24834 = CARTESIAN_POINT ( 'NONE',  ( 0.9754292580325141238, -34.21816593646880733, -24.19596220133207964 ) ) ;
#24835 =( GEOMETRIC_REPRESENTATION_CONTEXT ( 3 ) GLOBAL_UNCERTAINTY_ASSIGNED_CONTEXT ( ( #9788 ) ) GLOBAL_UNIT_ASSIGNED_CONTEXT ( ( #33208, #24404, #47291 ) ) REPRESENTATION_CONTEXT ( 'NONE', 'WORKASPACE' ) );
#24836 = EDGE_CURVE ( 'NONE', #13813, #52796, #1266, .T. ) ;
#24837 = CARTESIAN_POINT ( 'NONE',  ( 1.827119703190779765, 41.24693285842928958, -12.32825544177793731 ) ) ;
#24838 = ORIENTED_EDGE ( 'NONE', *, *, #58733, .T. ) ;
#24839 = ORIENTED_EDGE ( 'NONE', *, *, #23004, .T. ) ;
#24840 = FACE_OUTER_BOUND ( 'NONE', #49980, .T. ) ;
#24841 = DIRECTION ( 'NONE',  ( -1.000000000000000000, -0.000000000000000000, -0.000000000000000000 ) ) ;
#24842 = CARTESIAN_POINT ( 'NONE',  ( 0.7056759521544981872, -14.69874540808407914, 44.53869904414941061 ) ) ;
#24843 = CARTESIAN_POINT ( 'NONE',  ( 0.1097557419366048670, 5.849988371690505673, 42.72583172879055269 ) ) ;
#24844 =( REPRESENTATION_RELATIONSHIP ('NONE','NONE', #44881, #362 ) REPRESENTATION_RELATIONSHIP_WITH_TRANSFORMATION ( #4815 )SHAPE_REPRESENTATION_RELATIONSHIP( ) );
#24845 = VERTEX_POINT ( 'NONE', #44316 ) ;
#24846 = CARTESIAN_POINT ( 'NONE',  ( 0.1149546198390367369, -1.140471116448518840, -44.10947620019723558 ) ) ;
#24847 = CARTESIAN_POINT ( 'NONE',  ( 0.7056759521545005187, 46.58786211884279993, -5.414788298048260451 ) ) ;
#24848 = CYLINDRICAL_SURFACE ( 'NONE', #54469, 6.887500000000022382 ) ;
#24849 = CARTESIAN_POINT ( 'NONE',  ( 4.967162193818130511, 0.000000000000000000, 0.000000000000000000 ) ) ;
#24850 = VERTEX_POINT ( 'NONE', #31109 ) ;
#24851 = CARTESIAN_POINT ( 'NONE',  ( 2.624215991343608501, 40.85210347989531243, 25.21574086439720119 ) ) ;
#24852 = CARTESIAN_POINT ( 'NONE',  ( 4.833616638992205949, 30.83411269743563921, -34.47248434257878813 ) ) ;
#24853 = CARTESIAN_POINT ( 'NONE',  ( 4.967162193818131399, -19.45289607368795259, -38.44485641567092671 ) ) ;
#24854 = CARTESIAN_POINT ( 'NONE',  ( 4.967162193818130511, -32.68434214048149045, -28.07411493385329138 ) ) ;
#24855 = VECTOR ( 'NONE', #30991, 1000.000000000000114 ) ;
#24856 = VECTOR ( 'NONE', #29415, 1000.000000000000000 ) ;
#24857 = VERTEX_POINT ( 'NONE', #6336 ) ;
#24858 = ORIENTED_EDGE ( 'NONE', *, *, #14099, .F. ) ;
#24859 = CARTESIAN_POINT ( 'NONE',  ( 0.5998501479064708430, -46.60114184914326074, 11.94461217097388328 ) ) ;
#24860 = DIRECTION ( 'NONE',  ( -1.000000000000000000, 0.000000000000000000, -0.000000000000000000 ) ) ;
#24861 = CARTESIAN_POINT ( 'NONE',  ( 0.9790320750461888322, 15.14249547772530313, -39.07738429385034351 ) ) ;
#24863 = ADVANCED_FACE ( 'NONE', ( #1343 ), #21686, .F. ) ;
#24862 = DIRECTION ( 'NONE',  ( 0.1011922191286468015, -0.01903003979493037359, 0.9946848708878722745 ) ) ;
#24864 = CARTESIAN_POINT ( 'NONE',  ( 0.1103744047535531458, 34.23648668783393845, -26.22174028894833953 ) ) ;
#24865 = CARTESIAN_POINT ( 'NONE',  ( 0.1154773475650540393, -31.57118803706288190, 30.82537454718983128 ) ) ;
#24866 = CARTESIAN_POINT ( 'NONE',  ( 0.9785694773339257413, 9.931640869912628844, -40.71483655064518103 ) ) ;
#24867 = EDGE_CURVE ( 'NONE', #37278, #17539, #58987, .T. ) ;
#24868 = CARTESIAN_POINT ( 'NONE',  ( 4.960156602257182357, 35.23783291257208106, -30.22163187094351144 ) ) ;
#24869 = FACE_OUTER_BOUND ( 'NONE', #14701, .T. ) ;
#24870 = CARTESIAN_POINT ( 'NONE',  ( 0.9762797500689124330, -0.8945891712298984499, -41.89897964629236782 ) ) ;
#24871 = CARTESIAN_POINT ( 'NONE',  ( 4.303969348037258058, 4.133486515473990153, -47.93217632892343971 ) ) ;
#24872 = ORIENTED_EDGE ( 'NONE', *, *, #30122, .T. ) ;
#24873 = AXIS2_PLACEMENT_3D ( 'NONE', #45584, #59649, #18231 ) ;
#24874 = FACE_OUTER_BOUND ( 'NONE', #49710, .T. ) ;
#24875 = CARTESIAN_POINT ( 'NONE',  ( 3.238741278300274029, -41.96285461600087530, 9.350673766180072732 ) ) ;
#24876 = CARTESIAN_POINT ( 'NONE',  ( 4.549368137175248350, -38.40568845698262379, -19.17571786012310753 ) ) ;
#24877 = DIRECTION ( 'NONE',  ( -0.07906939808003035641, -0.8172634100798066292, 0.5708139353869940980 ) ) ;
#24878 = CARTESIAN_POINT ( 'NONE',  ( 0.1129192098497455998, -42.80154921430131054, 10.72283417016679508 ) ) ;
#24879 = FACE_OUTER_BOUND ( 'NONE', #54377, .T. ) ;
#24880 = DIRECTION ( 'NONE',  ( 0.000000000000000000, 0.000000000000000000, 1.000000000000000000 ) ) ;
#24881 = CARTESIAN_POINT ( 'NONE',  ( 1.827326673878743701, 9.946825761453919057, 41.88502433275007775 ) ) ;
#24882 = AXIS2_PLACEMENT_3D ( 'NONE', #20870, #59063, #54666 ) ;
#24883 = CARTESIAN_POINT ( 'NONE',  ( 0.6008123274975389894, -30.95730127580523217, 38.12086107208866537 ) ) ;
#24885 =( BOUNDED_SURFACE ( )  B_SPLINE_SURFACE ( 3, 1, ( 
 ( #9866, #20200 ),
 ( #33686, #58069 ),
 ( #43402, #39621 ),
 ( #38700, #10173 ) ),
 .UNSPECIFIED., .F., .F., .F. ) 
 B_SPLINE_SURFACE_WITH_KNOTS ( ( 4, 4 ),
 ( 2, 2 ),
 ( 0.000000000000000000, 1.000000000000000000 ),
 ( 0.000000000000000000, 1.000000000000000000 ),
 .UNSPECIFIED. ) 
 GEOMETRIC_REPRESENTATION_ITEM ( )  RATIONAL_B_SPLINE_SURFACE ( (
 ( 1.000000000000000000, 1.000000000000000000),
 ( 0.7282232189291694135, 0.9929344683865672927),
 ( 0.7282232189291694135, 0.9929344683865672927),
 ( 1.000000000000000000, 1.000000000000000000) ) ) 
 REPRESENTATION_ITEM ( '' )  SURFACE ( )  );
#24884 = CARTESIAN_POINT ( 'NONE',  ( 4.963659409799330291, 29.86601237216407156, 33.33129552235096327 ) ) ;
#24886 = CARTESIAN_POINT ( 'NONE',  ( 0.1073791018717578927, 16.05399293000759542, 40.02496097243063389 ) ) ;
#24888 = ORIENTED_EDGE ( 'NONE', *, *, #56856, .T. ) ;
#24887 = CARTESIAN_POINT ( 'NONE',  ( 0.7245667037590748372, -7.091191019330533862, -47.57651946688172018 ) ) ;
#24889 = ORIENTED_EDGE ( 'NONE', *, *, #11307, .F. ) ;
#24890 = CARTESIAN_POINT ( 'NONE',  ( 0.1081432562775998252, -43.12249629849792854, -0.4234896101210040564 ) ) ;
#24891 = CARTESIAN_POINT ( 'NONE',  ( 0.2940135542859018680, -43.84964715722291118, -4.842416016667067780 ) ) ;
#24892 = VECTOR ( 'NONE', #15873, 999.9999999999998863 ) ;
#24893 = CARTESIAN_POINT ( 'NONE',  ( 4.549368137175248350, -35.57418903283131328, 24.02461520945210793 ) ) ;
#24894 = ORIENTED_EDGE ( 'NONE', *, *, #20583, .F. ) ;
#24895 = CARTESIAN_POINT ( 'NONE',  ( 0.7044674535453004927, -2.415488218027067369, -49.05066910328012142 ) ) ;
#24896 = CARTESIAN_POINT ( 'NONE',  ( -6.077587904424778920, -4.290907484552348272, 18.77189746277512583 ) ) ;
#24897 = CARTESIAN_POINT ( 'NONE',  ( 5.960721111146673579, 7.860635756377621242, 18.96073515164551537 ) ) ;
#24898 = B_SPLINE_CURVE_WITH_KNOTS ( 'NONE', 3,
 ( #25268, #19978, #35299, #40022 ),
 .UNSPECIFIED., .F., .F.,
 ( 4, 4 ),
 ( 0.000000000000000000, 0.004442905043737216571 ),
 .UNSPECIFIED. ) ;
#24899 = EDGE_CURVE ( 'NONE', #36963, #59719, #1969, .T. ) ;
#24900 = B_SPLINE_CURVE_WITH_KNOTS ( 'NONE', 3,
 ( #8453, #46710, #23193, #50761 ),
 .UNSPECIFIED., .F., .F.,
 ( 4, 4 ),
 ( 0.000000000000000000, 0.004446090762761377262 ),
 .UNSPECIFIED. ) ;
#24901 = ORIENTED_EDGE ( 'NONE', *, *, #14049, .F. ) ;
#24902 = ORIENTED_EDGE ( 'NONE', *, *, #8681, .T. ) ;
#24903 = CARTESIAN_POINT ( 'NONE',  ( 0.6001305935487422083, 46.33281397023063874, -12.95698906763762537 ) ) ;
#24904 = ADVANCED_FACE ( 'NONE', ( #60215 ), #28093, .F. ) ;
#24905 = CARTESIAN_POINT ( 'NONE',  ( 1.157643937452367933, 33.40146143681677415, 25.32478328593544958 ) ) ;
#24906 = AXIS2_PLACEMENT_3D ( 'NONE', #61450, #27347, #32676 ) ;
#24907 = EDGE_CURVE ( 'NONE', #19440, #35096, #47558, .T. ) ;
#24908 =( BOUNDED_SURFACE ( )  B_SPLINE_SURFACE ( 3, 1, ( 
 ( #55666, #50973 ),
 ( #8070, #35680 ),
 ( #27180, #54740 ),
 ( #49747, #6809 ) ),
 .UNSPECIFIED., .F., .F., .F. ) 
 B_SPLINE_SURFACE_WITH_KNOTS ( ( 4, 4 ),
 ( 2, 2 ),
 ( 0.000000000000000000, 1.000000000000000000 ),
 ( 0.000000000000000000, 1.000000000000000000 ),
 .UNSPECIFIED. ) 
 GEOMETRIC_REPRESENTATION_ITEM ( )  RATIONAL_B_SPLINE_SURFACE ( (
 ( 1.000000000000000000, 1.000000000000000000),
 ( 0.9953390228620291325, 0.8624445117761032620),
 ( 0.9953390228620291325, 0.8624445117761032620),
 ( 1.000000000000000000, 1.000000000000000000) ) ) 
 REPRESENTATION_ITEM ( '' )  SURFACE ( )  );
#24909 = CIRCLE ( 'NONE', #40942, 5.000000000000000000 ) ;
#24910 = CARTESIAN_POINT ( 'NONE',  ( -4.000000000000000000, 0.000000000000000000, 0.000000000000000000 ) ) ;
#24911 = CARTESIAN_POINT ( 'NONE',  ( 1.092182651088185796, -41.22225533107799578, -7.582008300028149073 ) ) ;
#24912 = CARTESIAN_POINT ( 'NONE',  ( 0.7413678028165010536, -11.64920183752063387, 42.52978001728846635 ) ) ;
#24913 = EDGE_CURVE ( 'NONE', #44423, #25842, #60834, .T. ) ;
#24914 =( BOUNDED_SURFACE ( )  B_SPLINE_SURFACE ( 3, 1, ( 
 ( #61707, #1167 ),
 ( #4081, #23221 ),
 ( #20605, #56712 ),
 ( #52322, #58477 ) ),
 .UNSPECIFIED., .F., .F., .F. ) 
 B_SPLINE_SURFACE_WITH_KNOTS ( ( 4, 4 ),
 ( 2, 2 ),
 ( 0.000000000000000000, 1.000000000000000000 ),
 ( 0.000000000000000000, 1.000000000000000000 ),
 .UNSPECIFIED. ) 
 GEOMETRIC_REPRESENTATION_ITEM ( )  RATIONAL_B_SPLINE_SURFACE ( (
 ( 1.000000000000000000, 1.000000000000000000),
 ( 0.7269869731126821222, 0.9931720237060910339),
 ( 0.7269869731126821222, 0.9931720237060910339),
 ( 1.000000000000000000, 1.000000000000000000) ) ) 
 REPRESENTATION_ITEM ( '' )  SURFACE ( )  );
#24915 = CARTESIAN_POINT ( 'NONE',  ( 0.2285344041767097267, 4.992133951191583208, 43.83582745778637246 ) ) ;
#24916 = CARTESIAN_POINT ( 'NONE',  ( 5.000000000000012434, -80.00000000000001421, -1.569632904675596344E-31 ) ) ;
#24917 = CARTESIAN_POINT ( 'NONE',  ( 4.549368137175248350, -24.02461520945298545, 35.57418903283073064 ) ) ;
#24918 = ORIENTED_EDGE ( 'NONE', *, *, #31598, .T. ) ;
#24919 = ORIENTED_EDGE ( 'NONE', *, *, #49010, .F. ) ;
#24920 = CARTESIAN_POINT ( 'NONE',  ( 1.092182651088182688, -30.55625471937437965, 28.68930954148243728 ) ) ;
#24921 = CARTESIAN_POINT ( 'NONE',  ( 2.281448460670567169, 19.56578495220171021, 43.80196084514285815 ) ) ;
#24922 = VECTOR ( 'NONE', #38683, 1000.000000000000000 ) ;
#24923 = ORIENTED_EDGE ( 'NONE', *, *, #4675, .F. ) ;
#24924 = CARTESIAN_POINT ( 'NONE',  ( 4.963659409799330291, -29.86601237216385485, -33.33129552235118354 ) ) ;
#24925 = CARTESIAN_POINT ( 'NONE',  ( 3.678834586032787346, -21.50130846795401851, 44.00347831472237914 ) ) ;
#24926 = CARTESIAN_POINT ( 'NONE',  ( 2.528100132419516477, -8.172757371798878623, -41.17596162293945383 ) ) ;
#24927 = ORIENTED_EDGE ( 'NONE', *, *, #49432, .T. ) ;
#24928 = CARTESIAN_POINT ( 'NONE',  ( 0.5817217712918341110, 46.53606702067560974, -5.799087881344962447 ) ) ;
#24929 = CARTESIAN_POINT ( 'NONE',  ( 0.6845945791218034371, -2.432797934429833830, 46.84536278997290282 ) ) ;
#24930 = CARTESIAN_POINT ( 'NONE',  ( 0.1103744047535531458, -37.32746539760805149, -21.59576373962403650 ) ) ;
#24931 = CARTESIAN_POINT ( 'NONE',  ( 0.5809828226811553087, -0.5448590168529036104, -47.89273459658654275 ) ) ;
#24932 = CARTESIAN_POINT ( 'NONE',  ( 4.303969348037258058, 40.54345935592815664, -25.89994482339327320 ) ) ;
#24933 = ORIENTED_EDGE ( 'NONE', *, *, #30200, .F. ) ;
#24934 = CARTESIAN_POINT ( 'NONE',  ( 0.5807400328401574052, -47.89582301953902999, -0.5448834511094979849 ) ) ;
#24935 = ORIENTED_EDGE ( 'NONE', *, *, #36296, .F. ) ;
#24936 = CARTESIAN_POINT ( 'NONE',  ( 0.7764139734771232648, -44.00885462842416729, -16.22532542666233013 ) ) ;
#24937 = CARTESIAN_POINT ( 'NONE',  ( 0.5836750258453350382, 24.10509086647810051, -41.38803015411981789 ) ) ;
#24938 = VERTEX_POINT ( 'NONE', #55831 ) ;
#24939 = CARTESIAN_POINT ( 'NONE',  ( -6.016761891674564211, -4.873659902332494909, 18.20201388312094082 ) ) ;
#24940 = CARTESIAN_POINT ( 'NONE',  ( -6.015611763856276717, 16.32183393015596451, 9.416239407363361735 ) ) ;
#24941 = CARTESIAN_POINT ( 'NONE',  ( 4.553261556744873317, 12.28162544311275006, -42.17465165592624032 ) ) ;
#24942 = CARTESIAN_POINT ( 'NONE',  ( 0.6023143664670691511, -41.79259346737339342, 23.82663958122363823 ) ) ;
#24943 = CARTESIAN_POINT ( 'NONE',  ( 0.1158516988532803521, 33.56623812058064971, -28.64000379303876187 ) ) ;
#24944 = CARTESIAN_POINT ( 'NONE',  ( 0.7056313189692692278, 45.45044948170761501, 11.57606521527523391 ) ) ;
#24945 = CARTESIAN_POINT ( 'NONE',  ( 0.2885700199627517781, -20.85752789928088191, 37.73587457854630856 ) ) ;
#24947 = EDGE_CURVE ( 'NONE', #4970, #7001, #6457, .T. ) ;
#24946 = B_SPLINE_CURVE_WITH_KNOTS ( 'NONE', 3,
 ( #55202, #16705, #45847, #21705 ),
 .UNSPECIFIED., .F., .F.,
 ( 4, 4 ),
 ( 0.000000000000000000, 0.004041751736740989073 ),
 .UNSPECIFIED. ) ;
#24948 = DIRECTION ( 'NONE',  ( 0.000000000000000000, 1.000000000000000000, -1.224646799147353207E-16 ) ) ;
#24949 = VERTEX_POINT ( 'NONE', #37370 ) ;
#24950 = CARTESIAN_POINT ( 'NONE',  ( 5.901463166500145796, -20.11262442202718148, -0.01446371710611837197 ) ) ;
#24951 = CARTESIAN_POINT ( 'NONE',  ( 0.9789889208857702751, 41.54742805390438321, 5.490548255685043344 ) ) ;
#24952 = CARTESIAN_POINT ( 'NONE',  ( 1.479689385636123067, -16.75487965742231111, 40.75362380123991102 ) ) ;
#24953 = ORIENTED_EDGE ( 'NONE', *, *, #54801, .F. ) ;
#24954 = CARTESIAN_POINT ( 'NONE',  ( 5.960221823109900008, 2.684531185214417803, -20.34928172836727711 ) ) ;
#24955 = CARTESIAN_POINT ( 'NONE',  ( 5.272380000000000067, 0.000000000000000000, 12.49999999999999822 ) ) ;
#24956 = CARTESIAN_POINT ( 'NONE',  ( 0.7242003506639981270, 10.12622957855171357, -48.04655189135312554 ) ) ;
#24957 = CARTESIAN_POINT ( 'NONE',  ( 0.8751705887134553219, -34.63284514348562482, -33.37254303619542384 ) ) ;
#24958 = CARTESIAN_POINT ( 'NONE',  ( -6.016761891674565099, -17.40752468084777504, -7.214149619366543753 ) ) ;
#24959 = CARTESIAN_POINT ( 'NONE',  ( 0.5998501479064708430, 38.48283596222029956, -28.86886762351084812 ) ) ;
#24960 = CARTESIAN_POINT ( 'NONE',  ( -1.599999999999950795, -2.705576974306825009E-13, 80.00000000000001421 ) ) ;
#24961 = CARTESIAN_POINT ( 'NONE',  ( 0.1073791018717483448, -41.77800844988507123, -10.69234304550039383 ) ) ;
#24962 = CARTESIAN_POINT ( 'NONE',  ( 1.154321713695927176, 29.75729669971110880, 30.92445811446658510 ) ) ;
#24963 = B_SPLINE_CURVE_WITH_KNOTS ( 'NONE', 3,
 ( #50560, #51473, #32093, #41501, #3551, #61187, #60565, #18307, #13605, #32711, #51793, #31783, #7636, #8892, #46823, #37416 ),
 .UNSPECIFIED., .F., .F.,
 ( 4, 3, 3, 3, 3, 4 ),
 ( 9.813676791237319219E-18, 0.0002732102107931875601, 0.0004098135523333743240, 0.0005464168938824992506, 0.0008195847345945445278, 0.001092771384553111553 ),
 .UNSPECIFIED. ) ;
#24964 = CARTESIAN_POINT ( 'NONE',  ( 4.963659409799330291, -29.14784479683089558, -33.96111158240276495 ) ) ;
#24966 = VERTEX_POINT ( 'NONE', #22331 ) ;
#24965 = CARTESIAN_POINT ( 'NONE',  ( -6.010958268070873523, -7.197664668556567946, 17.41463273278775858 ) ) ;
#24967 = ORIENTED_EDGE ( 'NONE', *, *, #23972, .F. ) ;
#24969 = AXIS2_PLACEMENT_3D ( 'NONE', #57637, #323, #958 ) ;
#24968 = FACE_OUTER_BOUND ( 'NONE', #27451, .T. ) ;
#24970 = CARTESIAN_POINT ( 'NONE',  ( 0.8551540677456834771, 33.23105123575948028, -34.52115452272894203 ) ) ;
#24971 = CARTESIAN_POINT ( 'NONE',  ( 5.959547316686252039, -16.28190225198610008, -12.49803383497744136 ) ) ;
#24972 = CARTESIAN_POINT ( 'NONE',  ( 0.1129192098497455998, -23.28677643606931014, 37.47903188453085477 ) ) ;
#24973 = CARTESIAN_POINT ( 'NONE',  ( -2.569797478183783568, -6.924386868080936175, 12.89088113963424043 ) ) ;
#24974 = CARTESIAN_POINT ( 'NONE',  ( 0.1157506346131639274, 9.728079385241393595, -43.03841459995100394 ) ) ;
#24975 = ADVANCED_FACE ( 'NONE', ( #41459 ), #38539, .F. ) ;
#24976 = ORIENTED_EDGE ( 'NONE', *, *, #44411, .F. ) ;
#24977 = ORIENTED_EDGE ( 'NONE', *, *, #61263, .T. ) ;
#24978 = EDGE_CURVE ( 'NONE', #18352, #33579, #54291, .T. ) ;
#24979 = CARTESIAN_POINT ( 'NONE',  ( 5.894904586330512508, 5.960138742492036457, 19.20953300400320174 ) ) ;
#24980 = LINE ( 'NONE', #44118, #25207 ) ;
#24981 = DIRECTION ( 'NONE',  ( -0.1011922191286467460, -0.5796805626819985235, 0.8085360721925158867 ) ) ;
#24982 = VERTEX_POINT ( 'NONE', #3820 ) ;
#24983 = ADVANCED_FACE ( 'NONE', ( #22956 ), #34508, .F. ) ;
#24984 = DIRECTION ( 'NONE',  ( -0.9990097760809875105, 0.000000000000000000, 0.04449120468828677427 ) ) ;
#24985 = CARTESIAN_POINT ( 'NONE',  ( 0.5827357941260212781, 47.43746130990125920, -6.611647889510720688 ) ) ;
#24986 =( BOUNDED_SURFACE ( )  B_SPLINE_SURFACE ( 3, 1, ( 
 ( #3961, #51275 ),
 ( #60355, #50660 ),
 ( #27176, #46300 ),
 ( #41600, #60984 ) ),
 .UNSPECIFIED., .F., .F., .F. ) 
 B_SPLINE_SURFACE_WITH_KNOTS ( ( 4, 4 ),
 ( 2, 2 ),
 ( 0.000000000000000000, 1.000000000000000000 ),
 ( 0.000000000000000000, 1.000000000000000000 ),
 .UNSPECIFIED. ) 
 GEOMETRIC_REPRESENTATION_ITEM ( )  RATIONAL_B_SPLINE_SURFACE ( (
 ( 1.000000000000000000, 1.000000000000000000),
 ( 0.7223157951917476005, 0.9931996967497186413),
 ( 0.7223157951917476005, 0.9931996967497186413),
 ( 1.000000000000000000, 1.000000000000000000) ) ) 
 REPRESENTATION_ITEM ( '' )  SURFACE ( )  );
#24987 = VERTEX_POINT ( 'NONE', #22643 ) ;
#24988 = CARTESIAN_POINT ( 'NONE',  ( 4.975610109902397937, -48.11736577406850301, -8.784561349451310619 ) ) ;
#24989 = ORIENTED_EDGE ( 'NONE', *, *, #48374, .F. ) ;
#24990 = CARTESIAN_POINT ( 'NONE',  ( 0.5832655196449132440, -34.93280808371936530, 31.28792262773866995 ) ) ;
#24991 = EDGE_CURVE ( 'NONE', #19627, #25537, #55208, .T. ) ;
#24993 = CARTESIAN_POINT ( 'NONE',  ( 0.6017667736363750963, 33.76945004754868762, 34.26315558341202205 ) ) ;
#24992 = AXIS2_PLACEMENT_3D ( 'NONE', #9640, #15593, #29363 ) ;
#24994 = ORIENTED_EDGE ( 'NONE', *, *, #14871, .F. ) ;
#24995 = CARTESIAN_POINT ( 'NONE',  ( 4.956445790444004018, -45.27177431812773278, -12.96165499572285817 ) ) ;
#24996 = CARTESIAN_POINT ( 'NONE',  ( 5.910764540655178756, -20.11221018249587544, 0.01549336220059224084 ) ) ;
#24997 = CARTESIAN_POINT ( 'NONE',  ( 0.9790320750461896093, 40.39682900182685898, 11.15496925766059633 ) ) ;
#24998 = CARTESIAN_POINT ( 'NONE',  ( 3.660087539127327982, -47.34518630204117073, 8.130906407639885813 ) ) ;
#24999 = EDGE_CURVE ( 'NONE', #59028, #49007, #36758, .T. ) ;
#25000 = ORIENTED_EDGE ( 'NONE', *, *, #34459, .F. ) ;
#25001 = FACE_OUTER_BOUND ( 'NONE', #32820, .T. ) ;
#25002 = ORIENTED_EDGE ( 'NONE', *, *, #59231, .T. ) ;
#25003 = CARTESIAN_POINT ( 'NONE',  ( 1.827119703190780653, -34.89020442382241072, -25.21842556008173375 ) ) ;
#25004 = ORIENTED_EDGE ( 'NONE', *, *, #52828, .T. ) ;
#25005 = CARTESIAN_POINT ( 'NONE',  ( 5.901764892641307547, -48.05798712428978092, -9.403262253137295801 ) ) ;
#25006 = ORIENTED_EDGE ( 'NONE', *, *, #51608, .T. ) ;
#25007 = CARTESIAN_POINT ( 'NONE',  ( 0.6008123274975393224, -48.64681338165629398, -6.711341070811670306 ) ) ;
#25008 = VECTOR ( 'NONE', #57896, 1000.000000000000114 ) ;
#25009 = CARTESIAN_POINT ( 'NONE',  ( 0.9749527285493315709, 33.86694354778357052, 26.34702925571509624 ) ) ;
#25010 = ORIENTED_EDGE ( 'NONE', *, *, #14362, .F. ) ;
#25011 = CARTESIAN_POINT ( 'NONE',  ( -6.016761891674565099, 7.214149619366596156, -17.40752468084775373 ) ) ;
#25012 = CARTESIAN_POINT ( 'NONE',  ( 0.5809828226811556418, -5.711058609465654357, 47.55412398569204413 ) ) ;
#25013 = CARTESIAN_POINT ( 'NONE',  ( -6.010958268070873523, -14.94067681728541963, -11.48268200989212495 ) ) ;
#25014 = VERTEX_POINT ( 'NONE', #3506 ) ;
#25015 = ORIENTED_EDGE ( 'NONE', *, *, #34129, .F. ) ;
#25016 = CARTESIAN_POINT ( 'NONE',  ( 0.9769922540276034795, -30.78348955484764460, -28.43779748701913235 ) ) ;
#25017 = CARTESIAN_POINT ( 'NONE',  ( 4.335381028904216727, 47.63237751920352991, -11.44174197980444774 ) ) ;
#25018 = CARTESIAN_POINT ( 'NONE',  ( 0.1119899015040013296, 24.78191846902677398, 36.50777759857500371 ) ) ;
#25019 = DIRECTION ( 'NONE',  ( 0.000000000000000000, 0.000000000000000000, 1.000000000000000000 ) ) ;
#25020 = EDGE_CURVE ( 'NONE', #36409, #58875, #8521, .T. ) ;
#25021 = CARTESIAN_POINT ( 'NONE',  ( 0.9780303403264768436, -27.30392181875063784, -31.79363877744474820 ) ) ;
#25022 = CARTESIAN_POINT ( 'NONE',  ( 0.7948884756798498818, -45.82899951237259728, 17.61821353869637008 ) ) ;
#25023 = ORIENTED_EDGE ( 'NONE', *, *, #4051, .F. ) ;
#25024 = CARTESIAN_POINT ( 'NONE',  ( 4.956445790443988031, 0.000000000000000000, 0.000000000000000000 ) ) ;
#25025 = VERTEX_POINT ( 'NONE', #47369 ) ;
#25026 = CARTESIAN_POINT ( 'NONE',  ( 0.8560838555295158248, -8.701885300216421371, 46.09392613244839509 ) ) ;
#25027 = CARTESIAN_POINT ( 'NONE',  ( 3.531697314441601065, 0.2975892744534772150, 47.02729111494448944 ) ) ;
#25028 = CARTESIAN_POINT ( 'NONE',  ( 0.8753041380234530822, 41.63161868429038037, 26.03740873433499203 ) ) ;
#25029 = CARTESIAN_POINT ( 'NONE',  ( 5.959547316686252039, -18.96183906913549322, 7.858107265727413804 ) ) ;
#25030 = CARTESIAN_POINT ( 'NONE',  ( 0.8753041380234465318, -48.57841546934875510, -7.160717726619147072 ) ) ;
#25031 = FILL_AREA_STYLE_COLOUR ( '', #58843 ) ;
#25032 = LINE ( 'NONE', #58514, #5657 ) ;
#25033 = CARTESIAN_POINT ( 'NONE',  ( 1.827119703190779765, 22.58367210012840687, 36.65069040194717331 ) ) ;
#25034 = CARTESIAN_POINT ( 'NONE',  ( 0.8744876279028263033, -47.70753782033983725, 11.59055156152357213 ) ) ;
#25035 = CARTESIAN_POINT ( 'NONE',  ( -2.681483223904239210, 3.070647092368425479, 2.604296331179000749E-15 ) ) ;
#25036 = LINE ( 'NONE', #19727, #40267 ) ;
#25037 = CARTESIAN_POINT ( 'NONE',  ( 1.657374760986086049, -18.95778414414311541, -39.76798797520839912 ) ) ;
#25038 = CARTESIAN_POINT ( 'NONE',  ( 5.896782393890504181, 3.351618377817072947, 19.83160964539921167 ) ) ;
#25039 = ORIENTED_EDGE ( 'NONE', *, *, #48770, .F. ) ;
#25040 = EDGE_CURVE ( 'NONE', #39239, #54529, #18491, .T. ) ;
#25041 = CARTESIAN_POINT ( 'NONE',  ( 1.830465331921977912, 24.17895171870296878, 36.82056965424381190 ) ) ;
#25042 = VECTOR ( 'NONE', #55448, 1000.000000000000000 ) ;
#25043 = CARTESIAN_POINT ( 'NONE',  ( 0.5834872094924155039, 18.53852119651626396, -44.16273175734626477 ) ) ;
#25044 = CARTESIAN_POINT ( 'NONE',  ( 3.390910168358337362, 40.43814545685926021, 17.28738061545269744 ) ) ;
#25045 = CARTESIAN_POINT ( 'NONE',  ( 0.2940133293163010308, 5.036457840397877916, -43.82778390473260544 ) ) ;
#25046 = ORIENTED_EDGE ( 'NONE', *, *, #20152, .T. ) ;
#25047 = ADVANCED_FACE ( 'NONE', ( #665 ), #60098, .F. ) ;
#25048 = CARTESIAN_POINT ( 'NONE',  ( 0.9756950546413950542, -37.11135009583540523, 21.53795086961250149 ) ) ;
#25049 = CARTESIAN_POINT ( 'NONE',  ( 0.9745511491811745808, 16.73445648040624789, -39.51062171155243874 ) ) ;
#25050 = ADVANCED_FACE ( 'NONE', ( #42686 ), #4455, .F. ) ;
#25051 = FACE_OUTER_BOUND ( 'NONE', #51644, .T. ) ;
#25052 = ORIENTED_EDGE ( 'NONE', *, *, #10970, .F. ) ;
#25053 = CARTESIAN_POINT ( 'NONE',  ( 0.6001305935487315502, 47.76436356026960084, 5.760103278698184504 ) ) ;
#25054 = CARTESIAN_POINT ( 'NONE',  ( 1.227938101723748288, -41.23019537246701560, -11.92353943227992197 ) ) ;
#25055 = ORIENTED_EDGE ( 'NONE', *, *, #41062, .T. ) ;
#25056 = ORIENTED_EDGE ( 'NONE', *, *, #59059, .T. ) ;
#25057 = CARTESIAN_POINT ( 'NONE',  ( 0.6254311100348660668, -46.64066536338349778, 11.78487556908926770 ) ) ;
#25058 = ORIENTED_EDGE ( 'NONE', *, *, #43345, .T. ) ;
#25059 = CARTESIAN_POINT ( 'NONE',  ( 0.1158516988532803244, 29.62825737391777281, -32.69722501708185547 ) ) ;
#25060 = CARTESIAN_POINT ( 'NONE',  ( 0.5988103564986354543, 41.35593036885933316, -24.57719524907199826 ) ) ;
#25061 = ORIENTED_EDGE ( 'NONE', *, *, #51218, .T. ) ;
#25062 = CARTESIAN_POINT ( 'NONE',  ( 5.896278296736517710, 8.471169747519724069, -18.24188210473607441 ) ) ;
#25063 = EDGE_CURVE ( 'NONE', #10591, #56576, #58725, .T. ) ;
#25064 = ORIENTED_EDGE ( 'NONE', *, *, #26805, .F. ) ;
#25065 = CARTESIAN_POINT ( 'NONE',  ( 0.2230388203127593172, -41.44703429209694434, 11.89247826311202516 ) ) ;
#25066 = CARTESIAN_POINT ( 'NONE',  ( 0.1147471544378676767, -1.103879636312829815, 44.11047084561418785 ) ) ;
#25067 = VECTOR ( 'NONE', #51150, 1000.000000000000114 ) ;
#25068 = ORIENTED_EDGE ( 'NONE', *, *, #13457, .T. ) ;
#25069 = CARTESIAN_POINT ( 'NONE',  ( 4.963659409799328515, -39.92545197189537021, -20.22157859941772529 ) ) ;
#25070 = CARTESIAN_POINT ( 'NONE',  ( 3.894904216938898323, -36.51224477628893794, -24.47407432105578806 ) ) ;
#25071 = LINE ( 'NONE', #54476, #14281 ) ;
#25072 = CARTESIAN_POINT ( 'NONE',  ( 5.331199999999999939, 1.538011871406776419E-15, -12.55882000000000076 ) ) ;
#25073 = EDGE_LOOP ( 'NONE', ( #18214, #4383, #15126, #39096 ) ) ;
#25074 = CARTESIAN_POINT ( 'NONE',  ( 0.6001305935487422083, -46.60388846085714931, -11.94532529598361670 ) ) ;
#25075 = ORIENTED_EDGE ( 'NONE', *, *, #37937, .T. ) ;
#25076 = CARTESIAN_POINT ( 'NONE',  ( 0.5834584762367742705, -46.77877185694124051, -3.313984394868909611 ) ) ;
#25077 = ORIENTED_EDGE ( 'NONE', *, *, #35199, .F. ) ;
#25078 = CIRCLE ( 'NONE', #23079, 48.09070567114147110 ) ;
#25079 = CARTESIAN_POINT ( 'NONE',  ( 0.8751705887134553219, -7.160166390003972481, -47.55935879196468363 ) ) ;
#25080 = CARTESIAN_POINT ( 'NONE',  ( 5.960221823109900008, 0.005450390361721958211, -20.52559243573973546 ) ) ;
#25081 = ORIENTED_EDGE ( 'NONE', *, *, #58983, .F. ) ;
#25082 = CARTESIAN_POINT ( 'NONE',  ( 0.5980894510889448457, 13.12879507229288478, -46.28687279963680368 ) ) ;
#25083 = CARTESIAN_POINT ( 'NONE',  ( 2.301430502907644282, -46.04685681264155050, -13.67112791032026919 ) ) ;
#25084 = CARTESIAN_POINT ( 'NONE',  ( 52.11715515643994223, 12.32162532810768241, 2.106428410961948217 ) ) ;
#25085 = CARTESIAN_POINT ( 'NONE',  ( 0.3622758884714730732, 17.25816669464937902, 39.50828911767005280 ) ) ;
#25086 = ORIENTED_EDGE ( 'NONE', *, *, #23062, .T. ) ;
#25087 = CARTESIAN_POINT ( 'NONE',  ( 0.6031357023905875581, 18.45021748202282552, -44.42879114414639474 ) ) ;
#25088 = EDGE_CURVE ( 'NONE', #22556, #17976, #7938, .T. ) ;
#25089 = CARTESIAN_POINT ( 'NONE',  ( 0.9789233960466707796, 41.55206370043617170, -5.455522804208261967 ) ) ;
#25090 = B_SPLINE_CURVE_WITH_KNOTS ( 'NONE', 3,
 ( #36248, #27137, #50617, #3007 ),
 .UNSPECIFIED., .F., .F.,
 ( 4, 4 ),
 ( 0.000000000000000000, 0.004446090762761357312 ),
 .UNSPECIFIED. ) ;
#25091 = ADVANCED_FACE ( 'NONE', ( #1901 ), #17305, .F. ) ;
#25092 = LINE ( 'NONE', #54738, #29912 ) ;
#25093 = PRESENTATION_STYLE_ASSIGNMENT (( #31341 ) ) ;
#25094 = CARTESIAN_POINT ( 'NONE',  ( 0.7057020205115043243, 46.04437542275044137, 13.20843872046504330 ) ) ;
#25095 =( BOUNDED_SURFACE ( )  B_SPLINE_SURFACE ( 3, 1, ( 
 ( #44982, #25225 ),
 ( #39350, #30227 ),
 ( #1704, #44368 ),
 ( #20843, #44071 ) ),
 .UNSPECIFIED., .F., .F., .F. ) 
 B_SPLINE_SURFACE_WITH_KNOTS ( ( 4, 4 ),
 ( 2, 2 ),
 ( 0.000000000000000000, 1.000000000000000000 ),
 ( 0.000000000000000000, 1.000000000000000000 ),
 .UNSPECIFIED. ) 
 GEOMETRIC_REPRESENTATION_ITEM ( )  RATIONAL_B_SPLINE_SURFACE ( (
 ( 1.000000000000000000, 1.000000000000000000),
 ( 0.9732289882329797637, 0.9999525324661233672),
 ( 0.9732289882329797637, 0.9999525324661233672),
 ( 1.000000000000000000, 1.000000000000000000) ) ) 
 REPRESENTATION_ITEM ( '' )  SURFACE ( )  );
#25096 = CARTESIAN_POINT ( 'NONE',  ( 2.533389852662419894, -8.582510520014036359, -43.17164630758787069 ) ) ;
#25097 = EDGE_CURVE ( 'NONE', #35307, #58937, #42357, .T. ) ;
#25098 = CARTESIAN_POINT ( 'NONE',  ( 0.8551540677456715978, 41.94570365541235901, -23.16399837394502015 ) ) ;
#25099 = CARTESIAN_POINT ( 'NONE',  ( -15.88746099330916373, -7.996356313915863545, -0.2766558318553649642 ) ) ;
#25100 = CARTESIAN_POINT ( 'NONE',  ( 7.999999999999996447, 1.469527624586858429E-15, -1.540743955509788245E-31 ) ) ;
#25101 = CARTESIAN_POINT ( 'NONE',  ( -6.078726893082806448, -12.94836301907731801, -14.25250631976393656 ) ) ;
#25102 = B_SPLINE_CURVE_WITH_KNOTS ( 'NONE', 3,
 ( #57889, #61965, #4333, #19103, #38216, #43219, #254, #15016, #44163, #45078, #59127, #39762, #16238, #30017, #35053, #11541, #44465, #43848, #25318 ),
 .UNSPECIFIED., .F., .F.,
 ( 4, 3, 3, 3, 3, 3, 4 ),
 ( 1.250973872328959318E-17, 0.0002732106629380585830, 0.0004098138914053691979, 0.0005464171197651370403, 0.0006830203481512451408, 0.0008196235766963510562, 0.001011968216111142896 ),
 .UNSPECIFIED. ) ;
#25103 = CARTESIAN_POINT ( 'NONE',  ( 0.1139756605157205005, -43.81112104903924376, -5.247941703320747386 ) ) ;
#25104 = CARTESIAN_POINT ( 'NONE',  ( 1.231276596079881047, 38.25526645152027072, 17.14092645516147684 ) ) ;
#25105 = CARTESIAN_POINT ( 'NONE',  ( 0.8551540677456715978, -28.44084013485092655, -38.56334384152460615 ) ) ;
#25106 = ADVANCED_FACE ( 'NONE', ( #5960 ), #42934, .F. ) ;
#25107 = DIRECTION ( 'NONE',  ( 1.000000000000000000, 1.836909530733573776E-16, 0.000000000000000000 ) ) ;
#25108 = CARTESIAN_POINT ( 'NONE',  ( 0.1129192098497455998, 36.71339784380029414, 24.47607416535571545 ) ) ;
#25109 = ORIENTED_EDGE ( 'NONE', *, *, #35672, .T. ) ;
#25110 = FACE_OUTER_BOUND ( 'NONE', #41644, .T. ) ;
#25111 = CARTESIAN_POINT ( 'NONE',  ( 2.282816707992312288, -35.70555677707368858, -30.52228991486604670 ) ) ;
#25112 = CARTESIAN_POINT ( 'NONE',  ( -6.016761891674565099, -9.424569481870369358, 16.31696541414269319 ) ) ;
#25113 = VERTEX_POINT ( 'NONE', #58587 ) ;
#25114 = EDGE_CURVE ( 'NONE', #9246, #58767, #40467, .T. ) ;
#25115 = DIRECTION ( 'NONE',  ( 0.000000000000000000, 0.7071067811865382469, 0.7071067811865566766 ) ) ;
#25116 = DIRECTION ( 'NONE',  ( -0.07906939808003034253, 0.9868658484044072754, -0.1408681210931379824 ) ) ;
#25117 = EDGE_CURVE ( 'NONE', #47332, #17815, #489, .T. ) ;
#25119 = VERTEX_POINT ( 'NONE', #26337 ) ;
#25118 = AXIS2_PLACEMENT_3D ( 'NONE', #979, #14793, #47684 ) ;
#25120 = ORIENTED_EDGE ( 'NONE', *, *, #634, .T. ) ;
#25121 = CARTESIAN_POINT ( 'NONE',  ( 0.8760168074887090262, -13.30888447662048435, -46.22580377597781620 ) ) ;
#25122 = VERTEX_POINT ( 'NONE', #11965 ) ;
#25123 = CARTESIAN_POINT ( 'NONE',  ( 0.7764146366350239692, 28.53559796717425456, 37.22579914958128455 ) ) ;
#25124 = ORIENTED_EDGE ( 'NONE', *, *, #24314, .T. ) ;
#25125 = VERTEX_POINT ( 'NONE', #35139 ) ;
#25126 = CARTESIAN_POINT ( 'NONE',  ( 0.1081432562775997142, 10.75186376283284062, 41.76274004527636663 ) ) ;
#25127 = EDGE_LOOP ( 'NONE', ( #19369, #61844 ) ) ;
#25128 = DIRECTION ( 'NONE',  ( -1.000000000000000000, -0.000000000000000000, -0.000000000000000000 ) ) ;
#25129 = EDGE_CURVE ( 'NONE', #22672, #4231, #21026, .T. ) ;
#25130 = CARTESIAN_POINT ( 'NONE',  ( 0.5997462898726536595, -43.04230894295718457, -23.64130434225950950 ) ) ;
#25131 = ORIENTED_EDGE ( 'NONE', *, *, #2307, .T. ) ;
#25132 = CARTESIAN_POINT ( 'NONE',  ( 1.231276596079881935, -34.07446381689681658, -24.41736444846283405 ) ) ;
#25133 = CARTESIAN_POINT ( 'NONE',  ( 0.9730545539215892381, 39.83279466599039154, 15.95224156741843835 ) ) ;
#25134 = ORIENTED_EDGE ( 'NONE', *, *, #7328, .T. ) ;
#25135 = EDGE_LOOP ( 'NONE', ( #49560, #59560, #38425, #42916 ) ) ;
#25136 = CARTESIAN_POINT ( 'NONE',  ( 0.5782707292762423457, 23.17211662964077235, 40.77731433787596416 ) ) ;
#25137 = CARTESIAN_POINT ( 'NONE',  ( 47.86699140808116937, 12.49636532218518425, -0.3460709571827094710 ) ) ;
#25138 = CARTESIAN_POINT ( 'NONE',  ( 0.8744876279028306332, -43.20725972823464645, -23.31271664041680580 ) ) ;
#25139 = DIRECTION ( 'NONE',  ( -0.07439287786467652097, -0.5100024374914818859, -0.8569499480575037964 ) ) ;
#25140 = EDGE_LOOP ( 'NONE', ( #31075, #11404, #8532, #30833 ) ) ;
#25141 = CARTESIAN_POINT ( 'NONE',  ( 0.1129192098497447394, -1.898585089631814826, -44.08341142019957459 ) ) ;
#25142 =( BOUNDED_SURFACE ( )  B_SPLINE_SURFACE ( 3, 1, ( 
 ( #30692, #25074 ),
 ( #952, #44218 ),
 ( #34799, #5934 ),
 ( #1248, #30377 ) ),
 .UNSPECIFIED., .F., .F., .F. ) 
 B_SPLINE_SURFACE_WITH_KNOTS ( ( 4, 4 ),
 ( 2, 2 ),
 ( 0.000000000000000000, 1.000000000000000000 ),
 ( 0.000000000000000000, 1.000000000000000000 ),
 .UNSPECIFIED. ) 
 GEOMETRIC_REPRESENTATION_ITEM ( )  RATIONAL_B_SPLINE_SURFACE ( (
 ( 1.000000000000000000, 1.000000000000000000),
 ( 0.9751682680413298332, 0.9999560080971552356),
 ( 0.9751682680413298332, 0.9999560080971552356),
 ( 1.000000000000000000, 1.000000000000000000) ) ) 
 REPRESENTATION_ITEM ( '' )  SURFACE ( )  );
#25143 = CARTESIAN_POINT ( 'NONE',  ( 0.6000166863083090663, 48.10206967781400778, 9.900220927796539172 ) ) ;
#25144 = CARTESIAN_POINT ( 'NONE',  ( 2.301529144917014325, 30.25186323939223954, 37.31001381748743029 ) ) ;
#25145 = VERTEX_POINT ( 'NONE', #31043 ) ;
#25146 = CARTESIAN_POINT ( 'NONE',  ( 1.479689385636123067, -42.90531205933121583, -10.03583790020046784 ) ) ;
#25147 = CARTESIAN_POINT ( 'NONE',  ( -6.079354080745853928, 9.981161348512436859, -16.46722117975960842 ) ) ;
#25148 = CARTESIAN_POINT ( 'NONE',  ( 2.359973842542475886, 8.319337843647435449, -43.23105958076618549 ) ) ;
#25149 = FACE_BOUND ( 'NONE', #16977, .T. ) ;
#25150 = ORIENTED_EDGE ( 'NONE', *, *, #10126, .F. ) ;
#25151 = ORIENTED_EDGE ( 'NONE', *, *, #15211, .T. ) ;
#25152 = CARTESIAN_POINT ( 'NONE',  ( 0.9780303403264782869, -39.69490490238998603, -13.44076404767592692 ) ) ;
#25153 = CARTESIAN_POINT ( 'NONE',  ( 0.1073791018717578927, 37.58707531572206051, -21.14095454447521405 ) ) ;
#25154 = ADVANCED_FACE ( 'NONE', ( #50155 ), #18040, .F. ) ;
#25155 = CARTESIAN_POINT ( 'NONE',  ( 0.9772918015221170318, 14.67438192764145199, -39.25556483853453926 ) ) ;
#25156 = CARTESIAN_POINT ( 'NONE',  ( 0.8560838555295223751, 36.24009790160352651, -29.78301761346427767 ) ) ;
#25157 = AXIS2_PLACEMENT_3D ( 'NONE', #15609, #53180, #10285 ) ;
#25158 = CARTESIAN_POINT ( 'NONE',  ( 0.1104177457020372871, 34.20994892372210217, -26.25638621857955712 ) ) ;
#25159 = EDGE_CURVE ( 'NONE', #38023, #32695, #51305, .T. ) ;
#25160 = CARTESIAN_POINT ( 'NONE',  ( 4.322998006666179727, 4.155494336618708928, -47.80838462754061169 ) ) ;
#25161 =( BOUNDED_SURFACE ( )  B_SPLINE_SURFACE ( 3, 1, ( 
 ( #22511, #13126 ),
 ( #33151, #32532 ),
 ( #23430, #36621 ),
 ( #60696, #51611 ) ),
 .UNSPECIFIED., .F., .F., .F. ) 
 B_SPLINE_SURFACE_WITH_KNOTS ( ( 4, 4 ),
 ( 2, 2 ),
 ( 0.000000000000000000, 1.000000000000000000 ),
 ( 0.000000000000000000, 1.000000000000000000 ),
 .UNSPECIFIED. ) 
 GEOMETRIC_REPRESENTATION_ITEM ( )  RATIONAL_B_SPLINE_SURFACE ( (
 ( 1.000000000000000000, 1.000000000000000000),
 ( 0.9952954269826590483, 0.8620686068821307169),
 ( 0.9952954269826590483, 0.8620686068821307169),
 ( 1.000000000000000000, 1.000000000000000000) ) ) 
 REPRESENTATION_ITEM ( '' )  SURFACE ( )  );
#25162 = AXIS2_PLACEMENT_3D ( 'NONE', #16116, #60460, #34925 ) ;
#25163 = CARTESIAN_POINT ( 'NONE',  ( 0.8551540677456834771, -34.52115452272905571, -33.23105123575936659 ) ) ;
#25164 = CARTESIAN_POINT ( 'NONE',  ( 0.6039202388192952409, 44.16863261170576749, 21.46382086351711749 ) ) ;
#25165 = DIRECTION ( 'NONE',  ( 1.000000000000000000, -0.000000000000000000, -0.000000000000000000 ) ) ;
#25166 = EDGE_CURVE ( 'NONE', #12159, #9208, #48324, .T. ) ;
#25167 = CARTESIAN_POINT ( 'NONE',  ( 0.1087620492084206275, 30.74858804150686709, -30.23658359364789305 ) ) ;
#25168 = EDGE_CURVE ( 'NONE', #5258, #60330, #34027, .T. ) ;
#25169 = CARTESIAN_POINT ( 'NONE',  ( 0.5998501479064708430, -34.38546660123321175, 33.64490850298784608 ) ) ;
#25170 = ADVANCED_FACE ( 'NONE', ( #59217 ), #51308, .F. ) ;
#25171 = CARTESIAN_POINT ( 'NONE',  ( 3.376099380956838925, 9.644725941469024733, -9.310620019419843629 ) ) ;
#25172 = DIRECTION ( 'NONE',  ( 0.000000000000000000, 0.000000000000000000, 1.000000000000000000 ) ) ;
#25173 = CARTESIAN_POINT ( 'NONE',  ( 0.5800708119828333897, 29.65250521075944334, 37.61306658477484888 ) ) ;
#25174 = CARTESIAN_POINT ( 'NONE',  ( 0.5998501479064699549, -23.59887241503383493, 41.92175333043579144 ) ) ;
#25175 = CARTESIAN_POINT ( 'NONE',  ( 0.5839880159502348622, -41.50181427378120702, 23.90868446765462707 ) ) ;
#25176 = DIRECTION ( 'NONE',  ( -1.000000000000000000, -0.000000000000000000, -0.000000000000000000 ) ) ;
#25177 = ITEM_DEFINED_TRANSFORMATION ( 'NONE', 'NONE', #24882,  #14677 ) ;
#25178 = CARTESIAN_POINT ( 'NONE',  ( 0.9736507210033049642, -26.47691119766813728, 33.76542629919396887 ) ) ;
#25179 = EDGE_CURVE ( 'NONE', #12452, #57986, #22053, .T. ) ;
#25180 = CARTESIAN_POINT ( 'NONE',  ( 0.9762797500689124330, 29.49606728235512776, 29.77090526101756751 ) ) ;
#25181 = EDGE_CURVE ( 'NONE', #1177, #23932, #57042, .T. ) ;
#25182 = CARTESIAN_POINT ( 'NONE',  ( -1.139999999999999902, 0.000000000000000000, -5.633200000000004870 ) ) ;
#25183 = DIRECTION ( 'NONE',  ( -1.000000000000000000, -0.000000000000000000, -0.000000000000000000 ) ) ;
#25185 = ORIENTED_EDGE ( 'NONE', *, *, #41186, .T. ) ;
#25184 = CARTESIAN_POINT ( 'NONE',  ( -49.49999999999975842, 5.000000000000000000, 1.078520768856852078E-29 ) ) ;
#25187 = ORIENTED_EDGE ( 'NONE', *, *, #29408, .T. ) ;
#25186 = B_SPLINE_CURVE_WITH_KNOTS ( 'NONE', 3,
 ( #3953, #46917, #47210, #42519 ),
 .UNSPECIFIED., .F., .F.,
 ( 4, 4 ),
 ( 7.296157027441120170E-17, 0.005004741218457514282 ),
 .UNSPECIFIED. ) ;
#25188 = DIRECTION ( 'NONE',  ( -0.07500201931887527651, -0.8960136144483755727, -0.4376463181854141071 ) ) ;
#25189 = CARTESIAN_POINT ( 'NONE',  ( 1.231276596079887264, -18.40965318903149495, -37.66113965983570466 ) ) ;
#25190 = CARTESIAN_POINT ( 'NONE',  ( 0.3622758884714600280, -34.70015533914845918, 25.58609868863709380 ) ) ;
#25191 = EDGE_LOOP ( 'NONE', ( #50412, #48482, #41438, #18981 ) ) ;
#25192 = ORIENTED_EDGE ( 'NONE', *, *, #20449, .T. ) ;
#25193 = CARTESIAN_POINT ( 'NONE',  ( 0.1098349054025746369, -11.36734385884033927, 41.59932877996178746 ) ) ;
#25194 = CARTESIAN_POINT ( 'NONE',  ( -6.016761891674565099, -13.32657647165364700, 13.32172022638586917 ) ) ;
#25195 = CARTESIAN_POINT ( 'NONE',  ( 4.335381028904216727, 48.44495715814551318, 7.269317272604989277 ) ) ;
#25196 = VERTEX_POINT ( 'NONE', #59849 ) ;
#25197 = VERTEX_POINT ( 'NONE', #22573 ) ;
#25198 = CARTESIAN_POINT ( 'NONE',  ( -6.016761891674565099, -18.20201388312099056, 4.873659902332302174 ) ) ;
#25199 = CARTESIAN_POINT ( 'NONE',  ( -4.000000000000000000, -2.309401076758531346, -0.3572655899081733644 ) ) ;
#25200 = CARTESIAN_POINT ( 'NONE',  ( 0.7242003506639976829, -0.7549803952411664465, 49.09624913095526466 ) ) ;
#25201 = CARTESIAN_POINT ( 'NONE',  ( -6.078457390727109555, -19.21618051603926958, -1.238110420156709246 ) ) ;
#25202 = CARTESIAN_POINT ( 'NONE',  ( 0.1129192098497455998, -1.898585089632445433, 44.08341142019953907 ) ) ;
#25203 = EDGE_CURVE ( 'NONE', #17743, #48550, #19822, .T. ) ;
#25204 = B_SPLINE_CURVE_WITH_KNOTS ( 'NONE', 3,
 ( #20019, #58188, #53787, #15924 ),
 .UNSPECIFIED., .F., .F.,
 ( 4, 4 ),
 ( 0.000000000000000000, 0.004444103432399267029 ),
 .UNSPECIFIED. ) ;
#25205 = CIRCLE ( 'NONE', #59219, 12.55882000000000076 ) ;
#25206 = DIRECTION ( 'NONE',  ( -1.000000000000000000, -1.836909530733573776E-16, 1.925929944387235853E-32 ) ) ;
#25207 = VECTOR ( 'NONE', #1148, 999.9999999999998863 ) ;
#25208 = B_SPLINE_CURVE_WITH_KNOTS ( 'NONE', 3,
 ( #20729, #44255, #5055, #38618, #5364, #24493, #43632, #674, #19817, #57988, #53295, #10407, #29500, #48607, #5664, #43952, #20121, #39241, #58290 ),
 .UNSPECIFIED., .F., .F.,
 ( 4, 3, 3, 3, 3, 3, 4 ),
 ( 8.782706832233357974E-18, 0.0002732106629380614562, 0.0004098138914053768957, 0.0005464171197651472318, 0.0006830203481512577175, 0.0008196235766963645003, 0.001011968216111141811 ),
 .UNSPECIFIED. ) ;
#25209 = EDGE_CURVE ( 'NONE', #7463, #49001, #40035, .T. ) ;
#25210 = CARTESIAN_POINT ( 'NONE',  ( 0.6001305935487315502, 18.89378601236065691, -44.24520387813809208 ) ) ;
#25211 = VERTEX_POINT ( 'NONE', #32594 ) ;
#25212 = ORIENTED_EDGE ( 'NONE', *, *, #11084, .F. ) ;
#25213 = CARTESIAN_POINT ( 'NONE',  ( 4.549368137175248350, 2.596185425821331272, 42.84816078363931524 ) ) ;
#25214 = VERTEX_POINT ( 'NONE', #16966 ) ;
#25215 = CARTESIAN_POINT ( 'NONE',  ( 0.8760168074887090262, 46.22580377597785883, -13.30888447662032092 ) ) ;
#25216 = CARTESIAN_POINT ( 'NONE',  ( 5.981074661064941900, 14.51919955600735612, -14.50705827991430930 ) ) ;
#25217 = CARTESIAN_POINT ( 'NONE',  ( 0.5782707292762442330, -20.39674625896916993, 42.23398034468034012 ) ) ;
#25218 = CARTESIAN_POINT ( 'NONE',  ( 0.1140933569871964842, -40.75566919115180298, -16.90932816126367300 ) ) ;
#25219 = ORIENTED_EDGE ( 'NONE', *, *, #3323, .F. ) ;
#25220 = DIRECTION ( 'NONE',  ( 1.000000000000000000, 0.000000000000000000, 0.000000000000000000 ) ) ;
#25221 = CARTESIAN_POINT ( 'NONE',  ( 0.6008122571543325074, -34.97209109721812581, 34.47473560091786737 ) ) ;
#25222 = DIRECTION ( 'NONE',  ( 1.000000000000000000, 1.836909530733573776E-16, -1.925929944387235853E-32 ) ) ;
#25223 = CARTESIAN_POINT ( 'NONE',  ( 5.896782393890504181, -19.39988559968493576, 5.307591317834223332 ) ) ;
#25224 = ORIENTED_EDGE ( 'NONE', *, *, #10862, .F. ) ;
#25225 = CARTESIAN_POINT ( 'NONE',  ( 0.5807400328401574052, 23.47602859900773353, -41.75144119563861267 ) ) ;
#25226 = CARTESIAN_POINT ( 'NONE',  ( 5.960221823109900008, 2.684531185214145577, 20.34928172836731619 ) ) ;
#25227 = VERTEX_POINT ( 'NONE', #8771 ) ;
#25228 = CARTESIAN_POINT ( 'NONE',  ( 0.7056759521544988534, -44.02266877934305001, -16.17879670004061055 ) ) ;
#25229 = CARTESIAN_POINT ( 'NONE',  ( 0.1152809850208375703, 9.602783458000070382, 43.06659764072982455 ) ) ;
#25230 = B_SPLINE_CURVE_WITH_KNOTS ( 'NONE', 3,
 ( #48588, #19794, #58272, #53887, #5643, #39847, #38916, #26025, #44544, #39222, #30714, #25089, #11309, #58903, #59209, #1573, #53572, #20709, #58581 ),
 .UNSPECIFIED., .F., .F.,
 ( 4, 3, 3, 3, 3, 3, 4 ),
 ( 8.674294979774126656E-18, 0.0002732106629380616188, 0.0004098138914053757031, 0.0005464171197651461476, 0.0006830203481512564165, 0.0008196235766963625487, 0.001011968216111142245 ),
 .UNSPECIFIED. ) ;
#25231 = EDGE_LOOP ( 'NONE', ( #48794, #60810, #35005, #11269 ) ) ;
#25232 = CARTESIAN_POINT ( 'NONE',  ( 10.00000000000001599, -58.44237546506844438, 54.69470952477916370 ) ) ;
#25233 = CARTESIAN_POINT ( 'NONE',  ( 0.6030672727741701600, -47.70721108823352807, 6.192762795893642647 ) ) ;
#25234 = EDGE_CURVE ( 'NONE', #47712, #60852, #19165, .T. ) ;
#25235 = LINE ( 'NONE', #49346, #13844 ) ;
#25236 = EDGE_CURVE ( 'NONE', #40875, #29142, #32077, .T. ) ;
#25237 = CARTESIAN_POINT ( 'NONE',  ( 0.6027935024548037868, -41.74929432965634390, 23.90242449907741218 ) ) ;
#25238 = LINE ( 'NONE', #29940, #55814 ) ;
#25239 = DIRECTION ( 'NONE',  ( 0.000000000000000000, -1.000000000000000000, -0.000000000000000000 ) ) ;
#25240 = CARTESIAN_POINT ( 'NONE',  ( 7.000000000000006217, -2.780326704359372228E-13, 80.00000000000001421 ) ) ;
#25241 = DIRECTION ( 'NONE',  ( -1.000000000000000000, -0.000000000000000000, -0.000000000000000000 ) ) ;
#25242 = VERTEX_POINT ( 'NONE', #46093 ) ;
#25243 = DIRECTION ( 'NONE',  ( 0.000000000000000000, 0.000000000000000000, -1.000000000000000000 ) ) ;
#25244 = EDGE_CURVE ( 'NONE', #5027, #35750, #43810, .T. ) ;
#25245 = CARTESIAN_POINT ( 'NONE',  ( 0.3622758884714730732, -40.13994584881772454, -15.73321244754840720 ) ) ;
#25246 = EDGE_CURVE ( 'NONE', #48814, #25197, #29028, .T. ) ;
#25247 = CARTESIAN_POINT ( 'NONE',  ( 4.956653778116987930, -47.05699031914942054, -9.917440902361647659 ) ) ;
#25248 = ORIENTED_EDGE ( 'NONE', *, *, #39326, .F. ) ;
#25249 = EDGE_CURVE ( 'NONE', #59402, #41892, #23576, .T. ) ;
#25250 = CARTESIAN_POINT ( 'NONE',  ( 4.960386119450148179, 43.62260476509040785, 3.391875319207611206 ) ) ;
#25251 = CARTESIAN_POINT ( 'NONE',  ( 4.956653778116989706, -40.28700667097662347, -26.26162724282415084 ) ) ;
#25252 = CARTESIAN_POINT ( 'NONE',  ( 4.956653778116975495, -9.917440902361487787, 47.05699031914946318 ) ) ;
#25253 = CARTESIAN_POINT ( 'NONE',  ( 0.7048096507298579061, 17.62869676200345737, 44.76417498422321728 ) ) ;
#25254 = CARTESIAN_POINT ( 'NONE',  ( 0.6008122571543326185, -19.47898650447827507, 45.07908201398593206 ) ) ;
#25255 = AXIS2_PLACEMENT_3D ( 'NONE', #18189, #37011, #18494 ) ;
#25256 = LINE ( 'NONE', #38769, #10607 ) ;
#25257 = CARTESIAN_POINT ( 'NONE',  ( -1.599999999999961231, 56.56854249492449327, -56.56854249492312903 ) ) ;
#25258 = LINE ( 'NONE', #44401, #48899 ) ;
#25259 = AXIS2_PLACEMENT_3D ( 'NONE', #27331, #3501, #41768 ) ;
#25260 = EDGE_CURVE ( 'NONE', #36276, #55939, #45783, .T. ) ;
#25261 = DIRECTION ( 'NONE',  ( -1.000000000000000000, -0.000000000000000000, -0.000000000000000000 ) ) ;
#25262 = B_SPLINE_CURVE_WITH_KNOTS ( 'NONE', 3,
 ( #2914, #12047, #31121, #7289 ),
 .UNSPECIFIED., .F., .F.,
 ( 4, 4 ),
 ( 0.000000000000000000, 0.004446090762761356445 ),
 .UNSPECIFIED. ) ;
#25263 = CARTESIAN_POINT ( 'NONE',  ( 0.6009453534118439633, 0.4363813339958033111, -48.10564080474284765 ) ) ;
#25265 = VERTEX_POINT ( 'NONE', #20274 ) ;
#25264 = FACE_OUTER_BOUND ( 'NONE', #28828, .T. ) ;
#25266 = EDGE_LOOP ( 'NONE', ( #57635, #28991, #6006, #4001 ) ) ;
#25267 = CYLINDRICAL_SURFACE ( 'NONE', #20050, 11.40403086437694569 ) ;
#25268 = CARTESIAN_POINT ( 'NONE',  ( 0.8744876279028306332, -26.20733431478126008, -41.51536677536140729 ) ) ;
#25269 =( BOUNDED_SURFACE ( )  B_SPLINE_SURFACE ( 3, 1, ( 
 ( #46355, #31006 ),
 ( #7169, #45435 ),
 ( #12847, #31939 ),
 ( #11601, #59186 ) ),
 .UNSPECIFIED., .F., .F., .F. ) 
 B_SPLINE_SURFACE_WITH_KNOTS ( ( 4, 4 ),
 ( 2, 2 ),
 ( 0.000000000000000000, 1.000000000000000000 ),
 ( 0.000000000000000000, 1.000000000000000000 ),
 .UNSPECIFIED. ) 
 GEOMETRIC_REPRESENTATION_ITEM ( )  RATIONAL_B_SPLINE_SURFACE ( (
 ( 1.000000000000000000, 1.000000000000000000),
 ( 0.7211978278499970862, 0.9934217856018976445),
 ( 0.7211978278499970862, 0.9934217856018976445),
 ( 1.000000000000000000, 1.000000000000000000) ) ) 
 REPRESENTATION_ITEM ( '' )  SURFACE ( )  );
#25270 = CARTESIAN_POINT ( 'NONE',  ( 0.1158403557922069033, -22.90600150134859803, 37.71280157193356075 ) ) ;
#25271 = CARTESIAN_POINT ( 'NONE',  ( 0.5827357941260216112, -47.43746130990120236, 6.611647889511030662 ) ) ;
#25272 = CARTESIAN_POINT ( 'NONE',  ( 0.1156867017252034419, 9.940337221640810128, -42.98991164442244894 ) ) ;
#25273 =( BOUNDED_SURFACE ( )  B_SPLINE_SURFACE ( 3, 1, ( 
 ( #42144, #8266 ),
 ( #3254, #8576 ),
 ( #32102, #22381 ),
 ( #36814, #27703 ) ),
 .UNSPECIFIED., .F., .F., .F. ) 
 B_SPLINE_SURFACE_WITH_KNOTS ( ( 4, 4 ),
 ( 2, 2 ),
 ( 0.000000000000000000, 1.000000000000000000 ),
 ( 0.000000000000000000, 1.000000000000000000 ),
 .UNSPECIFIED. ) 
 GEOMETRIC_REPRESENTATION_ITEM ( )  RATIONAL_B_SPLINE_SURFACE ( (
 ( 1.000000000000000000, 1.000000000000000000),
 ( 0.7223157951917476005, 0.9931996967497186413),
 ( 0.7223157951917476005, 0.9931996967497186413),
 ( 1.000000000000000000, 1.000000000000000000) ) ) 
 REPRESENTATION_ITEM ( '' )  SURFACE ( )  );
#25274 = ORIENTED_EDGE ( 'NONE', *, *, #42873, .T. ) ;
#25275 = EDGE_LOOP ( 'NONE', ( #9639, #19468, #6586, #1589 ) ) ;
#25276 = CARTESIAN_POINT ( 'NONE',  ( 0.1073791018717578927, -5.147744207006579309, -42.81622261970993293 ) ) ;
#25277 = CARTESIAN_POINT ( 'NONE',  ( -19.65183073023187532, -7.897491201526634974, 1.291549906873825870 ) ) ;
#25278 = CARTESIAN_POINT ( 'NONE',  ( 0.6027444965799114707, 37.30784590784681853, 31.93216481236119719 ) ) ;
#25279 = EDGE_LOOP ( 'NONE', ( #38255, #32267, #45944, #44072 ) ) ;
#25280 = CARTESIAN_POINT ( 'NONE',  ( 0.2230388203127542934, 36.95676097786380154, -22.21453373073351756 ) ) ;
#25281 = CARTESIAN_POINT ( 'NONE',  ( 4.956653778117001252, 47.27023054223765541, -8.845409907520457082 ) ) ;
#25282 = ORIENTED_EDGE ( 'NONE', *, *, #3459, .F. ) ;
#25283 = EDGE_CURVE ( 'NONE', #38360, #57884, #54959, .T. ) ;
#25284 = CARTESIAN_POINT ( 'NONE',  ( 4.694002226626920127, -20.78018001817206439, 40.57670378257081012 ) ) ;
#25285 = ORIENTED_EDGE ( 'NONE', *, *, #25863, .F. ) ;
#25286 = CARTESIAN_POINT ( 'NONE',  ( 0.3622758884714600280, 41.85013935980101962, -10.35929834645879133 ) ) ;
#25287 = CARTESIAN_POINT ( 'NONE',  ( 0.9730545539215883499, 42.90536227157002003, -0.5054011016614180507 ) ) ;
#25288 = VERTEX_POINT ( 'NONE', #24655 ) ;
#25289 = CARTESIAN_POINT ( 'NONE',  ( 0.5837799406558225046, -19.65753372021275069, 42.57728170768891829 ) ) ;
#25290 = LINE ( 'NONE', #57232, #27717 ) ;
#25291 = CARTESIAN_POINT ( 'NONE',  ( 4.975801465491694664, -47.84403947906841381, 2.564218696447319257 ) ) ;
#25292 = STYLED_ITEM ( 'NONE', ( #60309 ), #31769 ) ;
#25293 = ORIENTED_EDGE ( 'NONE', *, *, #12006, .F. ) ;
#25294 = CARTESIAN_POINT ( 'NONE',  ( 4.335381028904201628, -27.18827219542433227, 40.74990432739517843 ) ) ;
#25295 = CARTESIAN_POINT ( 'NONE',  ( -3.319141568766058814, -12.31039395171775830, 0.000000000000000000 ) ) ;
#25296 = VERTEX_POINT ( 'NONE', #51988 ) ;
#25297 = CARTESIAN_POINT ( 'NONE',  ( 1.231276596079881047, 40.64579686208666232, -10.25650859035628315 ) ) ;
#25298 = ORIENTED_EDGE ( 'NONE', *, *, #5935, .T. ) ;
#25299 = CARTESIAN_POINT ( 'NONE',  ( 4.975610109902397937, 35.53430708602537891, 33.61193875773635398 ) ) ;
#25300 = VERTEX_POINT ( 'NONE', #58752 ) ;
#25301 = CARTESIAN_POINT ( 'NONE',  ( 1.231276596079887264, -31.65135013586864332, -27.48579279545554144 ) ) ;
#25302 = DIRECTION ( 'NONE',  ( -0.000000000000000000, 0.000000000000000000, 1.000000000000000000 ) ) ;
#25303 = CARTESIAN_POINT ( 'NONE',  ( 0.9745511491811754690, 33.83313387735789490, 26.39034508612545693 ) ) ;
#25304 = ORIENTED_EDGE ( 'NONE', *, *, #38102, .F. ) ;
#25305 = CARTESIAN_POINT ( 'NONE',  ( 0.1119898979215351864, 41.69625316766367717, -14.43550414879666732 ) ) ;
#25306 = CARTESIAN_POINT ( 'NONE',  ( 3.270143674763207553, -8.113405361969434182, -11.02405647745178641 ) ) ;
#25307 = ADVANCED_FACE ( 'NONE', ( #24968 ), #55694, .F. ) ;
#25308 = CARTESIAN_POINT ( 'NONE',  ( 4.834790513006555379, -39.34655703395279147, 26.16176199146916304 ) ) ;
#25309 = VERTEX_POINT ( 'NONE', #43796 ) ;
#25310 = ADVANCED_FACE ( 'NONE', ( #1137 ), #25267, .T. ) ;
#25311 = B_SPLINE_CURVE_WITH_KNOTS ( 'NONE', 3,
 ( #13253, #42385, #32667, #51129 ),
 .UNSPECIFIED., .F., .F.,
 ( 4, 4 ),
 ( 0.000000000000000000, 0.004446090762761359047 ),
 .UNSPECIFIED. ) ;
#25312 = EDGE_LOOP ( 'NONE', ( #42701, #56961, #52145, #42821 ) ) ;
#25313 = CARTESIAN_POINT ( 'NONE',  ( 0.8557997880470690211, -24.73961900479222820, -41.02602466100805145 ) ) ;
#25314 = CARTESIAN_POINT ( 'NONE',  ( 2.359973842542475886, 30.69728382343663498, 31.55649949686871381 ) ) ;
#25315 = FACE_OUTER_BOUND ( 'NONE', #57878, .T. ) ;
#25316 = CARTESIAN_POINT ( 'NONE',  ( 3.678748215320120085, -15.69769956952215395, -46.39175619142379503 ) ) ;
#25317 = CARTESIAN_POINT ( 'NONE',  ( 4.962356264823596597, 41.32726869310139506, 7.955655864260913646 ) ) ;
#25318 = CARTESIAN_POINT ( 'NONE',  ( 0.9762797500689124330, 38.38274741215467145, 16.82526333465357382 ) ) ;
#25319 = VERTEX_POINT ( 'NONE', #39392 ) ;
#25320 = ADVANCED_FACE ( 'NONE', ( #27886 ), #12928, .F. ) ;
#25321 = CARTESIAN_POINT ( 'NONE',  ( 0.5809828226811553087, 6.791453954330313181, 47.41188724015881917 ) ) ;
#25322 = EDGE_CURVE ( 'NONE', #47737, #35307, #34801, .T. ) ;
#25323 = EDGE_LOOP ( 'NONE', ( #27304, #30659, #20927, #23815 ) ) ;
#25324 = EDGE_CURVE ( 'NONE', #30112, #12663, #4138, .T. ) ;
#25325 = CARTESIAN_POINT ( 'NONE',  ( 0.3676999524040366896, -38.83470403830472151, -20.92406140260821346 ) ) ;
#25326 = CARTESIAN_POINT ( 'NONE',  ( 0.6067375320500727476, -38.42671567536872601, 28.59217831627001516 ) ) ;
#25327 = CARTESIAN_POINT ( 'NONE',  ( 4.967162193818131399, -42.34252806656588319, -7.970725651240238463 ) ) ;
#25328 = B_SPLINE_CURVE_WITH_KNOTS ( 'NONE', 3,
 ( #10283, #11515, #54087, #34710 ),
 .UNSPECIFIED., .F., .F.,
 ( 4, 4 ),
 ( 4.470280076681872512E-19, 0.004048833967417084755 ),
 .UNSPECIFIED. ) ;
#25329 = CARTESIAN_POINT ( 'NONE',  ( 5.965394784446458765, -18.96850062921629743, -7.841344330024877074 ) ) ;
#25330 = CARTESIAN_POINT ( 'NONE',  ( 0.5997462898726536595, -31.02483596213057737, 38.06587952047342327 ) ) ;
#25331 = B_SPLINE_CURVE_WITH_KNOTS ( 'NONE', 3,
 ( #52634, #38888, #43276, #33560 ),
 .UNSPECIFIED., .F., .F.,
 ( 4, 4 ),
 ( 1.939479807224432123E-18, 0.004050076154992998147 ),
 .UNSPECIFIED. ) ;
#25332 = SHAPE_REPRESENTATION_RELATIONSHIP ( 'NONE' , 'NONE' ,  #6760, #4831 ) ;
#25333 = B_SPLINE_CURVE_WITH_KNOTS ( 'NONE', 3,
 ( #5216, #52846, #24036, #201 ),
 .UNSPECIFIED., .F., .F.,
 ( 4, 4 ),
 ( 1.734723475976807094E-18, 0.004048833967417087357 ),
 .UNSPECIFIED. ) ;
#25334 = CARTESIAN_POINT ( 'NONE',  ( 0.6028777368367060907, 37.44903595938922791, -31.76648446119660107 ) ) ;
#25335 = FACE_OUTER_BOUND ( 'NONE', #52387, .T. ) ;
#25336 = CARTESIAN_POINT ( 'NONE',  ( 1.000110580585053199, 10.35431645662686151, -40.61041262395552565 ) ) ;
#25338 = EDGE_CURVE ( 'NONE', #24433, #23785, #29564, .T. ) ;
#25337 = CARTESIAN_POINT ( 'NONE',  ( 1.157643937452369487, 5.016389049135196565, 41.61535912980291130 ) ) ;
#25339 = CARTESIAN_POINT ( 'NONE',  ( 4.956653778116966613, 0.000000000000000000, 0.000000000000000000 ) ) ;
#25340 = CARTESIAN_POINT ( 'NONE',  ( 0.9769922540276054779, 9.284899304422724597, 40.86712859980321610 ) ) ;
#25341 = EDGE_CURVE ( 'NONE', #41494, #23520, #48218, .T. ) ;
#25342 = CARTESIAN_POINT ( 'NONE',  ( 3.727782113643637540, -19.72952865065639116, -39.28770132151922923 ) ) ;
#25343 = VECTOR ( 'NONE', #61665, 1000.000000000000114 ) ;
#25344 = CARTESIAN_POINT ( 'NONE',  ( 4.553261556744875094, -4.442710778082547662, 43.70128015019636791 ) ) ;
#25345 = CARTESIAN_POINT ( 'NONE',  ( -2.739355103387247858, -14.83685109948653391, 1.647852057280082771 ) ) ;
#25346 =( BOUNDED_SURFACE ( )  B_SPLINE_SURFACE ( 3, 1, ( 
 ( #22094, #12398 ),
 ( #32427, #3267 ),
 ( #13632, #27401 ),
 ( #41526, #26789 ) ),
 .UNSPECIFIED., .F., .F., .F. ) 
 B_SPLINE_SURFACE_WITH_KNOTS ( ( 4, 4 ),
 ( 2, 2 ),
 ( 0.000000000000000000, 1.000000000000000000 ),
 ( 0.000000000000000000, 1.000000000000000000 ),
 .UNSPECIFIED. ) 
 GEOMETRIC_REPRESENTATION_ITEM ( )  RATIONAL_B_SPLINE_SURFACE ( (
 ( 1.000000000000000000, 1.000000000000000000),
 ( 0.9952954269826590483, 0.8620686068821339365),
 ( 0.9952954269826590483, 0.8620686068821339365),
 ( 1.000000000000000000, 1.000000000000000000) ) ) 
 REPRESENTATION_ITEM ( '' )  SURFACE ( )  );
#25347 = ORIENTED_EDGE ( 'NONE', *, *, #58680, .T. ) ;
#25348 = SURFACE_SIDE_STYLE ('',( #6203 ) ) ;
#25349 = CARTESIAN_POINT ( 'NONE',  ( 0.1081432562775997419, 43.12249629849793564, 0.4234896101213052044 ) ) ;
#25350 = B_SPLINE_CURVE_WITH_KNOTS ( 'NONE', 3,
 ( #30160, #1035, #49270, #1643 ),
 .UNSPECIFIED., .F., .F.,
 ( 4, 4 ),
 ( 8.673617379884035472E-19, 0.004042984057420972825 ),
 .UNSPECIFIED. ) ;
#25351 = CARTESIAN_POINT ( 'NONE',  ( 1.479689385636123067, 24.23631239248258495, -36.79925280330684956 ) ) ;
#25352 = CARTESIAN_POINT ( 'NONE',  ( 5.331200000000000827, 0.000000000000000000, 0.000000000000000000 ) ) ;
#25353 = CARTESIAN_POINT ( 'NONE',  ( 0.5809828226811553087, -24.41822904836894637, -41.20389530892332886 ) ) ;
#25354 = ORIENTED_EDGE ( 'NONE', *, *, #31695, .F. ) ;
#25355 = CARTESIAN_POINT ( 'NONE',  ( 5.981074661064941900, 16.28853686865598860, -12.48781255314272087 ) ) ;
#25356 = CARTESIAN_POINT ( 'NONE',  ( 58.00000000000000000, 8.437969416220405915E-15, -2.995852231480068572E-16 ) ) ;
#25357 = CARTESIAN_POINT ( 'NONE',  ( 4.691466044806102964, 40.13652286047893369, -19.42108863068337143 ) ) ;
#25358 = EDGE_LOOP ( 'NONE', ( #61966, #42343, #47789, #10353 ) ) ;
#25359 = CARTESIAN_POINT ( 'NONE',  ( 5.896278296736517710, 12.98960347168511120, 15.35568888922831121 ) ) ;
#25360 = ADVANCED_FACE ( 'NONE', ( #838 ), #19320, .F. ) ;
#25361 = CARTESIAN_POINT ( 'NONE',  ( 2.282803330402972453, 6.007211579933096957, -46.58766270688949618 ) ) ;
#25362 = ORIENTED_EDGE ( 'NONE', *, *, #19031, .F. ) ;
#25363 = DIRECTION ( 'NONE',  ( 0.07836865515943411409, -0.007886984708671416350, 0.9968932487286222832 ) ) ;
#25364 = VERTEX_POINT ( 'NONE', #55291 ) ;
#25365 = ORIENTED_EDGE ( 'NONE', *, *, #31470, .F. ) ;
#25366 = DIRECTION ( 'NONE',  ( -1.000000000000000000, -0.000000000000000000, -0.000000000000000000 ) ) ;
#25367 = DIRECTION ( 'NONE',  ( -0.1024043820194934645, -0.7126273545981489654, 0.6940285268068233648 ) ) ;
#25368 = ORIENTED_EDGE ( 'NONE', *, *, #54923, .F. ) ;
#25369 = PRODUCT_DEFINITION_SHAPE ( 'NONE', 'NONE',  #62002 ) ;
#25370 = B_SPLINE_CURVE_WITH_KNOTS ( 'NONE', 3,
 ( #17168, #36281, #6179, #7109, #21242, #26235 ),
 .UNSPECIFIED., .F., .F.,
 ( 4, 2, 4 ),
 ( 2.032850612904068153E-17, 0.0002293319059085098999, 0.0004586638118169994709 ),
 .UNSPECIFIED. ) ;
#25371 = ORIENTED_EDGE ( 'NONE', *, *, #60027, .F. ) ;
#25372 = DIRECTION ( 'NONE',  ( 0.000000000000000000, 0.000000000000000000, -1.000000000000000000 ) ) ;
#25373 = DIRECTION ( 'NONE',  ( 0.000000000000000000, 0.000000000000000000, 1.000000000000000000 ) ) ;
#25374 = ORIENTED_EDGE ( 'NONE', *, *, #31514, .F. ) ;
#25376 = CARTESIAN_POINT ( 'NONE',  ( 0.8753041380234530822, 43.84722337925244062, -22.10337824412636820 ) ) ;
#25375 = B_SPLINE_CURVE_WITH_KNOTS ( 'NONE', 3,
 ( #16386, #39915, #34893, #53957, #1036, #20174 ),
 .UNSPECIFIED., .F., .F.,
 ( 4, 2, 4 ),
 ( 2.005774019098183203E-18, 0.0002293801035737089383, 0.0004587602071474158709 ),
 .UNSPECIFIED. ) ;
#25377 = CARTESIAN_POINT ( 'NONE',  ( 2.185380717157383135, -36.12942123712758047, -25.16912243478889977 ) ) ;
#25378 = DIRECTION ( 'NONE',  ( 0.09722883295013595717, 0.6746907015591536716, -0.7316686485512220450 ) ) ;
#25379 = CARTESIAN_POINT ( 'NONE',  ( 0.8551540677456715978, 17.49081417858787191, 44.61036085020956676 ) ) ;
#25380 = EDGE_LOOP ( 'NONE', ( #22138, #14109, #21613, #41554 ) ) ;
#25381 = CARTESIAN_POINT ( 'NONE',  ( -6.077587904424778920, -11.02178778841139284, 15.78975032548507151 ) ) ;
#25382 = ORIENTED_EDGE ( 'NONE', *, *, #61384, .F. ) ;
#25383 = DIRECTION ( 'NONE',  ( 0.000000000000000000, 0.000000000000000000, 1.000000000000000000 ) ) ;
#25384 = ORIENTED_EDGE ( 'NONE', *, *, #58959, .T. ) ;
#25385 = CARTESIAN_POINT ( 'NONE',  ( 4.956445790444004018, -46.73954499432468879, 5.740468958468036398 ) ) ;
#25386 = CARTESIAN_POINT ( 'NONE',  ( 0.6846871229502899947, 0.8641397935259540475, 47.90045233486064546 ) ) ;
#25387 = ORIENTED_EDGE ( 'NONE', *, *, #27430, .F. ) ;
#25388 = CARTESIAN_POINT ( 'NONE',  ( 0.9762797500689124330, -12.89881610234921006, -39.87411852747946028 ) ) ;
#25389 = CARTESIAN_POINT ( 'NONE',  ( 0.5806925824938499181, 32.20670061096218006, 34.08739940358331921 ) ) ;
#25390 = CARTESIAN_POINT ( 'NONE',  ( 2.500000000000000000, -1.178949249685214307, 2.042000000000001592 ) ) ;
#25391 = CARTESIAN_POINT ( 'NONE',  ( -19.86127894103453073, -12.46596387912833315, 0.9305556580907108355 ) ) ;
#25392 = ADVANCED_FACE ( 'NONE', ( #35297, #60002 ), #17112, .T. ) ;
#25393 = ORIENTED_EDGE ( 'NONE', *, *, #22957, .F. ) ;
#25394 = FACE_OUTER_BOUND ( 'NONE', #14309, .T. ) ;
#25395 = EDGE_CURVE ( 'NONE', #25122, #3613, #10159, .T. ) ;
#25396 = CARTESIAN_POINT ( 'NONE',  ( 3.270143674763207553, -0.2742231296310536637, 13.68510027222513159 ) ) ;
#25397 = CARTESIAN_POINT ( 'NONE',  ( -2.739355103387247858, 9.839932234829875668, 11.22601000199861510 ) ) ;
#25398 = CIRCLE ( 'NONE', #38397, 42.92674063221959813 ) ;
#25399 = SURFACE_STYLE_FILL_AREA ( #6255 ) ;
#25400 = FILL_AREA_STYLE ('',( #30094 ) ) ;
#25401 = CARTESIAN_POINT ( 'NONE',  ( -2.569797478183790229, -6.011723966604236580, 13.34095667500594828 ) ) ;
#25402 = CARTESIAN_POINT ( 'NONE',  ( 4.967162193818130511, 0.000000000000000000, 0.000000000000000000 ) ) ;
#25403 = CARTESIAN_POINT ( 'NONE',  ( 4.967162193818130511, 14.26841313271336809, -40.65506779172149976 ) ) ;
#25404 = CARTESIAN_POINT ( 'NONE',  ( -2.601141883200662974, 13.24771294992769555, -6.877029087164502563 ) ) ;
#25405 = DIRECTION ( 'NONE',  ( -1.000000000000000000, -0.000000000000000000, -0.000000000000000000 ) ) ;
#25406 = ADVANCED_FACE ( 'NONE', ( #12414 ), #32129, .F. ) ;
#25407 = DIRECTION ( 'NONE',  ( -1.626303258728256651E-16, 1.000000000000000000, 0.000000000000000000 ) ) ;
#25408 = CARTESIAN_POINT ( 'NONE',  ( 0.5830081025819948692, -1.293956464538003948, 46.87811548100160053 ) ) ;
#25409 = DIRECTION ( 'NONE',  ( -1.000000000000000000, -0.000000000000000000, -0.000000000000000000 ) ) ;
#25410 = CARTESIAN_POINT ( 'NONE',  ( 0.6026112563231247332, -45.58358175611240171, 18.26685712398343853 ) ) ;
#25411 = ORIENTED_EDGE ( 'NONE', *, *, #48783, .T. ) ;
#25412 = CARTESIAN_POINT ( 'NONE',  ( 0.8560838555295158248, 31.94705745926175311, 34.34761059777461867 ) ) ;
#25413 = CARTESIAN_POINT ( 'NONE',  ( 1.657374760986086271, 19.27187991371560827, -39.61672742470747011 ) ) ;
#25414 = CARTESIAN_POINT ( 'NONE',  ( 0.5804410086790514622, 46.89585601637879364, -0.5463884574786298520 ) ) ;
#25415 = ORIENTED_EDGE ( 'NONE', *, *, #42260, .T. ) ;
#25416 = DIRECTION ( 'NONE',  ( 0.000000000000000000, 0.000000000000000000, 1.000000000000000000 ) ) ;
#25417 = CARTESIAN_POINT ( 'NONE',  ( 0.000000000000000000, 0.000000000000000000, -1.199999999999999956 ) ) ;
#25418 = VECTOR ( 'NONE', #41541, 1000.000000000000227 ) ;
#25419 = PLANE ( 'NONE',  #33730 ) ;
#25420 = B_SPLINE_CURVE_WITH_KNOTS ( 'NONE', 3,
 ( #41172, #32373, #41481, #33610, #990, #24813, #19509, #57675, #53299, #39245, #38940, #14200, #48311, #33921, #48611, #52996, #57993, #28576, #20126, #9471, #43327, #10412, #58294, #57368, #47699 ),
 .UNSPECIFIED., .F., .F.,
 ( 4, 3, 3, 3, 3, 3, 3, 3, 4 ),
 ( 6.254634441385501517E-18, 0.0005656085177311398569, 0.001131215744874498972, 0.001696821861372767000, 0.002262427090022497284, 0.002828031679238744624, 0.003393635864401603561, 0.003977030878808131623, 0.004561030005651157265 ),
 .UNSPECIFIED. ) ;
#25421 = ORIENTED_EDGE ( 'NONE', *, *, #13045, .F. ) ;
#25422 = EDGE_LOOP ( 'NONE', ( #8042, #38645, #11280, #24747 ) ) ;
#25423 = EDGE_CURVE ( 'NONE', #55303, #28115, #11060, .T. ) ;
#25424 = CARTESIAN_POINT ( 'NONE',  ( 0.5987334308729317378, 37.78232974793878185, 31.36970617311787990 ) ) ;
#25425 = ORIENTED_EDGE ( 'NONE', *, *, #20415, .T. ) ;
#25426 = FACE_OUTER_BOUND ( 'NONE', #23418, .T. ) ;
#25427 = ORIENTED_EDGE ( 'NONE', *, *, #1960, .F. ) ;
#25428 = ORIENTED_EDGE ( 'NONE', *, *, #34244, .F. ) ;
#25429 = DIRECTION ( 'NONE',  ( 0.000000000000000000, 0.000000000000000000, 1.000000000000000000 ) ) ;
#25430 = ORIENTED_EDGE ( 'NONE', *, *, #50647, .F. ) ;
#25431 = CARTESIAN_POINT ( 'NONE',  ( 0.3676999524040323597, -11.75791688508830646, -42.51707861373114383 ) ) ;
#25432 = EDGE_CURVE ( 'NONE', #46904, #31029, #57166, .T. ) ;
#25433 = CARTESIAN_POINT ( 'NONE',  ( 0.9787284016396606834, -17.81048079543711538, -37.93577167745763035 ) ) ;
#25434 = ORIENTED_EDGE ( 'NONE', *, *, #9385, .T. ) ;
#25436 = B_SPLINE_CURVE_WITH_KNOTS ( 'NONE', 3,
 ( #25286, #51542, #3309, #27140 ),
 .UNSPECIFIED., .F., .F.,
 ( 4, 4 ),
 ( 2.276721302528256204E-17, 0.004564976165746189446 ),
 .UNSPECIFIED. ) ;
#25435 = CARTESIAN_POINT ( 'NONE',  ( 4.960156602257185909, -45.42786611289321286, 9.558288641081595927 ) ) ;
#25437 = EDGE_CURVE ( 'NONE', #58998, #56168, #24359, .T. ) ;
#25438 = ORIENTED_EDGE ( 'NONE', *, *, #38088, .T. ) ;
#25439 = DIRECTION ( 'NONE',  ( 1.000000000000000000, 0.000000000000000000, 0.000000000000000000 ) ) ;
#25440 = CARTESIAN_POINT ( 'NONE',  ( 0.9762797500689124330, -37.17323042682959766, -19.35137526946170183 ) ) ;
#25441 = CARTESIAN_POINT ( 'NONE',  ( 4.975801465491694664, 20.67815041659077835, 43.22084481528228395 ) ) ;
#25442 = CARTESIAN_POINT ( 'NONE',  ( 4.967162193818131399, 18.65818244221258126, 38.83676580803773248 ) ) ;
#25443 = VERTEX_POINT ( 'NONE', #49682 ) ;
#25444 = B_SPLINE_CURVE_WITH_KNOTS ( 'NONE', 3,
 ( #9315, #46946, #52532, #23120, #37545, #18423 ),
 .UNSPECIFIED., .F., .F.,
 ( 4, 2, 4 ),
 ( 3.471140604459641645E-18, 0.0002291459268755730266, 0.0004582918537511425838 ),
 .UNSPECIFIED. ) ;
#25445 = EDGE_LOOP ( 'NONE', ( #8098, #4926, #6311, #51384 ) ) ;
#25446 = CARTESIAN_POINT ( 'NONE',  ( 0.5850706913938534814, -23.79070617305411162, 41.56998471741220413 ) ) ;
#25447 = CARTESIAN_POINT ( 'NONE',  ( 0.8554163680231720024, -14.77070554666819291, -44.53124443315552128 ) ) ;
#25448 = CARTESIAN_POINT ( 'NONE',  ( 4.553261556744875094, 38.38432632180499837, -21.35844232721162683 ) ) ;
#25449 = EDGE_LOOP ( 'NONE', ( #40423, #20320, #15631, #37564 ) ) ;
#25450 = CARTESIAN_POINT ( 'NONE',  ( 5.959828726073459926, -17.77796293532166061, -10.25888482581853012 ) ) ;
#25451 = CARTESIAN_POINT ( 'NONE',  ( 0.6039202388192952409, -25.60584472520900334, 41.90351332236327409 ) ) ;
#25452 = CARTESIAN_POINT ( 'NONE',  ( 0.8554163680231720024, 46.90810212776801791, -0.9140174411379322628 ) ) ;
#25453 = CARTESIAN_POINT ( 'NONE',  ( 0.6009452777970410997, -41.87890062806020097, -23.67489783211079413 ) ) ;
#25454 = EDGE_CURVE ( 'NONE', #5563, #41175, #55743, .T. ) ;
#25455 = VERTEX_POINT ( 'NONE', #21486 ) ;
#25456 = B_SPLINE_CURVE_WITH_KNOTS ( 'NONE', 3,
 ( #54482, #49812, #49192, #20088, #53562, #25076, #6870, #35116, #26010, #16004, #10679, #39206, #58258, #29774, #53871, #5938 ),
 .UNSPECIFIED., .F., .F.,
 ( 4, 3, 3, 3, 3, 4 ),
 ( 1.127622383284612036E-17, 0.0002732102107931881564, 0.0004098135523333793113, 0.0005464168938824963233, 0.0008195847345945414921, 0.001092771384553107000 ),
 .UNSPECIFIED. ) ;
#25457 = EDGE_LOOP ( 'NONE', ( #53101, #23961, #37328, #23171 ) ) ;
#25458 = CARTESIAN_POINT ( 'NONE',  ( 0.9772918015221172539, -39.72398724205338993, -13.35446342403389863 ) ) ;
#25459 = CARTESIAN_POINT ( 'NONE',  ( 0.1103744047535531458, 34.18931094755004807, 26.28322091066887722 ) ) ;
#25460 = ADVANCED_FACE ( 'NONE', ( #59692 ), #58015, .T. ) ;
#25461 = DIRECTION ( 'NONE',  ( 0.000000000000000000, 0.000000000000000000, 1.000000000000000000 ) ) ;
#25462 = CARTESIAN_POINT ( 'NONE',  ( 0.5997462898726536595, -49.10477184366966696, 0.5225058138009974762 ) ) ;
#25463 = CARTESIAN_POINT ( 'NONE',  ( 0.1092355843206037486, 34.39511076960603475, -26.01340835034376653 ) ) ;
#25464 = EDGE_CURVE ( 'NONE', #41690, #50298, #34563, .T. ) ;
#25465 = CARTESIAN_POINT ( 'NONE',  ( 4.963659409799330291, 33.96111158240283601, -29.14784479683076412 ) ) ;
#25466 = CARTESIAN_POINT ( 'NONE',  ( 5.959547316686252039, 16.28190225198618535, -12.49803383497733122 ) ) ;
#25467 = VECTOR ( 'NONE', #37971, 1000.000000000000000 ) ;
#25468 = CARTESIAN_POINT ( 'NONE',  ( 4.549368137175248350, 0.000000000000000000, 0.000000000000000000 ) ) ;
#25469 = CARTESIAN_POINT ( 'NONE',  ( 0.5850706913938533704, 33.73916126769452006, 33.99603398296602563 ) ) ;
#25470 = AXIS2_PLACEMENT_3D ( 'NONE', #22418, #51216, #55919 ) ;
#25471 = CARTESIAN_POINT ( 'NONE',  ( 4.549368137175248350, -19.17571786012296187, -38.40568845698270195 ) ) ;
#25472 = CARTESIAN_POINT ( 'NONE',  ( 4.960386119450144626, 35.80440191906002667, -25.14918026279881502 ) ) ;
#25473 = CARTESIAN_POINT ( 'NONE',  ( 0.6001305935487315502, 44.24520387813827682, -18.89378601236018795 ) ) ;
#25474 = EDGE_CURVE ( 'NONE', #10066, #52565, #51192, .T. ) ;
#25475 = CIRCLE ( 'NONE', #30435, 5.453125000000000000 ) ;
#25476 = CARTESIAN_POINT ( 'NONE',  ( 5.895596859100789899, 14.91916793517919970, -13.48875870250514630 ) ) ;
#25477 = CARTESIAN_POINT ( 'NONE',  ( 0.6021448801613057400, 33.20790775271667172, -36.17700929200764648 ) ) ;
#25478 = CARTESIAN_POINT ( 'NONE',  ( 5.960721111146673579, -20.35079619394244332, -2.672857320903232470 ) ) ;
#25479 = ITEM_DEFINED_TRANSFORMATION ( 'NONE', 'NONE', #60903,  #14677 ) ;
#25480 = CARTESIAN_POINT ( 'NONE',  ( 4.549368137175248350, 8.582197505783829783, 42.06008734272398897 ) ) ;
#25481 = CARTESIAN_POINT ( 'NONE',  ( 0.6021447746440204973, -30.41329242676998135, 38.55609916540136339 ) ) ;
#25482 = B_SPLINE_CURVE_WITH_KNOTS ( 'NONE', 3,
 ( #20556, #44690, #40003, #48439, #44394, #823 ),
 .UNSPECIFIED., .F., .F.,
 ( 4, 2, 4 ),
 ( 1.267283937151336631E-16, 0.0002450741128632353779, 0.0004901482257263440126 ),
 .UNSPECIFIED. ) ;
#25483 = DIRECTION ( 'NONE',  ( 0.000000000000000000, 0.000000000000000000, -1.000000000000000000 ) ) ;
#25484 = CARTESIAN_POINT ( 'NONE',  ( 4.958415959904820092, -21.38448066593259966, 40.07378121005046268 ) ) ;
#25486 = VERTEX_POINT ( 'NONE', #34876 ) ;
#25485 = CARTESIAN_POINT ( 'NONE',  ( 1.088313998177381503, 10.35171213034691995, 41.64627086748857465 ) ) ;
#25487 = ORIENTED_EDGE ( 'NONE', *, *, #46578, .F. ) ;
#25488 = CARTESIAN_POINT ( 'NONE',  ( 0.1092355843206037486, -43.12343565949664992, -0.3005923759132368422 ) ) ;
#25489 = CARTESIAN_POINT ( 'NONE',  ( 3.390910168358336918, 43.71773359279901427, -4.780889670625141363 ) ) ;
#25490 = LINE ( 'NONE', #30489, #61742 ) ;
#25491 = EDGE_LOOP ( 'NONE', ( #54910, #58946, #56534, #14530 ) ) ;
#25492 = EDGE_LOOP ( 'NONE', ( #14376, #28694, #43347, #43912 ) ) ;
#25493 = CARTESIAN_POINT ( 'NONE',  ( 0.8751705887134553219, -33.37254303619578621, 34.63284514348527665 ) ) ;
#25494 = CARTESIAN_POINT ( 'NONE',  ( 0.6001305935487315502, -28.87057754790966868, 38.48510059943998129 ) ) ;
#25495 = LINE ( 'NONE', #25811, #10051 ) ;
#25496 = VERTEX_POINT ( 'NONE', #24533 ) ;
#25497 = AXIS2_PLACEMENT_3D ( 'NONE', #9241, #37791, #13657 ) ;
#25498 = ORIENTED_EDGE ( 'NONE', *, *, #22100, .T. ) ;
#25499 = CARTESIAN_POINT ( 'NONE',  ( 0.6845945791218034371, -44.58955076018962416, 14.56634764511735547 ) ) ;
#25500 = EDGE_CURVE ( 'NONE', #31192, #38487, #54173, .T. ) ;
#25501 = FACE_OUTER_BOUND ( 'NONE', #5683, .T. ) ;
#25502 = CARTESIAN_POINT ( 'NONE',  ( 4.060580049360325461, -10.26916902627464623, 42.73186003287254664 ) ) ;
#25503 = ADVANCED_FACE ( 'NONE', ( #49257 ), #44951, .F. ) ;
#25504 = EDGE_LOOP ( 'NONE', ( #60720, #15741, #29787, #10519 ) ) ;
#25505 = CARTESIAN_POINT ( 'NONE',  ( 5.895881250540457863, -2.008683229081808186, -20.01231803898555128 ) ) ;
#25506 = EDGE_CURVE ( 'NONE', #10647, #21806, #6337, .T. ) ;
#25507 = CARTESIAN_POINT ( 'NONE',  ( 0.7048096507298635682, -48.10291524268441776, 0.8437160066905670108 ) ) ;
#25508 =( BOUNDED_SURFACE ( )  B_SPLINE_SURFACE ( 3, 1, ( 
 ( #52741, #48063 ),
 ( #5114, #10152 ),
 ( #29247, #24558 ),
 ( #736, #17025 ) ),
 .UNSPECIFIED., .F., .F., .F. ) 
 B_SPLINE_SURFACE_WITH_KNOTS ( ( 4, 4 ),
 ( 2, 2 ),
 ( 0.000000000000000000, 1.000000000000000000 ),
 ( 0.000000000000000000, 1.000000000000000000 ),
 .UNSPECIFIED. ) 
 GEOMETRIC_REPRESENTATION_ITEM ( )  RATIONAL_B_SPLINE_SURFACE ( (
 ( 1.000000000000000000, 1.000000000000000000),
 ( 0.7223157951917476005, 0.9931996967497186413),
 ( 0.7223157951917476005, 0.9931996967497186413),
 ( 1.000000000000000000, 1.000000000000000000) ) ) 
 REPRESENTATION_ITEM ( '' )  SURFACE ( )  );
#25509 = CIRCLE ( 'NONE', #43529, 2.649999999999992806 ) ;
#25510 = CARTESIAN_POINT ( 'NONE',  ( 0.1129192098497455998, 4.719118110135312349, -43.87119455916086963 ) ) ;
#25511 = ORIENTED_EDGE ( 'NONE', *, *, #50476, .F. ) ;
#25512 = EDGE_CURVE ( 'NONE', #41953, #36415, #43674, .T. ) ;
#25513 = ORIENTED_EDGE ( 'NONE', *, *, #46681, .T. ) ;
#25514 = CARTESIAN_POINT ( 'NONE',  ( 4.975801465491694664, 2.564218696446817880, 47.84403947906844223 ) ) ;
#25515 = DIRECTION ( 'NONE',  ( 0.09835009131224567436, -0.9592125346408703068, -0.2650256080583726637 ) ) ;
#25516 = AXIS2_PLACEMENT_3D ( 'NONE', #6518, #16905, #26585 ) ;
#25517 = ORIENTED_EDGE ( 'NONE', *, *, #37869, .F. ) ;
#25518 = CARTESIAN_POINT ( 'NONE',  ( 0.8760168074886960365, 34.63873394077486978, -33.37827814204089805 ) ) ;
#25519 = CARTESIAN_POINT ( 'NONE',  ( 0.2940135542859015350, 37.40612138948920773, 23.38851494401085773 ) ) ;
#25520 = CARTESIAN_POINT ( 'NONE',  ( 0.8753041380234530822, -38.81339214172321306, 30.07754840949971253 ) ) ;
#25521 = DIRECTION ( 'NONE',  ( 0.09722883295013597105, 0.7627152102960371716, -0.6393841271303396523 ) ) ;
#25522 = AXIS2_PLACEMENT_3D ( 'NONE', #60631, #32161, #51241 ) ;
#25523 = VERTEX_POINT ( 'NONE', #25448 ) ;
#25524 = CARTESIAN_POINT ( 'NONE',  ( 0.2224561200757610435, 4.874377913225924175, 42.84309024201777305 ) ) ;
#25525 = VECTOR ( 'NONE', #56547, 1000.000000000000114 ) ;
#25526 = FACE_OUTER_BOUND ( 'NONE', #702, .T. ) ;
#25527 = CARTESIAN_POINT ( 'NONE',  ( 0.5806925824938502512, 43.38503874128546300, 17.80339225430713057 ) ) ;
#25528 =( BOUNDED_SURFACE ( )  B_SPLINE_SURFACE ( 3, 1, ( 
 ( #15645, #6814 ),
 ( #54122, #25641 ),
 ( #59451, #34747 ),
 ( #53817, #10947 ) ),
 .UNSPECIFIED., .F., .F., .F. ) 
 B_SPLINE_SURFACE_WITH_KNOTS ( ( 4, 4 ),
 ( 2, 2 ),
 ( 0.000000000000000000, 1.000000000000000000 ),
 ( 0.000000000000000000, 1.000000000000000000 ),
 .UNSPECIFIED. ) 
 GEOMETRIC_REPRESENTATION_ITEM ( )  RATIONAL_B_SPLINE_SURFACE ( (
 ( 1.000000000000000000, 1.000000000000000000),
 ( 0.9953040768229013402, 0.8617119497784988535),
 ( 0.9953040768229013402, 0.8617119497784988535),
 ( 1.000000000000000000, 1.000000000000000000) ) ) 
 REPRESENTATION_ITEM ( '' )  SURFACE ( )  );
#25529 = CARTESIAN_POINT ( 'NONE',  ( 5.896782393890504181, 17.94821721415859628, 9.076760749925794514 ) ) ;
#25530 = ORIENTED_EDGE ( 'NONE', *, *, #419, .F. ) ;
#25531 = CARTESIAN_POINT ( 'NONE',  ( 0.1365634738349396082, 42.07174034091315917, -13.29779246002983939 ) ) ;
#25532 = CARTESIAN_POINT ( 'NONE',  ( 0.6064515330803597060, 5.400767718514963178, 46.58504099051251046 ) ) ;
#25533 = ORIENTED_EDGE ( 'NONE', *, *, #20010, .T. ) ;
#25534 = CARTESIAN_POINT ( 'NONE',  ( 0.8557997880470599172, 33.22501220301901270, 34.51495345639560952 ) ) ;
#25535 = CARTESIAN_POINT ( 'NONE',  ( -6.016761891674565099, 16.31696541414272161, 9.424569481870310739 ) ) ;
#25536 = ADVANCED_FACE ( 'NONE', ( #16075 ), #36075, .T. ) ;
#25537 = VERTEX_POINT ( 'NONE', #6314 ) ;
#25538 = CARTESIAN_POINT ( 'NONE',  ( 0.7245667037590756143, -5.464144792999733546, 47.79072416626834752 ) ) ;
#25539 = ADVANCED_FACE ( 'NONE', ( #20159 ), #2087, .F. ) ;
#25540 = CARTESIAN_POINT ( 'NONE',  ( 0.5782707292762442330, 27.23478191391665604, 38.18380557001903242 ) ) ;
#25541 = FACE_OUTER_BOUND ( 'NONE', #9795, .T. ) ;
#25542 = ADVANCED_FACE ( 'NONE', ( #19544 ), #13042, .T. ) ;
#25543 = CARTESIAN_POINT ( 'NONE',  ( 0.5998501479064708430, -41.92175333043635987, 23.59887241503281174 ) ) ;
#25544 = CARTESIAN_POINT ( 'NONE',  ( 4.390527457369402420, 22.50004464754335487, 37.73504110885762231 ) ) ;
#25545 = CARTESIAN_POINT ( 'NONE',  ( 0.8751705887134553219, -0.8911681664085087107, -48.08707113907594533 ) ) ;
#25546 = CARTESIAN_POINT ( 'NONE',  ( 0.3622758884714600280, -10.35929834645893699, -41.85013935980099120 ) ) ;
#25547 = CARTESIAN_POINT ( 'NONE',  ( 0.6000166863083090663, 48.97316450298212942, -3.667784109282604899 ) ) ;
#25548 = CARTESIAN_POINT ( 'NONE',  ( 4.960386119450146403, 27.88794419592758445, -33.71496749512250091 ) ) ;
#25549 = CARTESIAN_POINT ( 'NONE',  ( 0.9783242366443556381, 41.49812954613101823, 5.851472838444232494 ) ) ;
#25550 = CARTESIAN_POINT ( 'NONE',  ( 0.5997462898726536595, 33.39998138387895921, -35.99990102348682797 ) ) ;
#25551 = ORIENTED_EDGE ( 'NONE', *, *, #34879, .T. ) ;
#25552 = CARTESIAN_POINT ( 'NONE',  ( -17.97369999999976642, -12.32233744059949210, 2.099999999999994760 ) ) ;
#25553 = CARTESIAN_POINT ( 'NONE',  ( -6.015611763856276717, 4.882992715191555533, -18.19956619163653500 ) ) ;
#25554 = CARTESIAN_POINT ( 'NONE',  ( 0.8744876279028306332, 48.92939099258504143, -4.032957658373305776 ) ) ;
#25555 = CARTESIAN_POINT ( 'NONE',  ( 0.1158816050234198758, 44.03314403839271307, -2.832713787046244214 ) ) ;
#25556 = EDGE_CURVE ( 'NONE', #27976, #54850, #1151, .T. ) ;
#25557 = CARTESIAN_POINT ( 'NONE',  ( 2.526464513654348654, 36.59988118252434219, -22.53107770806383314 ) ) ;
#25558 = B_SPLINE_CURVE_WITH_KNOTS ( 'NONE', 3,
 ( #15153, #34261, #45222, #44598 ),
 .UNSPECIFIED., .F., .F.,
 ( 4, 4 ),
 ( 0.000000000000000000, 0.004048833967417087357 ),
 .UNSPECIFIED. ) ;
#25559 = CARTESIAN_POINT ( 'NONE',  ( 0.1313383488274128263, -0.6377633466097591963, -43.11882601516400371 ) ) ;
#25560 = DIRECTION ( 'NONE',  ( -1.000000000000000000, -1.836909530733562683E-16, -1.836909530733589307E-16 ) ) ;
#25561 = DIRECTION ( 'NONE',  ( 0.000000000000000000, 1.000000000000000000, 0.000000000000000000 ) ) ;
#25562 = EDGE_CURVE ( 'NONE', #45047, #30775, #18377, .T. ) ;
#25563 = CARTESIAN_POINT ( 'NONE',  ( 0.5998501479064708430, -0.5236536531318284338, 48.10473956285918717 ) ) ;
#25564 = MECHANICAL_DESIGN_GEOMETRIC_PRESENTATION_REPRESENTATION (  '', ( #15564 ), #27534 ) ;
#25565 = CARTESIAN_POINT ( 'NONE',  ( 0.5848930533535030563, -19.57496322689408075, -42.61565319285041653 ) ) ;
#25567 = ORIENTED_EDGE ( 'NONE', *, *, #3108, .T. ) ;
#25566 = CARTESIAN_POINT ( 'NONE',  ( 0.5997462898726536595, 48.29911994996563607, 8.873930482212578852 ) ) ;
#25568 = VERTEX_POINT ( 'NONE', #34257 ) ;
#25569 = CARTESIAN_POINT ( 'NONE',  ( 4.975801465491695552, 2.564218696447496004, -47.84403947906841381 ) ) ;
#25570 = AXIS2_PLACEMENT_3D ( 'NONE', #38639, #33624, #29210 ) ;
#25571 = DIRECTION ( 'NONE',  ( -1.000000000000000000, -0.000000000000000000, -0.000000000000000000 ) ) ;
#25572 = CARTESIAN_POINT ( 'NONE',  ( 0.1081432562775997419, 16.11101151263768827, 40.00205417854818535 ) ) ;
#25573 = CIRCLE ( 'NONE', #36597, 43.92652462719577500 ) ;
#25574 = ORIENTED_EDGE ( 'NONE', *, *, #26383, .T. ) ;
#25575 = CARTESIAN_POINT ( 'NONE',  ( 0.1149546198390367091, -23.10744346465573429, 37.58979411424008532 ) ) ;
#25576 = FACE_OUTER_BOUND ( 'NONE', #42061, .T. ) ;
#25577 = CARTESIAN_POINT ( 'NONE',  ( 4.975801465491695552, -15.94009207553018648, -45.18341283946452336 ) ) ;
#25578 = ORIENTED_EDGE ( 'NONE', *, *, #43194, .T. ) ;
#25579 = VERTEX_POINT ( 'NONE', #53333 ) ;
#25580 = CARTESIAN_POINT ( 'NONE',  ( 0.000000000000000000, 0.000000000000000000, 0.000000000000000000 ) ) ;
#25581 = CARTESIAN_POINT ( 'NONE',  ( 0.1097557419366048670, -11.37678103520307715, -41.59672960874308245 ) ) ;
#25582 = CARTESIAN_POINT ( 'NONE',  ( 7.147292112312093160, -11.82536368408644911, -2.999999999999993339 ) ) ;
#25583 = ORIENTED_EDGE ( 'NONE', *, *, #17947, .F. ) ;
#25584 = EDGE_CURVE ( 'NONE', #46397, #14283, #16160, .T. ) ;
#25585 = EDGE_CURVE ( 'NONE', #52183, #2408, #1929, .T. ) ;
#25586 = CARTESIAN_POINT ( 'NONE',  ( 3.376099380956838925, -4.408915724533057023, 12.65977273753491517 ) ) ;
#25587 = FACE_OUTER_BOUND ( 'NONE', #27756, .T. ) ;
#25588 = ORIENTED_EDGE ( 'NONE', *, *, #49956, .F. ) ;
#25589 = CARTESIAN_POINT ( 'NONE',  ( 0.9756950546413930558, 41.42124338356092750, -11.19893879603404940 ) ) ;
#25590 = ORIENTED_EDGE ( 'NONE', *, *, #46537, .F. ) ;
#25591 = EDGE_CURVE ( 'NONE', #2327, #40973, #43019, .T. ) ;
#25592 = EDGE_CURVE ( 'NONE', #23847, #27695, #10444, .T. ) ;
#25593 = FACE_OUTER_BOUND ( 'NONE', #20732, .T. ) ;
#25594 = CARTESIAN_POINT ( 'NONE',  ( 5.860006189529246790, -45.67886430272042020, 15.48781697582032102 ) ) ;
#25595 = B_SPLINE_CURVE_WITH_KNOTS ( 'NONE', 3,
 ( #25563, #6422, #34992, #15874, #15563, #10548, #34670, #48756, #11172, #52839 ),
 .UNSPECIFIED., .F., .F.,
 ( 4, 3, 3, 4 ),
 ( 2.027574016683678720E-17, 0.0002618515315864106976, 0.0003927756766341516958, 0.0005236741812378729226 ),
 .UNSPECIFIED. ) ;
#25596 = VERTEX_POINT ( 'NONE', #12931 ) ;
#25597 = EDGE_CURVE ( 'NONE', #13939, #40478, #13172, .T. ) ;
#25598 = CARTESIAN_POINT ( 'NONE',  ( 0.5806925824938494740, -19.24316026636509136, 42.76591101925167493 ) ) ;
#25599 = CARTESIAN_POINT ( 'NONE',  ( 0.5832366564991507962, 41.34220239954017728, -24.18352361336783929 ) ) ;
#25600 = CARTESIAN_POINT ( 'NONE',  ( 4.999999999999983125, 80.00000000000001421, 2.649999999999999467 ) ) ;
#25601 = ORIENTED_EDGE ( 'NONE', *, *, #39998, .F. ) ;
#25602 = CARTESIAN_POINT ( 'NONE',  ( 4.691466044806103852, 8.371234562541850721, -43.79545162262300551 ) ) ;
#25603 = CARTESIAN_POINT ( 'NONE',  ( 0.6064515330803564863, -19.09368311036443799, 42.83416395026369372 ) ) ;
#25604 = VERTEX_POINT ( 'NONE', #26079 ) ;
#25605 = CARTESIAN_POINT ( 'NONE',  ( 0.1064266379913942906, 21.07422113734163460, -37.62465837278053726 ) ) ;
#25606 = EDGE_CURVE ( 'NONE', #14390, #4686, #35585, .T. ) ;
#25607 = VERTEX_POINT ( 'NONE', #6945 ) ;
#25608 = CARTESIAN_POINT ( 'NONE',  ( 0.9785694773339246311, 3.973364312730550019, 41.71987274372960997 ) ) ;
#25609 = ORIENTED_EDGE ( 'NONE', *, *, #33336, .T. ) ;
#25610 = CARTESIAN_POINT ( 'NONE',  ( 4.549368137175248350, 0.000000000000000000, 0.000000000000000000 ) ) ;
#25611 = CARTESIAN_POINT ( 'NONE',  ( -1.500000000000000444, 5.453125000000000000, 0.000000000000000000 ) ) ;
#25612 = B_SPLINE_CURVE_WITH_KNOTS ( 'NONE', 3,
 ( #24153, #47064, #23537, #9130, #18238, #47977 ),
 .UNSPECIFIED., .F., .F.,
 ( 4, 2, 4 ),
 ( 8.673136251825839020E-17, 0.0002293366620881421387, 0.0004586733241761975412 ),
 .UNSPECIFIED. ) ;
#25613 = CONICAL_SURFACE ( 'NONE', #9645, 5.612499999999999822, 0.4883339510564123076 ) ;
#25614 = CARTESIAN_POINT ( 'NONE',  ( 0.9730545539215883499, 33.73144377768558400, 26.52009130076782739 ) ) ;
#25615 = ORIENTED_EDGE ( 'NONE', *, *, #7612, .F. ) ;
#25616 = CARTESIAN_POINT ( 'NONE',  ( 4.963659409799330291, -8.262218268420788547, 43.98510776953406776 ) ) ;
#25617 = CARTESIAN_POINT ( 'NONE',  ( -6.015611763856276717, 17.40650793417844255, 7.216738110653344584 ) ) ;
#25618 = CARTESIAN_POINT ( 'NONE',  ( 4.694002226626920127, 42.12595566887542020, -17.42666435179369344 ) ) ;
#25619 = AXIS2_PLACEMENT_3D ( 'NONE', #24335, #43466, #19964 ) ;
#25620 = ORIENTED_EDGE ( 'NONE', *, *, #58020, .F. ) ;
#25621 = ORIENTED_EDGE ( 'NONE', *, *, #17586, .T. ) ;
#25622 = CARTESIAN_POINT ( 'NONE',  ( 0.5832367798473389042, 18.07699868820190048, 44.35360901387653598 ) ) ;
#25623 = CARTESIAN_POINT ( 'NONE',  ( 1.657374760986086271, 30.52321381783924892, 31.76828395558549545 ) ) ;
#25624 = CARTESIAN_POINT ( 'NONE',  ( 0.9730545539215883499, 34.34678117142556175, 25.71816799638790840 ) ) ;
#25625 = DIRECTION ( 'NONE',  ( -0.07836865515943411409, 0.7860872967108267773, -0.6131273243286146091 ) ) ;
#25626 = CARTESIAN_POINT ( 'NONE',  ( 0.3622758884714600280, 29.89648521331588071, 31.06363466427737663 ) ) ;
#25627 = CARTESIAN_POINT ( 'NONE',  ( 0.1129192098497447394, -42.55567333040724520, 11.66046547873710537 ) ) ;
#25628 = EDGE_LOOP ( 'NONE', ( #45809, #28388, #48215, #16410, #8090, #30763 ) ) ;
#25629 = LINE ( 'NONE', #34128, #61672 ) ;
#25630 = CARTESIAN_POINT ( 'NONE',  ( 4.956445790444004906, -46.59545590650544966, 6.811867512257108181 ) ) ;
#25631 = ORIENTED_EDGE ( 'NONE', *, *, #19826, .T. ) ;
#25632 = CARTESIAN_POINT ( 'NONE',  ( 0.7048096507298579061, -28.61383451045671222, -38.67623024744037963 ) ) ;
#25633 = CARTESIAN_POINT ( 'NONE',  ( -4.000000000000000000, -1.549102112939103826, -5.442104661404060906 ) ) ;
#25634 = CARTESIAN_POINT ( 'NONE',  ( 0.1129192098497455998, -38.20615368646939203, -22.07354996984027196 ) ) ;
#25635 = EDGE_CURVE ( 'NONE', #31335, #23849, #13079, .T. ) ;
#25636 = CARTESIAN_POINT ( 'NONE',  ( 5.958863334805807099, -18.96276366205799135, 7.855954700275283642 ) ) ;
#25637 = FACE_OUTER_BOUND ( 'NONE', #25275, .T. ) ;
#25638 = CARTESIAN_POINT ( 'NONE',  ( 5.895596859100789899, -17.30333226730972385, -10.25294473112801619 ) ) ;
#25639 = EDGE_CURVE ( 'NONE', #31520, #57605, #9027, .T. ) ;
#25640 = CARTESIAN_POINT ( 'NONE',  ( 0.6016118706126977189, 37.61760366456271498, -31.56686473693274309 ) ) ;
#25641 = CARTESIAN_POINT ( 'NONE',  ( 0.5980894510889448457, 44.71414919659906673, -17.76188940524901838 ) ) ;
#25642 = CARTESIAN_POINT ( 'NONE',  ( 0.1152339509894530906, 29.82972479065796634, 32.51353886258534942 ) ) ;
#25643 = DIRECTION ( 'NONE',  ( 0.1024043820194936311, 0.8548216096550996790, -0.5087173657443492258 ) ) ;
#25644 = CYLINDRICAL_SURFACE ( 'NONE', #34253, 2.649999999999992806 ) ;
#25645 = CARTESIAN_POINT ( 'NONE',  ( 0.9785694773339252972, 9.498626739178066103, 40.81802905315790753 ) ) ;
#25646 = CARTESIAN_POINT ( 'NONE',  ( 0.1129192098497447394, -6.563350895509266536, 43.63340707310824484 ) ) ;
#25647 = CARTESIAN_POINT ( 'NONE',  ( 0.5807400328401574052, 47.89582301953903709, -0.5448834511091605881 ) ) ;
#25648 = CARTESIAN_POINT ( 'NONE',  ( -17.97369999999976642, 0.000000000000000000, -2.099999999999997424 ) ) ;
#25649 = ORIENTED_EDGE ( 'NONE', *, *, #33587, .T. ) ;
#25650 = AXIS2_PLACEMENT_3D ( 'NONE', #7885, #46131, #22306 ) ;
#25651 = CYLINDRICAL_SURFACE ( 'NONE', #34345, 15.14599999999999369 ) ;
#25652 = CARTESIAN_POINT ( 'NONE',  ( 0.5800708057587377064, 5.628966369369036826, 47.56394202401740046 ) ) ;
#25653 = AXIS2_PLACEMENT_3D ( 'NONE', #32092, #45577, #21755 ) ;
#25654 = CARTESIAN_POINT ( 'NONE',  ( 0.9730545539215883499, -39.83279466599027785, -15.95224156741871546 ) ) ;
#25655 = CARTESIAN_POINT ( 'NONE',  ( 5.894904586330512508, -13.98322986223381470, 14.45678714934875053 ) ) ;
#25656 = CARTESIAN_POINT ( 'NONE',  ( 2.299746137290199943, -6.551208167574801955, 48.59385773152035881 ) ) ;
#25657 = VECTOR ( 'NONE', #41139, 1000.000000000000000 ) ;
#25658 = EDGE_LOOP ( 'NONE', ( #57363, #14198 ) ) ;
#25659 = CARTESIAN_POINT ( 'NONE',  ( 5.960721111146673579, 16.28787783074227136, -12.49016043756454231 ) ) ;
#25660 = DIRECTION ( 'NONE',  ( 0.000000000000000000, 0.000000000000000000, 1.000000000000000000 ) ) ;
#25661 = B_SPLINE_CURVE_WITH_KNOTS ( 'NONE', 3,
 ( #33672, #22721, #13334, #41854, #28040, #32436, #60919, #46859, #37150, #61525, #4201, #8602, #52139, #27730, #3899, #42168 ),
 .UNSPECIFIED., .F., .F.,
 ( 4, 3, 3, 3, 3, 4 ),
 ( 1.551621725782133898E-17, 0.0002732102107931864759, 0.0004098135523333695535, 0.0005464168938824849392, 0.0008195847345945289153, 0.001092771384553104831 ),
 .UNSPECIFIED. ) ;
#25662 = EDGE_CURVE ( 'NONE', #8307, #37892, #7134, .T. ) ;
#25663 = CARTESIAN_POINT ( 'NONE',  ( 4.975801465491694664, 43.22084481528220579, -20.67815041659094888 ) ) ;
#25664 = ORIENTED_EDGE ( 'NONE', *, *, #14511, .F. ) ;
#25665 = CARTESIAN_POINT ( 'NONE',  ( 2.533389852662419894, -43.98803057297956798, 1.582307822211680870 ) ) ;
#25666 = EDGE_CURVE ( 'NONE', #34543, #39132, #37818, .T. ) ;
#25667 = CARTESIAN_POINT ( 'NONE',  ( 3.238741278300273141, 41.01623499585995347, 12.88350628398754516 ) ) ;
#25668 = EDGE_LOOP ( 'NONE', ( #26230, #7546, #33240, #43530 ) ) ;
#25669 = AXIS2_PLACEMENT_3D ( 'NONE', #15727, #34833, #11024 ) ;
#25670 = ADVANCED_FACE ( 'NONE', ( #50498 ), #3368, .F. ) ;
#25671 = CARTESIAN_POINT ( 'NONE',  ( 5.200000000000002842, 0.000000000000000000, 0.000000000000000000 ) ) ;
#25672 = ORIENTED_EDGE ( 'NONE', *, *, #10296, .F. ) ;
#25673 = EDGE_CURVE ( 'NONE', #129, #52874, #28019, .T. ) ;
#25674 = ORIENTED_EDGE ( 'NONE', *, *, #20809, .F. ) ;
#25675 = DIRECTION ( 'NONE',  ( 0.000000000000000000, 0.7071067811865540120, -0.7071067811865409114 ) ) ;
#25676 = ORIENTED_EDGE ( 'NONE', *, *, #42881, .T. ) ;
#25677 = AXIS2_PLACEMENT_3D ( 'NONE', #43790, #24650, #15262 ) ;
#25678 = ORIENTED_EDGE ( 'NONE', *, *, #52302, .F. ) ;
#25679 = B_SPLINE_CURVE_WITH_KNOTS ( 'NONE', 3,
 ( #10215, #29931, #44073, #29311 ),
 .UNSPECIFIED., .F., .F.,
 ( 4, 4 ),
 ( 0.000000000000000000, 0.005014147105413694315 ),
 .UNSPECIFIED. ) ;
#25680 = CARTESIAN_POINT ( 'NONE',  ( 0.6845945791218034371, -38.17654861005505040, -27.25724962167035414 ) ) ;
#25681 = B_SPLINE_CURVE_WITH_KNOTS ( 'NONE', 3,
 ( #5869, #54104, #15625, #1187, #20321, #24706, #11535, #34423, #15930, #38828, #39441, #34122, #58494, #34733, #49423, #10299, #16233, #25016, #6479 ),
 .UNSPECIFIED., .F., .F.,
 ( 4, 3, 3, 3, 3, 3, 4 ),
 ( 9.813676791237319219E-18, 0.0002732106629380673651, 0.0004098138914053816120, 0.0005464171197651560138, 0.0006830203481512717037, 0.0008196235766963805465, 0.001011968216111141161 ),
 .UNSPECIFIED. ) ;
#25682 = FACE_OUTER_BOUND ( 'NONE', #79, .T. ) ;
#25683 = B_SPLINE_CURVE_WITH_KNOTS ( 'NONE', 3,
 ( #58431, #15555, #20865, #34662 ),
 .UNSPECIFIED., .F., .F.,
 ( 4, 4 ),
 ( 0.000000000000000000, 0.004447772540403830202 ),
 .UNSPECIFIED. ) ;
#25684 = ORIENTED_EDGE ( 'NONE', *, *, #47769, .F. ) ;
#25685 = VERTEX_POINT ( 'NONE', #23237 ) ;
#25686 = CARTESIAN_POINT ( 'NONE',  ( 0.5804410086790514622, -8.338934868870362394, -46.15172821366644484 ) ) ;
#25687 = CARTESIAN_POINT ( 'NONE',  ( 0.9730545539215883499, -39.83279466599050522, 15.95224156741815236 ) ) ;
#25688 = EDGE_CURVE ( 'NONE', #16902, #5739, #42247, .T. ) ;
#25689 = CARTESIAN_POINT ( 'NONE',  ( 0.7056759521545044045, -34.21343630614968845, -32.08098510398369996 ) ) ;
#25690 = CARTESIAN_POINT ( 'NONE',  ( 4.549368137175248350, 35.57418903283081590, 24.02461520945284690 ) ) ;
#25691 = ORIENTED_EDGE ( 'NONE', *, *, #20960, .F. ) ;
#25692 = CARTESIAN_POINT ( 'NONE',  ( 0.6000166863083090663, 46.77044519531211364, 14.97828220927751630 ) ) ;
#25693 = EDGE_CURVE ( 'NONE', #61173, #49729, #16823, .T. ) ;
#25694 = CARTESIAN_POINT ( 'NONE',  ( -6.057079549204054558, 16.78313491342520436, -9.442330939842472404 ) ) ;
#25695 = ORIENTED_EDGE ( 'NONE', *, *, #50559, .F. ) ;
#25696 = CARTESIAN_POINT ( 'NONE',  ( 0.8557997880470599172, 41.93815086860288943, -23.15977007032279289 ) ) ;
#25697 = ORIENTED_EDGE ( 'NONE', *, *, #4438, .T. ) ;
#25698 = CARTESIAN_POINT ( 'NONE',  ( 4.956653778116968390, 48.02038484091101367, -2.599733001514498376 ) ) ;
#25699 = CARTESIAN_POINT ( 'NONE',  ( 4.967162193818130511, 19.45289607368822615, 38.44485641567079881 ) ) ;
#25700 = VERTEX_POINT ( 'NONE', #28534 ) ;
#25701 = CARTESIAN_POINT ( 'NONE',  ( 0.5806925824938511393, 5.237374507879287044, 46.60249210726590263 ) ) ;
#25702 = CARTESIAN_POINT ( 'NONE',  ( 3.782625744892853525, -36.71075882237605015, 20.48312209552882379 ) ) ;
#25703 = PLANE ( 'NONE',  #58678 ) ;
#25704 = CARTESIAN_POINT ( 'NONE',  ( 0.8744876279028263033, 46.30617036199606673, 16.31222353896886545 ) ) ;
#25705 = CIRCLE ( 'NONE', #60692, 47.09074272231896430 ) ;
#25706 = AXIS2_PLACEMENT_3D ( 'NONE', #37126, #51485, #22078 ) ;
#25707 = ORIENTED_EDGE ( 'NONE', *, *, #29655, .F. ) ;
#25708 = LINE ( 'NONE', #2505, #21956 ) ;
#25709 = ORIENTED_EDGE ( 'NONE', *, *, #40714, .F. ) ;
#25710 = B_SPLINE_CURVE_WITH_KNOTS ( 'NONE', 3,
 ( #40727, #60101, #45417, #54457 ),
 .UNSPECIFIED., .F., .F.,
 ( 4, 4 ),
 ( 2.294131830766625192E-17, 0.004564976165746188579 ),
 .UNSPECIFIED. ) ;
#25711 = DIRECTION ( 'NONE',  ( -0.1736481776669316357, 0.9848077530122079093, -5.551115123125819680E-17 ) ) ;
#25712 = CARTESIAN_POINT ( 'NONE',  ( 0.5800708057587394828, -5.628966369368725076, -47.56394202401742888 ) ) ;
#25713 = SURFACE_STYLE_USAGE ( .BOTH. , #16954 ) ;
#25714 = CARTESIAN_POINT ( 'NONE',  ( 0.9762797500689124330, 20.58271139965489738, 36.50584578699993443 ) ) ;
#25715 =( BOUNDED_SURFACE ( )  B_SPLINE_SURFACE ( 3, 1, ( 
 ( #15792, #39610 ),
 ( #35212, #58663 ),
 ( #21403, #49282 ),
 ( #11392, #45537 ) ),
 .UNSPECIFIED., .F., .F., .F. ) 
 B_SPLINE_SURFACE_WITH_KNOTS ( ( 4, 4 ),
 ( 2, 2 ),
 ( 0.000000000000000000, 1.000000000000000000 ),
 ( 0.000000000000000000, 1.000000000000000000 ),
 .UNSPECIFIED. ) 
 GEOMETRIC_REPRESENTATION_ITEM ( )  RATIONAL_B_SPLINE_SURFACE ( (
 ( 1.000000000000000000, 1.000000000000000000),
 ( 0.7223157951917480446, 0.9931996967497186413),
 ( 0.7223157951917480446, 0.9931996967497186413),
 ( 1.000000000000000000, 1.000000000000000000) ) ) 
 REPRESENTATION_ITEM ( '' )  SURFACE ( )  );
#25716 = EDGE_CURVE ( 'NONE', #61884, #5803, #56114, .T. ) ;
#25717 = CARTESIAN_POINT ( 'NONE',  ( 0.000000000000000000, 0.000000000000000000, -5.600000000000000533 ) ) ;
#25718 = CARTESIAN_POINT ( 'NONE',  ( -6.078457390727109555, 18.62514245781363798, 4.888617336594847096 ) ) ;
#25719 = CARTESIAN_POINT ( 'NONE',  ( 0.5997462898726536595, 22.24958391914503153, 43.77793560195857481 ) ) ;
#25720 = DIRECTION ( 'NONE',  ( 0.07836865515943411409, 0.9240274869783812184, -0.3742079063794873650 ) ) ;
#25721 = CARTESIAN_POINT ( 'NONE',  ( 0.1129192098497447394, -27.13044910148925837, 34.79785222304180081 ) ) ;
#25722 = DIRECTION ( 'NONE',  ( -1.000000000000000000, -1.836909530733573776E-16, -1.361838123766432833E-32 ) ) ;
#25723 = CARTESIAN_POINT ( 'NONE',  ( 0.1129192098497447394, -43.69739906996321110, 6.122834499276631703 ) ) ;
#25724 = B_SPLINE_CURVE_WITH_KNOTS ( 'NONE', 3,
 ( #60066, #11871, #50060, #40689 ),
 .UNSPECIFIED., .F., .F.,
 ( 4, 4 ),
 ( 1.734723475976807094E-18, 0.004050076154993002484 ),
 .UNSPECIFIED. ) ;
#25725 = B_SPLINE_CURVE_WITH_KNOTS ( 'NONE', 3,
 ( #52718, #33946, #53025, #10125, #33637, #9499 ),
 .UNSPECIFIED., .F., .F.,
 ( 4, 2, 4 ),
 ( 1.571494855748036957E-17, 0.0002448709889506572109, 0.0004897419779012987008 ),
 .UNSPECIFIED. ) ;
#25726 = FACE_OUTER_BOUND ( 'NONE', #5243, .T. ) ;
#25727 = CARTESIAN_POINT ( 'NONE',  ( 0.6029442701453591180, -45.48579272903533166, 18.50912977342572319 ) ) ;
#25728 = ORIENTED_EDGE ( 'NONE', *, *, #26667, .F. ) ;
#25729 = CARTESIAN_POINT ( 'NONE',  ( 2.185380717157383135, -2.848313382796944015, -43.93981012636012196 ) ) ;
#25730 = CARTESIAN_POINT ( 'NONE',  ( -6.016489644550737204, 18.68257207665199715, -2.455165042129548336 ) ) ;
#25731 = CARTESIAN_POINT ( 'NONE',  ( 2.879087469061463178, -42.08991748084939388, 12.82733500142047944 ) ) ;
#25732 = ORIENTED_EDGE ( 'NONE', *, *, #49940, .F. ) ;
#25733 = DIRECTION ( 'NONE',  ( -1.000000000000000000, -1.836909530733554547E-16, -1.836909530733573529E-16 ) ) ;
#25734 = CARTESIAN_POINT ( 'NONE',  ( 3.238018933889920792, 13.23534742317154134, -2.057442819521235311 ) ) ;
#25735 = CARTESIAN_POINT ( 'NONE',  ( 0.6031357023905875581, -12.40899271757806765, -46.47951061918806204 ) ) ;
#25736 = ORIENTED_EDGE ( 'NONE', *, *, #11743, .F. ) ;
#25737 = CARTESIAN_POINT ( 'NONE',  ( 5.974727161628367256, 12.50710176109986094, 16.27409205901379963 ) ) ;
#25738 = CARTESIAN_POINT ( 'NONE',  ( 0.8551540677456715978, -13.28067116677234694, 46.03951182599423930 ) ) ;
#25739 = ADVANCED_FACE ( 'NONE', ( #47658 ), #16569, .F. ) ;
#25740 = AXIS2_PLACEMENT_3D ( 'NONE', #34898, #34276, #1043 ) ;
#25741 = ORIENTED_EDGE ( 'NONE', *, *, #32462, .T. ) ;
#25742 = CARTESIAN_POINT ( 'NONE',  ( 0.8551540677456715978, -29.88829867897790038, -37.45266983663525906 ) ) ;
#25743 = AXIS2_PLACEMENT_3D ( 'NONE', #19542, #29226, #52721 ) ;
#25744 = AXIS2_PLACEMENT_3D ( 'NONE', #9943, #61908, #52216 ) ;
#25745 = ORIENTED_EDGE ( 'NONE', *, *, #7708, .T. ) ;
#25746 = EDGE_CURVE ( 'NONE', #40034, #41417, #1784, .T. ) ;
#25747 = VERTEX_POINT ( 'NONE', #22547 ) ;
#25748 = CARTESIAN_POINT ( 'NONE',  ( 0.1095718737110178281, 10.91304379105004330, 41.72082389913620659 ) ) ;
#25749 = ORIENTED_EDGE ( 'NONE', *, *, #20376, .F. ) ;
#25750 = CARTESIAN_POINT ( 'NONE',  ( 3.238018933889920792, -13.34321331060664839, -1.168824587054275943 ) ) ;
#25751 = B_SPLINE_CURVE_WITH_KNOTS ( 'NONE', 3,
 ( #60620, #8626, #60943, #51535, #18054, #21819, #12426, #13669, #22430, #27132, #22123, #31842, #3920, #3301, #55934, #45636 ),
 .UNSPECIFIED., .F., .F.,
 ( 4, 3, 3, 3, 3, 4 ),
 ( 1.868480190406682863E-17, 0.0002618515315864432236, 0.0003927756766342012438, 0.0005236998216950576731, 0.0007855159896329925008, 0.001047349442285930472 ),
 .UNSPECIFIED. ) ;
#25752 = CARTESIAN_POINT ( 'NONE',  ( 0.5997462898726536595, 46.76781179977627545, -14.97743000668059210 ) ) ;
#25753 = ORIENTED_EDGE ( 'NONE', *, *, #6333, .T. ) ;
#25754 = CARTESIAN_POINT ( 'NONE',  ( 0.1103936448916694457, -6.269440624735986453E-17, 43.12443171339902648 ) ) ;
#25755 = B_SPLINE_CURVE_WITH_KNOTS ( 'NONE', 3,
 ( #8245, #22991, #46491, #16743 ),
 .UNSPECIFIED., .F., .F.,
 ( 4, 4 ),
 ( 0.000000000000000000, 0.004442905043737216571 ),
 .UNSPECIFIED. ) ;
#25756 = CARTESIAN_POINT ( 'NONE',  ( -6.016761891674565099, 2.462934516564073917, -18.68153697670638991 ) ) ;
#25757 = VERTEX_POINT ( 'NONE', #37588 ) ;
#25758 = CARTESIAN_POINT ( 'NONE',  ( 0.3676999524040323597, 34.11874447325018167, -27.96179284115914854 ) ) ;
#25759 = EDGE_CURVE ( 'NONE', #32445, #25918, #15243, .T. ) ;
#25760 = CARTESIAN_POINT ( 'NONE',  ( 0.9754292580325130135, 14.51724361431902999, 39.31382841630305336 ) ) ;
#25761 = CARTESIAN_POINT ( 'NONE',  ( 0.000000000000000000, 0.000000000000000000, 0.000000000000000000 ) ) ;
#25762 = CARTESIAN_POINT ( 'NONE',  ( 4.956445790443988031, 46.25174887658550915, 8.849507104743643993 ) ) ;
#25763 = EDGE_LOOP ( 'NONE', ( #60145, #60234, #54932, #33828 ) ) ;
#25764 = EDGE_CURVE ( 'NONE', #12356, #23235, #19027, .T. ) ;
#25765 = ORIENTED_EDGE ( 'NONE', *, *, #13882, .T. ) ;
#25766 = VECTOR ( 'NONE', #24321, 1000.000000000000000 ) ;
#25767 = CARTESIAN_POINT ( 'NONE',  ( 0.1073791018717578927, 41.52698815987152159, 11.62916352156164557 ) ) ;
#25768 = CARTESIAN_POINT ( 'NONE',  ( 0.7044674535452954967, 48.03641533699654076, 10.21300760708961164 ) ) ;
#25769 = CARTESIAN_POINT ( 'NONE',  ( 0.2885697896453112143, -41.84838128162066795, 10.38006191081347218 ) ) ;
#25770 = VERTEX_POINT ( 'NONE', #55725 ) ;
#25771 = CARTESIAN_POINT ( 'NONE',  ( 3.390910168358337362, -42.99706393720556008, -9.238486310727259010 ) ) ;
#25772 = CARTESIAN_POINT ( 'NONE',  ( 4.291220156522059348, 6.853930411218122742, -46.60914754877926924 ) ) ;
#25773 = CARTESIAN_POINT ( 'NONE',  ( 0.7242486021783859362, 46.33600717073790065, 16.24764296282079457 ) ) ;
#25774 =( LENGTH_UNIT ( ) NAMED_UNIT ( * ) SI_UNIT ( .MILLI., .METRE. ) );
#25775 = ORIENTED_EDGE ( 'NONE', *, *, #35163, .T. ) ;
#25776 = B_SPLINE_CURVE_WITH_KNOTS ( 'NONE', 3,
 ( #25787, #16391, #1964, #17323 ),
 .UNSPECIFIED., .F., .F.,
 ( 4, 4 ),
 ( 6.938893903907228378E-18, 0.005014147105413696050 ),
 .UNSPECIFIED. ) ;
#25777 = VERTEX_POINT ( 'NONE', #55417 ) ;
#25778 = CARTESIAN_POINT ( 'NONE',  ( 4.975801465491695552, 20.67815041659141784, -43.22084481528199973 ) ) ;
#25779 = CARTESIAN_POINT ( 'NONE',  ( 0.1095718737110178281, 34.05592812063346031, 26.45591486700768513 ) ) ;
#25780 = CARTESIAN_POINT ( 'NONE',  ( 0.9730545539215892381, -15.95224156741857691, 39.83279466599033469 ) ) ;
#25781 = CARTESIAN_POINT ( 'NONE',  ( 4.956445790443989807, 44.30493387627029733, 15.95653108789479191 ) ) ;
#25782 = CARTESIAN_POINT ( 'NONE',  ( 0.1073791018717483448, -43.12183934961191056, 0.4849339620931858996 ) ) ;
#25783 = CARTESIAN_POINT ( 'NONE',  ( 4.226256110419178924, -43.20794779182517686, 7.993778681330654834 ) ) ;
#25784 = EDGE_CURVE ( 'NONE', #30302, #59869, #29492, .T. ) ;
#25785 = CARTESIAN_POINT ( 'NONE',  ( 0.5549461598389366923, -13.38796976693469531, -42.02356435366290555 ) ) ;
#25786 = LINE ( 'NONE', #7588, #13243 ) ;
#25787 = CARTESIAN_POINT ( 'NONE',  ( 4.975801465491694664, -20.67815041659109809, -43.22084481528213473 ) ) ;
#25788 =( BOUNDED_SURFACE ( )  B_SPLINE_SURFACE ( 3, 1, ( 
 ( #57005, #43559 ),
 ( #10031, #4362 ),
 ( #53228, #33229 ),
 ( #52301, #33852 ) ),
 .UNSPECIFIED., .F., .F., .F. ) 
 B_SPLINE_SURFACE_WITH_KNOTS ( ( 4, 4 ),
 ( 2, 2 ),
 ( 0.000000000000000000, 1.000000000000000000 ),
 ( 0.000000000000000000, 1.000000000000000000 ),
 .UNSPECIFIED. ) 
 GEOMETRIC_REPRESENTATION_ITEM ( )  RATIONAL_B_SPLINE_SURFACE ( (
 ( 1.000000000000000000, 1.000000000000000000),
 ( 0.9729067724841187204, 0.9999501103223794596),
 ( 0.9729067724841187204, 0.9999501103223794596),
 ( 1.000000000000000000, 1.000000000000000000) ) ) 
 REPRESENTATION_ITEM ( '' )  SURFACE ( )  );
#25789 = CARTESIAN_POINT ( 'NONE',  ( 2.624215991343620935, 4.864192649746072128, -47.76052319582212391 ) ) ;
#25790 = AXIS2_PLACEMENT_3D ( 'NONE', #30396, #54498, #44234 ) ;
#25791 = CYLINDRICAL_SURFACE ( 'NONE', #51920, 10.00000000000000711 ) ;
#25792 = FACE_OUTER_BOUND ( 'NONE', #48378, .T. ) ;
#25793 = CARTESIAN_POINT ( 'NONE',  ( 1.479689385636123067, 41.43333151104896217, -14.99542880891405083 ) ) ;
#25794 = CARTESIAN_POINT ( 'NONE',  ( 3.678834586032787790, 9.087502264074171165, 48.12514594501299570 ) ) ;
#25795 = CARTESIAN_POINT ( 'NONE',  ( 0.5809828226811617480, 0.5448590168539207967, -47.89273459658652854 ) ) ;
#25796 = CARTESIAN_POINT ( 'NONE',  ( 0.5998501479064699549, -6.798102206413803472, -47.62484632993685807 ) ) ;
#25797 = CARTESIAN_POINT ( 'NONE',  ( 0.7044674535452954967, 11.74740322167666307, -47.68439199946085694 ) ) ;
#25798 = B_SPLINE_CURVE_WITH_KNOTS ( 'NONE', 3,
 ( #22255, #37287, #22559, #41377 ),
 .UNSPECIFIED., .F., .F.,
 ( 4, 4 ),
 ( 0.000000000000000000, 0.004444103432399265294 ),
 .UNSPECIFIED. ) ;
#25799 = CARTESIAN_POINT ( 'NONE',  ( -6.015611763856276717, -4.882992715191171840, -18.19956619163663447 ) ) ;
#25800 = CARTESIAN_POINT ( 'NONE',  ( 5.959547316686252039, 10.25972575517505270, 17.77749189599220969 ) ) ;
#25802 = EDGE_LOOP ( 'NONE', ( #26462, #25620, #34322, #25421 ) ) ;
#25801 = DIRECTION ( 'NONE',  ( 0.000000000000000000, 0.000000000000000000, 1.000000000000000000 ) ) ;
#25803 = ORIENTED_EDGE ( 'NONE', *, *, #37511, .F. ) ;
#25804 = CIRCLE ( 'NONE', #39843, 2.649999999999997691 ) ;
#25805 = DIRECTION ( 'NONE',  ( -0.07906939808003035641, -0.6374189498685002286, 0.7664496804329689050 ) ) ;
#25806 = CARTESIAN_POINT ( 'NONE',  ( 4.553261556744875094, 43.59419396814060832, -5.393126930804686303 ) ) ;
#25807 = CARTESIAN_POINT ( 'NONE',  ( 1.157643937452369487, -34.08380114724293009, 24.39870434982061553 ) ) ;
#25808 = ORIENTED_EDGE ( 'NONE', *, *, #53010, .T. ) ;
#25809 = ORIENTED_EDGE ( 'NONE', *, *, #45490, .T. ) ;
#25810 = CARTESIAN_POINT ( 'NONE',  ( 4.549368137175248350, 42.14271863032833920, -8.166781970325278195 ) ) ;
#25811 = CARTESIAN_POINT ( 'NONE',  ( -2.601141883200662974, 4.732256851928817731, -14.15631211003633716 ) ) ;
#25812 = AXIS2_PLACEMENT_3D ( 'NONE', #26786, #41524, #7983 ) ;
#25813 = ORIENTED_EDGE ( 'NONE', *, *, #15789, .T. ) ;
#25814 = EDGE_LOOP ( 'NONE', ( #34035, #9295 ) ) ;
#25815 = CARTESIAN_POINT ( 'NONE',  ( -6.077587904424778920, -18.90214787454603851, -3.674891443665424973 ) ) ;
#25816 = ADVANCED_FACE ( 'NONE', ( #9052 ), #39834, .F. ) ;
#25817 = CARTESIAN_POINT ( 'NONE',  ( 3.660087539127330203, -47.83637163185225205, -4.399983418616626452 ) ) ;
#25818 = CARTESIAN_POINT ( 'NONE',  ( 0.5806925824938499181, -38.35106547415185929, -26.98922265166007861 ) ) ;
#25819 = ADVANCED_FACE ( 'NONE', ( #8421 ), #8047, .F. ) ;
#25820 = EDGE_LOOP ( 'NONE', ( #29585, #51095, #61820, #8666 ) ) ;
#25821 = CARTESIAN_POINT ( 'NONE',  ( 4.956653778116975495, 14.93973939759886704, 45.71126949320255761 ) ) ;
#25822 = ADVANCED_BREP_SHAPE_REPRESENTATION ( '', ( #10540, #14677 ), #46738 ) ;
#25823 = DIRECTION ( 'NONE',  ( -1.000000000000000000, -1.836909530733573776E-16, 1.925929944387234758E-32 ) ) ;
#25824 = ADVANCED_FACE ( 'NONE', ( #17233 ), #61364, .F. ) ;
#25825 = CARTESIAN_POINT ( 'NONE',  ( 0.5998501479064699549, -24.50586714782575726, -41.39809967730479201 ) ) ;
#25826 = ORIENTED_EDGE ( 'NONE', *, *, #38865, .T. ) ;
#25827 = CIRCLE ( 'NONE', #43889, 2.649999999999999467 ) ;
#25828 = VERTEX_POINT ( 'NONE', #32570 ) ;
#25829 = CARTESIAN_POINT ( 'NONE',  ( 0.6064782688330874194, 27.24299735947540313, 38.17268056202479443 ) ) ;
#25830 = CARTESIAN_POINT ( 'NONE',  ( 4.962356264823608143, -29.56943756613123497, 29.94802096775367772 ) ) ;
#25831 = AXIS2_PLACEMENT_3D ( 'NONE', #33761, #4584, #18728 ) ;
#25832 = ORIENTED_EDGE ( 'NONE', *, *, #24907, .T. ) ;
#25833 = CARTESIAN_POINT ( 'NONE',  ( 3.660176727303418698, 42.51126973288313593, -22.37119938028445176 ) ) ;
#25834 = CARTESIAN_POINT ( 'NONE',  ( 0.1119898979215346868, 37.28332023458525413, 23.59905380597269797 ) ) ;
#25835 = CARTESIAN_POINT ( 'NONE',  ( 5.896782393890504181, 8.460428369634545476, -18.24684188237228000 ) ) ;
#25836 = CARTESIAN_POINT ( 'NONE',  ( 3.407937589446178528, 13.10584870154472092, -3.987184287467649746 ) ) ;
#25837 = ADVANCED_FACE ( 'NONE', ( #26936 ), #61024, .T. ) ;
#25838 = ORIENTED_EDGE ( 'NONE', *, *, #41286, .F. ) ;
#25839 = CARTESIAN_POINT ( 'NONE',  ( 4.956445790444004018, -40.78973928653763181, -23.53157918788973291 ) ) ;
#25840 = DIRECTION ( 'NONE',  ( 3.273063162220399693E-16, -1.000000000000000000, -5.236901059552639509E-15 ) ) ;
#25841 = CARTESIAN_POINT ( 'NONE',  ( 2.618530812446115519, 44.94501346709303391, -13.77216590232000115 ) ) ;
#25842 = VERTEX_POINT ( 'NONE', #23162 ) ;
#25843 = CARTESIAN_POINT ( 'NONE',  ( 3.240649175237394708, -25.97541675339710565, -35.50412147744241764 ) ) ;
#25844 = DIRECTION ( 'NONE',  ( 1.836970198721033632E-16, -1.000000000000000000, 0.000000000000000000 ) ) ;
#25845 = ORIENTED_EDGE ( 'NONE', *, *, #48302, .F. ) ;
#25846 = CARTESIAN_POINT ( 'NONE',  ( 4.960386119450136633, 13.41207489487415572, 41.64796167505232916 ) ) ;
#25847 = CARTESIAN_POINT ( 'NONE',  ( 0.8560838555295167129, -41.44626783305055540, -21.96769712083564841 ) ) ;
#25848 = AXIS2_PLACEMENT_3D ( 'NONE', #60443, #60148, #55133 ) ;
#25849 = ORIENTED_EDGE ( 'NONE', *, *, #41396, .F. ) ;
#25850 = CARTESIAN_POINT ( 'NONE',  ( 4.967162193818129623, -40.65506779172174845, 14.26841313271267886 ) ) ;
#25851 = CARTESIAN_POINT ( 'NONE',  ( 0.1119899015040012463, -42.53546974785185597, -11.73435645964812046 ) ) ;
#25852 = CARTESIAN_POINT ( 'NONE',  ( 4.962356264823608143, -25.31392337492896161, 33.62202970123266965 ) ) ;
#25854 = CARTESIAN_POINT ( 'NONE',  ( 2.879087469061463178, 21.87161467977467666, 38.18028480882303910 ) ) ;
#25853 = COLOUR_RGB ( '', 0.66274510, 0.83137255, 0.94901961) ;
#25855 = CARTESIAN_POINT ( 'NONE',  ( 0.5839880159502331969, 46.27569712847351013, -12.35255585954135427 ) ) ;
#25856 = CARTESIAN_POINT ( 'NONE',  ( 4.956445790444011124, -17.42806872899762993, -43.74700527484106516 ) ) ;
#25857 = CARTESIAN_POINT ( 'NONE',  ( 0.5786265663353196143, 11.69877690266654824, 46.45062944555897388 ) ) ;
#25858 = CARTESIAN_POINT ( 'NONE',  ( 2.299652685299200972, -48.44937665196427190, -7.545835069377869075 ) ) ;
#25859 = CARTESIAN_POINT ( 'NONE',  ( 0.8554163680231816613, 42.82911630180360163, -19.15391004255791074 ) ) ;
#25860 = CARTESIAN_POINT ( 'NONE',  ( 0.5835871038041858805, 27.92758718982630839, -37.67339016674964114 ) ) ;
#25861 = ORIENTED_EDGE ( 'NONE', *, *, #18254, .F. ) ;
#25862 = VECTOR ( 'NONE', #5125, 1000.000000000000000 ) ;
#25863 = EDGE_CURVE ( 'NONE', #4535, #56737, #6990, .T. ) ;
#25864 = CARTESIAN_POINT ( 'NONE',  ( -15.87380398270803106, -12.49998253090622313, 0.2752802063126107979 ) ) ;
#25865 = FACE_OUTER_BOUND ( 'NONE', #12912, .T. ) ;
#25866 = CARTESIAN_POINT ( 'NONE',  ( 6.999999999999995559, 56.56854249492450037, -56.56854249492312192 ) ) ;
#25867 = DIRECTION ( 'NONE',  ( 0.000000000000000000, 0.000000000000000000, 1.000000000000000000 ) ) ;
#25868 = B_SPLINE_CURVE_WITH_KNOTS ( 'NONE', 3,
 ( #36821, #55571, #7026, #16774, #45912, #13015 ),
 .UNSPECIFIED., .F., .F.,
 ( 4, 2, 4 ),
 ( 5.421010862427522170E-19, 0.0002293801035737086673, 0.0004587602071474167925 ),
 .UNSPECIFIED. ) ;
#25869 = CARTESIAN_POINT ( 'NONE',  ( 0.9789889208857696090, -31.01704594793936565, 28.18293382005832726 ) ) ;
#25870 = EDGE_CURVE ( 'NONE', #31937, #9918, #33499, .T. ) ;
#25871 = B_SPLINE_CURVE_WITH_KNOTS ( 'NONE', 3,
 ( #46193, #50253, #22366, #7314 ),
 .UNSPECIFIED., .F., .F.,
 ( 4, 4 ),
 ( 0.000000000000000000, 0.004446298630425043336 ),
 .UNSPECIFIED. ) ;
#25872 = DIRECTION ( 'NONE',  ( -7.825462779892291622E-31, 0.003998373736184435839, 0.9999920064717846557 ) ) ;
#25873 = CARTESIAN_POINT ( 'NONE',  ( 0.6028618097248863439, -44.37846879336947836, 18.57111736963370419 ) ) ;
#25874 = B_SPLINE_CURVE_WITH_KNOTS ( 'NONE', 3,
 ( #23581, #25424, #5671, #44568, #19825, #30426 ),
 .UNSPECIFIED., .F., .F.,
 ( 4, 2, 4 ),
 ( 0.000000000000000000, 0.0002447195606305710598, 0.0004894391212611486248 ),
 .UNSPECIFIED. ) ;
#25875 = CARTESIAN_POINT ( 'NONE',  ( 0.6009453534118439633, 41.87889766923454715, -23.67490308139361588 ) ) ;
#25876 = ADVANCED_FACE ( 'NONE', ( #9667 ), #18967, .F. ) ;
#25877 = AXIS2_PLACEMENT_3D ( 'NONE', #4130, #37697, #42096 ) ;
#25878 = CARTESIAN_POINT ( 'NONE',  ( 0.1073791018717578927, 6.109314776652701617, -42.68962945260948061 ) ) ;
#25880 = ORIENTED_EDGE ( 'NONE', *, *, #17789, .T. ) ;
#25879 = CARTESIAN_POINT ( 'NONE',  ( 3.660087539127330647, -39.22752134874899355, -27.72868323267848822 ) ) ;
#25881 = EDGE_LOOP ( 'NONE', ( #4445, #36407, #50811, #42511 ) ) ;
#25882 = CARTESIAN_POINT ( 'NONE',  ( 1.088908134280559992, 42.43751564162690215, -6.374115321932653622 ) ) ;
#25883 = VECTOR ( 'NONE', #21459, 999.9999999999998863 ) ;
#25884 = CARTESIAN_POINT ( 'NONE',  ( 2.282816707992309624, -24.15823995494712761, 40.28494022196337454 ) ) ;
#25885 = CARTESIAN_POINT ( 'NONE',  ( 0.5998501479064708430, 0.5236536531314925913, -48.10473956285919428 ) ) ;
#25886 = ORIENTED_EDGE ( 'NONE', *, *, #21671, .T. ) ;
#25887 = CARTESIAN_POINT ( 'NONE',  ( -6.016489644550736315, -16.31649074174283598, 9.425415887801030124 ) ) ;
#25888 = CARTESIAN_POINT ( 'NONE',  ( 0.5837374860065650539, -47.46223477511615130, 6.431731162805607305 ) ) ;
#25889 = CARTESIAN_POINT ( 'NONE',  ( 0.6001305935487422083, 38.48510059944047157, -28.87057754790898656 ) ) ;
#25890 =( BOUNDED_SURFACE ( )  B_SPLINE_SURFACE ( 3, 1, ( 
 ( #53712, #10844 ),
 ( #34965, #25540 ),
 ( #53417, #9915 ),
 ( #10524, #44675 ) ),
 .UNSPECIFIED., .F., .F., .F. ) 
 B_SPLINE_SURFACE_WITH_KNOTS ( ( 4, 4 ),
 ( 2, 2 ),
 ( 0.000000000000000000, 1.000000000000000000 ),
 ( 0.000000000000000000, 1.000000000000000000 ),
 .UNSPECIFIED. ) 
 GEOMETRIC_REPRESENTATION_ITEM ( )  RATIONAL_B_SPLINE_SURFACE ( (
 ( 1.000000000000000000, 1.000000000000000000),
 ( 0.9952954269826590483, 0.8620686068821339365),
 ( 0.9952954269826590483, 0.8620686068821339365),
 ( 1.000000000000000000, 1.000000000000000000) ) ) 
 REPRESENTATION_ITEM ( '' )  SURFACE ( )  );
#25891 = ORIENTED_EDGE ( 'NONE', *, *, #20466, .F. ) ;
#25892 = ORIENTED_EDGE ( 'NONE', *, *, #33587, .F. ) ;
#25893 = DIRECTION ( 'NONE',  ( 1.000000000000000000, 0.000000000000000000, 0.000000000000000000 ) ) ;
#25894 = EDGE_CURVE ( 'NONE', #33022, #52994, #36221, .T. ) ;
#25895 = CIRCLE ( 'NONE', #22907, 2.649999999999997691 ) ;
#25896 = CARTESIAN_POINT ( 'NONE',  ( 4.956653778116480780, -21.75875759808806720, 42.88673967249081898 ) ) ;
#25897 = B_SPLINE_CURVE_WITH_KNOTS ( 'NONE', 3,
 ( #15326, #21246, #5876, #6487 ),
 .UNSPECIFIED., .F., .F.,
 ( 4, 4 ),
 ( 8.673617379884035472E-19, 0.004446298630425045070 ),
 .UNSPECIFIED. ) ;
#25898 = CARTESIAN_POINT ( 'NONE',  ( 0.7762777257811908083, 41.92424087089342066, -23.17763256463726762 ) ) ;
#25899 = EDGE_LOOP ( 'NONE', ( #22847, #12413, #20228, #490 ) ) ;
#25900 = ORIENTED_EDGE ( 'NONE', *, *, #44539, .T. ) ;
#25901 = LINE ( 'NONE', #16198, #58584 ) ;
#25902 = EDGE_CURVE ( 'NONE', #20913, #36543, #4765, .T. ) ;
#25903 = CARTESIAN_POINT ( 'NONE',  ( 4.956445790443991584, 25.79263028817558023, 39.39896284113483915 ) ) ;
#25904 = EDGE_LOOP ( 'NONE', ( #40377, #22456, #36798, #11185 ) ) ;
#25905 = COLOUR_RGB ( '', 0.09019608, 0.27058824, 0.51372549) ;
#25906 =( BOUNDED_SURFACE ( )  B_SPLINE_SURFACE ( 3, 1, ( 
 ( #48343, #43673 ),
 ( #53029, #33644 ),
 ( #9821, #28924 ),
 ( #19543, #713 ) ),
 .UNSPECIFIED., .F., .F., .F. ) 
 B_SPLINE_SURFACE_WITH_KNOTS ( ( 4, 4 ),
 ( 2, 2 ),
 ( 0.000000000000000000, 1.000000000000000000 ),
 ( 0.000000000000000000, 1.000000000000000000 ),
 .UNSPECIFIED. ) 
 GEOMETRIC_REPRESENTATION_ITEM ( )  RATIONAL_B_SPLINE_SURFACE ( (
 ( 1.000000000000000000, 1.000000000000000000),
 ( 0.7282232189291694135, 0.9929344683865672927),
 ( 0.7282232189291694135, 0.9929344683865672927),
 ( 1.000000000000000000, 1.000000000000000000) ) ) 
 REPRESENTATION_ITEM ( '' )  SURFACE ( )  );
#25907 = CARTESIAN_POINT ( 'NONE',  ( 0.2285344041767113921, 29.09448245089918217, -33.16643274773119998 ) ) ;
#25908 = DIRECTION ( 'NONE',  ( 1.000000000000000000, 0.000000000000000000, 0.000000000000000000 ) ) ;
#25909 = ORIENTED_EDGE ( 'NONE', *, *, #6740, .F. ) ;
#25910 = CARTESIAN_POINT ( 'NONE',  ( 4.303969348037258058, 14.52400616872369632, 45.86537346639062918 ) ) ;
#25911 = CARTESIAN_POINT ( 'NONE',  ( 0.6000166863083106206, -39.66797998683873772, 28.95297645272788500 ) ) ;
#25912 = ORIENTED_EDGE ( 'NONE', *, *, #48091, .T. ) ;
#25913 = CARTESIAN_POINT ( 'NONE',  ( 0.8751705887134553219, -24.81530984069179269, -41.19904111682499348 ) ) ;
#25914 = CARTESIAN_POINT ( 'NONE',  ( 0.5817217712918332229, -20.15223009300066792, 42.34527808725705000 ) ) ;
#25915 = CARTESIAN_POINT ( 'NONE',  ( 3.238018933889920792, 3.371911215444494125, 12.96293589904742838 ) ) ;
#25916 = CARTESIAN_POINT ( 'NONE',  ( 42.00000000000000711, 19.00000000000000355, -1.617781153285278467E-30 ) ) ;
#25917 = EDGE_CURVE ( 'NONE', #22617, #28594, #5560, .T. ) ;
#25918 = VERTEX_POINT ( 'NONE', #52574 ) ;
#25919 = DIRECTION ( 'NONE',  ( 0.000000000000000000, 0.000000000000000000, -1.000000000000000000 ) ) ;
#25920 = CARTESIAN_POINT ( 'NONE',  ( 0.1129192098497455998, 39.96249028893973332, -18.70698152272436587 ) ) ;
#25921 = ORIENTED_EDGE ( 'NONE', *, *, #10764, .T. ) ;
#25922 = LINE ( 'NONE', #21218, #13196 ) ;
#25923 = ORIENTED_EDGE ( 'NONE', *, *, #31698, .T. ) ;
#25924 = CARTESIAN_POINT ( 'NONE',  ( 0.5838002273316438284, -18.45474575185545163, 44.19779719735692680 ) ) ;
#25925 = ORIENTED_EDGE ( 'NONE', *, *, #13623, .F. ) ;
#25926 = CARTESIAN_POINT ( 'NONE',  ( 0.6001305935487422083, 0.5236757026882734589, 48.10757715638249010 ) ) ;
#25927 = CARTESIAN_POINT ( 'NONE',  ( 0.9787284016396613495, 25.00986318006678744, 33.62800533250774748 ) ) ;
#25928 = AXIS2_PLACEMENT_3D ( 'NONE', #39594, #39284, #403 ) ;
#25929 = CARTESIAN_POINT ( 'NONE',  ( 0.1119899015040012741, 10.36499862923388804, -42.88972034891910567 ) ) ;
#25930 = ORIENTED_EDGE ( 'NONE', *, *, #43760, .T. ) ;
#25931 = CARTESIAN_POINT ( 'NONE',  ( 0.6001305935487422083, -18.89378601236091981, 44.24520387813797129 ) ) ;
#25932 = CARTESIAN_POINT ( 'NONE',  ( 0.9968887458511694888, -11.73947777183250096, 41.27232779986115929 ) ) ;
#25933 = DIRECTION ( 'NONE',  ( -1.000000000000000000, -1.558861125776144859E-16, 3.851859888774471706E-32 ) ) ;
#25934 = ORIENTED_EDGE ( 'NONE', *, *, #5691, .T. ) ;
#25935 = VERTEX_POINT ( 'NONE', #242 ) ;
#25936 = CARTESIAN_POINT ( 'NONE',  ( 0.1119899015040011631, 29.24697023967760146, 33.03900785423071085 ) ) ;
#25937 = CARTESIAN_POINT ( 'NONE',  ( 1.834102595619085507, 30.56483960858423998, 31.71731900018039951 ) ) ;
#25938 = CARTESIAN_POINT ( 'NONE',  ( 0.3622758884714600280, -37.74294673546600620, 20.83792692158906235 ) ) ;
#25939 = CARTESIAN_POINT ( 'NONE',  ( 0.1092355843206037486, -5.330717085613026818, -42.79374386763043958 ) ) ;
#25940 = CARTESIAN_POINT ( 'NONE',  ( 0.5809828226811553087, -44.45562576850588243, -17.82437196699728332 ) ) ;
#25941 = CARTESIAN_POINT ( 'NONE',  ( 0.5980271706414734822, 40.77460832818560021, -27.37664257217675967 ) ) ;
#25942 = ORIENTED_EDGE ( 'NONE', *, *, #14781, .T. ) ;
#25943 = DIRECTION ( 'NONE',  ( 0.07500201931887537365, -0.08636880102338072296, -0.9934360207420882549 ) ) ;
#25944 = CARTESIAN_POINT ( 'NONE',  ( 4.694002226626921015, 39.55162978021514419, 22.67053932254223625 ) ) ;
#25945 = CIRCLE ( 'NONE', #11971, 10.00000000000000711 ) ;
#25946 = EDGE_LOOP ( 'NONE', ( #6854, #24889, #52029, #59473 ) ) ;
#25947 = ADVANCED_FACE ( 'NONE', ( #24388 ), #3736, .F. ) ;
#25948 = CARTESIAN_POINT ( 'NONE',  ( 4.975801465491695552, 35.64402118370958306, -32.01766832630274706 ) ) ;
#25949 = CARTESIAN_POINT ( 'NONE',  ( 4.975610109902397937, -41.30423662854430944, -26.19941685746064053 ) ) ;
#25950 = CARTESIAN_POINT ( 'NONE',  ( 0.8551540677456715978, 24.74404575822833507, -41.03346287276401938 ) ) ;
#25951 = FACE_OUTER_BOUND ( 'NONE', #14054, .T. ) ;
#25952 = CARTESIAN_POINT ( 'NONE',  ( -2.569797478183790229, -14.24379821351259601, 3.352038560005669687 ) ) ;
#25953 = EDGE_CURVE ( 'NONE', #40973, #48800, #43655, .T. ) ;
#25954 = PRESENTATION_STYLE_ASSIGNMENT (( #45391 ) ) ;
#25955 = CARTESIAN_POINT ( 'NONE',  ( 0.6041374136657476912, 48.10739871142803992, -0.1745662470639787467 ) ) ;
#25956 = CARTESIAN_POINT ( 'NONE',  ( 5.959547316686252039, -2.675599016784394379, -20.35048796920736081 ) ) ;
#25957 = EDGE_CURVE ( 'NONE', #6174, #51465, #46220, .T. ) ;
#25958 = CARTESIAN_POINT ( 'NONE',  ( 1.231276596079887264, 19.39962232756291272, -37.16088568059149111 ) ) ;
#25959 = ADVANCED_FACE ( 'NONE', ( #42588 ), #45064, .T. ) ;
#25960 = LINE ( 'NONE', #53215, #42858 ) ;
#25961 = EDGE_CURVE ( 'NONE', #43795, #59028, #12057, .T. ) ;
#25962 = FACE_OUTER_BOUND ( 'NONE', #13857, .T. ) ;
#25963 = CARTESIAN_POINT ( 'NONE',  ( 0.9775691876210983455, 9.347414102159763871, 40.85290147092045032 ) ) ;
#25964 = B_SPLINE_CURVE_WITH_KNOTS ( 'NONE', 3,
 ( #30357, #22433, #49469, #11582, #22743, #15975, #30664, #55618, #6520, #50614, #11267, #7701, #25665, #60944, #55936, #37171, #1846, #51231, #8313, #27433, #41876, #8628, #45960, #1528, #40117 ),
 .UNSPECIFIED., .F., .F.,
 ( 4, 3, 3, 3, 3, 3, 3, 3, 4 ),
 ( 5.057544569639794935E-18, 0.0005656085177311395316, 0.001131215744874499622, 0.001696821861372765916, 0.002262427090022498151, 0.002828031679238745925, 0.003393635864401605296, 0.003977030878808133357, 0.004561030005651159867 ),
 .UNSPECIFIED. ) ;
#25965 = DIRECTION ( 'NONE',  ( 0.000000000000000000, 0.000000000000000000, 1.000000000000000000 ) ) ;
#25966 = AXIS2_PLACEMENT_3D ( 'NONE', #23433, #44047, #37555 ) ;
#25967 = EDGE_CURVE ( 'NONE', #43343, #47186, #42071, .T. ) ;
#25968 = VERTEX_POINT ( 'NONE', #30311 ) ;
#25969 = CARTESIAN_POINT ( 'NONE',  ( 4.967162193818130511, 0.000000000000000000, 0.000000000000000000 ) ) ;
#25970 = ADVANCED_FACE ( 'NONE', ( #1484 ), #38180, .F. ) ;
#25971 = CONICAL_SURFACE ( 'NONE', #47011, 42.92674063221959813, 1.485477209440487556 ) ;
#25972 = CARTESIAN_POINT ( 'NONE',  ( 0.1104177457020373149, 43.12445244485484608, -0.004894317366372227286 ) ) ;
#25973 = CARTESIAN_POINT ( 'NONE',  ( 0.9756950546413926117, -39.67916378221926266, -16.33093981194364019 ) ) ;
#25974 = CARTESIAN_POINT ( 'NONE',  ( 0.6024113833632039894, -45.43637621081261813, -18.63001840928686903 ) ) ;
#25975 = CARTESIAN_POINT ( 'NONE',  ( 0.1081432562775998668, -41.76274004527640926, 10.75186376283269851 ) ) ;
#25976 = ORIENTED_EDGE ( 'NONE', *, *, #22998, .F. ) ;
#25977 = CARTESIAN_POINT ( 'NONE',  ( -4.000000000000000000, -2.309401076758531346, -5.242734410091827613 ) ) ;
#25978 = CARTESIAN_POINT ( 'NONE',  ( 0.6016117650947689910, 27.80883221307838582, -40.47492934137567033 ) ) ;
#25979 = CARTESIAN_POINT ( 'NONE',  ( 4.960386119450140185, -15.28553149072569006, 40.99742664751502019 ) ) ;
#25980 = ORIENTED_EDGE ( 'NONE', *, *, #47037, .F. ) ;
#25981 = CARTESIAN_POINT ( 'NONE',  ( 3.238931869106854933, 18.12707634097768761, 38.98364358950751551 ) ) ;
#25982 = ORIENTED_EDGE ( 'NONE', *, *, #31347, .T. ) ;
#25983 = CARTESIAN_POINT ( 'NONE',  ( 4.834790513006555379, 33.61992680604640071, -33.20075093247837117 ) ) ;
#25984 = AXIS2_PLACEMENT_3D ( 'NONE', #47751, #411, #42756 ) ;
#25985 = CARTESIAN_POINT ( 'NONE',  ( 5.894904586330512508, 20.06808393774118215, 1.342169560605994905 ) ) ;
#25986 = ORIENTED_EDGE ( 'NONE', *, *, #11385, .F. ) ;
#25987 = CARTESIAN_POINT ( 'NONE',  ( 5.974727161628367256, 12.48248968439928674, -16.29297756969635458 ) ) ;
#25988 = ORIENTED_EDGE ( 'NONE', *, *, #17818, .F. ) ;
#25989 = DIRECTION ( 'NONE',  ( 0.000000000000000000, 0.000000000000000000, 1.000000000000000000 ) ) ;
#25990 = CARTESIAN_POINT ( 'NONE',  ( 4.975610109902397937, 0.9924324126411095959, -48.90260202733707473 ) ) ;
#25991 = ORIENTED_EDGE ( 'NONE', *, *, #41212, .T. ) ;
#25992 = EDGE_CURVE ( 'NONE', #2416, #1120, #27990, .T. ) ;
#25993 = ORIENTED_EDGE ( 'NONE', *, *, #7899, .F. ) ;
#25994 = CARTESIAN_POINT ( 'NONE',  ( 4.960156602257181468, -15.40604254112611216, -43.79161740034492567 ) ) ;
#25995 = CARTESIAN_POINT ( 'NONE',  ( 0.5809828226811553087, -38.32755012159125840, -28.72298383114528519 ) ) ;
#25996 = B_SPLINE_CURVE_WITH_KNOTS ( 'NONE', 3,
 ( #45714, #12203, #36318, #59788, #54137, #45405, #1838, #16574, #49461, #55383, #39797, #58846, #21580, #55078, #11255, #35702, #40403, #6511, #59464 ),
 .UNSPECIFIED., .F., .F.,
 ( 4, 3, 3, 3, 3, 3, 4 ),
 ( 9.813676791237319219E-18, 0.0002724573126191676240, 0.0004086839781548304794, 0.0005449106435901656569, 0.0006811373090491328096, 0.0008459866663933593997, 0.001010840725717213366 ),
 .UNSPECIFIED. ) ;
#25997 = EDGE_CURVE ( 'NONE', #5948, #1788, #55035, .T. ) ;
#25998 = VERTEX_POINT ( 'NONE', #16534 ) ;
#25999 = EDGE_LOOP ( 'NONE', ( #20803, #59336, #49265, #8232 ) ) ;
#26000 = CARTESIAN_POINT ( 'NONE',  ( -6.016761891674565099, -9.418621820384382559, -16.32039929810266798 ) ) ;
#26001 = CARTESIAN_POINT ( 'NONE',  ( 0.6029442701453591180, -25.53140348424445705, -41.94869081727089366 ) ) ;
#26002 = CARTESIAN_POINT ( 'NONE',  ( 5.901764892641288895, -32.95403503760634578, -36.22185862403931367 ) ) ;
#26003 = CARTESIAN_POINT ( 'NONE',  ( 3.270143674763207553, 13.14781761974169072, 3.806843787665967760 ) ) ;
#26004 = EDGE_LOOP ( 'NONE', ( #5441, #4944, #51833, #12088 ) ) ;
#26005 = PRODUCT_DEFINITION ( 'UNKNOWN', '', #10894, #5976 ) ;
#26006 = CARTESIAN_POINT ( 'NONE',  ( 0.8753041380234530822, 27.35839019124417604, -40.77568900725792389 ) ) ;
#26007 = CARTESIAN_POINT ( 'NONE',  ( -6.077587904424778920, 15.43577113102525189, 11.51229738082446552 ) ) ;
#26008 = B_SPLINE_CURVE_WITH_KNOTS ( 'NONE', 3,
 ( #4463, #38343, #57393, #52716, #5085, #15140 ),
 .UNSPECIFIED., .F., .F.,
 ( 4, 2, 4 ),
 ( 9.543442895606953578E-18, 0.0002291978881530156451, 0.0004583957763060217492 ),
 .UNSPECIFIED. ) ;
#26009 = ORIENTED_EDGE ( 'NONE', *, *, #52932, .F. ) ;
#26010 = CARTESIAN_POINT ( 'NONE',  ( 0.5837800304671226792, -46.78824101889156850, -3.177709007698712007 ) ) ;
#26011 = ORIENTED_EDGE ( 'NONE', *, *, #55256, .F. ) ;
#26012 = DIRECTION ( 'NONE',  ( 0.000000000000000000, 0.000000000000000000, -1.000000000000000000 ) ) ;
#26013 = CARTESIAN_POINT ( 'NONE',  ( 0.6000166863083090663, -35.63988196839386546, 33.78790160674983412 ) ) ;
#26014 = FACE_OUTER_BOUND ( 'NONE', #36105, .T. ) ;
#26015 = VERTEX_POINT ( 'NONE', #30616 ) ;
#26016 = CARTESIAN_POINT ( 'NONE',  ( 3.782625744892853970, 35.26065757000644396, -22.88938906624093761 ) ) ;
#26017 = CARTESIAN_POINT ( 'NONE',  ( 0.7245667037590786119, 37.65687897229928183, -29.92941129926910904 ) ) ;
#26018 = CARTESIAN_POINT ( 'NONE',  ( 52.25045007007695830, 12.34004751916969411, 1.997177200709687739 ) ) ;
#26019 = CARTESIAN_POINT ( 'NONE',  ( 0.6023143664670691511, -29.07782746490727988, -38.32505149877503214 ) ) ;
#26020 = AXIS2_PLACEMENT_3D ( 'NONE', #25295, #44442, #1468 ) ;
#26021 = ORIENTED_EDGE ( 'NONE', *, *, #36173, .T. ) ;
#26022 = CARTESIAN_POINT ( 'NONE',  ( 0.3622758884714730732, 4.808133778521878732, -42.84426538328727219 ) ) ;
#26023 = EDGE_LOOP ( 'NONE', ( #34639, #36779 ) ) ;
#26024 = CARTESIAN_POINT ( 'NONE',  ( 0.5850706913938533704, -33.99603398296613932, 33.73916126769439217 ) ) ;
#26025 = CARTESIAN_POINT ( 'NONE',  ( 0.9790850452238881729, 41.52796822506905983, -5.636061156592599986 ) ) ;
#26026 = ADVANCED_FACE ( 'NONE', ( #12162 ), #6101, .F. ) ;
#26027 = CARTESIAN_POINT ( 'NONE',  ( 2.891212509700765487, 5.349982771599759140E-15, 41.99381090189422139 ) ) ;
#26028 = AXIS2_PLACEMENT_3D ( 'NONE', #45192, #40186, #50769 ) ;
#26029 = ORIENTED_EDGE ( 'NONE', *, *, #13257, .F. ) ;
#26030 = CARTESIAN_POINT ( 'NONE',  ( 0.1073791018717483448, -25.86618856530736466, 34.50606437925502945 ) ) ;
#26031 = DIRECTION ( 'NONE',  ( -1.000000000000000000, -0.000000000000000000, -0.000000000000000000 ) ) ;
#26032 = EDGE_CURVE ( 'NONE', #5799, #44283, #12947, .T. ) ;
#26033 = VECTOR ( 'NONE', #34589, 1000.000000000000114 ) ;
#26034 = CARTESIAN_POINT ( 'NONE',  ( -6.077587904424778920, 16.77513308702627981, 9.454677747363296803 ) ) ;
#26035 = ADVANCED_FACE ( 'NONE', ( #49119 ), #53901, .T. ) ;
#26036 = CARTESIAN_POINT ( 'NONE',  ( 0.9754402186311934564, 37.06569162601132206, -21.61645729243075209 ) ) ;
#26037 = CARTESIAN_POINT ( 'NONE',  ( 0.5837799406558230597, 32.66722334661169214, 33.64663532063480744 ) ) ;
#26038 = DIRECTION ( 'NONE',  ( 0.09835009131224566048, 0.8579344853044275077, 0.5042575517176716149 ) ) ;
#26039 = CARTESIAN_POINT ( 'NONE',  ( 0.5848930533535030563, -13.72019472029311160, 44.84450177251164149 ) ) ;
#26040 = CARTESIAN_POINT ( 'NONE',  ( 3.238018933889920792, -7.437505510345073567, 11.13961418323092545 ) ) ;
#26041 = B_SPLINE_CURVE_WITH_KNOTS ( 'NONE', 3,
 ( #48530, #20652, #15964, #57912, #39794, #58219 ),
 .UNSPECIFIED., .F., .F.,
 ( 4, 2, 4 ),
 ( 0.000000000000000000, 0.0002291459268755687982, 0.0004582918537511375965 ),
 .UNSPECIFIED. ) ;
#26042 = CARTESIAN_POINT ( 'NONE',  ( 5.974727161628369032, -7.868887636447738920, 18.95664195401504060 ) ) ;
#26043 = CARTESIAN_POINT ( 'NONE',  ( 3.661921753702023441, 20.93653541326595757, -42.12235283935475394 ) ) ;
#26044 = ORIENTED_EDGE ( 'NONE', *, *, #206, .T. ) ;
#26045 = LINE ( 'NONE', #2210, #30875 ) ;
#26046 = CARTESIAN_POINT ( 'NONE',  ( 0.8744876279028263033, 49.04340454744552602, -2.257104511335871422 ) ) ;
#26047 = CARTESIAN_POINT ( 'NONE',  ( 0.1119899015040012463, -18.37259944400937428, 40.11743882481150081 ) ) ;
#26048 = ORIENTED_EDGE ( 'NONE', *, *, #21854, .F. ) ;
#26049 = CARTESIAN_POINT ( 'NONE',  ( 0.8751705887134423323, 7.160166390004303771, -47.55935879196464100 ) ) ;
#26050 = CARTESIAN_POINT ( 'NONE',  ( 0.9722240750034573109, -5.023189755349235064, 42.61332880321398875 ) ) ;
#26051 = DIRECTION ( 'NONE',  ( 1.000000000000000000, 1.558861125776144859E-16, -3.851859888774471706E-32 ) ) ;
#26052 = ORIENTED_EDGE ( 'NONE', *, *, #61843, .T. ) ;
#26053 = CARTESIAN_POINT ( 'NONE',  ( 0.2279481005628788415, 3.480028581335672389, 43.98173357367804925 ) ) ;
#26054 = CARTESIAN_POINT ( 'NONE',  ( -6.016761891674564211, 13.32657647165355286, 13.32172022638596509 ) ) ;
#26055 = VERTEX_POINT ( 'NONE', #2098 ) ;
#26056 = CARTESIAN_POINT ( 'NONE',  ( 0.6846871229502899947, -29.84551600520608616, -37.47592888575278636 ) ) ;
#26057 = ORIENTED_EDGE ( 'NONE', *, *, #5351, .T. ) ;
#26058 = ORIENTED_EDGE ( 'NONE', *, *, #4488, .F. ) ;
#26059 = CARTESIAN_POINT ( 'NONE',  ( 0.1157991065609915854, 44.02822103802267151, 2.908284333540335886 ) ) ;
#26060 = EDGE_LOOP ( 'NONE', ( #57591, #36887, #58871, #25709 ) ) ;
#26061 = CARTESIAN_POINT ( 'NONE',  ( -6.057079549204054558, -8.914624657272197439, 17.06929109013297463 ) ) ;
#26062 = CARTESIAN_POINT ( 'NONE',  ( 4.975801465491695552, 43.22084481528192157, 20.67815041659156705 ) ) ;
#26063 = EDGE_LOOP ( 'NONE', ( #42142, #48214, #41071, #4219 ) ) ;
#26064 = CARTESIAN_POINT ( 'NONE',  ( 4.000000000000000000, 0.000000000000000000, -5.600000000000000533 ) ) ;
#26065 = AXIS2_PLACEMENT_3D ( 'NONE', #58943, #14822, #58306 ) ;
#26066 = ADVANCED_FACE ( 'NONE', ( #6789 ), #58918, .F. ) ;
#26067 = CARTESIAN_POINT ( 'NONE',  ( 5.896278296736517710, -19.93412839397023006, 2.675351339000858975 ) ) ;
#26068 = ORIENTED_EDGE ( 'NONE', *, *, #46334, .F. ) ;
#26069 = CARTESIAN_POINT ( 'NONE',  ( 0.1156867017252034974, 43.33420080233410232, -8.312030323463241999 ) ) ;
#26070 = CARTESIAN_POINT ( 'NONE',  ( 5.959547316686252039, -19.82715097195158194, -5.308980600728387067 ) ) ;
#26071 = DIRECTION ( 'NONE',  ( 0.09835009131224567436, 0.6119264800004780014, -0.7847759187265480607 ) ) ;
#26072 = CARTESIAN_POINT ( 'NONE',  ( 0.9790320750461904975, 36.01440475631515881, 21.43128047015612125 ) ) ;
#26073 = ORIENTED_EDGE ( 'NONE', *, *, #20089, .F. ) ;
#26074 = B_SPLINE_CURVE_WITH_KNOTS ( 'NONE', 3,
 ( #17715, #56217, #3583, #61220, #9530, #51205, #23337, #27408, #32746, #27727, #47156, #36841, #8598, #46856, #32434, #37454, #51822, #55909, #18645, #51509, #33063, #3897, #13031, #42465, #8927 ),
 .UNSPECIFIED., .F., .F.,
 ( 4, 3, 3, 3, 3, 3, 3, 3, 4 ),
 ( 6.992893892674702526E-18, 0.0005656085177311379053, 0.001131215744874499839, 0.001696821861372766350, 0.002262427090022498151, 0.002828031679238744191, 0.003393635864401603995, 0.003977030878808131623, 0.004561030005651159000 ),
 .UNSPECIFIED. ) ;
#26075 = EDGE_LOOP ( 'NONE', ( #54177, #56966, #50402, #23274 ) ) ;
#26076 = CARTESIAN_POINT ( 'NONE',  ( 5.958863334805807099, 10.26176968287945179, -17.77634700750918384 ) ) ;
#26077 =( BOUNDED_SURFACE ( )  B_SPLINE_SURFACE ( 3, 1, ( 
 ( #3896, #34282 ),
 ( #44016, #1051 ),
 ( #24249, #43699 ),
 ( #43076, #47452 ) ),
 .UNSPECIFIED., .F., .F., .F. ) 
 B_SPLINE_SURFACE_WITH_KNOTS ( ( 4, 4 ),
 ( 2, 2 ),
 ( 0.000000000000000000, 1.000000000000000000 ),
 ( 0.000000000000000000, 1.000000000000000000 ),
 .UNSPECIFIED. ) 
 GEOMETRIC_REPRESENTATION_ITEM ( )  RATIONAL_B_SPLINE_SURFACE ( (
 ( 1.000000000000000000, 1.000000000000000000),
 ( 0.9953040768229013402, 0.8617119497784988535),
 ( 0.9953040768229013402, 0.8617119497784988535),
 ( 1.000000000000000000, 1.000000000000000000) ) ) 
 REPRESENTATION_ITEM ( '' )  SURFACE ( )  );
#26078 = FACE_OUTER_BOUND ( 'NONE', #45198, .T. ) ;
#26079 = CARTESIAN_POINT ( 'NONE',  ( 0.3676999524040366896, -35.84016207189403502, -25.71834687500748373 ) ) ;
#26080 = EDGE_LOOP ( 'NONE', ( #15670, #22210, #17644, #25055 ) ) ;
#26081 = FACE_OUTER_BOUND ( 'NONE', #46580, .T. ) ;
#26082 = CARTESIAN_POINT ( 'NONE',  ( 0.5997462898726536595, 46.43852004798843325, 15.96920429754989890 ) ) ;
#26083 = CARTESIAN_POINT ( 'NONE',  ( 4.956653778116966613, 0.000000000000000000, 0.000000000000000000 ) ) ;
#26084 = VERTEX_POINT ( 'NONE', #34728 ) ;
#26085 = VERTEX_POINT ( 'NONE', #53789 ) ;
#26086 = CARTESIAN_POINT ( 'NONE',  ( 0.1310142868023658203, 15.91230901232167838, 40.08041389954887279 ) ) ;
#26087 = CYLINDRICAL_SURFACE ( 'NONE', #47703, 15.43999999999999240 ) ;
#26088 = CARTESIAN_POINT ( 'NONE',  ( 4.549368137175248350, -13.99871866169391765, 40.58005590356665948 ) ) ;
#26089 = DIRECTION ( 'NONE',  ( -1.000000000000000000, -0.000000000000000000, -0.000000000000000000 ) ) ;
#26090 = EDGE_CURVE ( 'NONE', #51012, #58502, #34937, .T. ) ;
#26091 = CARTESIAN_POINT ( 'NONE',  ( 0.5549461598389366923, -41.20260823449177678, -15.73412756214321817 ) ) ;
#26092 = CARTESIAN_POINT ( 'NONE',  ( 5.959547316686252039, 18.96456592444089395, 7.851524054666477959 ) ) ;
#26093 = CARTESIAN_POINT ( 'NONE',  ( 4.967162193818129623, -43.02067033766018511, 2.375726030842427061 ) ) ;
#26094 = EDGE_CURVE ( 'NONE', #40325, #52094, #4061, .T. ) ;
#26095 = FACE_OUTER_BOUND ( 'NONE', #58572, .T. ) ;
#26096 = CARTESIAN_POINT ( 'NONE',  ( 0.6025881611877910160, -6.495537368246224297, 47.66695236827163740 ) ) ;
#26097 = ADVANCED_FACE ( 'NONE', ( #21232 ), #22605, .F. ) ;
#26098 = CARTESIAN_POINT ( 'NONE',  ( 2.301529144917015213, 7.543875168382506047, 47.43735140118867122 ) ) ;
#26099 = CARTESIAN_POINT ( 'NONE',  ( 0.3622758884714600280, -41.85013935980108357, 10.35929834645850001 ) ) ;
#26100 = CARTESIAN_POINT ( 'NONE',  ( 0.8560838555295158248, 5.603718208094640829, -46.57221463840858888 ) ) ;
#26101 = CARTESIAN_POINT ( 'NONE',  ( 0.5804410086790514622, -34.41390132670994007, 31.86225427258511544 ) ) ;
#26102 = FACE_OUTER_BOUND ( 'NONE', #50303, .T. ) ;
#26103 = CARTESIAN_POINT ( 'NONE',  ( 0.8744876279028306332, 46.86690837902563089, 14.62336997314605469 ) ) ;
#26104 = CARTESIAN_POINT ( 'NONE',  ( 4.691466044806102076, -33.74235639413347343, 29.14742760351052198 ) ) ;
#26105 = VECTOR ( 'NONE', #6417, 1000.000000000000114 ) ;
#26106 = DIRECTION ( 'NONE',  ( 0.000000000000000000, 0.000000000000000000, 1.000000000000000000 ) ) ;
#26107 = CARTESIAN_POINT ( 'NONE',  ( 0.8557997880470599172, -43.90420959842167292, -19.17299735372055736 ) ) ;
#26108 = CARTESIAN_POINT ( 'NONE',  ( 0.6016117650947691020, 48.26733837696657048, 9.045169995523039574 ) ) ;
#26110 = ORIENTED_EDGE ( 'NONE', *, *, #22187, .T. ) ;
#26109 = CARTESIAN_POINT ( 'NONE',  ( 2.643462169533613793, 47.42536612906428672, -7.637863311827113755 ) ) ;
#26111 = VERTEX_POINT ( 'NONE', #42219 ) ;
#26112 = EDGE_CURVE ( 'NONE', #55162, #23761, #46642, .T. ) ;
#26113 = CARTESIAN_POINT ( 'NONE',  ( 0.6021448801613057400, 17.20492824988890490, -45.99490822409718760 ) ) ;
#26114 = CARTESIAN_POINT ( 'NONE',  ( 0.8557997880470697982, -46.03118133706034598, 13.27832040216623355 ) ) ;
#26115 = CARTESIAN_POINT ( 'NONE',  ( 0.9722240741986363233, 6.177112427866467748, -42.46141200043694397 ) ) ;
#26116 = ORIENTED_EDGE ( 'NONE', *, *, #5425, .T. ) ;
#26117 = EDGE_CURVE ( 'NONE', #16449, #21472, #41441, .T. ) ;
#26118 = ORIENTED_EDGE ( 'NONE', *, *, #44450, .T. ) ;
#26119 = CARTESIAN_POINT ( 'NONE',  ( 4.390527457369402420, -29.77348744142276971, 32.30672967361536507 ) ) ;
#26120 = FACE_OUTER_BOUND ( 'NONE', #21048, .T. ) ;
#26121 = CARTESIAN_POINT ( 'NONE',  ( 5.959547316686252039, 5.308980600728181010, 19.82715097195164233 ) ) ;
#26122 = UNCERTAINTY_MEASURE_WITH_UNIT (LENGTH_MEASURE( 1.000000000000000082E-05 ), #60994, 'distance_accuracy_value', 'NONE');
#26123 = VERTEX_POINT ( 'NONE', #36273 ) ;
#26124 = EDGE_LOOP ( 'NONE', ( #8553, #54003, #4427, #49474 ) ) ;
#26125 = CARTESIAN_POINT ( 'NONE',  ( 0.5809828226811617480, 47.89273459658653564, 0.5448590168534191980 ) ) ;
#26126 = CARTESIAN_POINT ( 'NONE',  ( 3.680882792899937250, -39.15943299201968841, -27.71664061799134515 ) ) ;
#26127 = CARTESIAN_POINT ( 'NONE',  ( 0.8760168074887076939, -7.161346975773376755, -47.56749362999710939 ) ) ;
#26128 = ORIENTED_EDGE ( 'NONE', *, *, #43030, .T. ) ;
#26129 = B_SPLINE_CURVE_WITH_KNOTS ( 'NONE', 3,
 ( #57165, #9266, #47809, #52173 ),
 .UNSPECIFIED., .F., .F.,
 ( 4, 4 ),
 ( 2.178848519881467612E-17, 0.004559932413162186803 ),
 .UNSPECIFIED. ) ;
#26130 = DIRECTION ( 'NONE',  ( 0.000000000000000000, 0.000000000000000000, 1.000000000000000000 ) ) ;
#26131 = CARTESIAN_POINT ( 'NONE',  ( 7.000000000000006217, 1.285836671513502826E-15, -1.348150961071066192E-31 ) ) ;
#26132 = EDGE_CURVE ( 'NONE', #14444, #16055, #40740, .T. ) ;
#26133 = CARTESIAN_POINT ( 'NONE',  ( 0.5988103564986354543, -24.57719524907214037, -41.35593036885926921 ) ) ;
#26134 = ORIENTED_EDGE ( 'NONE', *, *, #5508, .F. ) ;
#26135 = ORIENTED_EDGE ( 'NONE', *, *, #27579, .F. ) ;
#26136 = DIRECTION ( 'NONE',  ( -1.000000000000000000, -0.000000000000000000, -0.000000000000000000 ) ) ;
#26137 = CARTESIAN_POINT ( 'NONE',  ( 4.322998006666179727, -22.13465289016656712, 42.57894920390090476 ) ) ;
#26138 = ORIENTED_EDGE ( 'NONE', *, *, #55295, .F. ) ;
#26139 = CARTESIAN_POINT ( 'NONE',  ( 0.6026777506516367566, -48.68174550883031770, 6.452444873898463662 ) ) ;
#26140 = DIRECTION ( 'NONE',  ( 0.000000000000000000, 0.000000000000000000, 1.000000000000000000 ) ) ;
#26141 = CARTESIAN_POINT ( 'NONE',  ( 5.894904586330512508, -11.93156318452989950, -16.19157842939388914 ) ) ;
#26142 = CARTESIAN_POINT ( 'NONE',  ( 3.390910168358336918, -43.82545004431705138, -3.664295968764966549 ) ) ;
#26143 = B_SPLINE_CURVE_WITH_KNOTS ( 'NONE', 3,
 ( #40761, #7183, #55424, #12548, #31640, #11614 ),
 .UNSPECIFIED., .F., .F.,
 ( 4, 2, 4 ),
 ( 6.106282077343213345E-18, 0.0002291472222819927729, 0.0004582944445639794743 ),
 .UNSPECIFIED. ) ;
#26144 = VERTEX_POINT ( 'NONE', #26545 ) ;
#26145 = CARTESIAN_POINT ( 'NONE',  ( 0.9754642270333674370, -30.21634823122148106, -30.46484943293189218 ) ) ;
#26146 = CARTESIAN_POINT ( 'NONE',  ( 0.5997462898726536595, -34.91088276334750873, 34.53667463477217581 ) ) ;
#26147 = VECTOR ( 'NONE', #60299, 1000.000000000000114 ) ;
#26148 = CARTESIAN_POINT ( 'NONE',  ( 0.5848930533535030563, -34.90273318373206735, 31.32207366527264725 ) ) ;
#26149 = CARTESIAN_POINT ( 'NONE',  ( 0.9757892942422823346, -21.49867881049921081, -37.13414688883487713 ) ) ;
#26150 = ORIENTED_EDGE ( 'NONE', *, *, #44242, .T. ) ;
#26151 = PLANE ( 'NONE',  #28517 ) ;
#26152 = CARTESIAN_POINT ( 'NONE',  ( 5.960721111146673579, 2.685391721745764571, 20.34914600876576074 ) ) ;
#26153 = CARTESIAN_POINT ( 'NONE',  ( 0.7954190325252783467, 48.09103420665682194, -0.8690070772084271811 ) ) ;
#26154 = CARTESIAN_POINT ( 'NONE',  ( -6.016761891674565099, -4.880293656735092078, 18.20023637398597671 ) ) ;
#26155 =( BOUNDED_SURFACE ( )  B_SPLINE_SURFACE ( 3, 1, ( 
 ( #36629, #46645 ),
 ( #51009, #51312 ),
 ( #23137, #8102 ),
 ( #42266, #12214 ) ),
 .UNSPECIFIED., .F., .F., .F. ) 
 B_SPLINE_SURFACE_WITH_KNOTS ( ( 4, 4 ),
 ( 2, 2 ),
 ( 0.000000000000000000, 1.000000000000000000 ),
 ( 0.000000000000000000, 1.000000000000000000 ),
 .UNSPECIFIED. ) 
 GEOMETRIC_REPRESENTATION_ITEM ( )  RATIONAL_B_SPLINE_SURFACE ( (
 ( 1.000000000000000000, 1.000000000000000000),
 ( 0.9953040768229005630, 0.8617119497784937465),
 ( 0.9953040768229005630, 0.8617119497784937465),
 ( 1.000000000000000000, 1.000000000000000000) ) ) 
 REPRESENTATION_ITEM ( '' )  SURFACE ( )  );
#26156 = EDGE_LOOP ( 'NONE', ( #4439, #9, #15157, #33489, #959 ) ) ;
#26157 = CARTESIAN_POINT ( 'NONE',  ( 4.999999999999997335, -2.784000523420839360E-13, 80.00000000000001421 ) ) ;
#26158 = CARTESIAN_POINT ( 'NONE',  ( 0.1102847568649952675, -42.74337176234133295, 5.720244683737878866 ) ) ;
#26159 = CARTESIAN_POINT ( 'NONE',  ( 0.1064266379913941241, 25.80493164505204007, -34.55203636557783398 ) ) ;
#26160 = DIRECTION ( 'NONE',  ( -1.000000000000000000, -0.000000000000000000, -0.000000000000000000 ) ) ;
#26161 = CARTESIAN_POINT ( 'NONE',  ( 1.834102595619085063, 21.51996898927949431, 38.43291141142098155 ) ) ;
#26162 = CARTESIAN_POINT ( 'NONE',  ( 0.9752132459055877778, 42.90780255730422255, -0.2329632697545410136 ) ) ;
#26163 = CARTESIAN_POINT ( 'NONE',  ( 0.6067099128993237445, -47.57459301987699263, -5.548253864790892997 ) ) ;
#26164 = CARTESIAN_POINT ( 'NONE',  ( 0.1103744047535531458, -41.64495780681030368, -11.19884698423352276 ) ) ;
#26166 = ADVANCED_FACE ( 'NONE', ( #36900 ), #33412, .F. ) ;
#26165 = LINE ( 'NONE', #2346, #46862 ) ;
#26167 = CARTESIAN_POINT ( 'NONE',  ( 0.8753041380234471980, 10.05717963662801218, 48.06237057854693973 ) ) ;
#26168 = DIRECTION ( 'NONE',  ( 0.000000000000000000, 0.000000000000000000, -1.000000000000000000 ) ) ;
#26169 = ORIENTED_EDGE ( 'NONE', *, *, #16366, .F. ) ;
#26170 = EDGE_CURVE ( 'NONE', #1120, #19414, #13809, .T. ) ;
#26171 = CARTESIAN_POINT ( 'NONE',  ( 0.8560838555295223751, 46.89922841446243496, -0.9138972643637069959 ) ) ;
#26172 = CARTESIAN_POINT ( 'NONE',  ( 10.00000000000000533, -2.649999999999153033, -80.00000000000004263 ) ) ;
#26173 = CARTESIAN_POINT ( 'NONE',  ( 0.7056555295713275999, -13.20840017674985845, -46.04438433984169876 ) ) ;
#26174 = CARTESIAN_POINT ( 'NONE',  ( 0.5824936645240084143, -34.53516756923718134, -31.72633574816064694 ) ) ;
#26175 = B_SPLINE_CURVE_WITH_KNOTS ( 'NONE', 3,
 ( #40058, #16845, #30925, #2086, #7090, #2405 ),
 .UNSPECIFIED., .F., .F.,
 ( 4, 2, 4 ),
 ( 1.474357996003774831E-17, 0.0002293319059085077044, 0.0004586638118170006636 ),
 .UNSPECIFIED. ) ;
#26176 = CARTESIAN_POINT ( 'NONE',  ( 5.960221823109900008, 19.82478916873567698, 5.317678907195506177 ) ) ;
#26177 = FACE_OUTER_BOUND ( 'NONE', #34995, .T. ) ;
#26178 = PRODUCT_CONTEXT ( 'NONE', #20346, 'mechanical' ) ;
#26179 = CARTESIAN_POINT ( 'NONE',  ( 0.1073791018717578927, 37.10214135362858912, 21.98088480513677823 ) ) ;
#26181 = ORIENTED_EDGE ( 'NONE', *, *, #16646, .F. ) ;
#26180 = CARTESIAN_POINT ( 'NONE',  ( 5.917102823773431552, -18.51268610137615056, -7.859400191086862719 ) ) ;
#26182 = ORIENTED_EDGE ( 'NONE', *, *, #2605, .F. ) ;
#26183 = DIRECTION ( 'NONE',  ( 0.000000000000000000, 0.000000000000000000, 1.000000000000000000 ) ) ;
#26184 = CARTESIAN_POINT ( 'NONE',  ( 5.965394784446460541, 17.76824826579340666, 10.27521535480992654 ) ) ;
#26185 = DIRECTION ( 'NONE',  ( 0.1024043820194936311, -0.2447326578667395336, 0.9641676559171059591 ) ) ;
#26186 = EDGE_CURVE ( 'NONE', #9208, #45826, #61586, .T. ) ;
#26187 = ORIENTED_EDGE ( 'NONE', *, *, #56045, .F. ) ;
#26188 = FACE_OUTER_BOUND ( 'NONE', #9222, .T. ) ;
#26189 = LINE ( 'NONE', #45026, #32206 ) ;
#26190 = CARTESIAN_POINT ( 'NONE',  ( 0.1129192098497455998, 43.99990943031669843, 3.310552508129313232 ) ) ;
#26191 = CIRCLE ( 'NONE', #4121, 7.500000000000022204 ) ;
#26192 = ORIENTED_EDGE ( 'NONE', *, *, #29687, .T. ) ;
#26193 = ORIENTED_EDGE ( 'NONE', *, *, #26602, .F. ) ;
#26194 = FACE_OUTER_BOUND ( 'NONE', #26278, .T. ) ;
#26195 = CARTESIAN_POINT ( 'NONE',  ( 0.6000166863083106206, 48.30184070261004337, -8.874438937089886181 ) ) ;
#26196 = CARTESIAN_POINT ( 'NONE',  ( 5.860006189529246790, -15.52021937683308295, 45.66786516969924747 ) ) ;
#26197 = ORIENTED_EDGE ( 'NONE', *, *, #33249, .F. ) ;
#26198 = ORIENTED_EDGE ( 'NONE', *, *, #47910, .F. ) ;
#26199 = CARTESIAN_POINT ( 'NONE',  ( -6.078726893082806448, 9.979253153318998315, -16.46841060244408794 ) ) ;
#26200 = CARTESIAN_POINT ( 'NONE',  ( -79.49999999999975842, -5.510910596163058790E-15, 1.848892746611746419E-29 ) ) ;
#26201 = ORIENTED_EDGE ( 'NONE', *, *, #57238, .F. ) ;
#26202 = CARTESIAN_POINT ( 'NONE',  ( 0.1119898979215347840, 33.23178737380685988, -29.02773873717895015 ) ) ;
#26203 = CARTESIAN_POINT ( 'NONE',  ( 0.9745511491811753579, 41.53317535253989234, -10.77620558745893931 ) ) ;
#26204 = EDGE_LOOP ( 'NONE', ( #43828, #7226, #31375, #10873 ) ) ;
#26205 = CARTESIAN_POINT ( 'NONE',  ( 0.9730545539215883499, -33.73144377768539215, -26.52009130076805832 ) ) ;
#26206 = DIRECTION ( 'NONE',  ( 0.9848077530122079093, 0.1736481776669314137, -2.220446049250313081E-16 ) ) ;
#26207 = ORIENTED_EDGE ( 'NONE', *, *, #2519, .F. ) ;
#26208 = CARTESIAN_POINT ( 'NONE',  ( 5.838029081930955932, 42.14833990873909642, 21.32094043634829461 ) ) ;
#26209 = FACE_OUTER_BOUND ( 'NONE', #40495, .T. ) ;
#26210 = CARTESIAN_POINT ( 'NONE',  ( 0.5809828226811617480, 41.74875432577682233, -23.47450554821666202 ) ) ;
#26211 = VERTEX_POINT ( 'NONE', #31553 ) ;
#26212 = EDGE_CURVE ( 'NONE', #9808, #6747, #38443, .T. ) ;
#26213 = PLANE ( 'NONE',  #26733 ) ;
#26214 = DIRECTION ( 'NONE',  ( 0.000000000000000000, -0.5000000000000013323, -0.8660254037844380415 ) ) ;
#26215 = ORIENTED_EDGE ( 'NONE', *, *, #42768, .F. ) ;
#26216 = CARTESIAN_POINT ( 'NONE',  ( 3.238018933889920792, 8.164940828002086093, -10.61796749113866767 ) ) ;
#26217 = ORIENTED_EDGE ( 'NONE', *, *, #19977, .T. ) ;
#26218 = CARTESIAN_POINT ( 'NONE',  ( 0.9780106845699481077, 3.882692594035769496, 41.72835899811612848 ) ) ;
#26219 = EDGE_CURVE ( 'NONE', #7367, #2003, #24284, .T. ) ;
#26220 = ORIENTED_EDGE ( 'NONE', *, *, #37568, .T. ) ;
#26221 = CARTESIAN_POINT ( 'NONE',  ( -6.016761891674565099, 0.003433883960047550993, -18.84319130225482297 ) ) ;
#26222 = CARTESIAN_POINT ( 'NONE',  ( 0.6028777368367060907, -48.69304970598422955, -6.366061548683123128 ) ) ;
#26223 = CARTESIAN_POINT ( 'NONE',  ( 0.1139756605157201813, -43.70943680385401819, 6.036584629152037529 ) ) ;
#26224 = ORIENTED_EDGE ( 'NONE', *, *, #53242, .F. ) ;
#26225 = CARTESIAN_POINT ( 'NONE',  ( 0.000000000000000000, 0.000000000000000000, 0.000000000000000000 ) ) ;
#26226 = CARTESIAN_POINT ( 'NONE',  ( 0.5807400328401637335, 33.48217046439159361, -34.25275203086200548 ) ) ;
#26227 = CARTESIAN_POINT ( 'NONE',  ( 2.643462169533613793, 38.93558293168500484, 28.13401304854733453 ) ) ;
#26228 = ORIENTED_EDGE ( 'NONE', *, *, #42887, .F. ) ;
#26229 = CIRCLE ( 'NONE', #28198, 47.91270532121795611 ) ;
#26230 = ORIENTED_EDGE ( 'NONE', *, *, #19576, .F. ) ;
#26231 = AXIS2_PLACEMENT_3D ( 'NONE', #1026, #20162, #58330 ) ;
#26232 = DIRECTION ( 'NONE',  ( 1.000000000000000000, 0.000000000000000000, 0.000000000000000000 ) ) ;
#26233 = FACE_OUTER_BOUND ( 'NONE', #26273, .T. ) ;
#26234 = CARTESIAN_POINT ( 'NONE',  ( 0.9790850452238875068, 38.56342381347958792, -16.40730550837503898 ) ) ;
#26235 = CARTESIAN_POINT ( 'NONE',  ( 0.3622758884714600280, 41.85013935980101962, -10.35929834645879133 ) ) ;
#26236 = CARTESIAN_POINT ( 'NONE',  ( -14.84250595937556483, -4.999999999999993783, 6.123233995736803753E-16 ) ) ;
#26237 = CARTESIAN_POINT ( 'NONE',  ( 3.238931869106854489, 36.28407486357521350, -23.06038324659529337 ) ) ;
#26238 = ORIENTED_EDGE ( 'NONE', *, *, #10690, .T. ) ;
#26239 = EDGE_CURVE ( 'NONE', #33551, #56726, #49612, .T. ) ;
#26240 = CARTESIAN_POINT ( 'NONE',  ( 4.962356264823600149, -40.47344704301802665, 11.53844366967928892 ) ) ;
#26241 = CARTESIAN_POINT ( 'NONE',  ( 4.975801465491695552, -46.87746200127462970, 9.906103548667402947 ) ) ;
#26242 = ORIENTED_EDGE ( 'NONE', *, *, #23480, .T. ) ;
#26243 = EDGE_CURVE ( 'NONE', #39259, #17964, #57805, .T. ) ;
#26244 = CARTESIAN_POINT ( 'NONE',  ( 0.8551540677456715978, 41.94570365541202506, 23.16399837394560635 ) ) ;
#26245 = CARTESIAN_POINT ( 'NONE',  ( 2.500000000000000000, -1.178949249685214307, 2.042000000000001592 ) ) ;
#26246 = CARTESIAN_POINT ( 'NONE',  ( 3.238741278300274029, 40.38334873621882082, -14.74792908357263066 ) ) ;
#26247 = CARTESIAN_POINT ( 'NONE',  ( 1.830465331921978134, -11.34470899496544405, -42.56375962832630222 ) ) ;
#26248 = DIRECTION ( 'NONE',  ( 0.000000000000000000, 0.000000000000000000, 1.000000000000000000 ) ) ;
#26249 = CARTESIAN_POINT ( 'NONE',  ( 3.660176727303400934, -20.10773453922317344, 43.62748706623516171 ) ) ;
#26250 = CARTESIAN_POINT ( 'NONE',  ( 4.291220156522060236, 2.567299637375230592, -47.04038658299514708 ) ) ;
#26251 = EDGE_CURVE ( 'NONE', #48322, #44297, #47943, .T. ) ;
#26252 = CARTESIAN_POINT ( 'NONE',  ( 0.1158816050234198758, -12.55998807466990819, -42.29880306662720102 ) ) ;
#26253 =( BOUNDED_SURFACE ( )  B_SPLINE_SURFACE ( 3, 1, ( 
 ( #42170, #36223 ),
 ( #61227, #18349 ),
 ( #56530, #4203 ),
 ( #55287, #12411 ) ),
 .UNSPECIFIED., .F., .F., .F. ) 
 B_SPLINE_SURFACE_WITH_KNOTS ( ( 4, 4 ),
 ( 2, 2 ),
 ( 0.000000000000000000, 1.000000000000000000 ),
 ( 0.000000000000000000, 1.000000000000000000 ),
 .UNSPECIFIED. ) 
 GEOMETRIC_REPRESENTATION_ITEM ( )  RATIONAL_B_SPLINE_SURFACE ( (
 ( 1.000000000000000000, 1.000000000000000000),
 ( 0.9754377213608244057, 0.9999580625633939235),
 ( 0.9754377213608244057, 0.9999580625633939235),
 ( 1.000000000000000000, 1.000000000000000000) ) ) 
 REPRESENTATION_ITEM ( '' )  SURFACE ( )  );
#26254 = CARTESIAN_POINT ( 'NONE',  ( 0.5998501479064708430, -37.84527566984837677, -29.69975237324600315 ) ) ;
#26255 = CARTESIAN_POINT ( 'NONE',  ( 0.5850706913938534814, 6.431767090162812117, 47.46255051844956085 ) ) ;
#26256 = CARTESIAN_POINT ( 'NONE',  ( 8.000000000000007105, -56.56854249492410958, 56.56854249492351983 ) ) ;
#26257 = CARTESIAN_POINT ( 'NONE',  ( 5.974727161628369032, 7.840226266082271245, 18.96851388233661595 ) ) ;
#26258 = B_SPLINE_CURVE_WITH_KNOTS ( 'NONE', 3,
 ( #1975, #36455, #16103, #16716, #2596, #7923 ),
 .UNSPECIFIED., .F., .F.,
 ( 4, 2, 4 ),
 ( 8.560751122900633232E-17, 0.0002293366620881451474, 0.0004586733241762046970 ),
 .UNSPECIFIED. ) ;
#26259 = DIRECTION ( 'NONE',  ( 0.000000000000000000, 0.000000000000000000, 1.000000000000000000 ) ) ;
#26260 = CARTESIAN_POINT ( 'NONE',  ( 0.9787464366903563251, 9.542966726804086974, 40.80766813898550538 ) ) ;
#26261 = ADVANCED_FACE ( 'NONE', ( #24628 ), #18580, .F. ) ;
#26262 = CARTESIAN_POINT ( 'NONE',  ( 0.7948884756798486606, 40.66950405776249511, 27.50800036890706579 ) ) ;
#26263 = CARTESIAN_POINT ( 'NONE',  ( 0.7057020205115004385, -47.37450661940665242, -7.085441699094105594 ) ) ;
#26264 = B_SPLINE_CURVE_WITH_KNOTS ( 'NONE', 3,
 ( #1075, #19916, #29282, #57772, #58082, #5756 ),
 .UNSPECIFIED., .F., .F.,
 ( 4, 2, 4 ),
 ( 0.000000000000000000, 0.0002291966416970790514, 0.0004583932833941581028 ),
 .UNSPECIFIED. ) ;
#26265 =( BOUNDED_SURFACE ( )  B_SPLINE_SURFACE ( 3, 1, ( 
 ( #60186, #17297 ),
 ( #8483, #31388 ),
 ( #35799, #36416 ),
 ( #55482, #31700 ) ),
 .UNSPECIFIED., .F., .F., .F. ) 
 B_SPLINE_SURFACE_WITH_KNOTS ( ( 4, 4 ),
 ( 2, 2 ),
 ( 0.000000000000000000, 1.000000000000000000 ),
 ( 0.000000000000000000, 1.000000000000000000 ),
 .UNSPECIFIED. ) 
 GEOMETRIC_REPRESENTATION_ITEM ( )  RATIONAL_B_SPLINE_SURFACE ( (
 ( 1.000000000000000000, 1.000000000000000000),
 ( 0.7282232189291694135, 0.9929344683865672927),
 ( 0.7282232189291694135, 0.9929344683865672927),
 ( 1.000000000000000000, 1.000000000000000000) ) ) 
 REPRESENTATION_ITEM ( '' )  SURFACE ( )  );
#26266 = ORIENTED_EDGE ( 'NONE', *, *, #40389, .F. ) ;
#26267 = B_SPLINE_CURVE_WITH_KNOTS ( 'NONE', 3,
 ( #48066, #13954, #38077, #52130 ),
 .UNSPECIFIED., .F., .F.,
 ( 4, 4 ),
 ( 0.000000000000000000, 0.004444103432399268763 ),
 .UNSPECIFIED. ) ;
#26268 = B_SPLINE_CURVE_WITH_KNOTS ( 'NONE', 3,
 ( #25940, #30948, #50056, #45680, #3569, #42751 ),
 .UNSPECIFIED., .F., .F.,
 ( 4, 2, 4 ),
 ( 1.084202172485504434E-19, 0.0002445244328975360471, 0.0004890488657950719858 ),
 .UNSPECIFIED. ) ;
#26269 = CARTESIAN_POINT ( 'NONE',  ( 0.1100053167205931048, 43.12409768020066281, -0.1794603581039966034 ) ) ;
#26270 = CARTESIAN_POINT ( 'NONE',  ( 0.1158816050234198758, -38.44899847554016503, -21.64755315348761755 ) ) ;
#26271 = CARTESIAN_POINT ( 'NONE',  ( 5.901764892641307547, 30.56558498816019309, -38.25880920482542535 ) ) ;
#26272 = CARTESIAN_POINT ( 'NONE',  ( 0.5782707292762423457, 46.57382484760229602, 5.533099743586860519 ) ) ;
#26273 = EDGE_LOOP ( 'NONE', ( #45324, #31308, #15189, #3397 ) ) ;
#26274 = CARTESIAN_POINT ( 'NONE',  ( 3.660176727303400046, -30.71420464230597247, 36.93665184075209851 ) ) ;
#26275 = CARTESIAN_POINT ( 'NONE',  ( 0.3622758884714600280, -10.35929834645893699, -41.85013935980099120 ) ) ;
#26276 = CARTESIAN_POINT ( 'NONE',  ( 0.6024113833632039894, -14.18099286842164020, 47.01533058872011850 ) ) ;
#26277 = VECTOR ( 'NONE', #6948, 1000.000000000000227 ) ;
#26278 = EDGE_LOOP ( 'NONE', ( #29168, #39820, #22046, #41055 ) ) ;
#26279 = CARTESIAN_POINT ( 'NONE',  ( 4.694002226626921015, -40.92287315640955114, -20.08987864748195307 ) ) ;
#26280 = ORIENTED_EDGE ( 'NONE', *, *, #47, .T. ) ;
#26281 = EDGE_CURVE ( 'NONE', #59424, #46608, #2890, .T. ) ;
#26282 = CARTESIAN_POINT ( 'NONE',  ( 1.227938101723756947, -39.96870412324324917, -15.63977281655884077 ) ) ;
#26283 = CARTESIAN_POINT ( 'NONE',  ( 4.975801465491694664, -26.14269827151650816, -40.15204426031524321 ) ) ;
#26284 = ORIENTED_EDGE ( 'NONE', *, *, #45848, .T. ) ;
#26285 = CARTESIAN_POINT ( 'NONE',  ( 0.5998501479064708430, -46.60114184914326074, 11.94461217097388328 ) ) ;
#26286 = ORIENTED_EDGE ( 'NONE', *, *, #6897, .T. ) ;
#26287 = CARTESIAN_POINT ( 'NONE',  ( 3.782625744892855746, -35.60519336021494041, -22.34968254532283183 ) ) ;
#26288 = CARTESIAN_POINT ( 'NONE',  ( 0.1155031312995260795, 20.25957159725990664, 39.19810443410890599 ) ) ;
#26289 = EDGE_CURVE ( 'NONE', #44212, #14421, #18935, .T. ) ;
#26290 = VERTEX_POINT ( 'NONE', #19316 ) ;
#26291 = B_SPLINE_CURVE_WITH_KNOTS ( 'NONE', 3,
 ( #54589, #13260, #61147, #8530, #42092, #31743, #2909, #26725, #50834, #55216, #12963, #12339, #3827, #50527, #32363, #55839 ),
 .UNSPECIFIED., .F., .F.,
 ( 4, 3, 3, 3, 3, 4 ),
 ( 1.868480190406682863E-17, 0.0002618515315864417057, 0.0003927756766341974491, 0.0005236998216950559384, 0.0007855159896329909830, 0.001047349442285930039 ),
 .UNSPECIFIED. ) ;
#26292 = EDGE_LOOP ( 'NONE', ( #22259, #6952, #27656, #36658 ) ) ;
#26293 = EDGE_CURVE ( 'NONE', #30775, #52200, #61906, .T. ) ;
#26294 = CARTESIAN_POINT ( 'NONE',  ( 2.618530812446111078, 21.34567399517355213, 41.88184560033108284 ) ) ;
#26295 = EDGE_LOOP ( 'NONE', ( #51605, #60356, #44496, #27162 ) ) ;
#26296 = CARTESIAN_POINT ( 'NONE',  ( 0.1135584504625008484, -1.845938478027137730, 44.08565031016998148 ) ) ;
#26297 = AXIS2_PLACEMENT_3D ( 'NONE', #15418, #34531, #25115 ) ;
#26298 = ORIENTED_EDGE ( 'NONE', *, *, #23361, .T. ) ;
#26299 = ADVANCED_FACE ( 'NONE', ( #15237 ), #14316, .F. ) ;
#26300 = VERTEX_POINT ( 'NONE', #42829 ) ;
#26301 = CARTESIAN_POINT ( 'NONE',  ( 0.9756950546413932779, -0.09673755062766570267, -42.90834738653779823 ) ) ;
#26303 = EDGE_CURVE ( 'NONE', #40451, #35096, #42950, .T. ) ;
#26302 = CARTESIAN_POINT ( 'NONE',  ( 4.967162193818130511, 0.000000000000000000, 0.000000000000000000 ) ) ;
#26304 = CARTESIAN_POINT ( 'NONE',  ( 0.5797568599927139799, -44.50349610438583170, 14.78729668187938806 ) ) ;
#26305 = CARTESIAN_POINT ( 'NONE',  ( 0.1103310638050662013, -16.57910240621667342, 39.81020119244053035 ) ) ;
#26306 = CARTESIAN_POINT ( 'NONE',  ( 0.7048096507298579061, 41.23648859290891266, 24.78213711671612884 ) ) ;
#26307 = ORIENTED_EDGE ( 'NONE', *, *, #42124, .T. ) ;
#26308 = CARTESIAN_POINT ( 'NONE',  ( 0.9757402383260944667, 11.02350435907904469, 41.46830379850858606 ) ) ;
#26309 = CARTESIAN_POINT ( 'NONE',  ( 5.981074661064941900, 2.687517936919997741, -20.34795181394746066 ) ) ;
#26310 = CARTESIAN_POINT ( 'NONE',  ( 5.901764892641288895, -37.31543133725893568, -31.71040919877874487 ) ) ;
#26311 = VERTEX_POINT ( 'NONE', #9588 ) ;
#26312 = EDGE_LOOP ( 'NONE', ( #57064, #31218, #29729, #35804 ) ) ;
#26313 = CARTESIAN_POINT ( 'NONE',  ( -6.017396004339687465, 18.84316306185412415, 0.001173774849048346645 ) ) ;
#26314 = CARTESIAN_POINT ( 'NONE',  ( -6.010958268070873523, 2.445171577616032987, -18.68413620842261835 ) ) ;
#26315 = CARTESIAN_POINT ( 'NONE',  ( 0.9785694773339231878, 40.47783839118113747, -10.85725586380356766 ) ) ;
#26316 = ORIENTED_EDGE ( 'NONE', *, *, #28935, .T. ) ;
#26317 = CARTESIAN_POINT ( 'NONE',  ( 4.549368137175248350, -28.46244473166695954, 32.13400537129875545 ) ) ;
#26318 = CARTESIAN_POINT ( 'NONE',  ( -4.000000000000000000, 2.309401076758531346, -5.242734410091827613 ) ) ;
#26319 = CARTESIAN_POINT ( 'NONE',  ( -19.85996189817664259, -12.46576327517147043, -0.9332767033992659389 ) ) ;
#26320 = EDGE_CURVE ( 'NONE', #35399, #49767, #60886, .T. ) ;
#26321 = EDGE_LOOP ( 'NONE', ( #41544, #27662, #366, #7862 ) ) ;
#26322 = CARTESIAN_POINT ( 'NONE',  ( 4.975610109902397937, -46.23629923292386934, 15.95788333023201488 ) ) ;
#26323 = ORIENTED_EDGE ( 'NONE', *, *, #17712, .F. ) ;
#26324 = EDGE_CURVE ( 'NONE', #8570, #33938, #40665, .T. ) ;
#26325 = CARTESIAN_POINT ( 'NONE',  ( 0.9756008150404616996, -33.95486284030242530, 26.23365443298902377 ) ) ;
#26326 = CARTESIAN_POINT ( 'NONE',  ( 5.981074661064941900, -20.35019299530690162, 2.670494474391653661 ) ) ;
#26327 = B_SPLINE_CURVE_WITH_KNOTS ( 'NONE', 3,
 ( #2445, #55067, #26573, #17494, #36613, #12194, #17804, #8084, #55374, #3671, #50675, #46319, #21571, #12812, #46026, #2756, #31588, #55678, #3361, #51596, #22497, #13116, #7764, #3065, #32523 ),
 .UNSPECIFIED., .F., .F.,
 ( 4, 3, 3, 3, 3, 3, 3, 3, 4 ),
 ( 6.254634441385501517E-18, 0.0005656085177311384474, 0.001131215744874498321, 0.001696821861372765266, 0.002262427090022496850, 0.002828031679238745492, 0.003393635864401603128, 0.003977030878808130755, 0.004561030005651157265 ),
 .UNSPECIFIED. ) ;
#26328 = AXIS2_PLACEMENT_3D ( 'NONE', #50609, #21815, #49384 ) ;
#26329 = ADVANCED_FACE ( 'NONE', ( #25541 ), #35843, .T. ) ;
#26330 = ORIENTED_EDGE ( 'NONE', *, *, #29823, .F. ) ;
#26331 = CARTESIAN_POINT ( 'NONE',  ( 0.9757402383260955769, 21.52772413548534658, -37.11731350497332471 ) ) ;
#26332 = CARTESIAN_POINT ( 'NONE',  ( 2.528100132419517365, -11.27643546515609962, 40.43631760969642386 ) ) ;
#26333 = FACE_OUTER_BOUND ( 'NONE', #22613, .T. ) ;
#26334 = CARTESIAN_POINT ( 'NONE',  ( 4.549368137175248350, -2.596185425821630588, -42.84816078363929392 ) ) ;
#26335 = CARTESIAN_POINT ( 'NONE',  ( 0.5850706913938534814, 12.22095376872101546, -46.31100969101474618 ) ) ;
#26336 = LINE ( 'NONE', #31352, #47437 ) ;
#26337 = CARTESIAN_POINT ( 'NONE',  ( -1.129531546211690163, 0.000000000000000000, -6.887500000000022382 ) ) ;
#26338 = EDGE_CURVE ( 'NONE', #6976, #7392, #51827, .T. ) ;
#26339 = CARTESIAN_POINT ( 'NONE',  ( 4.956653778116975495, 20.77844580450561551, 43.37017594958062006 ) ) ;
#26340 = CIRCLE ( 'NONE', #7307, 43.08621763946400307 ) ;
#26341 = CARTESIAN_POINT ( 'NONE',  ( 4.958415959904820092, 37.15973263041097141, 26.12198737958135197 ) ) ;
#26342 = EDGE_CURVE ( 'NONE', #376, #12101, #45296, .T. ) ;
#26343 = CARTESIAN_POINT ( 'NONE',  ( 4.291220156522060236, 45.95810865397713485, 10.35573494518514792 ) ) ;
#26344 = CARTESIAN_POINT ( 'NONE',  ( 0.5832367798473383491, -28.94059862654968640, -38.16362489683119463 ) ) ;
#26345 = ORIENTED_EDGE ( 'NONE', *, *, #24741, .F. ) ;
#26346 = CARTESIAN_POINT ( 'NONE',  ( 1.479689385636123067, -2.586709720683578073, -43.98741613335128875 ) ) ;
#26347 = LINE ( 'NONE', #40177, #21555 ) ;
#26348 = CARTESIAN_POINT ( 'NONE',  ( 0.7413678028165009426, -42.40789325331365944, 12.08539124669933607 ) ) ;
#26349 = VERTEX_POINT ( 'NONE', #15851 ) ;
#26350 = CARTESIAN_POINT ( 'NONE',  ( 0.5998501479064699549, -44.64337787626236320, -17.92509395669093308 ) ) ;
#26351 = CARTESIAN_POINT ( 'NONE',  ( 0.7948884756798504370, 44.60603610063805036, -20.51828910968767872 ) ) ;
#26352 = DIRECTION ( 'NONE',  ( 0.000000000000000000, 1.000000000000000000, 0.000000000000000000 ) ) ;
#26353 = ORIENTED_EDGE ( 'NONE', *, *, #38511, .T. ) ;
#26354 = CARTESIAN_POINT ( 'NONE',  ( 0.8557997880470606944, -33.22501220301877112, -34.51495345639583689 ) ) ;
#26355 = CARTESIAN_POINT ( 'NONE',  ( 0.8557997880470599172, -46.03118133706016835, -13.27832040216687304 ) ) ;
#26356 = VERTEX_POINT ( 'NONE', #49651 ) ;
#26357 = FACE_OUTER_BOUND ( 'NONE', #30198, .T. ) ;
#26358 = EDGE_LOOP ( 'NONE', ( #36335, #15608, #7025, #7192 ) ) ;
#26359 = VERTEX_POINT ( 'NONE', #44677 ) ;
#26360 = CARTESIAN_POINT ( 'NONE',  ( 0.9757402383260942447, -5.684842778069517877, 42.53022961222601594 ) ) ;
#26361 = EDGE_CURVE ( 'NONE', #53602, #57538, #49969, .T. ) ;
#26362 = EDGE_LOOP ( 'NONE', ( #36153, #10217, #36262, #21 ) ) ;
#26363 = CARTESIAN_POINT ( 'NONE',  ( 0.7954196712028465122, 42.08256091708702940, -23.29293472883145455 ) ) ;
#26364 = ORIENTED_EDGE ( 'NONE', *, *, #4727, .F. ) ;
#26365 = EDGE_CURVE ( 'NONE', #44145, #32619, #13103, .T. ) ;
#26366 = CARTESIAN_POINT ( 'NONE',  ( 4.975610109902397937, 42.89797504594955058, -23.49921581872176191 ) ) ;
#26367 =( BOUNDED_SURFACE ( )  B_SPLINE_SURFACE ( 3, 1, ( 
 ( #15208, #8953 ),
 ( #33705, #52470 ),
 ( #56858, #28363 ),
 ( #33393, #4844 ) ),
 .UNSPECIFIED., .F., .F., .F. ) 
 B_SPLINE_SURFACE_WITH_KNOTS ( ( 4, 4 ),
 ( 2, 2 ),
 ( 0.000000000000000000, 1.000000000000000000 ),
 ( 0.000000000000000000, 1.000000000000000000 ),
 .UNSPECIFIED. ) 
 GEOMETRIC_REPRESENTATION_ITEM ( )  RATIONAL_B_SPLINE_SURFACE ( (
 ( 1.000000000000000000, 1.000000000000000000),
 ( 0.9953040768229005630, 0.8617119497784937465),
 ( 0.9953040768229005630, 0.8617119497784937465),
 ( 1.000000000000000000, 1.000000000000000000) ) ) 
 REPRESENTATION_ITEM ( '' )  SURFACE ( )  );
#26368 = CARTESIAN_POINT ( 'NONE',  ( 0.7044674535453004927, 37.93506595837544637, 31.18867572604858651 ) ) ;
#26369 = EDGE_CURVE ( 'NONE', #6519, #37845, #46717, .T. ) ;
#26370 = ORIENTED_EDGE ( 'NONE', *, *, #2679, .F. ) ;
#26371 = ADVANCED_FACE ( 'NONE', ( #40601 ), #5370, .F. ) ;
#26372 = FACE_OUTER_BOUND ( 'NONE', #58013, .T. ) ;
#26373 = B_SPLINE_CURVE_WITH_KNOTS ( 'NONE', 3,
 ( #54053, #53735, #29646, #10868, #24962, #30258 ),
 .UNSPECIFIED., .F., .F.,
 ( 4, 2, 4 ),
 ( 0.000000000000000000, 0.0002291966416970795664, 0.0004583932833941591328 ),
 .UNSPECIFIED. ) ;
#26374 = CARTESIAN_POINT ( 'NONE',  ( 0.8560838555295158248, -6.899551485031924614, -46.39794201672231111 ) ) ;
#26375 = CARTESIAN_POINT ( 'NONE',  ( 4.975801465491695552, 47.76942479135485797, -3.702618843596948039 ) ) ;
#26376 = CARTESIAN_POINT ( 'NONE',  ( 0.5806925824938502512, 27.37593026015236219, -38.07598724570169679 ) ) ;
#26378 = EDGE_CURVE ( 'NONE', #59637, #57224, #53713, .T. ) ;
#26377 = VERTEX_POINT ( 'NONE', #1106 ) ;
#26379 = COLOUR_RGB ( '', 0.40784314, 0.44705882, 0.49803922) ;
#26380 = ORIENTED_EDGE ( 'NONE', *, *, #23004, .F. ) ;
#26381 = DIRECTION ( 'NONE',  ( 1.000000000000000000, 1.836909530733573776E-16, 0.000000000000000000 ) ) ;
#26382 = CARTESIAN_POINT ( 'NONE',  ( 0.3622758884714730732, -6.444611261694294768, -42.62881903538208661 ) ) ;
#26383 = EDGE_CURVE ( 'NONE', #4156, #40797, #32512, .T. ) ;
#26384 = CARTESIAN_POINT ( 'NONE',  ( 0.5998501479064708430, -47.76154736470761719, 5.759754759339972274 ) ) ;
#26385 = VERTEX_POINT ( 'NONE', #35584 ) ;
#26386 = CARTESIAN_POINT ( 'NONE',  ( 0.1073791018717578927, 25.86618856530665767, 34.50606437925554815 ) ) ;
#26387 = CARTESIAN_POINT ( 'NONE',  ( 3.661921753701995463, 45.82839444823501651, 10.60138604763640835 ) ) ;
#26388 = CARTESIAN_POINT ( 'NONE',  ( 3.221118495291109163, 7.937357278700688745, -43.26383916265416474 ) ) ;
#26389 =( NAMED_UNIT ( * ) SI_UNIT ( $, .STERADIAN. ) SOLID_ANGLE_UNIT ( ) );
#26390 = B_SPLINE_CURVE_WITH_KNOTS ( 'NONE', 3,
 ( #47738, #57404, #13934, #4175 ),
 .UNSPECIFIED., .F., .F.,
 ( 4, 4 ),
 ( 0.000000000000000000, 0.005004948556313794025 ),
 .UNSPECIFIED. ) ;
#26391 = VERTEX_POINT ( 'NONE', #48735 ) ;
#26392 = ORIENTED_EDGE ( 'NONE', *, *, #42331, .T. ) ;
#26393 = CARTESIAN_POINT ( 'NONE',  ( 5.960721111146673579, -19.82454228767742066, -5.318514366754864220 ) ) ;
#26394 = CARTESIAN_POINT ( 'NONE',  ( 4.226256110419178924, 42.39738639032160705, 11.54508021873209422 ) ) ;
#26395 = CARTESIAN_POINT ( 'NONE',  ( 0.9758171775293927874, -16.41489794146152548, 39.64453667157740568 ) ) ;
#26396 = DIRECTION ( 'NONE',  ( -1.000000000000000000, 0.000000000000000000, 0.000000000000000000 ) ) ;
#26397 = CARTESIAN_POINT ( 'NONE',  ( 4.390527457369401532, -14.87174614414513485, -41.34025282037742954 ) ) ;
#26398 = CARTESIAN_POINT ( 'NONE',  ( 4.956653778116966613, 0.000000000000000000, 0.000000000000000000 ) ) ;
#26399 = LINE ( 'NONE', #40235, #16717 ) ;
#26400 = CARTESIAN_POINT ( 'NONE',  ( 4.691466044806102964, -42.11359095667479835, -14.64802401911215135 ) ) ;
#26401 = CARTESIAN_POINT ( 'NONE',  ( 0.8557997880470697982, -23.15977007032352475, 41.93815086860250574 ) ) ;
#26402 = CARTESIAN_POINT ( 'NONE',  ( 0.6067375320500711933, -41.82999795871622695, 23.33187539052113380 ) ) ;
#26403 = CARTESIAN_POINT ( 'NONE',  ( 0.3622758884714730732, -11.95365414648468594, -41.42293301073622303 ) ) ;
#26404 = CARTESIAN_POINT ( 'NONE',  ( 5.960221823109900008, 20.34928172836727356, 2.684531185214488413 ) ) ;
#26405 = CIRCLE ( 'NONE', #40441, 43.08621763946400307 ) ;
#26406 = CARTESIAN_POINT ( 'NONE',  ( 0.5835871038041854364, -13.76363918287266586, -44.83075606484005959 ) ) ;
#26407 = CARTESIAN_POINT ( 'NONE',  ( 4.553261556744873317, 1.182159483579998449, -43.91061448874312845 ) ) ;
#26408 = CARTESIAN_POINT ( 'NONE',  ( 1.227938101723756947, -26.79402671879305231, -33.52879263017890565 ) ) ;
#26409 = EDGE_CURVE ( 'NONE', #13823, #5867, #288, .T. ) ;
#26410 = CARTESIAN_POINT ( 'NONE',  ( 5.283180000000047727, 0.000000000000000000, 0.000000000000000000 ) ) ;
#26411 = CARTESIAN_POINT ( 'NONE',  ( 0.6041374136657476912, -47.71861871402585109, -6.106202762793307315 ) ) ;
#26412 = CARTESIAN_POINT ( 'NONE',  ( 0.8744876279028263033, 27.35388303025786882, 40.76904626731490566 ) ) ;
#26414 = ORIENTED_EDGE ( 'NONE', *, *, #47760, .F. ) ;
#26413 = CARTESIAN_POINT ( 'NONE',  ( 0.5806925824938499181, 23.01490136172973067, -40.85996423950240342 ) ) ;
#26415 = ORIENTED_EDGE ( 'NONE', *, *, #35059, .F. ) ;
#26416 = CARTESIAN_POINT ( 'NONE',  ( 0.000000000000000000, 0.000000000000000000, -5.599999999999999645 ) ) ;
#26417 = CARTESIAN_POINT ( 'NONE',  ( 0.5997462898726536595, 17.44942740672471260, -45.90282249842328355 ) ) ;
#26418 = CARTESIAN_POINT ( 'NONE',  ( 0.5997462898726536595, 32.62638226927734308, -36.70246327105708417 ) ) ;
#26419 = VERTEX_POINT ( 'NONE', #16159 ) ;
#26420 = ORIENTED_EDGE ( 'NONE', *, *, #61917, .F. ) ;
#26421 = CARTESIAN_POINT ( 'NONE',  ( 0.8744876279028306332, -47.70753782033967383, -11.59055156152427557 ) ) ;
#26422 = CIRCLE ( 'NONE', #30398, 42.08604991992415023 ) ;
#26423 = CARTESIAN_POINT ( 'NONE',  ( 0.1129192098497447394, -38.20615368646970467, 22.07354996983974260 ) ) ;
#26424 = ORIENTED_EDGE ( 'NONE', *, *, #11878, .T. ) ;
#26425 = ORIENTED_EDGE ( 'NONE', *, *, #5654, .F. ) ;
#26426 = FACE_OUTER_BOUND ( 'NONE', #18379, .T. ) ;
#26427 = CARTESIAN_POINT ( 'NONE',  ( 4.962356264823609031, -20.60668162140307658, 36.69605251817252878 ) ) ;
#26428 = CARTESIAN_POINT ( 'NONE',  ( 0.5980894510889457338, -6.974827154143770080, -47.60453381548690288 ) ) ;
#26429 = B_SPLINE_CURVE_WITH_KNOTS ( 'NONE', 3,
 ( #5541, #47881, #28761, #48477 ),
 .UNSPECIFIED., .F., .F.,
 ( 4, 4 ),
 ( 6.254634441385501517E-18, 0.004566006591234648103 ),
 .UNSPECIFIED. ) ;
#26430 = ORIENTED_EDGE ( 'NONE', *, *, #53256, .T. ) ;
#26431 = CARTESIAN_POINT ( 'NONE',  ( 0.5809828226811553087, -38.32755012159125840, -28.72298383114528519 ) ) ;
#26432 = B_SPLINE_CURVE_WITH_KNOTS ( 'NONE', 3,
 ( #48073, #19887, #15486, #53363 ),
 .UNSPECIFIED., .F., .F.,
 ( 4, 4 ),
 ( 0.000000000000000000, 0.004446090762761378129 ),
 .UNSPECIFIED. ) ;
#26433 = CARTESIAN_POINT ( 'NONE',  ( 4.975801465491694664, -47.76942479135482955, -3.702618843597289544 ) ) ;
#26434 = EDGE_CURVE ( 'NONE', #16055, #61015, #25235, .T. ) ;
#26435 =( BOUNDED_SURFACE ( )  B_SPLINE_SURFACE ( 3, 1, ( 
 ( #5882, #48829 ),
 ( #25329, #2432 ),
 ( #45087, #59446 ),
 ( #11556, #40385 ) ),
 .UNSPECIFIED., .F., .F., .F. ) 
 B_SPLINE_SURFACE_WITH_KNOTS ( ( 4, 4 ),
 ( 2, 2 ),
 ( 0.000000000000000000, 1.000000000000000000 ),
 ( 0.000000000000000000, 1.000000000000000000 ),
 .UNSPECIFIED. ) 
 GEOMETRIC_REPRESENTATION_ITEM ( )  RATIONAL_B_SPLINE_SURFACE ( (
 ( 1.000000000000000000, 1.000000000000000000),
 ( 0.7269869731126821222, 0.9931720237060910339),
 ( 0.7269869731126821222, 0.9931720237060910339),
 ( 1.000000000000000000, 1.000000000000000000) ) ) 
 REPRESENTATION_ITEM ( '' )  SURFACE ( )  );
#26436 = CARTESIAN_POINT ( 'NONE',  ( 0.1157506346131639274, 15.15184229040494124, -41.44107063058978468 ) ) ;
#26437 = EDGE_CURVE ( 'NONE', #1494, #29154, #56331, .T. ) ;
#26438 = EDGE_LOOP ( 'NONE', ( #57304, #44064, #14627, #4252 ) ) ;
#26439 = VERTEX_POINT ( 'NONE', #59043 ) ;
#26440 = ADVANCED_FACE ( 'NONE', ( #55265 ), #34817, .T. ) ;
#26441 = CARTESIAN_POINT ( 'NONE',  ( 4.549368137175248350, 42.82045902618772715, -3.018832571116098151 ) ) ;
#26442 = CARTESIAN_POINT ( 'NONE',  ( 0.5806925824938499181, -44.11884900496058748, -15.89809815106991309 ) ) ;
#26443 = EDGE_LOOP ( 'NONE', ( #11491, #31636, #37048, #18690 ) ) ;
#26444 = FACE_OUTER_BOUND ( 'NONE', #19638, .T. ) ;
#26445 = CARTESIAN_POINT ( 'NONE',  ( 0.2285344041767132794, 37.38477457461466003, 23.42818388822967535 ) ) ;
#26446 = EDGE_CURVE ( 'NONE', #47520, #3369, #30144, .T. ) ;
#26447 = FACE_BOUND ( 'NONE', #43513, .T. ) ;
#26448 = CARTESIAN_POINT ( 'NONE',  ( 2.359973842542475886, -43.83014173065230779, -4.129717968993866783 ) ) ;
#26449 = ORIENTED_EDGE ( 'NONE', *, *, #20809, .T. ) ;
#26450 = CARTESIAN_POINT ( 'NONE',  ( 2.500000000000000000, 1.178949249685212974, -2.042000000000001148 ) ) ;
#26451 = CARTESIAN_POINT ( 'NONE',  ( 0.6031356219577718170, 18.49057407199394021, 44.41207482560214004 ) ) ;
#26452 = DIRECTION ( 'NONE',  ( 0.000000000000000000, 0.000000000000000000, -1.000000000000000000 ) ) ;
#26453 = CARTESIAN_POINT ( 'NONE',  ( 2.282816707992306959, 12.16314365252773300, 45.37130043205660712 ) ) ;
#26454 = B_SPLINE_CURVE_WITH_KNOTS ( 'NONE', 3,
 ( #16793, #16469, #29951, #49059 ),
 .UNSPECIFIED., .F., .F.,
 ( 4, 4 ),
 ( 0.000000000000000000, 0.005013413432710150247 ),
 .UNSPECIFIED. ) ;
#26455 = VECTOR ( 'NONE', #33722, 1000.000000000000114 ) ;
#26456 = ORIENTED_EDGE ( 'NONE', *, *, #54598, .F. ) ;
#26457 = FACE_OUTER_BOUND ( 'NONE', #28579, .T. ) ;
#26458 = CARTESIAN_POINT ( 'NONE',  ( 0.8554163680231738898, -26.01084021241273092, 39.04666009476549959 ) ) ;
#26459 = CARTESIAN_POINT ( 'NONE',  ( 0.8557997880470606944, 29.88293891557523807, -37.44587306708065455 ) ) ;
#26460 = CARTESIAN_POINT ( 'NONE',  ( 1.088313998177382169, 36.76812638579230708, 22.12859469727350614 ) ) ;
#26461 = EDGE_CURVE ( 'NONE', #24074, #39259, #6268, .T. ) ;
#26462 = ORIENTED_EDGE ( 'NONE', *, *, #43822, .T. ) ;
#26463 = CARTESIAN_POINT ( 'NONE',  ( 4.975610109902397937, 39.54077024310134902, 28.79195887257488451 ) ) ;
#26464 = DIRECTION ( 'NONE',  ( 0.09722883295013595717, 0.8299705264940721028, 0.5492681305103249700 ) ) ;
#26465 = EDGE_CURVE ( 'NONE', #13205, #11980, #30941, .T. ) ;
#26466 = DIRECTION ( 'NONE',  ( -1.000000000000000000, -0.000000000000000000, -0.000000000000000000 ) ) ;
#26467 = CIRCLE ( 'NONE', #61457, 48.91267123290010943 ) ;
#26468 = FACE_OUTER_BOUND ( 'NONE', #3099, .T. ) ;
#26469 = LINE ( 'NONE', #2649, #34387 ) ;
#26470 = CARTESIAN_POINT ( 'NONE',  ( 0.5837374860065656090, 46.21667939904230593, -12.57177159055114046 ) ) ;
#26471 = CARTESIAN_POINT ( 'NONE',  ( 0.9740398440564312921, -6.011466167923821935, -42.48528956276143731 ) ) ;
#26472 = CARTESIAN_POINT ( 'NONE',  ( 0.1073791018717483448, -41.77800844988507123, -10.69234304550039383 ) ) ;
#26473 = CARTESIAN_POINT ( 'NONE',  ( 0.6041374136657475802, -6.106202762793164318, -47.71861871402587241 ) ) ;
#26474 = CARTESIAN_POINT ( 'NONE',  ( 2.282816707992324723, 44.93953228679972511, -13.67243227270301809 ) ) ;
#26475 = EDGE_LOOP ( 'NONE', ( #17254, #2767, #4179, #12120 ) ) ;
#26476 = CARTESIAN_POINT ( 'NONE',  ( 5.959547316686252039, 17.77392908783919978, 10.26589671991369457 ) ) ;
#26477 = CARTESIAN_POINT ( 'NONE',  ( 0.7242003506639981270, 32.40045956039464414, -36.89474074175420526 ) ) ;
#26478 = CARTESIAN_POINT ( 'NONE',  ( 4.975801465491694664, 2.564218696446817880, 47.84403947906844223 ) ) ;
#26479 = CARTESIAN_POINT ( 'NONE',  ( 0.1155031312995260795, 44.04397861420763860, -2.658868248527860079 ) ) ;
#26480 = FACE_OUTER_BOUND ( 'NONE', #38258, .T. ) ;
#26481 = B_SPLINE_CURVE_WITH_KNOTS ( 'NONE', 3,
 ( #2329, #39664, #44983, #7021 ),
 .UNSPECIFIED., .F., .F.,
 ( 4, 4 ),
 ( 0.000000000000000000, 0.005014147105413705591 ),
 .UNSPECIFIED. ) ;
#26482 = CARTESIAN_POINT ( 'NONE',  ( 4.291220156522060236, -46.54716543045775978, -7.262946213162822851 ) ) ;
#26483 = APPLICATION_PROTOCOL_DEFINITION ( 'draft international standard', 'automotive_design', 1998, #17150 ) ;
#26484 = CARTESIAN_POINT ( 'NONE',  ( 0.6031356755773454870, -44.44547243635334866, 18.40994522247679654 ) ) ;
#26485 = CIRCLE ( 'NONE', #48484, 42.08604991992415023 ) ;
#26487 = EDGE_CURVE ( 'NONE', #34393, #22293, #14538, .T. ) ;
#26486 = B_SPLINE_CURVE_WITH_KNOTS ( 'NONE', 3,
 ( #33385, #38706, #9242, #34299 ),
 .UNSPECIFIED., .F., .F.,
 ( 4, 4 ),
 ( 5.818439421673296370E-18, 0.004566006591234648970 ),
 .UNSPECIFIED. ) ;
#26488 = CARTESIAN_POINT ( 'NONE',  ( 0.7413678028165011646, 36.43924871080639605, -24.83278569074033015 ) ) ;
#26489 = DIRECTION ( 'NONE',  ( -1.000000000000000000, -0.000000000000000000, -0.000000000000000000 ) ) ;
#26491 = VERTEX_POINT ( 'NONE', #12389 ) ;
#26490 = CARTESIAN_POINT ( 'NONE',  ( 4.694002226626920127, 23.33724324709868370, -39.16194388780874647 ) ) ;
#26492 = ORIENTED_EDGE ( 'NONE', *, *, #54374, .F. ) ;
#26493 = DIRECTION ( 'NONE',  ( 1.000000000000000000, 0.000000000000000000, 0.000000000000000000 ) ) ;
#26494 = CARTESIAN_POINT ( 'NONE',  ( -2.569797478183783568, 14.55946937464481827, 1.464172661884213689 ) ) ;
#26495 = CARTESIAN_POINT ( 'NONE',  ( -2.601141883200665639, 7.298105880293888070, -13.02048685838622433 ) ) ;
#26496 = ORIENTED_EDGE ( 'NONE', *, *, #9460, .F. ) ;
#26497 = DIRECTION ( 'NONE',  ( 0.9990097760809871774, 0.000000000000000000, -0.04449120468829421277 ) ) ;
#26498 = CARTESIAN_POINT ( 'NONE',  ( 0.8554163680231738898, -35.40260165760500399, 30.78735566729891815 ) ) ;
#26499 = DIRECTION ( 'NONE',  ( 0.000000000000000000, -0.4999999999999993339, 0.8660254037844390407 ) ) ;
#26500 = ORIENTED_EDGE ( 'NONE', *, *, #43667, .T. ) ;
#26501 = ORIENTED_EDGE ( 'NONE', *, *, #60867, .T. ) ;
#26502 = CIRCLE ( 'NONE', #16496, 2.649999999999985700 ) ;
#26503 = CARTESIAN_POINT ( 'NONE',  ( 0.6067099128993203028, -43.97493306231474719, 18.98236771638443443 ) ) ;
#26505 = DIRECTION ( 'NONE',  ( 0.000000000000000000, 0.000000000000000000, 1.000000000000000000 ) ) ;
#26504 = AXIS2_PLACEMENT_3D ( 'NONE', #53594, #34221, #48920 ) ;
#26506 = CARTESIAN_POINT ( 'NONE',  ( 0.6021448801613057400, 37.22278796205431206, 32.03131584807110954 ) ) ;
#26507 = ORIENTED_EDGE ( 'NONE', *, *, #16853, .T. ) ;
#26508 = VECTOR ( 'NONE', #58016, 1000.000000000000114 ) ;
#26509 = ORIENTED_EDGE ( 'NONE', *, *, #13734, .F. ) ;
#26510 = CARTESIAN_POINT ( 'NONE',  ( 5.895596859100789899, -18.51832497669328959, 7.848555489391991991 ) ) ;
#26511 = CARTESIAN_POINT ( 'NONE',  ( 4.967162193818130511, 0.000000000000000000, 0.000000000000000000 ) ) ;
#26512 = EDGE_LOOP ( 'NONE', ( #38181, #23208, #54252, #38312, #29437, #6227, #46725, #44812, #36366, #59131, #31123, #25274, #44669, #17144, #11988, #19071, #23102, #13782, #40510, #31141, #56000, #38567, #31487, #60976, #54541, #42204, #15265, #32547, #7692, #37472, #18638, #39067, #60789, #46604, #3268, #36875, #12670, #59812, #18820, #46068, #17378, #35016, #6514, #5381, #21066, #16231, #41565, #39883, #41597, #13192, #6551, #32946, #33561, #61555, #18986, #26192, #61653, #17352, #10806, #15453, #34737, #39683, #26520, #13759, #53990, #3870, #3186, #53410, #30075, #39022, #23776, #54869, #52022, #56464, #49626, #7954, #58048, #19506, #32955, #61721, #5690, #1914, #39398, #60502, #26284, #57086, #42413, #52763, #15879, #43719, #34021, #7699, #45839, #43426, #23578, #26840, #17230, #48804, #46481, #52259, #361, #43652, #26316, #42172, #42662, #24464, #31597, #43346, #47135, #35011, #53634, #25886, #55027, #1925, #42369, #31938, #30880, #51254, #35564, #59862, #51457, #42422, #3598, #47432, #53404, #15004, #51703, #28580, #61037, #14076, #33736, #19379, #24262, #15746, #32757, #61482, #16805, #22901, #35412, #50957, #42630, #45203, #18080, #27808, #871, #32275, #43645, #38629, #52857, #2010 ) ) ;
#26513 = CARTESIAN_POINT ( 'NONE',  ( 0.5809828226811553087, 34.25055090842153760, 33.48000389720628789 ) ) ;
#26514 = FACE_OUTER_BOUND ( 'NONE', #7487, .T. ) ;
#26515 = ADVANCED_FACE ( 'NONE', ( #50887 ), #20961, .F. ) ;
#26516 = VERTEX_POINT ( 'NONE', #42149 ) ;
#26517 =( BOUNDED_SURFACE ( )  B_SPLINE_SURFACE ( 3, 1, ( 
 ( #50206, #39920 ),
 ( #1647, #58979 ),
 ( #7270, #6959 ),
 ( #26092, #55200 ) ),
 .UNSPECIFIED., .F., .F., .F. ) 
 B_SPLINE_SURFACE_WITH_KNOTS ( ( 4, 4 ),
 ( 2, 2 ),
 ( 0.000000000000000000, 1.000000000000000000 ),
 ( 0.000000000000000000, 1.000000000000000000 ),
 .UNSPECIFIED. ) 
 GEOMETRIC_REPRESENTATION_ITEM ( )  RATIONAL_B_SPLINE_SURFACE ( (
 ( 1.000000000000000000, 1.000000000000000000),
 ( 0.9732289882329797637, 0.9999525324661233672),
 ( 0.9732289882329797637, 0.9999525324661233672),
 ( 1.000000000000000000, 1.000000000000000000) ) ) 
 REPRESENTATION_ITEM ( '' )  SURFACE ( )  );
#26518 = CARTESIAN_POINT ( 'NONE',  ( 4.549368137175248350, -18.79584381673559079, 38.59302160394720005 ) ) ;
#26519 = CARTESIAN_POINT ( 'NONE',  ( -15.25000000000000711, -2.688986455804108555, -9.952330921218299798E-16 ) ) ;
#26520 = ORIENTED_EDGE ( 'NONE', *, *, #54245, .T. ) ;
#26521 = CARTESIAN_POINT ( 'NONE',  ( 4.962356264823609031, -32.75738977283769771, -26.42326651140497873 ) ) ;
#26522 = CARTESIAN_POINT ( 'NONE',  ( 0.5835871038041856584, -19.86395462753460350, 42.48126362829555092 ) ) ;
#26523 = ADVANCED_FACE ( 'NONE', ( #31478 ), #5733, .F. ) ;
#26524 = CARTESIAN_POINT ( 'NONE',  ( 4.967162193818130511, 24.30453456948160351, -35.57684288741949530 ) ) ;
#26525 = LINE ( 'NONE', #22142, #41435 ) ;
#26526 = B_SPLINE_CURVE_WITH_KNOTS ( 'NONE', 3,
 ( #21628, #54495, #11622, #17246 ),
 .UNSPECIFIED., .F., .F.,
 ( 4, 4 ),
 ( 4.670885906470169924E-18, 0.004050076154993003351 ),
 .UNSPECIFIED. ) ;
#26527 = ORIENTED_EDGE ( 'NONE', *, *, #53849, .F. ) ;
#26529 = B_SPLINE_CURVE_WITH_KNOTS ( 'NONE', 3,
 ( #23012, #36495, #46828, #37123, #42140, #18312, #32099, #60572, #37423, #46508, #7968, #45904, #28007, #31788, #27699, #12380, #47129, #2950, #8573 ),
 .UNSPECIFIED., .F., .F.,
 ( 4, 3, 3, 3, 3, 3, 4 ),
 ( 1.180170631773780508E-16, 0.0002618519381806264589, 0.0003927759815485976015, 0.0005237000248299444058, 0.0006546240681324972830, 0.0007855481115631333597, 0.0009699050456655111587 ),
 .UNSPECIFIED. ) ;
#26528 = CARTESIAN_POINT ( 'NONE',  ( 0.5998501479064699549, 41.39809967730487017, -24.50586714782561160 ) ) ;
#26530 = CARTESIAN_POINT ( 'NONE',  ( 0.1158816050234198619, 39.75203506927189778, -19.14987595668801745 ) ) ;
#26531 = ORIENTED_EDGE ( 'NONE', *, *, #23271, .T. ) ;
#26532 = CARTESIAN_POINT ( 'NONE',  ( 5.896278296736517710, -7.223603833371068816, -18.77089575041346947 ) ) ;
#26533 = ORIENTED_EDGE ( 'NONE', *, *, #53181, .T. ) ;
#26534 = CARTESIAN_POINT ( 'NONE',  ( 0.5809828226811626362, -18.83114015454730961, 44.03860873105688967 ) ) ;
#26535 = ORIENTED_EDGE ( 'NONE', *, *, #22063, .T. ) ;
#26536 = CARTESIAN_POINT ( 'NONE',  ( 0.6041374136657476912, 0.1745662470638107422, 48.10739871142803992 ) ) ;
#26537 = CARTESIAN_POINT ( 'NONE',  ( 0.8751705887134423323, -17.57879340691512837, -44.76769609654229498 ) ) ;
#26538 =( BOUNDED_SURFACE ( )  B_SPLINE_SURFACE ( 3, 1, ( 
 ( #33793, #49103 ),
 ( #52872, #15602 ),
 ( #10903, #34708 ),
 ( #53769, #29993 ) ),
 .UNSPECIFIED., .F., .F., .F. ) 
 B_SPLINE_SURFACE_WITH_KNOTS ( ( 4, 4 ),
 ( 2, 2 ),
 ( 0.000000000000000000, 1.000000000000000000 ),
 ( 0.000000000000000000, 1.000000000000000000 ),
 .UNSPECIFIED. ) 
 GEOMETRIC_REPRESENTATION_ITEM ( )  RATIONAL_B_SPLINE_SURFACE ( (
 ( 1.000000000000000000, 1.000000000000000000),
 ( 0.9754377213608244057, 0.9999580625633939235),
 ( 0.9754377213608244057, 0.9999580625633939235),
 ( 1.000000000000000000, 1.000000000000000000) ) ) 
 REPRESENTATION_ITEM ( '' )  SURFACE ( )  );
#26539 = CARTESIAN_POINT ( 'NONE',  ( 0.1157991065609915993, -43.77224717097112006, 5.561721239068830869 ) ) ;
#26540 = ORIENTED_EDGE ( 'NONE', *, *, #22713, .T. ) ;
#26541 = CARTESIAN_POINT ( 'NONE',  ( 0.3622758884714600280, -22.26738722580193652, 36.91764744403282350 ) ) ;
#26542 = CARTESIAN_POINT ( 'NONE',  ( 1.088313998177386166, -11.85828975620036552, 41.24258460930634129 ) ) ;
#26543 =( BOUNDED_SURFACE ( )  B_SPLINE_SURFACE ( 3, 1, ( 
 ( #32317, #12605 ),
 ( #31078, #26368 ),
 ( #50481, #21994 ),
 ( #56407, #50183 ) ),
 .UNSPECIFIED., .F., .F., .F. ) 
 B_SPLINE_SURFACE_WITH_KNOTS ( ( 4, 4 ),
 ( 2, 2 ),
 ( 0.000000000000000000, 1.000000000000000000 ),
 ( 0.000000000000000000, 1.000000000000000000 ),
 .UNSPECIFIED. ) 
 GEOMETRIC_REPRESENTATION_ITEM ( )  RATIONAL_B_SPLINE_SURFACE ( (
 ( 1.000000000000000000, 1.000000000000000000),
 ( 0.9953485035131437453, 0.8621029689291515030),
 ( 0.9953485035131437453, 0.8621029689291515030),
 ( 1.000000000000000000, 1.000000000000000000) ) ) 
 REPRESENTATION_ITEM ( '' )  SURFACE ( )  );
#26544 = EDGE_CURVE ( 'NONE', #19096, #37493, #61540, .T. ) ;
#26545 = CARTESIAN_POINT ( 'NONE',  ( 4.962356264823601926, -38.91448554252674796, -16.02805081171206680 ) ) ;
#26546 = ORIENTED_EDGE ( 'NONE', *, *, #35502, .T. ) ;
#26547 = EDGE_LOOP ( 'NONE', ( #32556, #53300, #6539, #19615, #1100, #31378, #47941, #53534, #13385, #28283, #52314, #59104, #22944, #21182, #25425, #44577, #6657, #46194, #51334, #11074, #36363, #15569, #16527, #8979, #50784, #59930, #23962, #29144, #46494, #53885, #43138, #9685, #50014, #37573, #51789, #23129, #9542, #52418, #29509, #3760, #52879, #52690, #46283, #59691, #40989, #51219, #40802, #39435, #15441, #15089, #56539, #4249, #15193, #22253, #19834, #32366, #29064, #59620, #23268, #28717, #58105, #8393, #18170, #401, #18464, #47721, #25631, #43221, #19011, #17591, #6136, #44965, #14744, #14075, #47931, #59039, #24181, #26921, #2530, #17834, #20541, #49223, #8335, #45724, #26242, #17013, #22988, #31612, #34805, #15762, #52545, #52101, #15213, #55469, #41746, #45402, #13267, #26118, #14439, #8538, #49029, #45973, #39164, #10977, #32414, #59964, #25298, #58173, #20135, #16847, #50493, #59089, #19664, #40417, #30920, #20363, #21312, #42355, #17853, #4141, #42762, #58470, #8988, #26865, #33270, #34928, #954, #24977, #51395, #20160, #43111, #17056, #31311, #53141, #18591, #16632, #13025, #39503, #11861, #10927, #55009, #59267, #58380, #9891, #43210, #5666, #55884, #16284 ) ) ;
#26548 = DIRECTION ( 'NONE',  ( 0.000000000000000000, 0.000000000000000000, -1.000000000000000000 ) ) ;
#26549 = CARTESIAN_POINT ( 'NONE',  ( 4.975801465491694664, -40.15204426031552032, 26.14269827151608894 ) ) ;
#26550 = CARTESIAN_POINT ( 'NONE',  ( 0.9789233960466703355, 38.63436055929081903, -16.23954774638314191 ) ) ;
#26551 = CARTESIAN_POINT ( 'NONE',  ( 1.827326673878743701, -36.65065268305642832, -22.58371678864569176 ) ) ;
#26552 = CARTESIAN_POINT ( 'NONE',  ( 5.974727161628369032, -14.50236057684835522, -14.52429704002358690 ) ) ;
#26554 = VECTOR ( 'NONE', #25515, 1000.000000000000000 ) ;
#26553 = CARTESIAN_POINT ( 'NONE',  ( 0.5850706913938534814, 46.21698775168663076, -12.57184842331969143 ) ) ;
#26555 = VERTEX_POINT ( 'NONE', #60900 ) ;
#26556 = CARTESIAN_POINT ( 'NONE',  ( 5.910764540655177868, 20.06833201846866288, -1.327888724881951754 ) ) ;
#26557 = CARTESIAN_POINT ( 'NONE',  ( 4.999999999999986677, 58.44237546506807490, 54.69470952477956871 ) ) ;
#26558 = VERTEX_POINT ( 'NONE', #37132 ) ;
#26559 = CARTESIAN_POINT ( 'NONE',  ( 5.960721111146673579, 19.82454228767738158, 5.318514366755001888 ) ) ;
#26560 = DIRECTION ( 'NONE',  ( 0.1024043820194936449, -0.1167898032637411931, 0.9878630899050852010 ) ) ;
#26561 = CARTESIAN_POINT ( 'NONE',  ( 1.827326673878743701, 40.22837085190311512, -15.32882202537235550 ) ) ;
#26562 = AXIS2_PLACEMENT_3D ( 'NONE', #14705, #29094, #57888 ) ;
#26563 = CARTESIAN_POINT ( 'NONE',  ( 0.6041374136657476912, 38.27243465845302239, 29.14743607025096850 ) ) ;
#26564 = CARTESIAN_POINT ( 'NONE',  ( 5.860006189529246790, 26.81109398084765161, -40.09484204000572305 ) ) ;
#26565 = DIRECTION ( 'NONE',  ( -0.07439287786467650709, 0.5965490341031379762, -0.7991213610169762838 ) ) ;
#26566 = CARTESIAN_POINT ( 'NONE',  ( 0.5997462898726536595, 4.195097405482933972, 48.92803682862026449 ) ) ;
#26567 = CARTESIAN_POINT ( 'NONE',  ( 0.1129192098497455998, -12.08918212651712132, -42.43587472053631160 ) ) ;
#26568 = ADVANCED_FACE ( 'NONE', ( #26781 ), #54961, .F. ) ;
#26569 = CARTESIAN_POINT ( 'NONE',  ( 0.9758171775293925654, -39.64000636436369263, 16.42583507057852898 ) ) ;
#26570 = CARTESIAN_POINT ( 'NONE',  ( -5.719999999999999751, 4.781475508499492452E-15, 0.000000000000000000 ) ) ;
#26571 = CARTESIAN_POINT ( 'NONE',  ( 4.962356264823608143, 18.10963840443066530, -37.99048031708887407 ) ) ;
#26572 = CARTESIAN_POINT ( 'NONE',  ( 5.896782393890504181, 17.95394716461040829, 9.065421561537570838 ) ) ;
#26573 = CARTESIAN_POINT ( 'NONE',  ( 4.226256110419178924, 17.40803085720605381, 40.34585123233550519 ) ) ;
#26574 = CARTESIAN_POINT ( 'NONE',  ( 3.678834586032787346, 29.51645078674245326, -39.08185643725441594 ) ) ;
#26575 = CARTESIAN_POINT ( 'NONE',  ( 3.678748215320119197, -9.636375565730645576, -48.01825778030346470 ) ) ;
#26576 = EDGE_CURVE ( 'NONE', #24938, #27055, #36171, .T. ) ;
#26577 = ORIENTED_EDGE ( 'NONE', *, *, #22055, .T. ) ;
#26578 = B_SPLINE_CURVE_WITH_KNOTS ( 'NONE', 3,
 ( #5575, #20034, #19712, #39148, #24094, #53504 ),
 .UNSPECIFIED., .F., .F.,
 ( 4, 2, 4 ),
 ( 2.032984328646362425E-17, 0.0002293755540694319419, 0.0004587511081388435550 ),
 .UNSPECIFIED. ) ;
#26579 = CARTESIAN_POINT ( 'NONE',  ( 0.1087620492084206553, 11.51076657762335032, -41.55994353650429929 ) ) ;
#26580 = CARTESIAN_POINT ( 'NONE',  ( 4.303969348037258058, -47.36875205922778065, 8.413118729223894476 ) ) ;
#26581 = CARTESIAN_POINT ( 'NONE',  ( 1.227938101723756947, -25.45152231597080927, 34.55893248994497924 ) ) ;
#26582 = VERTEX_POINT ( 'NONE', #47746 ) ;
#26583 = CARTESIAN_POINT ( 'NONE',  ( 5.960721111146673579, 20.52557019979492026, 0.006321279846891981850 ) ) ;
#26584 = DIRECTION ( 'NONE',  ( 0.000000000000000000, 0.7071067811865395791, 0.7071067811865553443 ) ) ;
#26585 = DIRECTION ( 'NONE',  ( 0.000000000000000000, 0.000000000000000000, 1.000000000000000000 ) ) ;
#26586 = ORIENTED_EDGE ( 'NONE', *, *, #34671, .T. ) ;
#26587 = CARTESIAN_POINT ( 'NONE',  ( 4.553261556744875094, -39.47791437445886942, -19.26223877088359515 ) ) ;
#26588 = ADVANCED_FACE ( 'NONE', ( #53042 ), #37435, .T. ) ;
#26589 = VERTEX_POINT ( 'NONE', #29239 ) ;
#26590 = CARTESIAN_POINT ( 'NONE',  ( 4.975801465491695552, 9.906103548667566372, 46.87746200127460128 ) ) ;
#26591 = CARTESIAN_POINT ( 'NONE',  ( 0.5804410086790514622, -46.75463715370013773, -3.677466040800468239 ) ) ;
#26592 = AXIS2_PLACEMENT_3D ( 'NONE', #26131, #25206, #40570 ) ;
#26593 = VERTEX_POINT ( 'NONE', #33967 ) ;
#26594 = CARTESIAN_POINT ( 'NONE',  ( -6.057079549204054558, -16.13440658954581508, 10.51247616420408093 ) ) ;
#26596 = ORIENTED_EDGE ( 'NONE', *, *, #8217, .F. ) ;
#26595 = EDGE_CURVE ( 'NONE', #13208, #19087, #5104, .T. ) ;
#26597 = CARTESIAN_POINT ( 'NONE',  ( 0.5797568599927158672, 42.92520440875660626, 18.88523590367528726 ) ) ;
#26598 = CARTESIAN_POINT ( 'NONE',  ( 0.9762797500689124330, -7.469026406145721886, -41.23758515880873432 ) ) ;
#26599 = AXIS2_PLACEMENT_3D ( 'NONE', #30477, #12644, #40855 ) ;
#26600 = VERTEX_POINT ( 'NONE', #56507 ) ;
#26601 = CARTESIAN_POINT ( 'NONE',  ( 4.975610109902397937, 34.73360008816130318, 34.43873447229810836 ) ) ;
#26602 = EDGE_CURVE ( 'NONE', #3069, #20568, #52558, .T. ) ;
#26603 = ORIENTED_EDGE ( 'NONE', *, *, #49077, .F. ) ;
#26604 = CARTESIAN_POINT ( 'NONE',  ( 0.1155031312995260795, -1.582654180881167383, 44.09576893847694379 ) ) ;
#26605 = ORIENTED_EDGE ( 'NONE', *, *, #39459, .T. ) ;
#26606 = ORIENTED_EDGE ( 'NONE', *, *, #55612, .T. ) ;
#26607 = CARTESIAN_POINT ( 'NONE',  ( -6.017396004339686577, 13.32495836419624702, 13.32329839588559750 ) ) ;
#26609 = VECTOR ( 'NONE', #23479, 1000.000000000000114 ) ;
#26608 = DIRECTION ( 'NONE',  ( -0.07836865515943412797, -0.6993330359244914751, 0.7104869166657016288 ) ) ;
#26610 = CARTESIAN_POINT ( 'NONE',  ( 1.092182651088185352, -37.75446286322829792, -18.20334360361852433 ) ) ;
#26611 = CARTESIAN_POINT ( 'NONE',  ( 4.553261556744875094, 0.000000000000000000, 0.000000000000000000 ) ) ;
#26612 = CARTESIAN_POINT ( 'NONE',  ( 5.959828726073459926, -14.51699876360190267, -14.51059719297111705 ) ) ;
#26613 = VERTEX_POINT ( 'NONE', #13942 ) ;
#26614 = DIRECTION ( 'NONE',  ( 0.000000000000000000, 0.000000000000000000, -1.000000000000000000 ) ) ;
#26615 = CARTESIAN_POINT ( 'NONE',  ( 5.965394784446460541, 2.693446924985626101, -20.34787558161484355 ) ) ;
#26616 = ADVANCED_FACE ( 'NONE', ( #24234 ), #9787, .F. ) ;
#26617 = CARTESIAN_POINT ( 'NONE',  ( 0.5834872094924150598, -44.33648115256914224, 18.11905305011503842 ) ) ;
#26618 = VERTEX_POINT ( 'NONE', #28018 ) ;
#26619 =( BOUNDED_SURFACE ( )  B_SPLINE_SURFACE ( 3, 1, ( 
 ( #31802, #8587 ),
 ( #13317, #16781 ),
 ( #17091, #27713 ),
 ( #35893, #12093 ) ),
 .UNSPECIFIED., .F., .F., .F. ) 
 B_SPLINE_SURFACE_WITH_KNOTS ( ( 4, 4 ),
 ( 2, 2 ),
 ( 0.000000000000000000, 1.000000000000000000 ),
 ( 0.000000000000000000, 1.000000000000000000 ),
 .UNSPECIFIED. ) 
 GEOMETRIC_REPRESENTATION_ITEM ( )  RATIONAL_B_SPLINE_SURFACE ( (
 ( 1.000000000000000000, 1.000000000000000000),
 ( 0.9729067724841187204, 0.9999501103223794596),
 ( 0.9729067724841187204, 0.9999501103223794596),
 ( 1.000000000000000000, 1.000000000000000000) ) ) 
 REPRESENTATION_ITEM ( '' )  SURFACE ( )  );
#26620 = ORIENTED_EDGE ( 'NONE', *, *, #54010, .F. ) ;
#26621 = CARTESIAN_POINT ( 'NONE',  ( -6.017396004339686577, 18.84316306185412415, -0.001173774849047644949 ) ) ;
#26622 = CARTESIAN_POINT ( 'NONE',  ( 0.9783242366443547500, 40.48960050396856047, -10.81326690855047623 ) ) ;
#26623 = ORIENTED_EDGE ( 'NONE', *, *, #54245, .F. ) ;
#26624 = CARTESIAN_POINT ( 'NONE',  ( 0.8753041380234465318, 40.66072100792138855, 27.52896828776844274 ) ) ;
#26625 = CARTESIAN_POINT ( 'NONE',  ( -6.016761891674565099, -16.32039929810263601, 9.418621820384437626 ) ) ;
#26626 =( BOUNDED_SURFACE ( )  B_SPLINE_SURFACE ( 3, 1, ( 
 ( #44434, #26208 ),
 ( #45349, #2394 ),
 ( #29675, #30290 ),
 ( #48789, #1462 ) ),
 .UNSPECIFIED., .F., .F., .F. ) 
 B_SPLINE_SURFACE_WITH_KNOTS ( ( 4, 4 ),
 ( 2, 2 ),
 ( 0.000000000000000000, 1.000000000000000000 ),
 ( 0.000000000000000000, 1.000000000000000000 ),
 .UNSPECIFIED. ) 
 GEOMETRIC_REPRESENTATION_ITEM ( )  RATIONAL_B_SPLINE_SURFACE ( (
 ( 1.000000000000000000, 1.000000000000000000),
 ( 0.7282232189291693025, 0.9929344683865674037),
 ( 0.7282232189291693025, 0.9929344683865674037),
 ( 1.000000000000000000, 1.000000000000000000) ) ) 
 REPRESENTATION_ITEM ( '' )  SURFACE ( )  );
#26627 = B_SPLINE_CURVE_WITH_KNOTS ( 'NONE', 3,
 ( #7980, #60583, #36826, #32110, #40602, #44993 ),
 .UNSPECIFIED., .F., .F.,
 ( 4, 2, 4 ),
 ( 3.476216610979977084E-18, 0.0002291459268755703161, 0.0004582918537511371628 ),
 .UNSPECIFIED. ) ;
#26628 = EDGE_LOOP ( 'NONE', ( #34170, #28999, #61329, #4153 ) ) ;
#26629 = CARTESIAN_POINT ( 'NONE',  ( -5.995132425357893702, 13.33084941932925993, -13.31880955509713260 ) ) ;
#26630 = ORIENTED_EDGE ( 'NONE', *, *, #58243, .F. ) ;
#26631 = CARTESIAN_POINT ( 'NONE',  ( 0.5988103622719985752, 44.21009254328978244, 18.96890139670008679 ) ) ;
#26632 = CARTESIAN_POINT ( 'NONE',  ( 0.9762797500689124330, 19.69530149098661909, 36.99215976885973589 ) ) ;
#26633 = CARTESIAN_POINT ( 'NONE',  ( 5.960721111146673579, 17.77250458025991975, -10.26825948882907191 ) ) ;
#26634 = SURFACE_SIDE_STYLE ('',( #37604 ) ) ;
#26635 = CARTESIAN_POINT ( 'NONE',  ( 0.8557997880470599172, -5.347802024196930404, -47.60865952217005059 ) ) ;
#26636 = ORIENTED_EDGE ( 'NONE', *, *, #45461, .F. ) ;
#26637 = FACE_OUTER_BOUND ( 'NONE', #37819, .T. ) ;
#26638 = LINE ( 'NONE', #25401, #56609 ) ;
#26639 = AXIS2_PLACEMENT_3D ( 'NONE', #32324, #44664, #42056 ) ;
#26640 = CARTESIAN_POINT ( 'NONE',  ( 4.303969348037258058, 36.81598326424592216, -30.97035057417624060 ) ) ;
#26641 = CARTESIAN_POINT ( 'NONE',  ( -6.077587904424778920, -1.855182226445892812, -19.16648951426968850 ) ) ;
#26642 = AXIS2_PLACEMENT_3D ( 'NONE', #56577, #18386, #51877 ) ;
#26643 = CARTESIAN_POINT ( 'NONE',  ( 0.9780303403264780648, 29.36652971755217933, 29.89893887319762200 ) ) ;
#26644 = CARTESIAN_POINT ( 'NONE',  ( 4.975610109902397937, 25.84633036597824329, 41.52609557555928177 ) ) ;
#26645 = EDGE_CURVE ( 'NONE', #26948, #15373, #406, .T. ) ;
#26646 = DIRECTION ( 'NONE',  ( 1.000000000000000000, -0.000000000000000000, -0.000000000000000000 ) ) ;
#26647 = CARTESIAN_POINT ( 'NONE',  ( 0.5804410086790514622, -13.37224000219899800, 44.95223074752782821 ) ) ;
#26648 = B_SPLINE_CURVE_WITH_KNOTS ( 'NONE', 3,
 ( #30460, #1955, #26086, #30776, #21698, #22320 ),
 .UNSPECIFIED., .F., .F.,
 ( 4, 2, 4 ),
 ( 1.553373257785006303E-17, 0.0002293319059085112009, 0.0004586638118170068977 ),
 .UNSPECIFIED. ) ;
#26649 = FACE_OUTER_BOUND ( 'NONE', #32145, .T. ) ;
#26650 = EDGE_CURVE ( 'NONE', #7783, #32624, #53331, .T. ) ;
#26651 = EDGE_CURVE ( 'NONE', #8551, #3462, #50347, .T. ) ;
#26652 = CARTESIAN_POINT ( 'NONE',  ( 0.1129192098497447394, -44.12161472487018443, 0.4846667466135898827 ) ) ;
#26653 = CARTESIAN_POINT ( 'NONE',  ( 0.7954196712028465122, 33.39101545667288207, 34.61997730204591761 ) ) ;
#26654 = CONICAL_SURFACE ( 'NONE', #20673, 43.08621763946400307, 1.568696531533066763 ) ;
#26655 = ORIENTED_EDGE ( 'NONE', *, *, #3643, .F. ) ;
#26656 = CARTESIAN_POINT ( 'NONE',  ( 0.5797568599927147570, -46.07736688617723786, 8.723621352834124210 ) ) ;
#26657 = FACE_OUTER_BOUND ( 'NONE', #60927, .T. ) ;
#26658 = CARTESIAN_POINT ( 'NONE',  ( 2.185380717157383135, -42.20433799401791219, 12.55442780671010539 ) ) ;
#26659 = ORIENTED_EDGE ( 'NONE', *, *, #8711, .T. ) ;
#26660 = CARTESIAN_POINT ( 'NONE',  ( 3.783198216974394068, -14.86152287314652476, -40.39102707215872812 ) ) ;
#26661 = CARTESIAN_POINT ( 'NONE',  ( 5.981074661064941900, 10.25489689131130611, -17.77917279944622209 ) ) ;
#26662 = DIRECTION ( 'NONE',  ( -1.000000000000000000, -0.000000000000000000, -0.000000000000000000 ) ) ;
#26663 = EDGE_LOOP ( 'NONE', ( #4342, #59015, #42985, #36533 ) ) ;
#26664 = CARTESIAN_POINT ( 'NONE',  ( 0.5997462898726536595, -45.31995669577334240, -18.91172004968183984 ) ) ;
#26665 = CARTESIAN_POINT ( 'NONE',  ( 0.9736507210033050752, -41.32746151989292116, -11.54000710819857822 ) ) ;
#26666 = CARTESIAN_POINT ( 'NONE',  ( 3.727782113643637096, -10.44443373141009523, 42.70470208227845177 ) ) ;
#26667 = EDGE_CURVE ( 'NONE', #31387, #28847, #11835, .T. ) ;
#26668 = VERTEX_POINT ( 'NONE', #10142 ) ;
#26669 = CARTESIAN_POINT ( 'NONE',  ( 0.5807400328401574052, -47.55718917606846929, 5.711437504335798998 ) ) ;
#26671 = EDGE_LOOP ( 'NONE', ( #12422, #29075, #27261, #2568 ) ) ;
#26670 = EDGE_CURVE ( 'NONE', #29930, #49867, #50791, .T. ) ;
#26672 = VERTEX_POINT ( 'NONE', #38066 ) ;
#26673 = LINE ( 'NONE', #47035, #1705 ) ;
#26674 = VERTEX_POINT ( 'NONE', #14550 ) ;
#26675 = FACE_OUTER_BOUND ( 'NONE', #57954, .T. ) ;
#26676 = EDGE_LOOP ( 'NONE', ( #35056, #3554, #41350, #25980 ) ) ;
#26677 = CARTESIAN_POINT ( 'NONE',  ( 0.6039202388192952409, -42.70269169458205738, -24.24961514924442341 ) ) ;
#26678 = EDGE_CURVE ( 'NONE', #55702, #31335, #8509, .T. ) ;
#26679 = CARTESIAN_POINT ( 'NONE',  ( 0.9730545539215883499, 36.90443313492362165, -21.89037132892396897 ) ) ;
#26680 = AXIS2_PLACEMENT_3D ( 'NONE', #53342, #28934, #24860 ) ;
#26681 = ORIENTED_EDGE ( 'NONE', *, *, #32904, .F. ) ;
#26682 = CARTESIAN_POINT ( 'NONE',  ( 0.1135584504625008345, 43.39109096822844691, -8.010323134691606839 ) ) ;
#26683 = AXIS2_PLACEMENT_3D ( 'NONE', #21612, #36352, #60727 ) ;
#26684 = CARTESIAN_POINT ( 'NONE',  ( 2.299746137290198611, -43.34124262129089544, -22.93072231153081830 ) ) ;
#26685 = CIRCLE ( 'NONE', #32692, 5.000000000000000000 ) ;
#26686 = CARTESIAN_POINT ( 'NONE',  ( 0.6067375320500721925, 18.98242280073624144, -43.97491060910868299 ) ) ;
#26687 = VERTEX_POINT ( 'NONE', #57725 ) ;
#26688 = CARTESIAN_POINT ( 'NONE',  ( 2.299652685299200972, 3.424355312338875024, 48.91375589292864134 ) ) ;
#26689 = EDGE_CURVE ( 'NONE', #32871, #29523, #36960, .T. ) ;
#26690 = B_SPLINE_CURVE_WITH_KNOTS ( 'NONE', 3,
 ( #11789, #49987, #26174, #45311, #2353, #59681, #16795, #3272, #22099, #3582, #13638, #8286, #13030, #37773, #51508, #41227 ),
 .UNSPECIFIED., .F., .F.,
 ( 4, 3, 3, 3, 3, 4 ),
 ( 1.962735358247463844E-17, 0.0002732102107931921680, 0.0004098135523333891776, 0.0005464168938825009854, 0.0008195847345945413837, 0.001092771384553105265 ),
 .UNSPECIFIED. ) ;
#26691 = ORIENTED_EDGE ( 'NONE', *, *, #31773, .F. ) ;
#26692 = CARTESIAN_POINT ( 'NONE',  ( 0.9736507210033054083, -42.90603603725248405, -0.4504567742785494100 ) ) ;
#26693 = DIRECTION ( 'NONE',  ( 0.000000000000000000, 0.000000000000000000, 1.000000000000000000 ) ) ;
#26694 = CARTESIAN_POINT ( 'NONE',  ( 1.827326673878744367, 17.60663982372537717, -39.28486782721049053 ) ) ;
#26695 = EDGE_LOOP ( 'NONE', ( #47710, #36576, #9979, #41278 ) ) ;
#26696 = FACE_OUTER_BOUND ( 'NONE', #31950, .T. ) ;
#26697 = CARTESIAN_POINT ( 'NONE',  ( 4.963659409799330291, -29.86601237216433447, 33.33129552235077853 ) ) ;
#26698 = CARTESIAN_POINT ( 'NONE',  ( 3.407937589446178528, -7.970324840162034796, 11.14158115674370642 ) ) ;
#26699 = PRESENTATION_STYLE_ASSIGNMENT (( #36129 ) ) ;
#26700 = ORIENTED_EDGE ( 'NONE', *, *, #20997, .F. ) ;
#26701 = VERTEX_POINT ( 'NONE', #15462 ) ;
#26702 = FACE_OUTER_BOUND ( 'NONE', #20355, .T. ) ;
#26703 = CARTESIAN_POINT ( 'NONE',  ( 0.1102847568649952675, 34.26895182984662824, 26.17930421801163021 ) ) ;
#26704 = CARTESIAN_POINT ( 'NONE',  ( 3.407937589446178528, 1.331713209622699567, -13.63405474014706975 ) ) ;
#26705 = CARTESIAN_POINT ( 'NONE',  ( 3.238931869106855377, 38.98364358950744446, -18.12707634097783682 ) ) ;
#26706 = VECTOR ( 'NONE', #511, 1000.000000000000114 ) ;
#26707 = DIRECTION ( 'NONE',  ( 0.000000000000000000, 0.000000000000000000, 1.000000000000000000 ) ) ;
#26708 = DIRECTION ( 'NONE',  ( 0.000000000000000000, 0.000000000000000000, 1.000000000000000000 ) ) ;
#26709 = CARTESIAN_POINT ( 'NONE',  ( 4.553261556744873317, 43.92594400279101308, -0.2258523573157051323 ) ) ;
#26710 = CARTESIAN_POINT ( 'NONE',  ( -6.015611763856276717, 2.465697960551047618, 18.68122482568280773 ) ) ;
#26711 = LINE ( 'NONE', #49908, #16230 ) ;
#26712 = CARTESIAN_POINT ( 'NONE',  ( 0.5800708057587374844, -41.78924035064540021, 23.40241940841941570 ) ) ;
#26713 = ADVANCED_FACE ( 'NONE', ( #58651 ), #27356, .F. ) ;
#26714 = CARTESIAN_POINT ( 'NONE',  ( 0.5980271706414711508, -20.51809962909660356, 44.62125984832933767 ) ) ;
#26715 = B_SPLINE_CURVE_WITH_KNOTS ( 'NONE', 3,
 ( #17696, #18625, #14245, #8272 ),
 .UNSPECIFIED., .F., .F.,
 ( 4, 4 ),
 ( 0.000000000000000000, 0.005014147105413694315 ),
 .UNSPECIFIED. ) ;
#26716 = CARTESIAN_POINT ( 'NONE',  ( 2.533389852662419894, 41.24849501674540164, -15.36268826042980429 ) ) ;
#26717 = CARTESIAN_POINT ( 'NONE',  ( 0.5817216825391134938, -14.32835586215152901, -44.65347881738895808 ) ) ;
#26718 = CARTESIAN_POINT ( 'NONE',  ( 4.549368137175248350, 3.018832571116558672, -42.82045902618769873 ) ) ;
#26720 = EDGE_CURVE ( 'NONE', #40797, #31069, #51909, .T. ) ;
#26719 = CARTESIAN_POINT ( 'NONE',  ( 0.6030672727741701600, -6.192762795894120487, -47.70721108823347123 ) ) ;
#26721 = CARTESIAN_POINT ( 'NONE',  ( 0.9730545539215883499, -16.88610103448528221, -39.44597740938079511 ) ) ;
#26722 = AXIS2_PLACEMENT_3D ( 'NONE', #25468, #44611, #1648 ) ;
#26723 = EDGE_CURVE ( 'NONE', #37975, #46746, #18850, .T. ) ;
#26724 = CARTESIAN_POINT ( 'NONE',  ( 0.6016117650947691020, 17.28651784492412347, 45.96441400737769811 ) ) ;
#26725 = CARTESIAN_POINT ( 'NONE',  ( 0.6030672727741701600, 46.49075153683472905, -12.36682345648132753 ) ) ;
#26726 = EDGE_CURVE ( 'NONE', #47783, #13269, #21964, .T. ) ;
#26728 = ORIENTED_EDGE ( 'NONE', *, *, #58111, .T. ) ;
#26727 = CARTESIAN_POINT ( 'NONE',  ( 0.6041374136657475802, 47.71861871402589372, -6.106202762792999117 ) ) ;
#26729 = ORIENTED_EDGE ( 'NONE', *, *, #48770, .T. ) ;
#26730 = CIRCLE ( 'NONE', #61712, 48.09070567114147110 ) ;
#26731 = FACE_BOUND ( 'NONE', #17754, .T. ) ;
#26732 = CARTESIAN_POINT ( 'NONE',  ( 0.5549461598389365813, 3.360523605541063219, -43.97640931867226755 ) ) ;
#26733 = AXIS2_PLACEMENT_3D ( 'NONE', #12448, #25919, #30921 ) ;
#26734 = EDGE_CURVE ( 'NONE', #30011, #13746, #45176, .T. ) ;
#26735 = CARTESIAN_POINT ( 'NONE',  ( 0.5998501479064708430, 34.38546660123297727, -33.64490850298808056 ) ) ;
#26736 = ORIENTED_EDGE ( 'NONE', *, *, #2312, .T. ) ;
#26737 = ORIENTED_EDGE ( 'NONE', *, *, #52782, .F. ) ;
#26738 = DIRECTION ( 'NONE',  ( 0.000000000000000000, 0.000000000000000000, 1.000000000000000000 ) ) ;
#26739 = CARTESIAN_POINT ( 'NONE',  ( 0.3676999524040366896, 36.51379593394493384, -24.75264207750488055 ) ) ;
#26740 = ORIENTED_EDGE ( 'NONE', *, *, #21734, .F. ) ;
#26741 = APPLICATION_CONTEXT ( 'automotive_design' ) ;
#26742 = VERTEX_POINT ( 'NONE', #20778 ) ;
#26743 = EDGE_CURVE ( 'NONE', #46325, #34231, #33172, .T. ) ;
#26744 =( BOUNDED_SURFACE ( )  B_SPLINE_SURFACE ( 3, 1, ( 
 ( #41336, #51931 ),
 ( #46039, #17204 ),
 ( #23435, #18434 ),
 ( #8097, #4297 ) ),
 .UNSPECIFIED., .F., .F., .F. ) 
 B_SPLINE_SURFACE_WITH_KNOTS ( ( 4, 4 ),
 ( 2, 2 ),
 ( 0.000000000000000000, 1.000000000000000000 ),
 ( 0.000000000000000000, 1.000000000000000000 ),
 .UNSPECIFIED. ) 
 GEOMETRIC_REPRESENTATION_ITEM ( )  RATIONAL_B_SPLINE_SURFACE ( (
 ( 1.000000000000000000, 1.000000000000000000),
 ( 0.9952954269826590483, 0.8620686068821339365),
 ( 0.9952954269826590483, 0.8620686068821339365),
 ( 1.000000000000000000, 1.000000000000000000) ) ) 
 REPRESENTATION_ITEM ( '' )  SURFACE ( )  );
#26745 = CARTESIAN_POINT ( 'NONE',  ( 0.8554163680231720024, 45.48289776771366633, 11.51136324522541088 ) ) ;
#26746 = EDGE_CURVE ( 'NONE', #57526, #61588, #31727, .T. ) ;
#26747 = B_SPLINE_CURVE_WITH_KNOTS ( 'NONE', 3,
 ( #54185, #27470, #30390, #1569, #53883, #55968 ),
 .UNSPECIFIED., .F., .F.,
 ( 4, 2, 4 ),
 ( 2.335442953235084577E-18, 0.0002447193893791696538, 0.0004894387787583370309 ),
 .UNSPECIFIED. ) ;
#26748 = CARTESIAN_POINT ( 'NONE',  ( 5.959547316686252039, -18.96456592444095435, -7.851524054666348285 ) ) ;
#26749 = ORIENTED_EDGE ( 'NONE', *, *, #23858, .F. ) ;
#26750 = CARTESIAN_POINT ( 'NONE',  ( 4.553261556744873317, 43.92594400279101308, -0.2258523573157051323 ) ) ;
#26751 = DIRECTION ( 'NONE',  ( 0.000000000000000000, 0.000000000000000000, 1.000000000000000000 ) ) ;
#26752 = B_SPLINE_CURVE_WITH_KNOTS ( 'NONE', 3,
 ( #34919, #11106, #30189, #29268, #24580, #49296 ),
 .UNSPECIFIED., .F., .F.,
 ( 4, 2, 4 ),
 ( 8.699011523299071029E-17, 0.0002293366620881452287, 0.0004586733241762035044 ),
 .UNSPECIFIED. ) ;
#26753 = CARTESIAN_POINT ( 'NONE',  ( 0.6030672727741701600, -48.10738703097480595, -0.08725775308904697158 ) ) ;
#26754 = VERTEX_POINT ( 'NONE', #40844 ) ;
#26755 = VERTEX_POINT ( 'NONE', #26088 ) ;
#26756 = CARTESIAN_POINT ( 'NONE',  ( 5.960721111146673579, 7.848955554238515653, -18.96557324978279624 ) ) ;
#26757 = VERTEX_POINT ( 'NONE', #21392 ) ;
#26758 = CARTESIAN_POINT ( 'NONE',  ( 5.959828726073459926, 14.51699876360200214, -14.51059719297101758 ) ) ;
#26759 = CARTESIAN_POINT ( 'NONE',  ( 4.956653778116991482, -21.75875759808677046, -42.88673967249153662 ) ) ;
#26760 = CARTESIAN_POINT ( 'NONE',  ( 0.5998501479064708430, 34.38546660123297727, -33.64490850298808056 ) ) ;
#26761 = CARTESIAN_POINT ( 'NONE',  ( 0.8760168074887076939, -29.98565522133320371, -37.61398439004523198 ) ) ;
#26762 = CARTESIAN_POINT ( 'NONE',  ( 5.719999999999996199, 6.882900011658699842E-15, 0.000000000000000000 ) ) ;
#26763 = EDGE_CURVE ( 'NONE', #23477, #24133, #12941, .T. ) ;
#26764 = B_SPLINE_CURVE_WITH_KNOTS ( 'NONE', 3,
 ( #41361, #22545, #41662, #51031, #12235, #18157, #21928, #59819, #36048, #41981, #60729, #31318, #8123, #37275, #56343, #55722, #46669, #51335, #36975, #45746, #56037, #60416, #2796, #13156, #17849 ),
 .UNSPECIFIED., .F., .F.,
 ( 4, 3, 3, 3, 3, 3, 3, 3, 4 ),
 ( 5.057544569639794935E-18, 0.0005656085177311396400, 0.001131215744874499406, 0.001696821861372766133, 0.002262427090022497717, 0.002828031679238745492, 0.003393635864401605296, 0.003977030878808131623, 0.004561030005651158133 ),
 .UNSPECIFIED. ) ;
#26765 = ORIENTED_EDGE ( 'NONE', *, *, #56199, .T. ) ;
#26766 = CARTESIAN_POINT ( 'NONE',  ( 0.5809828226811617480, 44.45562576850627323, -17.82437196699632054 ) ) ;
#26767 = CARTESIAN_POINT ( 'NONE',  ( 0.3622758884714600280, -10.35929834645893699, -41.85013935980099120 ) ) ;
#26768 = B_SPLINE_CURVE_WITH_KNOTS ( 'NONE', 3,
 ( #16263, #31594, #54446, #50385, #7141, #21269, #40717, #2454, #26270, #20965, #30348, #20657, #21896, #26900, #41031, #7450, #11574, #7774, #50683 ),
 .UNSPECIFIED., .F., .F.,
 ( 4, 3, 3, 3, 3, 3, 4 ),
 ( 0.000000000000000000, 0.0002612768053151701911, 0.0003919133833142908170, 0.0005225499612322570672, 0.0006531865391693378016, 0.0008112755173415183395, 0.0009693688056799708384 ),
 .UNSPECIFIED. ) ;
#26769 = EDGE_CURVE ( 'NONE', #57844, #2002, #48914, .T. ) ;
#26770 = CARTESIAN_POINT ( 'NONE',  ( -6.077587904424778920, 3.067159685105589784, -19.01022232536993783 ) ) ;
#26771 = ORIENTED_EDGE ( 'NONE', *, *, #17148, .F. ) ;
#26772 = CARTESIAN_POINT ( 'NONE',  ( 0.1103744047535531458, 42.76053735246612320, -5.590449877750151231 ) ) ;
#26773 = CARTESIAN_POINT ( 'NONE',  ( 5.895596859100789899, 12.98817590332826200, -15.35693556399487392 ) ) ;
#26774 = CARTESIAN_POINT ( 'NONE',  ( 0.5809828226811617480, 33.48000389720616710, 34.25055090842165839 ) ) ;
#26775 = CARTESIAN_POINT ( 'NONE',  ( 5.838029081930957709, 47.12733084333035549, -3.174861530240974172 ) ) ;
#26776 = AXIS2_PLACEMENT_3D ( 'NONE', #34735, #30014, #55656 ) ;
#26777 = EDGE_LOOP ( 'NONE', ( #7875, #44947, #21217, #7800 ) ) ;
#26778 = CARTESIAN_POINT ( 'NONE',  ( 5.965394784446460541, 10.25014670152090268, 17.78272165951804595 ) ) ;
#26779 = TOROIDAL_SURFACE ( 'NONE', #12665, 12.55882000000000076, 0.05882000000000109363 ) ;
#26780 = DIRECTION ( 'NONE',  ( 0.09835009131224552170, 0.8579344853044343910, -0.5042575517176598465 ) ) ;
#26781 = FACE_OUTER_BOUND ( 'NONE', #4368, .T. ) ;
#26782 = PRODUCT_DEFINITION_SHAPE ( 'NONE', 'NONE',  #61983 ) ;
#26783 = CARTESIAN_POINT ( 'NONE',  ( 0.6017666602106490625, -41.48673504406963275, 24.35550044372372369 ) ) ;
#26784 = CARTESIAN_POINT ( 'NONE',  ( 0.6016118706126977189, -42.95818191652615781, 23.79381560848482735 ) ) ;
#26785 = CARTESIAN_POINT ( 'NONE',  ( 5.959547316686252039, 12.49238070347976226, -16.28624005235086614 ) ) ;
#26786 = CARTESIAN_POINT ( 'NONE',  ( -4.908599999999998964, 0.000000000000000000, 0.000000000000000000 ) ) ;
#26787 = CARTESIAN_POINT ( 'NONE',  ( 0.5807400328401637335, 11.87003418057242321, 46.40483864045149431 ) ) ;
#26788 = CARTESIAN_POINT ( 'NONE',  ( 0.6028777368367060907, 41.20378776142268862, -26.71680563657839258 ) ) ;
#26789 = CARTESIAN_POINT ( 'NONE',  ( 0.8554163680231708922, 9.985124899324334891, 45.84215040611327652 ) ) ;
#26790 = ORIENTED_EDGE ( 'NONE', *, *, #12608, .F. ) ;
#26791 = CARTESIAN_POINT ( 'NONE',  ( -16.08632264266780609, -12.46593278125092219, -0.9310146124893876607 ) ) ;
#26792 = DIRECTION ( 'NONE',  ( 1.000000000000000000, 0.000000000000000000, 0.000000000000000000 ) ) ;
#26793 = CARTESIAN_POINT ( 'NONE',  ( 0.9762797500689124330, 41.59901070109202692, -5.084003725031680077 ) ) ;
#26794 = CARTESIAN_POINT ( 'NONE',  ( 0.6016117650947689910, -39.56281703554725482, -29.09182982310174381 ) ) ;
#26795 = CARTESIAN_POINT ( 'NONE',  ( -6.010958268070873523, 0.01451635840189641029, -18.84344976839986785 ) ) ;
#26796 = AXIS2_PLACEMENT_3D ( 'NONE', #39677, #25241, #49656 ) ;
#26797 = CARTESIAN_POINT ( 'NONE',  ( 0.8551540677456715978, -47.61725548905994287, 5.348818140990729830 ) ) ;
#26798 = SHAPE_DEFINITION_REPRESENTATION ( #2230, #19619 ) ;
#26800 = EDGE_CURVE ( 'NONE', #14380, #39397, #35821, .T. ) ;
#26799 = CARTESIAN_POINT ( 'NONE',  ( 0.1310142868023685403, 37.02349354742214160, 22.11113027429300004 ) ) ;
#26801 =( BOUNDED_CURVE ( )  B_SPLINE_CURVE ( 3, ( #8108, #22527, #33168, #27220 ),
 .UNSPECIFIED., .F., .F. ) 
 B_SPLINE_CURVE_WITH_KNOTS ( ( 4, 4 ),
 ( 0.000000000000000000, 3.141592653589793116 ),
 .UNSPECIFIED. ) 
 CURVE ( )  GEOMETRIC_REPRESENTATION_ITEM ( )  RATIONAL_B_SPLINE_CURVE ( ( 1.000000000000000000, 0.3333333333333333703, 0.3333333333333333703, 1.000000000000000000 ) ) 
 REPRESENTATION_ITEM ( '' )  );
#26802 = CARTESIAN_POINT ( 'NONE',  ( 4.060580049360325461, 35.51942230849218163, -25.88123515658008600 ) ) ;
#26803 = ADVANCED_FACE ( 'NONE', ( #22629 ), #28802, .T. ) ;
#26804 = AXIS2_PLACEMENT_3D ( 'NONE', #37291, #60751, #17871 ) ;
#26805 = EDGE_CURVE ( 'NONE', #34863, #21853, #7906, .T. ) ;
#26807 = EDGE_LOOP ( 'NONE', ( #61489, #5158, #40039, #14685 ) ) ;
#26806 = CARTESIAN_POINT ( 'NONE',  ( -2.601141883200665639, 11.07005473184224975, 10.01245802505087390 ) ) ;
#26808 = ORIENTED_EDGE ( 'NONE', *, *, #15484, .T. ) ;
#26809 = FACE_OUTER_BOUND ( 'NONE', #12766, .T. ) ;
#26810 = FACE_OUTER_BOUND ( 'NONE', #55297, .T. ) ;
#26811 = ADVANCED_FACE ( 'NONE', ( #41762 ), #1717, .F. ) ;
#26812 = CARTESIAN_POINT ( 'NONE',  ( 0.5804410086790514622, 23.01644811389264689, -40.86273324284469055 ) ) ;
#26813 = ORIENTED_EDGE ( 'NONE', *, *, #13563, .F. ) ;
#26814 = DIRECTION ( 'NONE',  ( -1.000000000000000000, -0.000000000000000000, -0.000000000000000000 ) ) ;
#26815 = FACE_BOUND ( 'NONE', #1885, .T. ) ;
#26816 = CARTESIAN_POINT ( 'NONE',  ( 0.5998501479064708430, 44.24259072156059602, 18.89267974119682947 ) ) ;
#26817 =( BOUNDED_SURFACE ( )  B_SPLINE_SURFACE ( 3, 1, ( 
 ( #30269, #16188 ),
 ( #25887, #20884 ),
 ( #44711, #20576 ),
 ( #11179, #19979 ) ),
 .UNSPECIFIED., .F., .F., .F. ) 
 B_SPLINE_SURFACE_WITH_KNOTS ( ( 4, 4 ),
 ( 2, 2 ),
 ( 0.000000000000000000, 1.000000000000000000 ),
 ( 0.000000000000000000, 1.000000000000000000 ),
 .UNSPECIFIED. ) 
 GEOMETRIC_REPRESENTATION_ITEM ( )  RATIONAL_B_SPLINE_SURFACE ( (
 ( 1.000000000000000000, 1.000000000000000000),
 ( 0.9953040768229013402, 0.8617119497784988535),
 ( 0.9953040768229013402, 0.8617119497784988535),
 ( 1.000000000000000000, 1.000000000000000000) ) ) 
 REPRESENTATION_ITEM ( '' )  SURFACE ( )  );
#26818 = VERTEX_POINT ( 'NONE', #32039 ) ;
#26819 = VERTEX_POINT ( 'NONE', #59906 ) ;
#26820 = CARTESIAN_POINT ( 'NONE',  ( 4.975610109902397937, 20.32389311291169065, 44.49032227207074186 ) ) ;
#26821 = B_SPLINE_CURVE_WITH_KNOTS ( 'NONE', 3,
 ( #14185, #56445, #46779, #32985 ),
 .UNSPECIFIED., .F., .F.,
 ( 4, 4 ),
 ( 0.000000000000000000, 0.005013413432710144176 ),
 .UNSPECIFIED. ) ;
#26822 = CIRCLE ( 'NONE', #29852, 12.50000000000000000 ) ;
#26823 = CONICAL_SURFACE ( 'NONE', #29807, 42.92674063221959813, 1.485477209440487556 ) ;
#26824 = CARTESIAN_POINT ( 'NONE',  ( 0.8560838555295158248, -13.02223058219810881, -45.06433561859972059 ) ) ;
#26825 = CARTESIAN_POINT ( 'NONE',  ( 4.549368137175248350, 3.018832571115968033, 42.82045902618773425 ) ) ;
#26826 = VERTEX_POINT ( 'NONE', #55197 ) ;
#26827 = CARTESIAN_POINT ( 'NONE',  ( 0.5987334308729321819, 43.97851305131931809, -21.85070471093932909 ) ) ;
#26828 = CARTESIAN_POINT ( 'NONE',  ( 0.1149546198390366814, -42.61083234180030388, -11.45702981414493316 ) ) ;
#26829 = CARTESIAN_POINT ( 'NONE',  ( 0.1064266418746772913, 11.70292610004324985, -41.50637583369811523 ) ) ;
#26830 = ORIENTED_EDGE ( 'NONE', *, *, #35863, .T. ) ;
#26831 = CARTESIAN_POINT ( 'NONE',  ( -6.015611763856276717, 18.68122482568280063, 2.465697960551114232 ) ) ;
#26832 =( LENGTH_UNIT ( ) NAMED_UNIT ( * ) SI_UNIT ( .MILLI., .METRE. ) );
#26833 = AXIS2_PLACEMENT_3D ( 'NONE', #6803, #54736, #12475 ) ;
#26834 = ORIENTED_EDGE ( 'NONE', *, *, #30141, .T. ) ;
#26835 = CARTESIAN_POINT ( 'NONE',  ( 0.6029303876144825880, -47.67862422489729113, -6.409038528275959656 ) ) ;
#26836 = CARTESIAN_POINT ( 'NONE',  ( 0.8753041380234465318, -43.21430456406349663, 23.31656511833038437 ) ) ;
#26837 = CARTESIAN_POINT ( 'NONE',  ( 0.5827359174754822568, 41.65957726278070083, -23.63273677570873232 ) ) ;
#26838 = B_SPLINE_CURVE_WITH_KNOTS ( 'NONE', 3,
 ( #28689, #39047, #39347, #5478 ),
 .UNSPECIFIED., .F., .F.,
 ( 4, 4 ),
 ( 1.430489624538199204E-17, 0.005004948556313822648 ),
 .UNSPECIFIED. ) ;
#26839 = ORIENTED_EDGE ( 'NONE', *, *, #9843, .T. ) ;
#26840 = ORIENTED_EDGE ( 'NONE', *, *, #5571, .T. ) ;
#26841 = DIRECTION ( 'NONE',  ( -1.000000000000000000, -0.000000000000000000, -0.000000000000000000 ) ) ;
#26842 = CARTESIAN_POINT ( 'NONE',  ( 0.6009452777970412107, 44.27681866781104247, -18.81240106508482057 ) ) ;
#26843 = VERTEX_POINT ( 'NONE', #50509 ) ;
#26844 = CARTESIAN_POINT ( 'NONE',  ( 0.6039202388192953519, -30.75412344224312378, -38.28508331123577335 ) ) ;
#26845 = ADVANCED_FACE ( 'NONE', ( #2887 ), #7775, .F. ) ;
#26846 = ORIENTED_EDGE ( 'NONE', *, *, #47930, .F. ) ;
#26847 = CARTESIAN_POINT ( 'NONE',  ( -6.017396004339686577, 7.212050743684176979, 17.40836349643169711 ) ) ;
#26848 = CIRCLE ( 'NONE', #37881, 6.866799999999992465 ) ;
#26849 = EDGE_LOOP ( 'NONE', ( #10308, #13121, #38585, #61150 ) ) ;
#26850 = CARTESIAN_POINT ( 'NONE',  ( 0.8744876279028263033, 10.05549467470504865, 48.05452192277508061 ) ) ;
#26851 = CARTESIAN_POINT ( 'NONE',  ( 0.5988103622719991304, -17.84821742497965857, -44.67429504351052572 ) ) ;
#26852 = CARTESIAN_POINT ( 'NONE',  ( 0.1100247026804066219, -26.38690693952982613, 34.10937070541699256 ) ) ;
#26853 = VERTEX_POINT ( 'NONE', #36436 ) ;
#26854 = CARTESIAN_POINT ( 'NONE',  ( 0.1157991065609915715, 43.29484680596880253, 8.514611299724311522 ) ) ;
#26855 = CARTESIAN_POINT ( 'NONE',  ( 0.9730545539215892381, -11.59290486963536360, 41.31259007387227911 ) ) ;
#26856 = CARTESIAN_POINT ( 'NONE',  ( 2.301529144917016101, 47.43735140118864280, -7.543875168382650820 ) ) ;
#26857 = ORIENTED_EDGE ( 'NONE', *, *, #52758, .T. ) ;
#26858 = B_SPLINE_CURVE_WITH_KNOTS ( 'NONE', 3,
 ( #30871, #54347, #7670, #16472, #50901, #35603 ),
 .UNSPECIFIED., .F., .F.,
 ( 4, 2, 4 ),
 ( 0.000000000000000000, 0.0002450742804987349893, 0.0004901485609974699786 ),
 .UNSPECIFIED. ) ;
#26859 = VERTEX_POINT ( 'NONE', #55819 ) ;
#26860 = CARTESIAN_POINT ( 'NONE',  ( 3.238018933889920792, 1.614035038994167559, 13.29670572963665087 ) ) ;
#26861 = CARTESIAN_POINT ( 'NONE',  ( 4.962356264823608143, 6.570263404306589727, 41.57002810511892221 ) ) ;
#26862 = CARTESIAN_POINT ( 'NONE',  ( 0.6029443449137436017, 32.98273704066490808, 36.38239402911363385 ) ) ;
#26863 = CARTESIAN_POINT ( 'NONE',  ( 0.1103310638050661874, 26.31782144882240715, -34.16271402810842517 ) ) ;
#26864 = CARTESIAN_POINT ( 'NONE',  ( 0.3676999524040323597, 33.04872056100222011, 29.21870381457103605 ) ) ;
#26865 = ORIENTED_EDGE ( 'NONE', *, *, #18626, .T. ) ;
#26866 = CARTESIAN_POINT ( 'NONE',  ( 5.901463166500145796, 20.06867656024513380, -1.328943738803248786 ) ) ;
#26867 = VECTOR ( 'NONE', #38094, 1000.000000000000000 ) ;
#26868 = CARTESIAN_POINT ( 'NONE',  ( 3.660087539127326206, -46.85281175970447975, -10.60624038924642143 ) ) ;
#26869 = VERTEX_POINT ( 'NONE', #55506 ) ;
#26870 = VECTOR ( 'NONE', #54026, 1000.000000000000000 ) ;
#26871 = CARTESIAN_POINT ( 'NONE',  ( -6.078457390727109555, 16.77598442640648457, 9.453087197443768019 ) ) ;
#26872 = CARTESIAN_POINT ( 'NONE',  ( 4.335381028904216727, 43.17230378757408005, -23.14970914153703418 ) ) ;
#26873 = CARTESIAN_POINT ( 'NONE',  ( 0.5797568665920720399, -42.13545912329951904, -20.58709287564965607 ) ) ;
#26874 = CARTESIAN_POINT ( 'NONE',  ( 0.5835226383429291674, 45.27760575932801146, 12.21396296248002500 ) ) ;
#26875 = B_SPLINE_CURVE_WITH_KNOTS ( 'NONE', 3,
 ( #34442, #29718, #56985, #43233 ),
 .UNSPECIFIED., .F., .F.,
 ( 4, 4 ),
 ( 0.000000000000000000, 0.005013413432710139839 ),
 .UNSPECIFIED. ) ;
#26876 = CARTESIAN_POINT ( 'NONE',  ( 0.6067099128993229673, -47.38952184036239856, 6.954009037735986887 ) ) ;
#26877 = PLANE ( 'NONE',  #5061 ) ;
#26878 = CARTESIAN_POINT ( 'NONE',  ( 0.8560838555295223751, 5.603718208093996012, 46.57221463840868125 ) ) ;
#26880 = EDGE_CURVE ( 'NONE', #30283, #41860, #44400, .T. ) ;
#26879 = CARTESIAN_POINT ( 'NONE',  ( 0.1152339509894530906, -12.76855756083752347, -42.23631882954315842 ) ) ;
#26881 = CARTESIAN_POINT ( 'NONE',  ( -6.078726893082806448, -11.01388439747492498, -15.79520154185373038 ) ) ;
#26882 = CARTESIAN_POINT ( 'NONE',  ( 4.975610109902397937, 0.000000000000000000, 0.000000000000000000 ) ) ;
#26883 = EDGE_CURVE ( 'NONE', #16119, #3024, #2523, .T. ) ;
#26884 = CARTESIAN_POINT ( 'NONE',  ( 2.526464513654345989, -9.948146339971524199, 41.81190200959800052 ) ) ;
#26885 = CARTESIAN_POINT ( 'NONE',  ( 0.8551540677456834771, -19.17641535420820631, -43.91216198251559888 ) ) ;
#26886 = CONICAL_SURFACE ( 'NONE', #21885, 42.08604991992415023, 1.569615340895231137 ) ;
#26887 = DIRECTION ( 'NONE',  ( 0.000000000000000000, 0.000000000000000000, -1.000000000000000000 ) ) ;
#26888 = CARTESIAN_POINT ( 'NONE',  ( -5.995132425357893702, -14.94489030678159480, 11.47834865841090490 ) ) ;
#26889 = EDGE_CURVE ( 'NONE', #48800, #49846, #9303, .T. ) ;
#26890 = CARTESIAN_POINT ( 'NONE',  ( 0.5819845079324652559, -24.34013310064366564, -41.25022834067375754 ) ) ;
#26891 = CARTESIAN_POINT ( 'NONE',  ( 4.967162193818130511, 28.74031574030012237, 32.10009971360082659 ) ) ;
#26892 = CARTESIAN_POINT ( 'NONE',  ( 4.956653778116991482, -2.599733001514001440, -48.02038484091103498 ) ) ;
#26893 = B_SPLINE_CURVE_WITH_KNOTS ( 'NONE', 3,
 ( #26205, #59403, #15289, #5840, #44432, #20596 ),
 .UNSPECIFIED., .F., .F.,
 ( 4, 2, 4 ),
 ( 3.476216610979977084E-18, 0.0002291966416970833069, 0.0004583932833941631443 ),
 .UNSPECIFIED. ) ;
#26894 = AXIS2_PLACEMENT_3D ( 'NONE', #15561, #1735, #30254 ) ;
#26895 = ORIENTED_EDGE ( 'NONE', *, *, #38350, .F. ) ;
#26896 = CARTESIAN_POINT ( 'NONE',  ( 0.9972139404380286898, 37.48536715150224552, 20.88226186415244001 ) ) ;
#26897 =( BOUNDED_SURFACE ( )  B_SPLINE_SURFACE ( 3, 1, ( 
 ( #24250, #53968 ),
 ( #15482, #28955 ),
 ( #34283, #427 ),
 ( #9853, #43700 ) ),
 .UNSPECIFIED., .F., .F., .F. ) 
 B_SPLINE_SURFACE_WITH_KNOTS ( ( 4, 4 ),
 ( 2, 2 ),
 ( 0.000000000000000000, 1.000000000000000000 ),
 ( 0.000000000000000000, 1.000000000000000000 ),
 .UNSPECIFIED. ) 
 GEOMETRIC_REPRESENTATION_ITEM ( )  RATIONAL_B_SPLINE_SURFACE ( (
 ( 1.000000000000000000, 1.000000000000000000),
 ( 0.7223157951917476005, 0.9931996967497186413),
 ( 0.7223157951917476005, 0.9931996967497186413),
 ( 1.000000000000000000, 1.000000000000000000) ) ) 
 REPRESENTATION_ITEM ( '' )  SURFACE ( )  );
#26898 = ADVANCED_FACE ( 'NONE', ( #61427 ), #46585, .F. ) ;
#26899 = CARTESIAN_POINT ( 'NONE',  ( -5.995132425357893702, 18.68405145320024019, 2.451215106828409596 ) ) ;
#26900 = CARTESIAN_POINT ( 'NONE',  ( 0.1152809850208375841, -38.33721451012828396, -21.84498262975196425 ) ) ;
#26901 = CARTESIAN_POINT ( 'NONE',  ( 0.8744876279028306332, -20.68330519280286239, -44.52584571550401193 ) ) ;
#26902 = ORIENTED_EDGE ( 'NONE', *, *, #29681, .T. ) ;
#26903 = EDGE_CURVE ( 'NONE', #29313, #11906, #19480, .T. ) ;
#26904 = CARTESIAN_POINT ( 'NONE',  ( 0.7242486021783826056, -7.027028552307343467, -48.59662881413720470 ) ) ;
#26905 = B_SPLINE_CURVE_WITH_KNOTS ( 'NONE', 3,
 ( #3980, #14347, #32525, #42861, #43169, #48162 ),
 .UNSPECIFIED., .F., .F.,
 ( 4, 2, 4 ),
 ( 1.267283937151336631E-16, 0.0002450741128632354321, 0.0004901482257263441210 ),
 .UNSPECIFIED. ) ;
#26906 = CARTESIAN_POINT ( 'NONE',  ( 2.526552050251864134, 42.75269566045972169, -4.405466163646869049 ) ) ;
#26907 = EDGE_LOOP ( 'NONE', ( #23146, #24516, #845, #6294 ) ) ;
#26908 = CARTESIAN_POINT ( 'NONE',  ( 1.827119703190778877, 6.838980420687405193, 42.50321986945171204 ) ) ;
#26909 = VERTEX_POINT ( 'NONE', #51736 ) ;
#26910 = AXIS2_PLACEMENT_3D ( 'NONE', #9085, #28189, #47310 ) ;
#26911 =( BOUNDED_SURFACE ( )  B_SPLINE_SURFACE ( 3, 1, ( 
 ( #8924, #28035 ),
 ( #3581, #33366 ),
 ( #61217, #4195 ),
 ( #13956, #18340 ) ),
 .UNSPECIFIED., .F., .F., .F. ) 
 B_SPLINE_SURFACE_WITH_KNOTS ( ( 4, 4 ),
 ( 2, 2 ),
 ( 0.000000000000000000, 1.000000000000000000 ),
 ( 0.000000000000000000, 1.000000000000000000 ),
 .UNSPECIFIED. ) 
 GEOMETRIC_REPRESENTATION_ITEM ( )  RATIONAL_B_SPLINE_SURFACE ( (
 ( 1.000000000000000000, 1.000000000000000000),
 ( 0.9953040768229013402, 0.8617119497784988535),
 ( 0.9953040768229013402, 0.8617119497784988535),
 ( 1.000000000000000000, 1.000000000000000000) ) ) 
 REPRESENTATION_ITEM ( '' )  SURFACE ( )  );
#26912 = CARTESIAN_POINT ( 'NONE',  ( 0.5819845079324651449, -0.4540594263149760890, -47.89381220525412175 ) ) ;
#26914 = CARTESIAN_POINT ( 'NONE',  ( 4.962356264823608143, 0.000000000000000000, 0.000000000000000000 ) ) ;
#26913 = VECTOR ( 'NONE', #35628, 1000.000000000000000 ) ;
#26915 = ORIENTED_EDGE ( 'NONE', *, *, #9907, .F. ) ;
#26916 = FACE_OUTER_BOUND ( 'NONE', #31672, .T. ) ;
#26917 = ORIENTED_EDGE ( 'NONE', *, *, #29485, .T. ) ;
#26918 = CARTESIAN_POINT ( 'NONE',  ( -2.739355103387247858, -10.53896796905780597, -10.57249833758277724 ) ) ;
#26919 = LINE ( 'NONE', #3089, #51320 ) ;
#26920 =( BOUNDED_SURFACE ( )  B_SPLINE_SURFACE ( 3, 1, ( 
 ( #49551, #35796 ),
 ( #59567, #44580 ),
 ( #10741, #40501 ),
 ( #25756, #39261 ) ),
 .UNSPECIFIED., .F., .F., .F. ) 
 B_SPLINE_SURFACE_WITH_KNOTS ( ( 4, 4 ),
 ( 2, 2 ),
 ( 0.000000000000000000, 1.000000000000000000 ),
 ( 0.000000000000000000, 1.000000000000000000 ),
 .UNSPECIFIED. ) 
 GEOMETRIC_REPRESENTATION_ITEM ( )  RATIONAL_B_SPLINE_SURFACE ( (
 ( 1.000000000000000000, 1.000000000000000000),
 ( 0.9953040768229005630, 0.8617119497784937465),
 ( 0.9953040768229005630, 0.8617119497784937465),
 ( 1.000000000000000000, 1.000000000000000000) ) ) 
 REPRESENTATION_ITEM ( '' )  SURFACE ( )  );
#26921 = ORIENTED_EDGE ( 'NONE', *, *, #55415, .T. ) ;
#26922 = LINE ( 'NONE', #31617, #48732 ) ;
#26923 = VERTEX_POINT ( 'NONE', #9440 ) ;
#26924 = CARTESIAN_POINT ( 'NONE',  ( 0.1149546198390367924, -1.687975947156362233, 44.09191878592994129 ) ) ;
#26925 = ADVANCED_FACE ( 'NONE', ( #9138 ), #12562, .F. ) ;
#26926 = AXIS2_PLACEMENT_3D ( 'NONE', #24007, #24311, #57182 ) ;
#26927 = VERTEX_POINT ( 'NONE', #57648 ) ;
#26928 = ORIENTED_EDGE ( 'NONE', *, *, #687, .F. ) ;
#26929 = CARTESIAN_POINT ( 'NONE',  ( 0.6041374136657476912, 24.20487816031464234, 41.57494627055152847 ) ) ;
#26930 = CARTESIAN_POINT ( 'NONE',  ( 0.5800708057587404820, 44.00606528161386422, 18.90714313908675237 ) ) ;
#26931 = FACE_BOUND ( 'NONE', #56337, .T. ) ;
#26932 = CARTESIAN_POINT ( 'NONE',  ( 0.5807400328401574052, 46.12278621143497048, 12.92266817606031104 ) ) ;
#26933 = CARTESIAN_POINT ( 'NONE',  ( 5.000000000000012434, -80.00000000000001421, -1.569632904675596344E-31 ) ) ;
#26934 = ORIENTED_EDGE ( 'NONE', *, *, #37497, .F. ) ;
#26935 = CARTESIAN_POINT ( 'NONE',  ( 0.9790850452238860635, -17.59487447451424913, 38.03626851426523814 ) ) ;
#26936 = FACE_OUTER_BOUND ( 'NONE', #31295, .T. ) ;
#26937 = VERTEX_POINT ( 'NONE', #3808 ) ;
#26938 = EDGE_LOOP ( 'NONE', ( #57168, #45227, #53920, #10380 ) ) ;
#26939 = CARTESIAN_POINT ( 'NONE',  ( 0.1098349054025746091, 37.23978094195821598, 21.74670956129773458 ) ) ;
#26940 = CARTESIAN_POINT ( 'NONE',  ( 0.6001305935487422083, -48.10757715638248300, 0.5236757026887773891 ) ) ;
#26941 = DIRECTION ( 'NONE',  ( 0.000000000000000000, -1.000000000000000000, 0.000000000000000000 ) ) ;
#26942 = CARTESIAN_POINT ( 'NONE',  ( 0.5817217712918332229, -44.44846655092862164, 14.95221640023155807 ) ) ;
#26943 = ORIENTED_EDGE ( 'NONE', *, *, #17816, .T. ) ;
#26944 = LINE ( 'NONE', #55122, #34576 ) ;
#26945 = CARTESIAN_POINT ( 'NONE',  ( 0.5809828226811617480, -17.82437196699647686, -44.45562576850621639 ) ) ;
#26946 = ORIENTED_EDGE ( 'NONE', *, *, #17583, .T. ) ;
#26947 = DIRECTION ( 'NONE',  ( -0.07500201931887527651, -0.4074616462826595731, 0.9101371896075425294 ) ) ;
#26948 = VERTEX_POINT ( 'NONE', #47985 ) ;
#26949 = CARTESIAN_POINT ( 'NONE',  ( -79.49999999999975842, 4.999999999999994671, 1.229372086083732569E-29 ) ) ;
#26950 = CARTESIAN_POINT ( 'NONE',  ( 0.9741495583595161101, -34.28086552274312737, 25.80610403442896228 ) ) ;
#26951 = CARTESIAN_POINT ( 'NONE',  ( 5.965394784446460541, 14.50338846149112904, 14.52385693119007648 ) ) ;
#26952 = CARTESIAN_POINT ( 'NONE',  ( 0.8744876279028263033, 36.80052600666216023, 32.49725120702480297 ) ) ;
#26953 = CIRCLE ( 'NONE', #58948, 15.50000000000000000 ) ;
#26954 = ORIENTED_EDGE ( 'NONE', *, *, #30224, .F. ) ;
#26955 = CARTESIAN_POINT ( 'NONE',  ( 0.9757892942422816684, 21.40977514834436235, -37.18547544211192246 ) ) ;
#26956 = CARTESIAN_POINT ( 'NONE',  ( 0.5786265663353196143, 38.43785771743242208, -28.58414684753446977 ) ) ;
#26957 = ADVANCED_FACE ( 'NONE', ( #4405 ), #27633, .F. ) ;
#26958 = CARTESIAN_POINT ( 'NONE',  ( 40.00000000000000000, 1.530808498934191521E-15, -12.50000000000000000 ) ) ;
#26959 = CARTESIAN_POINT ( 'NONE',  ( 0.3676999524040323597, 9.009680404095913531, 43.18305503711946614 ) ) ;
#26960 = VECTOR ( 'NONE', #47874, 1000.000000000000000 ) ;
#26961 = CARTESIAN_POINT ( 'NONE',  ( 0.9756008150404604784, 37.08855330282530360, -21.57722292874418812 ) ) ;
#26962 = ADVANCED_FACE ( 'NONE', ( #5035 ), #59353, .F. ) ;
#26963 = CARTESIAN_POINT ( 'NONE',  ( 5.896278296736517710, -18.51475911848188716, -7.856887067979012151 ) ) ;
#26964 = DIRECTION ( 'NONE',  ( 0.000000000000000000, 0.000000000000000000, -1.000000000000000000 ) ) ;
#26965 = CARTESIAN_POINT ( 'NONE',  ( 4.960156602257181468, 45.62767441207046204, 8.553784487773027578 ) ) ;
#26966 = CARTESIAN_POINT ( 'NONE',  ( 4.956653778116988818, -43.37017594958040689, -20.77844580450608447 ) ) ;
#26967 = ADVANCED_FACE ( 'NONE', ( #37359 ), #22976, .F. ) ;
#26968 = CARTESIAN_POINT ( 'NONE',  ( 0.7044674535452954967, 10.10543771684589309, 48.05915991111220364 ) ) ;
#26969 = DIRECTION ( 'NONE',  ( 1.000000000000000000, 0.000000000000000000, 0.000000000000000000 ) ) ;
#26970 = ORIENTED_EDGE ( 'NONE', *, *, #56869, .F. ) ;
#26971 = VECTOR ( 'NONE', #44533, 1000.000000000000000 ) ;
#26972 = CARTESIAN_POINT ( 'NONE',  ( 6.999999999999991118, 80.00000000000001421, 2.649999999999999467 ) ) ;
#26973 = CARTESIAN_POINT ( 'NONE',  ( 0.8560838555295158248, -18.91252766612255698, -42.92655508376930129 ) ) ;
#26974 = CARTESIAN_POINT ( 'NONE',  ( 3.678748215320120085, 15.16704763906588660, -46.56794477120276099 ) ) ;
#26975 = ORIENTED_EDGE ( 'NONE', *, *, #20231, .T. ) ;
#26976 = EDGE_CURVE ( 'NONE', #28210, #30576, #19178, .T. ) ;
#26977 = CARTESIAN_POINT ( 'NONE',  ( 3.680974057930773036, 8.091325130366421092, -47.28851186370999216 ) ) ;
#26978 = CARTESIAN_POINT ( 'NONE',  ( 4.956653778116987041, -48.02038484091099235, -2.599733001514835884 ) ) ;
#26979 = B_SPLINE_CURVE_WITH_KNOTS ( 'NONE', 3,
 ( #47642, #56706, #38264, #33555 ),
 .UNSPECIFIED., .F., .F.,
 ( 4, 4 ),
 ( 3.127317220692750759E-18, 0.004042984057420972825 ),
 .UNSPECIFIED. ) ;
#26980 =( NAMED_UNIT ( * ) SI_UNIT ( $, .STERADIAN. ) SOLID_ANGLE_UNIT ( ) );
#26981 = VERTEX_POINT ( 'NONE', #26557 ) ;
#26982 = CARTESIAN_POINT ( 'NONE',  ( 4.549368137175248350, 32.13400537129885493, 28.46244473166684941 ) ) ;
#26983 = CARTESIAN_POINT ( 'NONE',  ( 4.956653778117001252, 47.05699031914963371, -9.917440902360649346 ) ) ;
#26984 = ORIENTED_EDGE ( 'NONE', *, *, #40002, .T. ) ;
#26985 = LINE ( 'NONE', #41416, #2836 ) ;
#26986 = B_SPLINE_CURVE_WITH_KNOTS ( 'NONE', 3,
 ( #40703, #50671, #8079, #46315, #36927, #11562 ),
 .UNSPECIFIED., .F., .F.,
 ( 4, 2, 4 ),
 ( 7.589415207398530075E-19, 0.0002293801035737103749, 0.0004587602071474199909 ),
 .UNSPECIFIED. ) ;
#26987 = EDGE_LOOP ( 'NONE', ( #20499, #45037, #24070, #2162 ) ) ;
#26988 = ORIENTED_EDGE ( 'NONE', *, *, #40211, .F. ) ;
#26989 = CARTESIAN_POINT ( 'NONE',  ( 0.9754402186311932343, -5.414674803234063027, 42.56545569314710775 ) ) ;
#26990 = ORIENTED_EDGE ( 'NONE', *, *, #17240, .T. ) ;
#26991 = CARTESIAN_POINT ( 'NONE',  ( 0.8753041380234524160, 21.91949880997755074, -43.93943445007425908 ) ) ;
#26992 = ORIENTED_EDGE ( 'NONE', *, *, #6578, .T. ) ;
#26993 =( BOUNDED_SURFACE ( )  B_SPLINE_SURFACE ( 3, 1, ( 
 ( #60987, #12795 ),
 ( #16872, #60669 ),
 ( #8360, #55051 ),
 ( #21556, #31889 ) ),
 .UNSPECIFIED., .F., .F., .F. ) 
 B_SPLINE_SURFACE_WITH_KNOTS ( ( 4, 4 ),
 ( 2, 2 ),
 ( 0.000000000000000000, 1.000000000000000000 ),
 ( 0.000000000000000000, 1.000000000000000000 ),
 .UNSPECIFIED. ) 
 GEOMETRIC_REPRESENTATION_ITEM ( )  RATIONAL_B_SPLINE_SURFACE ( (
 ( 1.000000000000000000, 1.000000000000000000),
 ( 0.9953390228620291325, 0.8624445117761032620),
 ( 0.9953390228620291325, 0.8624445117761032620),
 ( 1.000000000000000000, 1.000000000000000000) ) ) 
 REPRESENTATION_ITEM ( '' )  SURFACE ( )  );
#26994 = B_SPLINE_CURVE_WITH_KNOTS ( 'NONE', 3,
 ( #47934, #916, #57595, #20051 ),
 .UNSPECIFIED., .F., .F.,
 ( 4, 4 ),
 ( 2.194270917860438266E-17, 0.004559932413162188537 ),
 .UNSPECIFIED. ) ;
#26995 = CARTESIAN_POINT ( 'NONE',  ( 4.691466044806102076, 44.51344083442439370, -2.583163953528010204 ) ) ;
#26996 = ORIENTED_EDGE ( 'NONE', *, *, #58391, .T. ) ;
#26997 = CARTESIAN_POINT ( 'NONE',  ( 4.000000000000002665, 1.935983797701078313, -5.350530693383766412 ) ) ;
#26998 = AXIS2_PLACEMENT_3D ( 'NONE', #57607, #44197, #1229 ) ;
#26999 = CARTESIAN_POINT ( 'NONE',  ( 4.549368137175248350, 42.82045902618772715, -3.018832571116098151 ) ) ;
#27000 = LINE ( 'NONE', #41740, #27629 ) ;
#27001 = ORIENTED_EDGE ( 'NONE', *, *, #34900, .T. ) ;
#27002 = EDGE_CURVE ( 'NONE', #38495, #6221, #25724, .T. ) ;
#27003 = CARTESIAN_POINT ( 'NONE',  ( 3.407937589446174087, 5.663729899985241012, -12.47329436636623257 ) ) ;
#27004 = EDGE_LOOP ( 'NONE', ( #58816, #61326, #52240, #41868 ) ) ;
#27005 = CARTESIAN_POINT ( 'NONE',  ( 4.303969348037258058, -30.97035057417636850, -36.81598326424581558 ) ) ;
#27006 = B_SPLINE_CURVE_WITH_KNOTS ( 'NONE', 3,
 ( #57223, #19670, #14360, #535 ),
 .UNSPECIFIED., .F., .F.,
 ( 4, 4 ),
 ( 8.673617379884035472E-19, 0.004041751736740995145 ),
 .UNSPECIFIED. ) ;
#27007 = ADVANCED_FACE ( 'NONE', ( #30324, #40379 ), #59758, .F. ) ;
#27008 = B_SPLINE_CURVE_WITH_KNOTS ( 'NONE', 3,
 ( #13828, #32931, #12904, #4070 ),
 .UNSPECIFIED., .F., .F.,
 ( 4, 4 ),
 ( 1.192622389734054877E-18, 0.004446298630425097979 ),
 .UNSPECIFIED. ) ;
#27009 = EDGE_LOOP ( 'NONE', ( #41208, #43440, #36645, #37716 ) ) ;
#27010 = CARTESIAN_POINT ( 'NONE',  ( 3.782542959838394392, -25.80139896681886924, -33.18924019545502091 ) ) ;
#27011 = B_SPLINE_CURVE_WITH_KNOTS ( 'NONE', 3,
 ( #4902, #5815, #24964, #43471 ),
 .UNSPECIFIED., .F., .F.,
 ( 4, 4 ),
 ( 6.397344083151129036E-17, 0.005004741218457477853 ),
 .UNSPECIFIED. ) ;
#27012 = CARTESIAN_POINT ( 'NONE',  ( 1.112077966505211624, 14.23398767724693315, -41.71838827103148617 ) ) ;
#27013 = ORIENTED_EDGE ( 'NONE', *, *, #43706, .T. ) ;
#27014 = CARTESIAN_POINT ( 'NONE',  ( 5.960221823109900008, 2.673723662181335392, -20.35070456576731956 ) ) ;
#27015 = CARTESIAN_POINT ( 'NONE',  ( 4.960156602257177028, 8.553784487773508971, -45.62767441207027730 ) ) ;
#27016 = ADVANCED_FACE ( 'NONE', ( #59440 ), #806, .T. ) ;
#27017 = CARTESIAN_POINT ( 'NONE',  ( -6.078726893082806448, -18.90026279491055305, -3.684305572565921949 ) ) ;
#27018 = CARTESIAN_POINT ( 'NONE',  ( 5.880360259849739535, 26.69116321728517249, 39.86101557989678668 ) ) ;
#27019 = CIRCLE ( 'NONE', #16024, 2.649999999999999467 ) ;
#27020 = VERTEX_POINT ( 'NONE', #17172 ) ;
#27021 = VERTEX_POINT ( 'NONE', #2110 ) ;
#27022 = CARTESIAN_POINT ( 'NONE',  ( 0.9790724872846777727, -39.57652792371481354, -13.78526922061647575 ) ) ;
#27023 = CARTESIAN_POINT ( 'NONE',  ( -6.078457390727109555, -18.27642172158506995, 6.063573211587478085 ) ) ;
#27024 = CARTESIAN_POINT ( 'NONE',  ( 0.6067375320500707492, 6.954068056451403912, -47.38951440911009882 ) ) ;
#27025 = CARTESIAN_POINT ( 'NONE',  ( 4.553261556744873317, 17.98701270972406618, 40.07501640179154379 ) ) ;
#27026 = EDGE_CURVE ( 'NONE', #22462, #58253, #11532, .T. ) ;
#27027 = DIRECTION ( 'NONE',  ( 0.000000000000000000, 0.000000000000000000, 1.000000000000000000 ) ) ;
#27028 = DIRECTION ( 'NONE',  ( 0.000000000000000000, 0.000000000000000000, 1.000000000000000000 ) ) ;
#27029 = EDGE_CURVE ( 'NONE', #31834, #33849, #59325, .T. ) ;
#27030 = CARTESIAN_POINT ( 'NONE',  ( 0.9790850452238869517, 32.92126328992468132, 25.93314006553496398 ) ) ;
#27031 = CARTESIAN_POINT ( 'NONE',  ( 0.9730545539215883499, 33.73144377768594637, -26.52009130076736554 ) ) ;
#27032 = CARTESIAN_POINT ( 'NONE',  ( 0.6253024248130499840, 16.31346559490675929, 46.31754600258349797 ) ) ;
#27033 = CARTESIAN_POINT ( 'NONE',  ( 0.5835226383429282793, -14.06802566813686717, -44.73626189509590745 ) ) ;
#27034 = DIRECTION ( 'NONE',  ( 0.000000000000000000, 1.224646799147331020E-16, 1.000000000000000000 ) ) ;
#27035 = CARTESIAN_POINT ( 'NONE',  ( 0.6031356219577718170, -6.365832241666245395, -47.68448279784252719 ) ) ;
#27036 = EDGE_CURVE ( 'NONE', #24857, #19642, #19744, .T. ) ;
#27037 = CARTESIAN_POINT ( 'NONE',  ( 0.7048096507298579061, -41.23648859290909030, -24.78213711671583752 ) ) ;
#27038 = CARTESIAN_POINT ( 'NONE',  ( 0.5998501479064699549, -46.60114184914309021, -11.94461217097453343 ) ) ;
#27039 = CARTESIAN_POINT ( 'NONE',  ( 0.6026777506516366456, -47.45694871474268695, 12.62475383219417679 ) ) ;
#27041 = ORIENTED_EDGE ( 'NONE', *, *, #15178, .T. ) ;
#27040 = DIRECTION ( 'NONE',  ( 0.9848077530122080203, 0.1736481776669315247, -2.220446049250313081E-16 ) ) ;
#27042 = VERTEX_POINT ( 'NONE', #30952 ) ;
#27043 = B_SPLINE_CURVE_WITH_KNOTS ( 'NONE', 3,
 ( #37152, #37780, #47459, #42169 ),
 .UNSPECIFIED., .F., .F.,
 ( 4, 4 ),
 ( 0.000000000000000000, 0.004445488388166995118 ),
 .UNSPECIFIED. ) ;
#27044 = DIRECTION ( 'NONE',  ( 1.836909530733573776E-16, -1.000000000000000000, 0.000000000000000000 ) ) ;
#27045 = CARTESIAN_POINT ( 'NONE',  ( 0.6845945791218034371, -8.654967045698466421, 46.10312425586597129 ) ) ;
#27046 = CARTESIAN_POINT ( 'NONE',  ( 0.8751705887134423323, 34.63284514348585930, -33.37254303619518225 ) ) ;
#27047 = ORIENTED_EDGE ( 'NONE', *, *, #45557, .F. ) ;
#27048 = EDGE_CURVE ( 'NONE', #6465, #42044, #28592, .T. ) ;
#27049 = VERTEX_POINT ( 'NONE', #7426 ) ;
#27050 = CARTESIAN_POINT ( 'NONE',  ( -6.078726893082806448, 12.00859800336359129, -15.05282748397562820 ) ) ;
#27051 = CARTESIAN_POINT ( 'NONE',  ( 0.7242003506639982380, 5.529506971589458253, 48.78971435433054893 ) ) ;
#27052 = B_SPLINE_CURVE_WITH_KNOTS ( 'NONE', 3,
 ( #6837, #45110, #30984, #45410 ),
 .UNSPECIFIED., .F., .F.,
 ( 4, 4 ),
 ( 0.000000000000000000, 0.004445488388166993383 ),
 .UNSPECIFIED. ) ;
#27054 = ORIENTED_EDGE ( 'NONE', *, *, #32973, .T. ) ;
#27053 = AXIS2_PLACEMENT_3D ( 'NONE', #56857, #18366, #33704 ) ;
#27055 = VERTEX_POINT ( 'NONE', #34199 ) ;
#27056 = CARTESIAN_POINT ( 'NONE',  ( 4.549368137175248350, 42.06008734272383975, 8.582197505784577629 ) ) ;
#27057 = CARTESIAN_POINT ( 'NONE',  ( 5.959547316686252039, 7.851524054666140451, 18.96456592444103606 ) ) ;
#27058 = DIRECTION ( 'NONE',  ( 0.1736481776669315247, -0.9848077530122079093, 5.551115123125782702E-17 ) ) ;
#27059 = VERTEX_POINT ( 'NONE', #24474 ) ;
#27060 = CARTESIAN_POINT ( 'NONE',  ( 0.7048096507298579061, 7.115188260603842352, -47.58126109679093929 ) ) ;
#27061 = CARTESIAN_POINT ( 'NONE',  ( 0.7044674535452954967, -13.16383595884541613, -47.31295959522628181 ) ) ;
#27062 = CARTESIAN_POINT ( 'NONE',  ( 50.00005079999999680, 0.000000000000000000, 0.000000000000000000 ) ) ;
#27063 = ORIENTED_EDGE ( 'NONE', *, *, #18116, .T. ) ;
#27064 = EDGE_LOOP ( 'NONE', ( #26540, #35088, #42212, #45430 ) ) ;
#27065 = ADVANCED_FACE ( 'NONE', ( #21553 ), #15803, .T. ) ;
#27066 = CARTESIAN_POINT ( 'NONE',  ( 1.088313998177381503, -0.7798619649924283248, 42.90642884828984904 ) ) ;
#27067 = ORIENTED_EDGE ( 'NONE', *, *, #16655, .T. ) ;
#27068 = CARTESIAN_POINT ( 'NONE',  ( 0.6029443449137436017, -48.70980349588596425, 6.236552042235133264 ) ) ;
#27069 = CARTESIAN_POINT ( 'NONE',  ( 4.956445790443988031, 0.000000000000000000, 0.000000000000000000 ) ) ;
#27070 = CARTESIAN_POINT ( 'NONE',  ( 4.967162193818130511, 0.000000000000000000, 0.000000000000000000 ) ) ;
#27071 = CARTESIAN_POINT ( 'NONE',  ( 5.895596859100789899, -2.009647457887034694, 20.01223376606159121 ) ) ;
#27072 = DIRECTION ( 'NONE',  ( 1.000000000000000000, -0.000000000000000000, -0.000000000000000000 ) ) ;
#27073 = EDGE_CURVE ( 'NONE', #11037, #21146, #5385, .T. ) ;
#27074 = B_SPLINE_CURVE_WITH_KNOTS ( 'NONE', 3,
 ( #12042, #31116, #20196, #58364, #1354, #20490 ),
 .UNSPECIFIED., .F., .F.,
 ( 4, 2, 4 ),
 ( 3.476216610979977084E-18, 0.0002291459268755713190, 0.0004582918537511391686 ),
 .UNSPECIFIED. ) ;
#27075 = ORIENTED_EDGE ( 'NONE', *, *, #31277, .F. ) ;
#27076 = PLANE ( 'NONE',  #30882 ) ;
#27077 = CARTESIAN_POINT ( 'NONE',  ( 4.691466044806103852, 25.04870410140739523, 36.88741755356078045 ) ) ;
#27078 = EDGE_CURVE ( 'NONE', #42733, #12539, #968, .T. ) ;
#27079 = B_SPLINE_CURVE_WITH_KNOTS ( 'NONE', 3,
 ( #13847, #43280, #57320, #5324, #32951, #52330, #18853, #47051, #10055, #47649, #19161, #33564, #14455, #17, #4086, #42652, #57029, #37974, #14764 ),
 .UNSPECIFIED., .F., .F.,
 ( 4, 3, 3, 3, 3, 3, 4 ),
 ( 3.469870442581001870E-18, 0.0002612768053151703538, 0.0003919133833142884860, 0.0005225499612322571756, 0.0006531865391693334648, 0.0008112755173415197489, 0.0009693688056799711636 ),
 .UNSPECIFIED. ) ;
#27080 = CARTESIAN_POINT ( 'NONE',  ( 5.896782393890504181, -18.51935720350329362, -7.845985957613155648 ) ) ;
#27081 = EDGE_LOOP ( 'NONE', ( #30444, #1992, #50124, #41727, #39108 ) ) ;
#27082 = CARTESIAN_POINT ( 'NONE',  ( 5.959828726073459926, 7.850628836606585281, 18.96492317065697009 ) ) ;
#27083 = DIRECTION ( 'NONE',  ( 1.000000000000000000, 0.000000000000000000, 0.000000000000000000 ) ) ;
#27084 = ADVANCED_FACE ( 'NONE', ( #12173 ), #8146, .F. ) ;
#27085 = CARTESIAN_POINT ( 'NONE',  ( 0.5848930533535030563, -7.620589013870455730, 46.27309915565668064 ) ) ;
#27086 = CARTESIAN_POINT ( 'NONE',  ( 2.618530812446111078, 46.75512741918802107, -4.866708252370782084 ) ) ;
#27087 = EDGE_CURVE ( 'NONE', #18605, #26687, #36835, .T. ) ;
#27088 = VERTEX_POINT ( 'NONE', #27793 ) ;
#27089 = FACE_OUTER_BOUND ( 'NONE', #24754, .T. ) ;
#27090 = CARTESIAN_POINT ( 'NONE',  ( 5.896782393890504181, -15.78060201202832324, 12.46991126736593003 ) ) ;
#27091 = CARTESIAN_POINT ( 'NONE',  ( 1.227938101723756947, 37.58536632582779191, 20.72293514920763258 ) ) ;
#27092 = CARTESIAN_POINT ( 'NONE',  ( 3.661933894777893439, 34.02818518232189149, -32.47635721797108488 ) ) ;
#27093 = CARTESIAN_POINT ( 'NONE',  ( 0.1368894036331292086, 10.43885750709124771, 42.87063773575076198 ) ) ;
#27094 = AXIS2_PLACEMENT_3D ( 'NONE', #33867, #30065, #34477 ) ;
#27095 = EDGE_CURVE ( 'NONE', #11906, #40747, #39848, .T. ) ;
#27096 = FACE_OUTER_BOUND ( 'NONE', #55275, .T. ) ;
#27097 = CARTESIAN_POINT ( 'NONE',  ( 0.9747592971366210168, -5.921534893733859661, -42.49794971112905984 ) ) ;
#27098 = CARTESIAN_POINT ( 'NONE',  ( 0.7246131072078585422, -46.24389631750680962, -13.24054562911110722 ) ) ;
#27099 = ADVANCED_FACE ( 'NONE', ( #50969 ), #36590, .T. ) ;
#27100 = CARTESIAN_POINT ( 'NONE',  ( 4.956653778116975495, 8.845409907520915382, 47.27023054223757015 ) ) ;
#27101 = CARTESIAN_POINT ( 'NONE',  ( 0.7057020205115018818, -19.10543569325825430, 43.92641219669825148 ) ) ;
#27102 = VERTEX_POINT ( 'NONE', #31567 ) ;
#27103 = FACE_OUTER_BOUND ( 'NONE', #28305, .T. ) ;
#27104 = DIRECTION ( 'NONE',  ( 0.000000000000000000, 0.000000000000000000, 1.000000000000000000 ) ) ;
#27105 = CARTESIAN_POINT ( 'NONE',  ( 4.335381028904201628, 35.88831783935764008, 33.34344748710889661 ) ) ;
#27106 = CARTESIAN_POINT ( 'NONE',  ( 0.8744876279028306332, 10.05549467470575209, -48.05452192277493850 ) ) ;
#27107 = B_SPLINE_CURVE_WITH_KNOTS ( 'NONE', 3,
 ( #19660, #42246, #37860, #23730, #18422, #42860, #19053, #47858, #61912, #24346, #43477, #52847, #56921, #9625, #9314, #38780 ),
 .UNSPECIFIED., .F., .F.,
 ( 4, 2, 2, 2, 2, 2, 2, 4 ),
 ( 0.01245102954896282026, 0.01296947782926336466, 0.01348792610956391080, 0.01400637438986445521, 0.01452482267016500135, 0.01556171923076610578, 0.01608016751106664671, 0.01659861579136719112 ),
 .UNSPECIFIED. ) ;
#27108 = CARTESIAN_POINT ( 'NONE',  ( 0.1129192098497455998, -43.69739906996312584, -6.122834499277253428 ) ) ;
#27109 = CARTESIAN_POINT ( 'NONE',  ( 0.9772918015221170318, -30.80181925274452226, 28.41803628810295734 ) ) ;
#27110 = ITEM_DEFINED_TRANSFORMATION ( 'NONE', 'NONE', #41941,  #14677 ) ;
#27111 = CARTESIAN_POINT ( 'NONE',  ( 0.8554163680231708922, -42.27859581856526461, 20.34025095032543007 ) ) ;
#27112 =( BOUNDED_SURFACE ( )  B_SPLINE_SURFACE ( 3, 1, ( 
 ( #21220, #39741 ),
 ( #40060, #45059 ),
 ( #20308, #50039 ),
 ( #20609, #45360 ) ),
 .UNSPECIFIED., .F., .F., .F. ) 
 B_SPLINE_SURFACE_WITH_KNOTS ( ( 4, 4 ),
 ( 2, 2 ),
 ( 0.000000000000000000, 1.000000000000000000 ),
 ( 0.000000000000000000, 1.000000000000000000 ),
 .UNSPECIFIED. ) 
 GEOMETRIC_REPRESENTATION_ITEM ( )  RATIONAL_B_SPLINE_SURFACE ( (
 ( 1.000000000000000000, 1.000000000000000000),
 ( 0.9953390228620291325, 0.8624445117761032620),
 ( 0.9953390228620291325, 0.8624445117761032620),
 ( 1.000000000000000000, 1.000000000000000000) ) ) 
 REPRESENTATION_ITEM ( '' )  SURFACE ( )  );
#27113 = CARTESIAN_POINT ( 'NONE',  ( 0.9790320750461904975, -7.055398401008414311, 41.31051301963263001 ) ) ;
#27114 = CARTESIAN_POINT ( 'NONE',  ( 0.5997462898726536595, -2.096122762665173944, 49.06279547180476897 ) ) ;
#27116 = ORIENTED_EDGE ( 'NONE', *, *, #27361, .T. ) ;
#27115 = DIRECTION ( 'NONE',  ( -0.07500201931887529039, 0.9970919462213602147, -0.01350362464641123410 ) ) ;
#27117 = ORIENTED_EDGE ( 'NONE', *, *, #13975, .T. ) ;
#27118 = CARTESIAN_POINT ( 'NONE',  ( 0.9762797500689124330, 3.691134646837550104, 41.74566217230983511 ) ) ;
#27119 = CARTESIAN_POINT ( 'NONE',  ( 1.227938101723748288, -25.45152231597034387, -34.55893248994532030 ) ) ;
#27120 = DIRECTION ( 'NONE',  ( -1.000000000000000000, -1.836909530733573776E-16, 2.465190328815682145E-32 ) ) ;
#27121 = ADVANCED_FACE ( 'NONE', ( #32819, #8358 ), #31886, .F. ) ;
#27122 = EDGE_LOOP ( 'NONE', ( #4151, #16182, #60857, #42289 ) ) ;
#27123 = CARTESIAN_POINT ( 'NONE',  ( 4.956653778116966613, 0.000000000000000000, 0.000000000000000000 ) ) ;
#27124 = DIRECTION ( 'NONE',  ( 0.000000000000000000, 0.000000000000000000, 1.000000000000000000 ) ) ;
#27125 = CARTESIAN_POINT ( 'NONE',  ( 0.1073791018717578927, 6.109314776652701617, -42.68962945260948061 ) ) ;
#27127 = ADVANCED_FACE ( 'NONE', ( #56284 ), #23802, .T. ) ;
#27126 = ORIENTED_EDGE ( 'NONE', *, *, #37879, .F. ) ;
#27128 = ORIENTED_EDGE ( 'NONE', *, *, #54942, .T. ) ;
#27129 = B_SPLINE_CURVE_WITH_KNOTS ( 'NONE', 3,
 ( #9765, #10083, #29179, #48294 ),
 .UNSPECIFIED., .F., .F.,
 ( 4, 4 ),
 ( 2.153172013482225773E-17, 0.004559932413162188537 ),
 .UNSPECIFIED. ) ;
#27130 = CARTESIAN_POINT ( 'NONE',  ( 0.9790724872846775506, 24.89190385731563282, -33.71540200471602589 ) ) ;
#27131 = CARTESIAN_POINT ( 'NONE',  ( 3.559346040607745287, 37.93169158444295874, 22.23998774920272226 ) ) ;
#27132 = CARTESIAN_POINT ( 'NONE',  ( 0.6031356755773454870, 41.66228085015293203, 24.05369945659548492 ) ) ;
#27133 = ORIENTED_EDGE ( 'NONE', *, *, #43178, .T. ) ;
#27134 = CARTESIAN_POINT ( 'NONE',  ( 0.6846871229502899947, 47.60345020167351038, 5.395516691087355099 ) ) ;
#27135 = DIRECTION ( 'NONE',  ( -1.000000000000000000, -1.836909530733573776E-16, 1.925929944387235853E-32 ) ) ;
#27136 = CIRCLE ( 'NONE', #56142, 43.08621763946400307 ) ;
#27137 = CARTESIAN_POINT ( 'NONE',  ( 3.660176727303400934, -39.22755245663866930, 27.72864483302505434 ) ) ;
#27138 = CARTESIAN_POINT ( 'NONE',  ( -6.077587904424778920, -6.644566705895037728, 18.07334376048996916 ) ) ;
#27139 = ORIENTED_EDGE ( 'NONE', *, *, #22781, .F. ) ;
#27140 = CARTESIAN_POINT ( 'NONE',  ( 4.549368137175248350, 42.06008734272396765, -8.582197505783977221 ) ) ;
#27141 = CARTESIAN_POINT ( 'NONE',  ( 0.5807400328401637335, -47.41494605191439149, -6.791881299636087554 ) ) ;
#27142 = ORIENTED_EDGE ( 'NONE', *, *, #58830, .T. ) ;
#27143 = CARTESIAN_POINT ( 'NONE',  ( 0.5997462898726536595, -20.35457962188229430, 44.69052157405150183 ) ) ;
#27144 = CARTESIAN_POINT ( 'NONE',  ( 4.975801465491695552, 0.000000000000000000, 0.000000000000000000 ) ) ;
#27145 = CARTESIAN_POINT ( 'NONE',  ( 3.660176727303414257, 39.22755245663885404, -27.72864483302478078 ) ) ;
#27146 = EDGE_CURVE ( 'NONE', #17051, #27319, #32387, .T. ) ;
#27147 = ORIENTED_EDGE ( 'NONE', *, *, #29983, .T. ) ;
#27148 = ORIENTED_EDGE ( 'NONE', *, *, #28715, .F. ) ;
#27149 = CARTESIAN_POINT ( 'NONE',  ( 3.782625744892852637, -28.43542810602084359, -30.96230825572154544 ) ) ;
#27150 = CARTESIAN_POINT ( 'NONE',  ( 0.5839880159502343071, 41.45643525694605103, 23.98728323041064314 ) ) ;
#27151 = EDGE_CURVE ( 'NONE', #23973, #50134, #39059, .T. ) ;
#27152 = ORIENTED_EDGE ( 'NONE', *, *, #22492, .T. ) ;
#27153 = DIRECTION ( 'NONE',  ( -1.000000000000000000, -0.000000000000000000, -0.000000000000000000 ) ) ;
#27154 = B_SPLINE_CURVE_WITH_KNOTS ( 'NONE', 3,
 ( #13354, #37477, #32452, #17424, #27431, #55615, #27131, #46255, #51534, #3300, #22121, #22429, #8625, #41558, #27749, #17736, #13054, #32148, #46881, #51229, #3919, #8310, #23058, #61245, #56549 ),
 .UNSPECIFIED., .F., .F.,
 ( 4, 3, 3, 3, 3, 3, 3, 3, 4 ),
 ( 5.553824967135426632E-18, 0.0005656085177311389895, 0.001131215744874499622, 0.001696821861372764615, 0.002262427090022497284, 0.002828031679238744191, 0.003393635864401603128, 0.003977030878808129888, 0.004561030005651157265 ),
 .UNSPECIFIED. ) ;
#27155 = ORIENTED_EDGE ( 'NONE', *, *, #45156, .T. ) ;
#27157 = ORIENTED_EDGE ( 'NONE', *, *, #13002, .F. ) ;
#27156 = EDGE_CURVE ( 'NONE', #44940, #25242, #13641, .T. ) ;
#27158 = FACE_OUTER_BOUND ( 'NONE', #14344, .T. ) ;
#27159 = CARTESIAN_POINT ( 'NONE',  ( 0.9788927965476029724, 24.97331521197592963, 33.65516513040856239 ) ) ;
#27160 = ADVANCED_FACE ( 'NONE', ( #3345 ), #51819, .T. ) ;
#27161 = CARTESIAN_POINT ( 'NONE',  ( 3.660176727303401822, -8.130955556894797098, 47.34518114598556338 ) ) ;
#27162 = ORIENTED_EDGE ( 'NONE', *, *, #28249, .F. ) ;
#27163 = CARTESIAN_POINT ( 'NONE',  ( 0.1145239942831223490, 43.24690139962650903, 8.755055684326428889 ) ) ;
#27164 = ADVANCED_FACE ( 'NONE', ( #51576 ), #24986, .F. ) ;
#27165 = CARTESIAN_POINT ( 'NONE',  ( 4.303969348037246512, 48.06163817123226067, 2.158280495710376279 ) ) ;
#27166 = CARTESIAN_POINT ( 'NONE',  ( -6.072942160501519027, 0.6317110510324334127, -19.24591134337430631 ) ) ;
#27167 =( BOUNDED_SURFACE ( )  B_SPLINE_SURFACE ( 3, 1, ( 
 ( #45735, #55403 ),
 ( #7163, #12527 ),
 ( #55710, #51020 ),
 ( #51322, #8408 ) ),
 .UNSPECIFIED., .F., .F., .F. ) 
 B_SPLINE_SURFACE_WITH_KNOTS ( ( 4, 4 ),
 ( 2, 2 ),
 ( 0.000000000000000000, 1.000000000000000000 ),
 ( 0.000000000000000000, 1.000000000000000000 ),
 .UNSPECIFIED. ) 
 GEOMETRIC_REPRESENTATION_ITEM ( )  RATIONAL_B_SPLINE_SURFACE ( (
 ( 1.000000000000000000, 1.000000000000000000),
 ( 0.7223157951917480446, 0.9931996967497186413),
 ( 0.7223157951917480446, 0.9931996967497186413),
 ( 1.000000000000000000, 1.000000000000000000) ) ) 
 REPRESENTATION_ITEM ( '' )  SURFACE ( )  );
#27168 = EDGE_LOOP ( 'NONE', ( #48768, #4572, #57300, #46787 ) ) ;
#27169 = DIRECTION ( 'NONE',  ( 0.1011922191286468153, -0.9947837607124679904, 0.01286095682984215484 ) ) ;
#27170 = CARTESIAN_POINT ( 'NONE',  ( 0.5988103622719987973, -24.57719485303665863, 41.35593060299629542 ) ) ;
#27171 = EDGE_CURVE ( 'NONE', #50629, #43133, #13400, .T. ) ;
#27172 = CARTESIAN_POINT ( 'NONE',  ( 0.6025881611877910160, 47.72390913208165131, -6.062907795288870361 ) ) ;
#27173 = CARTESIAN_POINT ( 'NONE',  ( 0.6254311100348659558, -37.74260849418475061, -29.82834996731681443 ) ) ;
#27174 = ORIENTED_EDGE ( 'NONE', *, *, #4216, .T. ) ;
#27175 = CARTESIAN_POINT ( 'NONE',  ( 0.1103744047535531458, 37.36621271144537815, -21.52865142340098359 ) ) ;
#27176 = CARTESIAN_POINT ( 'NONE',  ( -6.010958268070873523, 18.68413620842267520, -2.445171577615575575 ) ) ;
#27177 = VERTEX_POINT ( 'NONE', #23101 ) ;
#27178 = CARTESIAN_POINT ( 'NONE',  ( 5.981074661064941900, 19.82308078259083572, 5.320466518161004466 ) ) ;
#27179 = FACE_OUTER_BOUND ( 'NONE', #18389, .T. ) ;
#27180 = CARTESIAN_POINT ( 'NONE',  ( 5.960221823109900008, -18.96526051813975045, -7.849768660536494025 ) ) ;
#27181 = CARTESIAN_POINT ( 'NONE',  ( 0.9968887458511656030, 41.61262323391482454, -10.46947792236050923 ) ) ;
#27182 = CARTESIAN_POINT ( 'NONE',  ( -6.016489644550736315, 18.68142234211827457, -2.463898142942573699 ) ) ;
#27183 = CARTESIAN_POINT ( 'NONE',  ( 3.999999999999990674, -2.309401076758548221, -0.3572655899081733644 ) ) ;
#27184 = VECTOR ( 'NONE', #56875, 1000.000000000000000 ) ;
#27185 = CARTESIAN_POINT ( 'NONE',  ( 4.975801465491695552, -32.01766832630288206, -35.64402118370946937 ) ) ;
#27186 = CARTESIAN_POINT ( 'NONE',  ( 1.227938101723756947, -42.65467462194914816, -4.762198645644879491 ) ) ;
#27187 =( BOUNDED_SURFACE ( )  B_SPLINE_SURFACE ( 3, 1, ( 
 ( #44924, #11705 ),
 ( #2891, #16390 ),
 ( #59912, #36138 ),
 ( #20786, #2583 ) ),
 .UNSPECIFIED., .F., .F., .F. ) 
 B_SPLINE_SURFACE_WITH_KNOTS ( ( 4, 4 ),
 ( 2, 2 ),
 ( 0.000000000000000000, 1.000000000000000000 ),
 ( 0.000000000000000000, 1.000000000000000000 ),
 .UNSPECIFIED. ) 
 GEOMETRIC_REPRESENTATION_ITEM ( )  RATIONAL_B_SPLINE_SURFACE ( (
 ( 1.000000000000000000, 1.000000000000000000),
 ( 0.9952954269826590483, 0.8620686068821339365),
 ( 0.9952954269826590483, 0.8620686068821339365),
 ( 1.000000000000000000, 1.000000000000000000) ) ) 
 REPRESENTATION_ITEM ( '' )  SURFACE ( )  );
#27188 = VECTOR ( 'NONE', #32602, 1000.000000000000000 ) ;
#27189 = CARTESIAN_POINT ( 'NONE',  ( 0.6039202388192953519, 28.23800208753055330, 40.17684595576924522 ) ) ;
#27190 = CARTESIAN_POINT ( 'NONE',  ( -1.139999999999998570, 0.000000000000000000, 0.000000000000000000 ) ) ;
#27191 = CARTESIAN_POINT ( 'NONE',  ( 0.8557997880470697982, -47.89938907511594834, 0.9121262075944505110 ) ) ;
#27192 = CARTESIAN_POINT ( 'NONE',  ( 1.000110580585050979, 9.074284568952180052, 40.91545969842667319 ) ) ;
#27193 = CARTESIAN_POINT ( 'NONE',  ( 0.7954190325252782356, -46.67728753507132922, -11.60747917225568493 ) ) ;
#27194 = CARTESIAN_POINT ( 'NONE',  ( 0.5997462898726536595, -2.096122762664449635, -49.06279547180479739 ) ) ;
#27195 = CARTESIAN_POINT ( 'NONE',  ( 0.5839879327111916485, -24.02664985973677148, -41.43370681949804890 ) ) ;
#27196 = B_SPLINE_CURVE_WITH_KNOTS ( 'NONE', 3,
 ( #61851, #28060, #455, #18991, #38107, #4840, #14287, #9881, #57152, #43415, #33391, #28982, #5148, #20214, #41413, #49312 ),
 .UNSPECIFIED., .F., .F.,
 ( 4, 3, 3, 3, 3, 4 ),
 ( 6.939740885162003740E-18, 0.0002732102107932001369, 0.0004098135523333949239, 0.0005464168938825121526, 0.0008195847345945504910, 0.001092771384553109168 ),
 .UNSPECIFIED. ) ;
#27197 = CARTESIAN_POINT ( 'NONE',  ( -2.601141883200662974, 8.168301201416390711, -12.49296934088642352 ) ) ;
#27198 = DIRECTION ( 'NONE',  ( 0.000000000000000000, 0.000000000000000000, -1.000000000000000000 ) ) ;
#27199 = DIRECTION ( 'NONE',  ( -1.000000000000000000, -0.000000000000000000, -0.000000000000000000 ) ) ;
#27200 = B_SPLINE_CURVE_WITH_KNOTS ( 'NONE', 3,
 ( #6298, #1930, #1611, #15437 ),
 .UNSPECIFIED., .F., .F.,
 ( 4, 4 ),
 ( 7.757919228897728493E-18, 0.004042984057420976295 ),
 .UNSPECIFIED. ) ;
#27201 = EDGE_CURVE ( 'NONE', #39665, #57549, #25804, .T. ) ;
#27202 = ORIENTED_EDGE ( 'NONE', *, *, #41831, .F. ) ;
#27203 = CARTESIAN_POINT ( 'NONE',  ( 0.9757402383260933565, 11.18751708556368918, -41.42435672089860788 ) ) ;
#27204 = CARTESIAN_POINT ( 'NONE',  ( 0.8760168074886960365, -47.56749362999708808, -7.161346975773533963 ) ) ;
#27205 = CARTESIAN_POINT ( 'NONE',  ( 0.9741495583595181085, -39.48917442789106502, -16.78504838919925035 ) ) ;
#27206 = CARTESIAN_POINT ( 'NONE',  ( 4.967162193818131399, -3.259922920618036901, 42.96271701169384016 ) ) ;
#27207 = ORIENTED_EDGE ( 'NONE', *, *, #56510, .F. ) ;
#27208 = DIRECTION ( 'NONE',  ( -0.07906939808003034253, -0.9784699099467746297, -0.1906427696400062044 ) ) ;
#27209 = CARTESIAN_POINT ( 'NONE',  ( 3.270143674763207553, -13.68510027222513514, 0.2742231296309043942 ) ) ;
#27210 = VERTEX_POINT ( 'NONE', #46607 ) ;
#27211 = DIRECTION ( 'NONE',  ( 0.000000000000000000, -1.000000000000000000, 0.000000000000000000 ) ) ;
#27212 = VERTEX_POINT ( 'NONE', #3653 ) ;
#27213 = CARTESIAN_POINT ( 'NONE',  ( 0.8557997880470599172, 47.89938907511594124, 0.9121262075947815795 ) ) ;
#27214 = CARTESIAN_POINT ( 'NONE',  ( 4.963659409799330291, 37.47512675766729018, -24.46566636552785212 ) ) ;
#27215 = B_SPLINE_CURVE_WITH_KNOTS ( 'NONE', 3,
 ( #41645, #46968, #13439, #28140, #23144, #13762, #18139, #47570, #4005, #42272, #60710, #32239, #61330, #42889, #18445, #28442 ),
 .UNSPECIFIED., .F., .F.,
 ( 4, 3, 3, 3, 3, 4 ),
 ( 1.040890552917501732E-17, 0.0002732102107931885359, 0.0004098135523333784440, 0.0005464168938824964317, 0.0008195847345945472383, 0.001092771384553108951 ),
 .UNSPECIFIED. ) ;
#27216 = ORIENTED_EDGE ( 'NONE', *, *, #25556, .F. ) ;
#27217 = CARTESIAN_POINT ( 'NONE',  ( -6.063463321072276813, -16.13029782234890419, 10.51826718817296502 ) ) ;
#27218 = CARTESIAN_POINT ( 'NONE',  ( 0.5839880159502323087, -29.19321933421524307, 37.97080096460575049 ) ) ;
#27219 = VERTEX_POINT ( 'NONE', #18093 ) ;
#27220 = CARTESIAN_POINT ( 'NONE',  ( -16.60577576646023346, 5.000000000000006217, 4.095239503579248533E-30 ) ) ;
#27221 = CARTESIAN_POINT ( 'NONE',  ( 2.500000000000000000, -2.629050547790028551E-15, -2.041999999999999815 ) ) ;
#27222 = B_SPLINE_CURVE_WITH_KNOTS ( 'NONE', 3,
 ( #30873, #16800, #13034, #7999 ),
 .UNSPECIFIED., .F., .F.,
 ( 4, 4 ),
 ( 2.380737581781750353E-07, 0.002336974151641521731 ),
 .UNSPECIFIED. ) ;
#27223 = CONICAL_SURFACE ( 'NONE', #36234, 42.92674063221959813, 1.485477209440487556 ) ;
#27224 = ORIENTED_EDGE ( 'NONE', *, *, #54161, .F. ) ;
#27225 = CARTESIAN_POINT ( 'NONE',  ( 4.962356264823602814, 41.15374796524927348, -8.809348799717806600 ) ) ;
#27226 = ADVANCED_FACE ( 'NONE', ( #22784 ), #33127, .T. ) ;
#27227 = ORIENTED_EDGE ( 'NONE', *, *, #14097, .T. ) ;
#27228 = CARTESIAN_POINT ( 'NONE',  ( 5.896782393890504181, 16.58545041924871910, -11.37756218478521930 ) ) ;
#27230 = EDGE_CURVE ( 'NONE', #15516, #31937, #12988, .T. ) ;
#27229 = ORIENTED_EDGE ( 'NONE', *, *, #18558, .F. ) ;
#27231 = ORIENTED_EDGE ( 'NONE', *, *, #28279, .F. ) ;
#27232 = CARTESIAN_POINT ( 'NONE',  ( 0.6254087463353951160, 34.49952850220925882, 33.52637152047093849 ) ) ;
#27233 = CARTESIAN_POINT ( 'NONE',  ( 1.231276596079881047, -7.805643096902013411, 41.18675402191647805 ) ) ;
#27234 = CARTESIAN_POINT ( 'NONE',  ( 0.6029443199889047422, -25.45693689080298583, -41.99383295189993248 ) ) ;
#27235 = EDGE_CURVE ( 'NONE', #60897, #25119, #43778, .T. ) ;
#27236 = CARTESIAN_POINT ( 'NONE',  ( 0.1073791018717483448, -16.05399293000841254, 40.02496097243031414 ) ) ;
#27237 = CARTESIAN_POINT ( 'NONE',  ( 2.299746137290199943, 41.78301696717512215, 25.66049163221338958 ) ) ;
#27238 = VERTEX_POINT ( 'NONE', #10231 ) ;
#27239 = CARTESIAN_POINT ( 'NONE',  ( 1.231276596079887264, -39.31472542100218703, 14.54747868495677743 ) ) ;
#27240 = EDGE_CURVE ( 'NONE', #3856, #11901, #3181, .T. ) ;
#27241 = CARTESIAN_POINT ( 'NONE',  ( 0.8551540677456739292, -46.51172240253128365, 11.51835730326464180 ) ) ;
#27242 = CARTESIAN_POINT ( 'NONE',  ( 1.114300000000000068, 0.000000000000000000, 0.000000000000000000 ) ) ;
#27243 = ORIENTED_EDGE ( 'NONE', *, *, #55849, .F. ) ;
#27244 = B_SPLINE_CURVE_WITH_KNOTS ( 'NONE', 3,
 ( #61582, #38440, #41911, #18704, #28394, #9287 ),
 .UNSPECIFIED., .F., .F.,
 ( 4, 2, 4 ),
 ( 7.589415207398530075E-19, 0.0002293801035737091281, 0.0004587602071474174972 ),
 .UNSPECIFIED. ) ;
#27245 = VERTEX_POINT ( 'NONE', #14949 ) ;
#27246 = DIRECTION ( 'NONE',  ( 0.000000000000000000, 0.000000000000000000, 1.000000000000000000 ) ) ;
#27247 = CARTESIAN_POINT ( 'NONE',  ( 0.8760168074886960365, -7.161346975774052659, 47.56749362999700992 ) ) ;
#27248 = B_SPLINE_CURVE_WITH_KNOTS ( 'NONE', 3,
 ( #35367, #50362, #30021, #44469, #45385, #35988, #40692, #31263, #55052, #6807, #58822, #49133, #54739, #7429, #2429, #6185 ),
 .UNSPECIFIED., .F., .F.,
 ( 4, 3, 3, 3, 3, 4 ),
 ( 9.813676791237317679E-18, 0.0002732102107931819765, 0.0004098135523333702041, 0.0005464168938824769161, 0.0008195847345945384563, 0.001092771384553104397 ),
 .UNSPECIFIED. ) ;
#27249 = CARTESIAN_POINT ( 'NONE',  ( 0.2230388203127610658, -42.64472907182734929, 6.380812898000848499 ) ) ;
#27250 = EDGE_LOOP ( 'NONE', ( #25415, #42656, #40647, #24543 ) ) ;
#27251 = CARTESIAN_POINT ( 'NONE',  ( 4.962356264823608143, 34.94214251265138671, -23.45809613945485950 ) ) ;
#27252 = CARTESIAN_POINT ( 'NONE',  ( 0.5848930533535030563, 4.512869149483607956, 46.67876491968481645 ) ) ;
#27253 = ADVANCED_FACE ( 'NONE', ( #39072 ), #48224, .F. ) ;
#27254 = ORIENTED_EDGE ( 'NONE', *, *, #37365, .F. ) ;
#27255 = CARTESIAN_POINT ( 'NONE',  ( 120.0000507999999968, 9.797174393178825657E-16, -8.000000000000000000 ) ) ;
#27256 = EDGE_CURVE ( 'NONE', #45995, #43148, #53124, .T. ) ;
#27257 = DIRECTION ( 'NONE',  ( -1.000000000000000000, -0.000000000000000000, -0.000000000000000000 ) ) ;
#27258 = CARTESIAN_POINT ( 'NONE',  ( 4.960156602257182357, -20.07163247083116886, -41.85906677498982020 ) ) ;
#27259 = DIRECTION ( 'NONE',  ( 0.000000000000000000, 0.000000000000000000, 1.000000000000000000 ) ) ;
#27260 = CARTESIAN_POINT ( 'NONE',  ( 1.657374760986086271, -43.51830422218594663, 6.859128580039654643 ) ) ;
#27261 = ORIENTED_EDGE ( 'NONE', *, *, #14603, .T. ) ;
#27262 = CARTESIAN_POINT ( 'NONE',  ( 1.157643937452368821, 41.64460120238013729, 4.767542898545625185 ) ) ;
#27263 = CARTESIAN_POINT ( 'NONE',  ( -6.057079549204054558, -18.27326637954053723, 6.076098001356776912 ) ) ;
#27264 =( BOUNDED_SURFACE ( )  B_SPLINE_SURFACE ( 3, 1, ( 
 ( #31911, #60091 ),
 ( #8092, #42256 ),
 ( #22509, #12503 ),
 ( #41029, #51300 ) ),
 .UNSPECIFIED., .F., .F., .F. ) 
 B_SPLINE_SURFACE_WITH_KNOTS ( ( 4, 4 ),
 ( 2, 2 ),
 ( 0.000000000000000000, 1.000000000000000000 ),
 ( 0.000000000000000000, 1.000000000000000000 ),
 .UNSPECIFIED. ) 
 GEOMETRIC_REPRESENTATION_ITEM ( )  RATIONAL_B_SPLINE_SURFACE ( (
 ( 1.000000000000000000, 1.000000000000000000),
 ( 0.7223157951917480446, 0.9931996967497186413),
 ( 0.7223157951917480446, 0.9931996967497186413),
 ( 1.000000000000000000, 1.000000000000000000) ) ) 
 REPRESENTATION_ITEM ( '' )  SURFACE ( )  );
#27265 = CARTESIAN_POINT ( 'NONE',  ( 5.974727161628369032, -16.29297756969656419, 12.48248968439901674 ) ) ;
#27266 = CARTESIAN_POINT ( 'NONE',  ( 0.1103310638050661596, -16.42686748615379244, -39.87325896099736156 ) ) ;
#27267 = CARTESIAN_POINT ( 'NONE',  ( 5.960721111146673579, -7.848955554238384202, -18.96557324978284242 ) ) ;
#27268 = CARTESIAN_POINT ( 'NONE',  ( 0.5797568599927128696, -38.30338218405706385, -27.05690710212579830 ) ) ;
#27269 = CARTESIAN_POINT ( 'NONE',  ( 4.967162193818129623, -32.10009971360051395, -28.74031574030045633 ) ) ;
#27270 = CARTESIAN_POINT ( 'NONE',  ( 0.5806925824938499181, 23.01490136172973067, -40.85996423950240342 ) ) ;
#27271 = EDGE_CURVE ( 'NONE', #26589, #58614, #14419, .T. ) ;
#27272 = CARTESIAN_POINT ( 'NONE',  ( 6.999999999999995559, 58.44237546506807490, 54.69470952477956871 ) ) ;
#27273 = CARTESIAN_POINT ( 'NONE',  ( 0.5809828226811617480, -28.72298383114462439, -38.32755012159175578 ) ) ;
#27274 = ORIENTED_EDGE ( 'NONE', *, *, #43305, .T. ) ;
#27275 = CARTESIAN_POINT ( 'NONE',  ( 0.7762783648524375080, 47.89627393592490989, -0.8897020150999853660 ) ) ;
#27276 = CARTESIAN_POINT ( 'NONE',  ( 0.1119899015040015933, 44.06612416965094781, -2.266717639542120022 ) ) ;
#27277 = CARTESIAN_POINT ( 'NONE',  ( 0.7954196712028491767, -38.68220069891187762, 28.58653687859100501 ) ) ;
#27278 = CARTESIAN_POINT ( 'NONE',  ( -79.49999999999975842, 2.999999999999996891, 1.500000000000000000 ) ) ;
#27279 = ORIENTED_EDGE ( 'NONE', *, *, #24150, .T. ) ;
#27280 =( BOUNDED_SURFACE ( )  B_SPLINE_SURFACE ( 3, 1, ( 
 ( #55622, #8317 ),
 ( #51539, #51858 ),
 ( #46263, #13359 ),
 ( #27138, #18058 ) ),
 .UNSPECIFIED., .F., .F., .F. ) 
 B_SPLINE_SURFACE_WITH_KNOTS ( ( 4, 4 ),
 ( 2, 2 ),
 ( 0.000000000000000000, 1.000000000000000000 ),
 ( 0.000000000000000000, 1.000000000000000000 ),
 .UNSPECIFIED. ) 
 GEOMETRIC_REPRESENTATION_ITEM ( )  RATIONAL_B_SPLINE_SURFACE ( (
 ( 1.000000000000000000, 1.000000000000000000),
 ( 0.9953485035131437453, 0.8621029689291523912),
 ( 0.9953485035131437453, 0.8621029689291523912),
 ( 1.000000000000000000, 1.000000000000000000) ) ) 
 REPRESENTATION_ITEM ( '' )  SURFACE ( )  );
#27281 = CARTESIAN_POINT ( 'NONE',  ( -6.078726893082806448, 5.482141236672210205, -18.45914864585846260 ) ) ;
#27282 = CARTESIAN_POINT ( 'NONE',  ( 4.956445790444004018, -46.73954499432468879, 5.740468958468036398 ) ) ;
#27283 = ORIENTED_EDGE ( 'NONE', *, *, #35132, .F. ) ;
#27284 = CARTESIAN_POINT ( 'NONE',  ( 0.1154773475650540254, 4.057870454246698344, -43.93719742339823853 ) ) ;
#27285 = CARTESIAN_POINT ( 'NONE',  ( -79.49999999999975842, 4.769696007084728961, -1.500000000000002887 ) ) ;
#27286 = FACE_OUTER_BOUND ( 'NONE', #31951, .T. ) ;
#27287 = ORIENTED_EDGE ( 'NONE', *, *, #17492, .F. ) ;
#27288 = CARTESIAN_POINT ( 'NONE',  ( 4.549368137175248350, -8.166781970325423856, -42.14271863032831078 ) ) ;
#27289 = ORIENTED_EDGE ( 'NONE', *, *, #61166, .T. ) ;
#27290 = ORIENTED_EDGE ( 'NONE', *, *, #40629, .F. ) ;
#27291 = CARTESIAN_POINT ( 'NONE',  ( 0.9754292580325137907, -6.395579163414738311, -41.41767779666673732 ) ) ;
#27292 = EDGE_LOOP ( 'NONE', ( #52744, #6449, #25075, #29301 ) ) ;
#27293 = CARTESIAN_POINT ( 'NONE',  ( 0.7044674535452954967, -49.10288787214294359, -0.8420958536080156431 ) ) ;
#27294 = PRODUCT ( 'straight bevel gear(wobble out)_iso_ISO - Straight bevel gear 2M 48GT 47PT 20PA 5FW ---48O1H50MD20.0S1', 'straight bevel gear(wobble out)_iso_ISO - Straight bevel gear 2M 48GT 47PT 20PA 5FW ---48O1H50MD20.0S1', '', ( #36526 ) ) ;
#27295 = ORIENTED_EDGE ( 'NONE', *, *, #36759, .F. ) ;
#27296 = CARTESIAN_POINT ( 'NONE',  ( -6.078726893082806448, 16.77644806189609739, 9.452239506869414498 ) ) ;
#27297 = DIRECTION ( 'NONE',  ( 0.07906939808003034253, -0.8535645278111539946, -0.5149520629629358304 ) ) ;
#27298 = EDGE_CURVE ( 'NONE', #51245, #61317, #21175, .T. ) ;
#27299 = ORIENTED_EDGE ( 'NONE', *, *, #5608, .F. ) ;
#27300 = CARTESIAN_POINT ( 'NONE',  ( 4.000000000000003553, 2.309401076758524685, -5.242734410091827613 ) ) ;
#27301 = CARTESIAN_POINT ( 'NONE',  ( 5.959828726073459926, -19.82738831247209532, -5.308046411395180186 ) ) ;
#27302 = CARTESIAN_POINT ( 'NONE',  ( 0.5806925824938499181, -44.11884900496058748, -15.89809815106991309 ) ) ;
#27303 = CARTESIAN_POINT ( 'NONE',  ( 0.6064515330803583737, 46.89167588063442338, -0.7106821670863709972 ) ) ;
#27304 = ORIENTED_EDGE ( 'NONE', *, *, #20282, .T. ) ;
#27305 = EDGE_CURVE ( 'NONE', #13508, #19147, #60764, .T. ) ;
#27306 = CARTESIAN_POINT ( 'NONE',  ( 0.1073791018717578927, -37.10214135362874543, -21.98088480513651888 ) ) ;
#27307 = ORIENTED_EDGE ( 'NONE', *, *, #46870, .T. ) ;
#27308 = CIRCLE ( 'NONE', #42359, 5.100000000000000533 ) ;
#27309 = CARTESIAN_POINT ( 'NONE',  ( 0.7056759521544992975, -30.91982873080885952, 35.26631566203700885 ) ) ;
#27310 = ORIENTED_EDGE ( 'NONE', *, *, #18619, .T. ) ;
#27311 = B_SPLINE_CURVE_WITH_KNOTS ( 'NONE', 3,
 ( #61619, #19989, #34388, #23745 ),
 .UNSPECIFIED., .F., .F.,
 ( 4, 4 ),
 ( 0.000000000000000000, 0.005014147105413704723 ),
 .UNSPECIFIED. ) ;
#27312 = CARTESIAN_POINT ( 'NONE',  ( 0.1135584504625007651, -12.96809409308794336, 42.17559232219589660 ) ) ;
#27313 = CARTESIAN_POINT ( 'NONE',  ( -6.017396004339686577, 11.47005965438160402, -14.95000090562869310 ) ) ;
#27314 = ORIENTED_EDGE ( 'NONE', *, *, #60812, .F. ) ;
#27315 = DIRECTION ( 'NONE',  ( -0.9990097760809875105, 0.000000000000000000, 0.04449120468828680897 ) ) ;
#27316 = CARTESIAN_POINT ( 'NONE',  ( 4.962356264823601926, -41.65024625884322518, 6.040909239515423579 ) ) ;
#27317 = CARTESIAN_POINT ( 'NONE',  ( 0.6067099128993246326, 24.55985149487322161, 41.12102523654863262 ) ) ;
#27318 = CARTESIAN_POINT ( 'NONE',  ( -48.95476116535499500, 0.000000000000000000, 0.000000000000000000 ) ) ;
#27319 = VERTEX_POINT ( 'NONE', #25247 ) ;
#27320 = VERTEX_POINT ( 'NONE', #35899 ) ;
#27321 = CARTESIAN_POINT ( 'NONE',  ( 0.3622758884714600280, -40.13994584881793770, 15.73321244754782811 ) ) ;
#27322 = CARTESIAN_POINT ( 'NONE',  ( 5.896278296736517710, -20.11285533178147844, 0.005478796673511841103 ) ) ;
#27323 = CARTESIAN_POINT ( 'NONE',  ( 0.9747592971366256798, -16.12077520819477527, 39.76507150545825908 ) ) ;
#27324 = ADVANCED_FACE ( 'NONE', ( #34656 ), #57801, .T. ) ;
#27325 = B_SPLINE_CURVE_WITH_KNOTS ( 'NONE', 3,
 ( #1882, #25702, #39523, #11947 ),
 .UNSPECIFIED., .F., .F.,
 ( 4, 4 ),
 ( 4.906538933386797396E-18, 0.004042984057420978897 ),
 .UNSPECIFIED. ) ;
#27326 = CARTESIAN_POINT ( 'NONE',  ( 3.319141568766058814, -12.31039395171775830, 0.000000000000000000 ) ) ;
#27327 = CONICAL_SURFACE ( 'NONE', #34361, 43.08621763946400307, 1.568696531533066763 ) ;
#27328 = CARTESIAN_POINT ( 'NONE',  ( 0.5800708057587373734, -29.65250565429469276, 37.61306623599830345 ) ) ;
#27329 = CARTESIAN_POINT ( 'NONE',  ( -6.057079549204054558, -19.21795591696652394, 1.225316886878610623 ) ) ;
#27330 = CARTESIAN_POINT ( 'NONE',  ( 3.727782113643637096, 11.85551640071832047, 42.33467263105117695 ) ) ;
#27331 = CARTESIAN_POINT ( 'NONE',  ( 6.999999999999995559, 56.56854249492371878, 56.56854249492391062 ) ) ;
#27332 = B_SPLINE_CURVE_WITH_KNOTS ( 'NONE', 3,
 ( #35364, #6183, #44467, #34431 ),
 .UNSPECIFIED., .F., .F.,
 ( 4, 4 ),
 ( 0.000000000000000000, 0.005004948556313802699 ),
 .UNSPECIFIED. ) ;
#27333 = CARTESIAN_POINT ( 'NONE',  ( 0.8557997880470690211, 0.9121262075946178216, 47.89938907511594124 ) ) ;
#27334 = CARTESIAN_POINT ( 'NONE',  ( -6.077587904424778920, 13.82827771187065302, 13.40055061993020935 ) ) ;
#27335 = CARTESIAN_POINT ( 'NONE',  ( 0.9754292589017201642, 35.75786470076489820, -21.85640818929475415 ) ) ;
#27336 = CARTESIAN_POINT ( 'NONE',  ( 5.895881250540457863, -18.51869114342267508, 7.847659520061995408 ) ) ;
#27337 = CARTESIAN_POINT ( 'NONE',  ( 0.5987334363312691865, 17.52678475750561660, -45.87346425261718252 ) ) ;
#27338 = CARTESIAN_POINT ( 'NONE',  ( 4.958415959904820092, -43.93947138327082058, 11.51202885599944459 ) ) ;
#27339 = CARTESIAN_POINT ( 'NONE',  ( 4.060580049360325461, -20.77244662311260015, 38.72948690144431794 ) ) ;
#27340 = CARTESIAN_POINT ( 'NONE',  ( 0.9756008150404608115, -37.23069985082527467, -21.33101788548767175 ) ) ;
#27341 = EDGE_CURVE ( 'NONE', #40152, #9472, #33840, .T. ) ;
#27342 = CARTESIAN_POINT ( 'NONE',  ( -6.001507490154110336, -4.892199142591176830, -18.19774963328913131 ) ) ;
#27343 = DIRECTION ( 'NONE',  ( -1.000000000000000000, -0.000000000000000000, -0.000000000000000000 ) ) ;
#27345 = VERTEX_POINT ( 'NONE', #54967 ) ;
#27344 = CARTESIAN_POINT ( 'NONE',  ( 4.553261556744873317, -43.85016385001095074, -2.588956575693968976 ) ) ;
#27346 = ORIENTED_EDGE ( 'NONE', *, *, #61197, .F. ) ;
#27347 = DIRECTION ( 'NONE',  ( 1.000000000000000000, 0.000000000000000000, 0.000000000000000000 ) ) ;
#27348 = CARTESIAN_POINT ( 'NONE',  ( 4.962356264823608143, -15.53171314616189846, 39.11523340857994668 ) ) ;
#27349 = CARTESIAN_POINT ( 'NONE',  ( -5.995132425357893702, -13.31880955509717701, -13.33084941932921197 ) ) ;
#27350 = EDGE_LOOP ( 'NONE', ( #54818, #164, #10937, #40130 ) ) ;
#27351 = ORIENTED_EDGE ( 'NONE', *, *, #19682, .T. ) ;
#27352 = CARTESIAN_POINT ( 'NONE',  ( 0.8744876279028263033, 49.04340454744552602, -2.257104511335871422 ) ) ;
#27353 = CARTESIAN_POINT ( 'NONE',  ( 1.227938101723756947, 4.762198645645047357, -42.65467462194912684 ) ) ;
#27354 = PRESENTATION_LAYER_ASSIGNMENT (  '', '', ( #40395 ) ) ;
#27355 = EDGE_CURVE ( 'NONE', #49781, #35221, #7345, .T. ) ;
#27356 =( BOUNDED_SURFACE ( )  B_SPLINE_SURFACE ( 3, 1, ( 
 ( #30778, #49898 ),
 ( #1957, #6325 ),
 ( #59277, #43685 ),
 ( #58038, #15776 ) ),
 .UNSPECIFIED., .F., .F., .F. ) 
 B_SPLINE_SURFACE_WITH_KNOTS ( ( 4, 4 ),
 ( 2, 2 ),
 ( 0.000000000000000000, 1.000000000000000000 ),
 ( 0.000000000000000000, 1.000000000000000000 ),
 .UNSPECIFIED. ) 
 GEOMETRIC_REPRESENTATION_ITEM ( )  RATIONAL_B_SPLINE_SURFACE ( (
 ( 1.000000000000000000, 1.000000000000000000),
 ( 0.9953040768229005630, 0.8617119497784937465),
 ( 0.9953040768229005630, 0.8617119497784937465),
 ( 1.000000000000000000, 1.000000000000000000) ) ) 
 REPRESENTATION_ITEM ( '' )  SURFACE ( )  );
#27357 = UNCERTAINTY_MEASURE_WITH_UNIT (LENGTH_MEASURE( 1.000000000000000082E-05 ), #24648, 'distance_accuracy_value', 'NONE');
#27358 = ORIENTED_EDGE ( 'NONE', *, *, #18988, .T. ) ;
#27359 = EDGE_LOOP ( 'NONE', ( #11728, #40380, #51874, #21685 ) ) ;
#27360 = FACE_OUTER_BOUND ( 'NONE', #35472, .T. ) ;
#27361 = EDGE_CURVE ( 'NONE', #24606, #34885, #14816, .T. ) ;
#27362 = DIRECTION ( 'NONE',  ( 1.000000000000000000, 1.836909530733573776E-16, 0.000000000000000000 ) ) ;
#27363 = CARTESIAN_POINT ( 'NONE',  ( 0.9730545539215883499, -41.31259007387239279, 11.59290486963492128 ) ) ;
#27364 = ORIENTED_EDGE ( 'NONE', *, *, #58906, .F. ) ;
#27365 = PLANE ( 'NONE',  #22049 ) ;
#27366 = CIRCLE ( 'NONE', #6359, 42.08604991992415023 ) ;
#27367 = CARTESIAN_POINT ( 'NONE',  ( 4.967162193818130511, 0.000000000000000000, 0.000000000000000000 ) ) ;
#27368 = DIRECTION ( 'NONE',  ( 0.000000000000000000, 0.000000000000000000, -1.000000000000000000 ) ) ;
#27369 = ORIENTED_EDGE ( 'NONE', *, *, #4899, .T. ) ;
#27370 = EDGE_CURVE ( 'NONE', #4827, #14464, #17403, .T. ) ;
#27371 = ORIENTED_EDGE ( 'NONE', *, *, #15426, .F. ) ;
#27372 = CARTESIAN_POINT ( 'NONE',  ( 0.5797568599927138688, 10.25842392134313208, 45.76013600636498779 ) ) ;
#27373 = ORIENTED_EDGE ( 'NONE', *, *, #7985, .F. ) ;
#27374 = CARTESIAN_POINT ( 'NONE',  ( 0.6029442701453591180, -48.69309925925927729, 6.366106320679863373 ) ) ;
#27375 = DIRECTION ( 'NONE',  ( -1.850371707708593823E-16, 1.000000000000000000, 0.000000000000000000 ) ) ;
#27376 = CARTESIAN_POINT ( 'NONE',  ( 0.7056759521544966329, -20.50402326997429014, 42.18215095109947299 ) ) ;
#27377 = CARTESIAN_POINT ( 'NONE',  ( 0.9268187852002115479, -43.84180739359310763, -4.652983706366343064 ) ) ;
#27378 = EDGE_CURVE ( 'NONE', #20909, #37975, #11414, .T. ) ;
#27379 = EDGE_LOOP ( 'NONE', ( #3654, #3565, #7558, #10093 ) ) ;
#27380 = CARTESIAN_POINT ( 'NONE',  ( 1.231276596079881047, 28.52807286890743654, 30.71523773966879745 ) ) ;
#27381 = DIRECTION ( 'NONE',  ( 0.000000000000000000, 0.7071067811865527908, -0.7071067811865421326 ) ) ;
#27382 = EDGE_CURVE ( 'NONE', #37898, #715, #172, .T. ) ;
#27383 = DIRECTION ( 'NONE',  ( 0.000000000000000000, 1.000000000000000000, 0.000000000000000000 ) ) ;
#27384 = EDGE_LOOP ( 'NONE', ( #45055, #54688, #43712, #35537, #19524, #5977 ) ) ;
#27385 = CARTESIAN_POINT ( 'NONE',  ( 0.1365634738349401078, 15.83466825643062670, -41.18404910680874309 ) ) ;
#27386 = CARTESIAN_POINT ( 'NONE',  ( 5.896782393890504181, 12.99025607003319038, -15.35510775321938404 ) ) ;
#27387 = DIRECTION ( 'NONE',  ( 0.000000000000000000, 0.000000000000000000, 1.000000000000000000 ) ) ;
#27388 = CARTESIAN_POINT ( 'NONE',  ( 3.783198216974389627, 33.06596988314798580, 27.54889409286091251 ) ) ;
#27389 = ORIENTED_EDGE ( 'NONE', *, *, #40139, .F. ) ;
#27390 = CARTESIAN_POINT ( 'NONE',  ( 0.8554163680231738898, 37.37991192211431013, -28.35397075908056408 ) ) ;
#27391 = DIRECTION ( 'NONE',  ( -1.000000000000000000, -5.380183451256491399E-17, -1.298891185607892835E-16 ) ) ;
#27392 = CARTESIAN_POINT ( 'NONE',  ( 3.678834586032788234, 47.03015561595837113, -13.66663207842711714 ) ) ;
#27393 = ADVANCED_FACE ( 'NONE', ( #21471 ), #54815, .T. ) ;
#27394 = CIRCLE ( 'NONE', #358, 43.08621763946400307 ) ;
#27395 = CARTESIAN_POINT ( 'NONE',  ( 0.1140933569871964148, -17.51328393204253331, -40.49981278968541432 ) ) ;
#27396 = CARTESIAN_POINT ( 'NONE',  ( 5.880360259849739535, 39.91356965504111542, 26.61251048557263132 ) ) ;
#27397 = CARTESIAN_POINT ( 'NONE',  ( 5.960221823109900008, -5.317678907195576343, 19.82478916873565922 ) ) ;
#27398 = CARTESIAN_POINT ( 'NONE',  ( 0.8557997880470697982, -7.156447707085392018, -47.37054680076713709 ) ) ;
#27399 = CARTESIAN_POINT ( 'NONE',  ( 1.088313998177382391, -22.12859469727364470, 36.76812638579223602 ) ) ;
#27400 = CARTESIAN_POINT ( 'NONE',  ( 0.9780303403264770656, -1.723996957088520299, -41.87323068366033851 ) ) ;
#27401 = CARTESIAN_POINT ( 'NONE',  ( 0.6845945791218034371, 10.02997083120958166, 45.82364243312646579 ) ) ;
#27402 = EDGE_LOOP ( 'NONE', ( #28240, #228, #47775, #54695 ) ) ;
#27403 = CARTESIAN_POINT ( 'NONE',  ( 0.5797568599927145350, -46.74494067847413703, -3.759764572009656636 ) ) ;
#27404 = CARTESIAN_POINT ( 'NONE',  ( 0.5806925824938499181, -25.69265091980040339, 39.23149310256803801 ) ) ;
#27405 = CARTESIAN_POINT ( 'NONE',  ( 0.5806925824938502512, 23.01490136172913026, 40.85996423950273737 ) ) ;
#27406 = CARTESIAN_POINT ( 'NONE',  ( 0.6024113833632039894, -39.22478373599367529, -29.54586620773526917 ) ) ;
#27407 = VECTOR ( 'NONE', #13308, 1000.000000000000114 ) ;
#27408 = CARTESIAN_POINT ( 'NONE',  ( 3.390910168358336918, -24.45985921503985239, -36.54876774549406804 ) ) ;
#27409 = CARTESIAN_POINT ( 'NONE',  ( 1.088908134280558437, -39.34174992079763911, 17.14055988408905762 ) ) ;
#27410 = APPLICATION_PROTOCOL_DEFINITION ( 'draft international standard', 'automotive_design', 1998, #50454 ) ;
#27411 = DIRECTION ( 'NONE',  ( 1.000000000000000000, 0.000000000000000000, 0.000000000000000000 ) ) ;
#27412 = CARTESIAN_POINT ( 'NONE',  ( 0.5809828226811617480, 11.86925843957166471, 46.40184912890843805 ) ) ;
#27413 = CARTESIAN_POINT ( 'NONE',  ( 0.6016118706126978299, -1.922093031779197103, 49.06991556097398188 ) ) ;
#27414 = EDGE_CURVE ( 'NONE', #18533, #35404, #24162, .T. ) ;
#27416 = ORIENTED_EDGE ( 'NONE', *, *, #11911, .T. ) ;
#27415 = CARTESIAN_POINT ( 'NONE',  ( 4.975801465491695552, 40.15204426031497320, 26.14269827151694514 ) ) ;
#27417 = VERTEX_POINT ( 'NONE', #8281 ) ;
#27418 = CARTESIAN_POINT ( 'NONE',  ( 0.7056555295713246023, -37.48482836297252163, 29.82339362082581502 ) ) ;
#27419 = LINE ( 'NONE', #36853, #20522 ) ;
#27420 = CARTESIAN_POINT ( 'NONE',  ( 0.9730545539215883499, 41.57420493492400482, -10.61654491617520080 ) ) ;
#27421 = EDGE_CURVE ( 'NONE', #7786, #1247, #19829, .T. ) ;
#27422 = EDGE_LOOP ( 'NONE', ( #32141, #12289, #56402, #14472 ) ) ;
#27423 = CARTESIAN_POINT ( 'NONE',  ( -2.569797478183790229, -4.218948559326347159, 14.01151037928415555 ) ) ;
#27424 = FACE_BOUND ( 'NONE', #31785, .T. ) ;
#27425 = DIRECTION ( 'NONE',  ( -0.07439287786467650709, 0.4871392060438144989, -0.8701500408883593440 ) ) ;
#27426 = EDGE_CURVE ( 'NONE', #5016, #17395, #35394, .T. ) ;
#27427 = VERTEX_POINT ( 'NONE', #51503 ) ;
#27428 = ORIENTED_EDGE ( 'NONE', *, *, #48852, .F. ) ;
#27429 = FILL_AREA_STYLE_COLOUR ( '', #274 ) ;
#27430 = EDGE_CURVE ( 'NONE', #41260, #45047, #37615, .T. ) ;
#27431 = CARTESIAN_POINT ( 'NONE',  ( 3.894904216938897878, 38.00528577904427863, 22.08444215572074398 ) ) ;
#27432 = CARTESIAN_POINT ( 'NONE',  ( 0.9790850452238858415, 32.85849888024883825, -26.01261966046257257 ) ) ;
#27433 = CARTESIAN_POINT ( 'NONE',  ( 1.296416391601052487, -44.05760425873812380, 1.111252022081158142 ) ) ;
#27434 = B_SPLINE_CURVE_WITH_KNOTS ( 'NONE', 3,
 ( #53033, #42215, #37198, #53336, #33956, #396 ),
 .UNSPECIFIED., .F., .F.,
 ( 4, 2, 4 ),
 ( 0.000000000000000000, 0.0002447195606305712767, 0.0004894391212611425533 ),
 .UNSPECIFIED. ) ;
#27435 = VECTOR ( 'NONE', #13337, 1000.000000000000000 ) ;
#27436 = CARTESIAN_POINT ( 'NONE',  ( 0.1158403557922069033, -42.67143984150880698, -11.22891486459464794 ) ) ;
#27437 = VECTOR ( 'NONE', #42434, 1000.000000000000000 ) ;
#27438 = CARTESIAN_POINT ( 'NONE',  ( 5.910764540655178756, 5.973554503640659874, 19.20463186476631279 ) ) ;
#27439 = ORIENTED_EDGE ( 'NONE', *, *, #17420, .T. ) ;
#27440 = EDGE_CURVE ( 'NONE', #26290, #5464, #56219, .T. ) ;
#27441 = CARTESIAN_POINT ( 'NONE',  ( 0.7242003506640002364, 21.98227798157471469, -43.90661828092436991 ) ) ;
#27442 = CARTESIAN_POINT ( 'NONE',  ( 0.8753041380234471980, 17.79089796329372675, -45.76704357430848802 ) ) ;
#27443 = B_SPLINE_CURVE_WITH_KNOTS ( 'NONE', 3,
 ( #47526, #61897, #9603, #187 ),
 .UNSPECIFIED., .F., .F.,
 ( 4, 4 ),
 ( 0.000000000000000000, 0.004442905043737214836 ),
 .UNSPECIFIED. ) ;
#27444 = EDGE_LOOP ( 'NONE', ( #52247, #6779, #15634, #8382 ) ) ;
#27445 = DIRECTION ( 'NONE',  ( -1.000000000000000000, -0.000000000000000000, 1.925929944387235853E-32 ) ) ;
#27446 = EDGE_CURVE ( 'NONE', #26757, #9163, #53989, .T. ) ;
#27447 = CARTESIAN_POINT ( 'NONE',  ( 5.917102823773431552, -9.672968949171048436, 17.63301987068904353 ) ) ;
#27448 = CARTESIAN_POINT ( 'NONE',  ( 0.9762797500689124330, 3.691134646838137190, -41.74566217230977117 ) ) ;
#27449 = CARTESIAN_POINT ( 'NONE',  ( 0.1119899015040010937, -35.02332288806953642, -26.83892997253300194 ) ) ;
#27450 = AXIS2_PLACEMENT_3D ( 'NONE', #43688, #38674, #1038 ) ;
#27451 = EDGE_LOOP ( 'NONE', ( #26902, #59486, #41355, #10684 ) ) ;
#27452 = ORIENTED_EDGE ( 'NONE', *, *, #36805, .F. ) ;
#27453 = CARTESIAN_POINT ( 'NONE',  ( 0.5980894510889457338, 28.72954109785603549, -38.59343625445417558 ) ) ;
#27454 = CARTESIAN_POINT ( 'NONE',  ( -6.078726893082806448, 18.62710865126528859, 4.881072071039118221 ) ) ;
#27455 = ORIENTED_EDGE ( 'NONE', *, *, #10941, .T. ) ;
#27456 = ADVANCED_FACE ( 'NONE', ( #55582 ), #25346, .F. ) ;
#27457 = CARTESIAN_POINT ( 'NONE',  ( 0.5806925824938502512, 4.150136846023314341, -46.71186922509998141 ) ) ;
#27458 = ORIENTED_EDGE ( 'NONE', *, *, #30109, .F. ) ;
#27459 = CARTESIAN_POINT ( 'NONE',  ( 4.975610109902397937, 8.374023221152469887, -48.19050883970174226 ) ) ;
#27460 = ORIENTED_EDGE ( 'NONE', *, *, #47334, .T. ) ;
#27461 = CARTESIAN_POINT ( 'NONE',  ( 0.5997462898726536595, 46.76781179977627545, -14.97743000668059210 ) ) ;
#27462 = CARTESIAN_POINT ( 'NONE',  ( 0.6008122571543326185, -25.08364935383093552, 42.21806586710685849 ) ) ;
#27463 = CARTESIAN_POINT ( 'NONE',  ( 0.8560838555295158248, 46.35895890951125153, 7.156798369940231552 ) ) ;
#27464 = VERTEX_POINT ( 'NONE', #32738 ) ;
#27465 = CARTESIAN_POINT ( 'NONE',  ( 0.1158516988532803660, -27.54943813816733211, -34.46694963445543891 ) ) ;
#27466 = CARTESIAN_POINT ( 'NONE',  ( 0.1158403557922069033, -27.54054956984768054, 34.47402553480782217 ) ) ;
#27467 = CARTESIAN_POINT ( 'NONE',  ( 0.9754292580325136797, 29.55040404863208892, -29.71701679958123066 ) ) ;
#27468 = EDGE_CURVE ( 'NONE', #31086, #46849, #12208, .T. ) ;
#27469 = ORIENTED_EDGE ( 'NONE', *, *, #1530, .F. ) ;
#27470 = CARTESIAN_POINT ( 'NONE',  ( 0.7948884756798507700, 49.04591923990457047, -2.279572440812163148 ) ) ;
#27471 = CARTESIAN_POINT ( 'NONE',  ( 4.967162193818130511, 40.93989340068628024, -13.42934394584121094 ) ) ;
#27472 = CARTESIAN_POINT ( 'NONE',  ( 0.6067375320500720814, -6.954068056451050417, 47.38951440911012725 ) ) ;
#27473 = EDGE_CURVE ( 'NONE', #41472, #129, #1733, .T. ) ;
#27474 = AXIS2_PLACEMENT_3D ( 'NONE', #41937, #36615, #55376 ) ;
#27475 = CARTESIAN_POINT ( 'NONE',  ( 0.6017667736363749853, 47.74032759880255128, -5.933018439714829562 ) ) ;
#27476 = CARTESIAN_POINT ( 'NONE',  ( 4.691466044806104740, -9.025781474741158661, -43.66525414675639638 ) ) ;
#27477 = ORIENTED_EDGE ( 'NONE', *, *, #61913, .F. ) ;
#27478 = B_SPLINE_CURVE_WITH_KNOTS ( 'NONE', 3,
 ( #55845, #35534, #21417, #11725 ),
 .UNSPECIFIED., .F., .F.,
 ( 4, 4 ),
 ( 0.000000000000000000, 0.004444878191957686055 ),
 .UNSPECIFIED. ) ;
#27479 = CARTESIAN_POINT ( 'NONE',  ( 0.7764139734771239310, 39.89513478963794313, 24.66614463233940668 ) ) ;
#27480 = ORIENTED_EDGE ( 'NONE', *, *, #28427, .F. ) ;
#27481 = CARTESIAN_POINT ( 'NONE',  ( 0.5786265663353153954, 17.66171603226140974, -44.52624106864126219 ) ) ;
#27482 = CARTESIAN_POINT ( 'NONE',  ( 4.967162193818130511, 24.30453456948110613, 35.57684288741985768 ) ) ;
#27483 = CARTESIAN_POINT ( 'NONE',  ( 5.910764540655178756, 14.92665574186491462, 13.47947279506933072 ) ) ;
#27484 = CARTESIAN_POINT ( 'NONE',  ( 1.231276596079887264, 32.36747132271594296, -26.63876069172940930 ) ) ;
#27485 = CARTESIAN_POINT ( 'NONE',  ( 5.959547316686252039, 2.682663672454640658, 20.34955788964377632 ) ) ;
#27486 = CARTESIAN_POINT ( 'NONE',  ( 20.55500000000001748, 3.061616997868384127E-16, -2.500000000000000888 ) ) ;
#27487 = DIRECTION ( 'NONE',  ( -1.000000000000000000, -0.000000000000000000, -0.000000000000000000 ) ) ;
#27488 = CARTESIAN_POINT ( 'NONE',  ( 4.834790513006553603, 13.88525928490777162, -45.16402235757200856 ) ) ;
#27489 = DIRECTION ( 'NONE',  ( 0.000000000000000000, 0.000000000000000000, -1.000000000000000000 ) ) ;
#27490 = CONICAL_SURFACE ( 'NONE', #11492, 43.92652462719577500, 1.486293639869522343 ) ;
#27491 = CARTESIAN_POINT ( 'NONE',  ( 0.6024113833632039894, 48.24301168413373375, -9.173532184791364230 ) ) ;
#27492 = LINE ( 'NONE', #11887, #1810 ) ;
#27493 = AXIS2_PLACEMENT_3D ( 'NONE', #38314, #57365, #52682 ) ;
#27494 = CARTESIAN_POINT ( 'NONE',  ( 0.2230388203127611768, 31.02270543585787621, 29.94794547692457343 ) ) ;
#27495 = DIRECTION ( 'NONE',  ( 0.1736481776669315247, -0.9848077530122079093, 5.551115123125782702E-17 ) ) ;
#27496 = CARTESIAN_POINT ( 'NONE',  ( 5.895596859100789899, 16.57987064389777743, -11.38578379577375088 ) ) ;
#27497 = EDGE_CURVE ( 'NONE', #30079, #21310, #48795, .T. ) ;
#27498 = AXIS2_PLACEMENT_3D ( 'NONE', #3253, #55885, #13009 ) ;
#27499 = CARTESIAN_POINT ( 'NONE',  ( -4.938558936750251149, -0.8708011863679817610, 8.896908036367455278E-17 ) ) ;
#27500 = DIRECTION ( 'NONE',  ( 0.000000000000000000, -0.7071067811865461294, -0.7071067811865487940 ) ) ;
#27501 = CARTESIAN_POINT ( 'NONE',  ( 0.5988103564986352323, -41.96244062389634166, -23.52668867203635372 ) ) ;
#27502 = ADVANCED_FACE ( 'NONE', ( #41842 ), #52593, .F. ) ;
#27503 = ORIENTED_EDGE ( 'NONE', *, *, #55638, .F. ) ;
#27504 = CARTESIAN_POINT ( 'NONE',  ( 4.549368137175248350, -13.59764261105780214, 40.71620287708320518 ) ) ;
#27505 = ADVANCED_FACE ( 'NONE', ( #19564 ), #10164, .F. ) ;
#27506 = EDGE_CURVE ( 'NONE', #51246, #5538, #2401, .T. ) ;
#27507 = CARTESIAN_POINT ( 'NONE',  ( 2.359973842542475886, -32.65604482613386494, -29.52488155685024296 ) ) ;
#27508 = CARTESIAN_POINT ( 'NONE',  ( 3.050102900204245682, 28.21179670450542432, -33.75677377774299259 ) ) ;
#27509 = CARTESIAN_POINT ( 'NONE',  ( 4.960156602257181468, -3.546989772330209512, 46.28683144126592452 ) ) ;
#27510 = EDGE_CURVE ( 'NONE', #45271, #37250, #34901, .T. ) ;
#27511 = VERTEX_POINT ( 'NONE', #34277 ) ;
#27512 = CARTESIAN_POINT ( 'NONE',  ( 0.5980271706414734822, -35.76345691233123603, -33.66042769368046095 ) ) ;
#27513 = CARTESIAN_POINT ( 'NONE',  ( 2.618530812446111078, -37.94055228201235508, -27.75322110555974930 ) ) ;
#27514 = ORIENTED_EDGE ( 'NONE', *, *, #28205, .T. ) ;
#27515 = CIRCLE ( 'NONE', #19527, 2.500000000000002220 ) ;
#27516 = EDGE_CURVE ( 'NONE', #7786, #23911, #6156, .T. ) ;
#27517 = CARTESIAN_POINT ( 'NONE',  ( 3.559346040607745287, -25.77953508153773043, 35.62086260215708933 ) ) ;
#27518 = ORIENTED_EDGE ( 'NONE', *, *, #55465, .F. ) ;
#27519 = B_SPLINE_CURVE_WITH_KNOTS ( 'NONE', 3,
 ( #4476, #23617, #33348, #23929 ),
 .UNSPECIFIED., .F., .F.,
 ( 4, 4 ),
 ( 2.168404344971008868E-19, 0.004444878191957648758 ),
 .UNSPECIFIED. ) ;
#27520 = CARTESIAN_POINT ( 'NONE',  ( 0.9762797500689124330, -37.17323042682988188, 19.35137526946117958 ) ) ;
#27521 = DIRECTION ( 'NONE',  ( -1.000000000000000000, 0.000000000000000000, 0.000000000000000000 ) ) ;
#27522 = ORIENTED_EDGE ( 'NONE', *, *, #20722, .F. ) ;
#27523 = CARTESIAN_POINT ( 'NONE',  ( -6.072942160501519915, -16.13052748855437102, 10.51714054436908441 ) ) ;
#27524 = CARTESIAN_POINT ( 'NONE',  ( 0.1073791018717578927, 25.86618856530665767, 34.50606437925554815 ) ) ;
#27525 = VERTEX_POINT ( 'NONE', #24559 ) ;
#27526 = CARTESIAN_POINT ( 'NONE',  ( 0.9754402186311942335, 21.61645729243112868, 37.06569162601108047 ) ) ;
#27527 = CARTESIAN_POINT ( 'NONE',  ( 3.376099380956842921, 6.035099650301375185, -11.97021118623223046 ) ) ;
#27528 = B_SPLINE_CURVE_WITH_KNOTS ( 'NONE', 3,
 ( #27646, #46780, #37072, #23561, #61749, #42088, #57059, #4420, #41775, #42689, #61140, #37688, #32359, #13560, #8220, #43007, #27960, #51432, #8526 ),
 .UNSPECIFIED., .F., .F.,
 ( 4, 3, 3, 3, 3, 3, 4 ),
 ( 3.469446951953614189E-18, 0.0002724573126191751050, 0.0004086839781548431104, 0.0005449106435901767157, 0.0006811373090491364959, 0.0008459866663933654713, 0.001010840725717215317 ),
 .UNSPECIFIED. ) ;
#27529 = EDGE_LOOP ( 'NONE', ( #6242, #622, #60533, #47248 ) ) ;
#27530 = FACE_OUTER_BOUND ( 'NONE', #2534, .T. ) ;
#27532 = ORIENTED_EDGE ( 'NONE', *, *, #3438, .F. ) ;
#27531 =( BOUNDED_SURFACE ( )  B_SPLINE_SURFACE ( 3, 1, ( 
 ( #23078, #42208 ),
 ( #46279, #41578 ),
 ( #61569, #18382 ),
 ( #9271, #8646 ) ),
 .UNSPECIFIED., .F., .F., .F. ) 
 B_SPLINE_SURFACE_WITH_KNOTS ( ( 4, 4 ),
 ( 2, 2 ),
 ( 0.000000000000000000, 1.000000000000000000 ),
 ( 0.000000000000000000, 1.000000000000000000 ),
 .UNSPECIFIED. ) 
 GEOMETRIC_REPRESENTATION_ITEM ( )  RATIONAL_B_SPLINE_SURFACE ( (
 ( 1.000000000000000000, 1.000000000000000000),
 ( 0.9754377213608244057, 0.9999580625633939235),
 ( 0.9754377213608244057, 0.9999580625633939235),
 ( 1.000000000000000000, 1.000000000000000000) ) ) 
 REPRESENTATION_ITEM ( '' )  SURFACE ( )  );
#27533 = CARTESIAN_POINT ( 'NONE',  ( 0.5850706913938534814, 47.46255051844963191, -6.431767090162336054 ) ) ;
#27534 =( GEOMETRIC_REPRESENTATION_CONTEXT ( 3 ) GLOBAL_UNCERTAINTY_ASSIGNED_CONTEXT ( ( #9165 ) ) GLOBAL_UNIT_ASSIGNED_CONTEXT ( ( #26832, #55942, #47188 ) ) REPRESENTATION_CONTEXT ( 'NONE', 'WORKASPACE' ) );
#27535 = ORIENTED_EDGE ( 'NONE', *, *, #48508, .T. ) ;
#27536 = ORIENTED_EDGE ( 'NONE', *, *, #27621, .F. ) ;
#27537 = CARTESIAN_POINT ( 'NONE',  ( 1.500000000000000444, 0.000000000000000000, -5.100000000000000533 ) ) ;
#27538 = CARTESIAN_POINT ( 'NONE',  ( 2.500000000000000000, 2.357898499370431722, -2.818925648462311528E-15 ) ) ;
#27539 = LINE ( 'NONE', #15226, #38472 ) ;
#27540 = CARTESIAN_POINT ( 'NONE',  ( 5.917102823773431552, 19.00193826451969770, -6.589086449814119284 ) ) ;
#27541 = CARTESIAN_POINT ( 'NONE',  ( 0.8557997880470599172, 23.15977007032323343, 41.93815086860265495 ) ) ;
#27542 = ORIENTED_EDGE ( 'NONE', *, *, #10423, .T. ) ;
#27543 = CARTESIAN_POINT ( 'NONE',  ( 0.9758171775293916772, 11.11125068417994122, 41.44488232057071997 ) ) ;
#27544 = CARTESIAN_POINT ( 'NONE',  ( 0.9775691876210965692, -17.98273630898676956, 37.85439081310702392 ) ) ;
#27545 = CARTESIAN_POINT ( 'NONE',  ( 2.533389852662419894, 0.1716090839524149758, 44.01614569741339267 ) ) ;
#27546 = CONICAL_SURFACE ( 'NONE', #26562, 43.08621763946400307, 1.568696531533066763 ) ;
#27548 = ORIENTED_EDGE ( 'NONE', *, *, #56671, .T. ) ;
#27547 = EDGE_CURVE ( 'NONE', #8543, #12597, #23394, .T. ) ;
#27549 = B_SPLINE_CURVE_WITH_KNOTS ( 'NONE', 3,
 ( #548, #19686, #35028, #13068 ),
 .UNSPECIFIED., .F., .F.,
 ( 4, 4 ),
 ( 0.000000000000000000, 0.005013413432710138971 ),
 .UNSPECIFIED. ) ;
#27550 = EDGE_LOOP ( 'NONE', ( #47058, #25086, #24147, #16301 ) ) ;
#27551 =( BOUNDED_SURFACE ( )  B_SPLINE_SURFACE ( 3, 1, ( 
 ( #11395, #48676 ),
 ( #53060, #29874 ),
 ( #39613, #20796 ),
 ( #25478, #39932 ) ),
 .UNSPECIFIED., .F., .F., .F. ) 
 B_SPLINE_SURFACE_WITH_KNOTS ( ( 4, 4 ),
 ( 2, 2 ),
 ( 0.000000000000000000, 1.000000000000000000 ),
 ( 0.000000000000000000, 1.000000000000000000 ),
 .UNSPECIFIED. ) 
 GEOMETRIC_REPRESENTATION_ITEM ( )  RATIONAL_B_SPLINE_SURFACE ( (
 ( 1.000000000000000000, 1.000000000000000000),
 ( 0.9953390228620291325, 0.8624445117761032620),
 ( 0.9953390228620291325, 0.8624445117761032620),
 ( 1.000000000000000000, 1.000000000000000000) ) ) 
 REPRESENTATION_ITEM ( '' )  SURFACE ( )  );
#27552 = CARTESIAN_POINT ( 'NONE',  ( 0.5980271706414711508, 44.54819170408511297, -20.67626317151492898 ) ) ;
#27554 = ADVANCED_FACE ( 'NONE', ( #52127, #4191 ), #28948, .T. ) ;
#27553 = CARTESIAN_POINT ( 'NONE',  ( 1.830465331921977024, 21.46140052792654274, -38.46796515619592327 ) ) ;
#27555 = DIRECTION ( 'NONE',  ( 0.000000000000000000, -1.000000000000000000, 0.000000000000000000 ) ) ;
#27556 = CYLINDRICAL_SURFACE ( 'NONE', #521, 10.00000000000000711 ) ;
#27557 = CARTESIAN_POINT ( 'NONE',  ( 4.958415959904820092, -27.34909152584691583, -36.26611568025293053 ) ) ;
#27558 = ORIENTED_EDGE ( 'NONE', *, *, #37675, .F. ) ;
#27559 = DIRECTION ( 'NONE',  ( 0.000000000000000000, 0.000000000000000000, 1.000000000000000000 ) ) ;
#27560 = CARTESIAN_POINT ( 'NONE',  ( 3.238931869106853600, -9.350562014686421008, 41.96286875554252305 ) ) ;
#27561 = CARTESIAN_POINT ( 'NONE',  ( -1.400000000000000355, 6.245698675651501825E-16, 5.100000000000000533 ) ) ;
#27562 = CARTESIAN_POINT ( 'NONE',  ( 0.8751705887134553219, 23.27176129838425922, -42.09020928323351995 ) ) ;
#27563 = CARTESIAN_POINT ( 'NONE',  ( 1.088908134280553552, 22.12904883058554617, 36.76788378223834286 ) ) ;
#27564 = SURFACE_SIDE_STYLE ('',( #2816 ) ) ;
#27565 = ORIENTED_EDGE ( 'NONE', *, *, #23266, .F. ) ;
#27566 = CARTESIAN_POINT ( 'NONE',  ( 0.9730545539215883499, 21.01499094264601908, -37.40983423658450846 ) ) ;
#27567 = CARTESIAN_POINT ( 'NONE',  ( 0.2885700199627515006, 4.828949117911770728, -42.84523253167937185 ) ) ;
#27568 = CARTESIAN_POINT ( 'NONE',  ( 4.956653778116991482, -31.29546495791826644, -36.51451553856450971 ) ) ;
#27569 = CARTESIAN_POINT ( 'NONE',  ( 0.1092355843206037486, 21.82203846347329090, -37.19569459163113834 ) ) ;
#27570 = B_SPLINE_CURVE_WITH_KNOTS ( 'NONE', 3,
 ( #29701, #10612, #34424, #29092 ),
 .UNSPECIFIED., .F., .F.,
 ( 4, 4 ),
 ( 4.670885906470169154E-18, 0.004566006591234647236 ),
 .UNSPECIFIED. ) ;
#27571 = CARTESIAN_POINT ( 'NONE',  ( 0.5839880159502323087, 6.296669079378848011, -47.48028790449882308 ) ) ;
#27572 = CARTESIAN_POINT ( 'NONE',  ( -6.010958268070873523, -7.224487401384171115, -17.40352239307065219 ) ) ;
#27573 = CARTESIAN_POINT ( 'NONE',  ( 0.5806925824938502512, 22.05663578530182889, -41.38510819338409163 ) ) ;
#27574 = ADVANCED_FACE ( 'NONE', ( #23331 ), #26886, .T. ) ;
#27575 = CIRCLE ( 'NONE', #16445, 85.00000000000001421 ) ;
#27576 = EDGE_CURVE ( 'NONE', #50764, #8016, #18637, .T. ) ;
#27577 = CARTESIAN_POINT ( 'NONE',  ( 0.8560838555295223751, -8.701885300215751684, -46.09392613244852299 ) ) ;
#27578 = ORIENTED_EDGE ( 'NONE', *, *, #47326, .T. ) ;
#27579 = EDGE_CURVE ( 'NONE', #2564, #61765, #30865, .T. ) ;
#27580 = CARTESIAN_POINT ( 'NONE',  ( 0.5997462898726536595, 46.43852004798865352, -15.96920429754923632 ) ) ;
#27581 = CARTESIAN_POINT ( 'NONE',  ( 0.9791128995231614951, 20.14502082081767398, 36.74936149615371761 ) ) ;
#27582 = CARTESIAN_POINT ( 'NONE',  ( 0.6253024248130479856, -42.44617096408522627, -24.69345658074805172 ) ) ;
#27583 = CARTESIAN_POINT ( 'NONE',  ( 4.553261556744875094, 0.000000000000000000, 0.000000000000000000 ) ) ;
#27584 = ADVANCED_FACE ( 'NONE', ( #13952 ), #14201, .F. ) ;
#27585 = ORIENTED_EDGE ( 'NONE', *, *, #10325, .T. ) ;
#27586 = DIRECTION ( 'NONE',  ( 0.000000000000000000, 0.000000000000000000, 1.000000000000000000 ) ) ;
#27587 = CIRCLE ( 'NONE', #49620, 47.91270532121795611 ) ;
#27588 = CARTESIAN_POINT ( 'NONE',  ( 5.974727161628367256, 10.24903993265009206, -17.78288073588492324 ) ) ;
#27589 = B_SPLINE_CURVE_WITH_KNOTS ( 'NONE', 3,
 ( #16784, #7341, #59048, #29942, #20856, #35274, #35589, #49049, #25855, #40604, #54334, #26470, #2651, #16460, #12095, #1412 ),
 .UNSPECIFIED., .F., .F.,
 ( 4, 3, 3, 3, 3, 4 ),
 ( 1.214354834101861570E-17, 0.0002724568934985554386, 0.0004086836638483811227, 0.0005449104342063607661, 0.0008173270854453699259, 0.001089761613562689876 ),
 .UNSPECIFIED. ) ;
#27590 = FILL_AREA_STYLE_COLOUR ( '', #50682 ) ;
#27591 = ORIENTED_EDGE ( 'NONE', *, *, #61318, .T. ) ;
#27592 = CARTESIAN_POINT ( 'NONE',  ( 0.1152339509894530906, 4.014506894015464233, -43.94117004419824468 ) ) ;
#27593 = B_SPLINE_CURVE_WITH_KNOTS ( 'NONE', 3,
 ( #6654, #30796, #39305, #5437, #39937, #29880 ),
 .UNSPECIFIED., .F., .F.,
 ( 4, 2, 4 ),
 ( 0.000000000000000000, 0.0002447195606305739330, 0.0004894391212611478659 ),
 .UNSPECIFIED. ) ;
#27594 = CARTESIAN_POINT ( 'NONE',  ( 0.5980894510889457338, -47.78766676462071672, -5.583794302585086911 ) ) ;
#27595 = CARTESIAN_POINT ( 'NONE',  ( -6.016104459813371719, 2.464823636987443223, 18.68131780085932547 ) ) ;
#27596 = EDGE_LOOP ( 'NONE', ( #52237, #54780, #35645, #26596 ) ) ;
#27597 = B_SPLINE_CURVE_WITH_KNOTS ( 'NONE', 3,
 ( #29566, #5730, #2592, #16398, #35524, #60217, #26406, #17031, #40242, #22333, #50827, #27033, #16098, #54902, #26717, #35214 ),
 .UNSPECIFIED., .F., .F.,
 ( 4, 3, 3, 3, 3, 4 ),
 ( 1.040890552917501732E-17, 0.0002732102107931881022, 0.0004098135523333803956, 0.0005464168938824994675, 0.0008195847345945422510, 0.001092771384553105699 ),
 .UNSPECIFIED. ) ;
#27598 = EDGE_CURVE ( 'NONE', #14660, #38699, #47756, .T. ) ;
#27599 = CARTESIAN_POINT ( 'NONE',  ( 2.299746137290199499, 12.16324681505486360, 47.50091330282182867 ) ) ;
#27600 = ORIENTED_EDGE ( 'NONE', *, *, #9843, .F. ) ;
#27601 = ORIENTED_EDGE ( 'NONE', *, *, #61454, .F. ) ;
#27602 = DIRECTION ( 'NONE',  ( 0.000000000000000000, 1.000000000000000000, -1.224646799147353207E-16 ) ) ;
#27603 = ORIENTED_EDGE ( 'NONE', *, *, #41331, .F. ) ;
#27604 = CARTESIAN_POINT ( 'NONE',  ( 0.5980894510889457338, -13.12879507229256326, -46.28687279963686763 ) ) ;
#27605 = VERTEX_POINT ( 'NONE', #38374 ) ;
#27606 = DIRECTION ( 'NONE',  ( -0.07439287786467652097, 0.9971416435352943308, -0.01320009283086595250 ) ) ;
#27607 = CARTESIAN_POINT ( 'NONE',  ( 0.8557997880470697982, 13.27832040216639520, 46.03118133706031045 ) ) ;
#27608 = CARTESIAN_POINT ( 'NONE',  ( 1.834102595619085507, -0.1089527116822509439, 44.04754106830824867 ) ) ;
#27609 = ORIENTED_EDGE ( 'NONE', *, *, #48813, .F. ) ;
#27610 = CARTESIAN_POINT ( 'NONE',  ( 0.1139756605157202785, 15.61149954950636243, 41.27028351623944502 ) ) ;
#27611 = CARTESIAN_POINT ( 'NONE',  ( 2.618530812446115519, -45.76452502972762204, 10.73941516106128979 ) ) ;
#27612 = CARTESIAN_POINT ( 'NONE',  ( 0.5837157313716042628, -44.27127822390313128, -15.46903319550977685 ) ) ;
#27613 = CARTESIAN_POINT ( 'NONE',  ( 0.5988103622719989083, -41.35593060299654411, -24.57719485303623230 ) ) ;
#27614 = VERTEX_POINT ( 'NONE', #57423 ) ;
#27615 = CARTESIAN_POINT ( 'NONE',  ( 0.8560838555295223751, 43.53454501559562573, 17.46757637357886850 ) ) ;
#27616 = CARTESIAN_POINT ( 'NONE',  ( 0.5988103622719989083, 29.76496569135161252, -37.79415722405566669 ) ) ;
#27617 = ORIENTED_EDGE ( 'NONE', *, *, #13232, .F. ) ;
#27618 = FACE_OUTER_BOUND ( 'NONE', #58548, .T. ) ;
#27619 = ORIENTED_EDGE ( 'NONE', *, *, #48974, .F. ) ;
#27620 = CARTESIAN_POINT ( 'NONE',  ( 0.1152809850208375703, -12.76645052879538866, 42.23698643825781573 ) ) ;
#27621 = EDGE_CURVE ( 'NONE', #5605, #59719, #15122, .T. ) ;
#27622 = CARTESIAN_POINT ( 'NONE',  ( 0.1073791018717578927, -41.52698815987159264, -11.62916352156135780 ) ) ;
#27623 = ORIENTED_EDGE ( 'NONE', *, *, #6009, .F. ) ;
#27624 = DIRECTION ( 'NONE',  ( 0.000000000000000000, 0.000000000000000000, 1.000000000000000000 ) ) ;
#27625 = CARTESIAN_POINT ( 'NONE',  ( -6.016104459813371719, -4.882138007282621928, -18.19977249352315596 ) ) ;
#27626 = DIRECTION ( 'NONE',  ( -1.000000000000000000, -0.000000000000000000, -0.000000000000000000 ) ) ;
#27627 = CARTESIAN_POINT ( 'NONE',  ( 0.5835871038041876568, -1.430526113707234037, -46.87417250405064806 ) ) ;
#27628 =( BOUNDED_SURFACE ( )  B_SPLINE_SURFACE ( 3, 1, ( 
 ( #55170, #41119 ),
 ( #12292, #3166 ),
 ( #22294, #13834 ),
 ( #57309, #42344 ) ),
 .UNSPECIFIED., .F., .F., .F. ) 
 B_SPLINE_SURFACE_WITH_KNOTS ( ( 4, 4 ),
 ( 2, 2 ),
 ( 0.000000000000000000, 1.000000000000000000 ),
 ( 0.000000000000000000, 1.000000000000000000 ),
 .UNSPECIFIED. ) 
 GEOMETRIC_REPRESENTATION_ITEM ( )  RATIONAL_B_SPLINE_SURFACE ( (
 ( 1.000000000000000000, 1.000000000000000000),
 ( 0.9732289882329797637, 0.9999525324661233672),
 ( 0.9732289882329797637, 0.9999525324661233672),
 ( 1.000000000000000000, 1.000000000000000000) ) ) 
 REPRESENTATION_ITEM ( '' )  SURFACE ( )  );
#27629 = VECTOR ( 'NONE', #12922, 1000.000000000000114 ) ;
#27630 = ORIENTED_EDGE ( 'NONE', *, *, #50137, .T. ) ;
#27631 = CARTESIAN_POINT ( 'NONE',  ( 0.5797568599927139799, 45.05935935907746881, 12.99536235818467667 ) ) ;
#27632 = CARTESIAN_POINT ( 'NONE',  ( 0.8551540677456715978, 38.56334384152431483, 28.44084013485131024 ) ) ;
#27633 = CYLINDRICAL_SURFACE ( 'NONE', #52807, 2.698940690764985550 ) ;
#27634 = CARTESIAN_POINT ( 'NONE',  ( 0.6000166863083090663, 46.44114019838995944, -15.97009639238106793 ) ) ;
#27635 = B_SPLINE_CURVE_WITH_KNOTS ( 'NONE', 3,
 ( #51282, #23109, #28108, #60992, #18720, #37531 ),
 .UNSPECIFIED., .F., .F.,
 ( 4, 2, 4 ),
 ( 0.000000000000000000, 0.0002450742804987327125, 0.0004901485609974654250 ),
 .UNSPECIFIED. ) ;
#27636 = DIRECTION ( 'NONE',  ( 0.1305261922200498248, 0.9914448613738106042, 0.000000000000000000 ) ) ;
#27637 = DIRECTION ( 'NONE',  ( 0.000000000000000000, 0.000000000000000000, 1.000000000000000000 ) ) ;
#27638 = CARTESIAN_POINT ( 'NONE',  ( 0.5830082357119558134, 4.965806736280845790, -46.63231495858044440 ) ) ;
#27639 = CARTESIAN_POINT ( 'NONE',  ( 0.5827357941260203900, -46.16863402900289515, 12.74691551863615224 ) ) ;
#27640 = CARTESIAN_POINT ( 'NONE',  ( 4.549368137175248350, -40.58005590356681580, -13.99871866169351442 ) ) ;
#27641 = CARTESIAN_POINT ( 'NONE',  ( 0.9783242366443558602, -12.67232041183570246, 39.94679944108532510 ) ) ;
#27642 = CARTESIAN_POINT ( 'NONE',  ( 2.648799415243708655, -36.17482712903017728, -33.10437048902125667 ) ) ;
#27643 = CARTESIAN_POINT ( 'NONE',  ( -6.078457390727109555, 7.790511441124262859, -17.60972579352727152 ) ) ;
#27644 = LINE ( 'NONE', #23258, #47144 ) ;
#27645 = FACE_OUTER_BOUND ( 'NONE', #61096, .T. ) ;
#27646 = CARTESIAN_POINT ( 'NONE',  ( 0.9730545539215883499, 37.40983423658472873, 21.01499094264562473 ) ) ;
#27647 = CARTESIAN_POINT ( 'NONE',  ( -2.708315649062916552, -7.544341609839897878, -12.54007339125012166 ) ) ;
#27648 = B_SPLINE_CURVE_WITH_KNOTS ( 'NONE', 3,
 ( #44806, #20357, #2139, #10965, #39173, #40114, #16268, #15666, #16580, #39802, #30050, #50093, #39478, #25978, #6212, #54452 ),
 .UNSPECIFIED., .F., .F.,
 ( 4, 3, 3, 3, 3, 4 ),
 ( 2.221635811791082109E-17, 0.0002612764279487699644, 0.0003919131003184752335, 0.0005225497727000622200, 0.0007837925190632447038, 0.001045051706266714132 ),
 .UNSPECIFIED. ) ;
#27649 = SHAPE_REPRESENTATION ( 'Input Eccentric Shaft', ( #14677 ), #15707 ) ;
#27650 = CARTESIAN_POINT ( 'NONE',  ( 0.8557997880470697982, -47.60865952216995822, -5.347802024197736870 ) ) ;
#27651 = ADVANCED_FACE ( 'NONE', ( #20788 ), #23840, .F. ) ;
#27652 = DIRECTION ( 'NONE',  ( 0.09835009131224553558, 0.9632152266566389454, 0.2500873580884741543 ) ) ;
#27653 = CARTESIAN_POINT ( 'NONE',  ( 0.6021448801613057400, -47.56697366610597300, 12.20344848290548079 ) ) ;
#27655 = ORIENTED_EDGE ( 'NONE', *, *, #53113, .F. ) ;
#27654 = CARTESIAN_POINT ( 'NONE',  ( 0.8760168074887076939, 24.81951362746021061, 41.20610493656918294 ) ) ;
#27656 = ORIENTED_EDGE ( 'NONE', *, *, #10264, .T. ) ;
#27657 = CARTESIAN_POINT ( 'NONE',  ( 4.960156602257180580, 20.99019478193107346, -41.40608197274610802 ) ) ;
#27658 = CARTESIAN_POINT ( 'NONE',  ( -6.057079549204054558, -17.34624894862996314, 8.362946760077596409 ) ) ;
#27659 = CARTESIAN_POINT ( 'NONE',  ( 2.060000000000000941, 0.000000000000000000, -0.3080913168122707546 ) ) ;
#27660 = ADVANCED_FACE ( 'NONE', ( #15474 ), #58992, .F. ) ;
#27661 = ORIENTED_EDGE ( 'NONE', *, *, #28194, .T. ) ;
#27662 = ORIENTED_EDGE ( 'NONE', *, *, #60509, .F. ) ;
#27663 = CARTESIAN_POINT ( 'NONE',  ( 1.296416391601053153, -30.87567274504310078, 31.44837367205435186 ) ) ;
#27664 = LINE ( 'NONE', #50846, #25067 ) ;
#27665 = B_SPLINE_CURVE_WITH_KNOTS ( 'NONE', 3,
 ( #15055, #34161, #19144, #28208, #24434, #33859 ),
 .UNSPECIFIED., .F., .F.,
 ( 4, 2, 4 ),
 ( 0.000000000000000000, 0.0002447195606305751798, 0.0004894391212611503596 ),
 .UNSPECIFIED. ) ;
#27666 = ORIENTED_EDGE ( 'NONE', *, *, #1833, .T. ) ;
#27667 = EDGE_LOOP ( 'NONE', ( #7248, #38654, #36956, #48403 ) ) ;
#27668 = CARTESIAN_POINT ( 'NONE',  ( 0.9736507210033062965, -10.66979144439339500, -41.56063510425041585 ) ) ;
#27669 = VECTOR ( 'NONE', #60983, 1000.000000000000114 ) ;
#27670 = EDGE_CURVE ( 'NONE', #12205, #3830, #58834, .T. ) ;
#27671 = DIRECTION ( 'NONE',  ( 0.07439287786467664587, 0.3693942911085579262, 0.9262902123089810091 ) ) ;
#27672 = CARTESIAN_POINT ( 'NONE',  ( 0.5809828226811626362, -18.83114015454730961, 44.03860873105688967 ) ) ;
#27673 = CONICAL_SURFACE ( 'NONE', #5592, 43.08621763946400307, 1.568696531533066763 ) ;
#27674 = ORIENTED_EDGE ( 'NONE', *, *, #23657, .F. ) ;
#27675 = ORIENTED_EDGE ( 'NONE', *, *, #50546, .T. ) ;
#27676 = DIRECTION ( 'NONE',  ( 0.000000000000000000, 0.000000000000000000, -1.000000000000000000 ) ) ;
#27678 = EDGE_LOOP ( 'NONE', ( #30605, #207 ) ) ;
#27677 = EDGE_CURVE ( 'NONE', #58998, #28511, #11088, .T. ) ;
#27679 = CARTESIAN_POINT ( 'NONE',  ( 7.000000000000021316, -80.00000000000001421, -2.649999999999992806 ) ) ;
#27680 = B_SPLINE_CURVE_WITH_KNOTS ( 'NONE', 3,
 ( #13048, #32142, #22115, #55923, #59696, #8011 ),
 .UNSPECIFIED., .F., .F.,
 ( 4, 2, 4 ),
 ( 0.000000000000000000, 0.0002450742804987301646, 0.0004901485609974603292 ),
 .UNSPECIFIED. ) ;
#27681 = CARTESIAN_POINT ( 'NONE',  ( 0.8751705887134423323, -19.22545746485690188, 44.08562551107050353 ) ) ;
#27682 = ORIENTED_EDGE ( 'NONE', *, *, #3991, .F. ) ;
#27683 = FACE_BOUND ( 'NONE', #23859, .T. ) ;
#27684 = ORIENTED_EDGE ( 'NONE', *, *, #47735, .T. ) ;
#27685 = CIRCLE ( 'NONE', #47678, 0.02570000000000870199 ) ;
#27686 = VERTEX_POINT ( 'NONE', #11388 ) ;
#27687 = CARTESIAN_POINT ( 'NONE',  ( 5.960721111146673579, 17.77882586010652943, 10.25731071096588920 ) ) ;
#27688 = ORIENTED_EDGE ( 'NONE', *, *, #3868, .T. ) ;
#27689 = CARTESIAN_POINT ( 'NONE',  ( 0.8557997880470697982, 34.51495345639548873, 33.22501220301912639 ) ) ;
#27690 = CARTESIAN_POINT ( 'NONE',  ( 0.6001305935487422083, 33.64689939321941381, -34.38748867424678224 ) ) ;
#27691 = CARTESIAN_POINT ( 'NONE',  ( 0.6031356219577718170, 33.95537057546184911, -34.07882816221585642 ) ) ;
#27692 = CARTESIAN_POINT ( 'NONE',  ( 5.894904586330512508, -2.011994607810974500, 20.01202862679799210 ) ) ;
#27693 = DIRECTION ( 'NONE',  ( 0.000000000000000000, 0.000000000000000000, 1.000000000000000000 ) ) ;
#27694 = B_SPLINE_CURVE_WITH_KNOTS ( 'NONE', 3,
 ( #31744, #7285, #46167, #6975 ),
 .UNSPECIFIED., .F., .F.,
 ( 4, 4 ),
 ( 5.818439421673296370E-18, 0.004566006591234646368 ),
 .UNSPECIFIED. ) ;
#27695 = VERTEX_POINT ( 'NONE', #25169 ) ;
#27696 = DIRECTION ( 'NONE',  ( -1.000000000000000000, -0.000000000000000000, -0.000000000000000000 ) ) ;
#27697 = CONICAL_SURFACE ( 'NONE', #19701, 43.92652462719577500, 1.486293639869522343 ) ;
#27698 = CARTESIAN_POINT ( 'NONE',  ( 7.000000000000016875, -56.56854249492331377, -56.56854249492430142 ) ) ;
#27699 = CARTESIAN_POINT ( 'NONE',  ( 0.1095718737110178559, 39.93945841550375064, -16.26534146842165995 ) ) ;
#27700 = ADVANCED_FACE ( 'NONE', ( #6962 ), #12197, .F. ) ;
#27701 = ORIENTED_EDGE ( 'NONE', *, *, #35083, .F. ) ;
#27702 = CARTESIAN_POINT ( 'NONE',  ( 0.1095718737110178559, 42.78833451865667570, -5.374020908746496517 ) ) ;
#27703 = CARTESIAN_POINT ( 'NONE',  ( 0.8760168074887090262, -34.63873394077464241, -33.37827814204113253 ) ) ;
#27704 = CARTESIAN_POINT ( 'NONE',  ( 0.9757892942422823346, 30.37715353261994977, 30.30456399643803067 ) ) ;
#27705 = CARTESIAN_POINT ( 'NONE',  ( 0.8751705887134553219, 38.69254731947794568, 28.56654290188667034 ) ) ;
#27706 = ORIENTED_EDGE ( 'NONE', *, *, #34129, .T. ) ;
#27707 = CARTESIAN_POINT ( 'NONE',  ( 0.5786265663353196143, -43.97352617418602705, -18.99608782658079775 ) ) ;
#27708 = CARTESIAN_POINT ( 'NONE',  ( 0.1098349054025745952, -42.78286259078966935, 5.417317591399088528 ) ) ;
#27709 = CARTESIAN_POINT ( 'NONE',  ( 0.5809828226811617480, -0.5448590168535863976, 47.89273459658653564 ) ) ;
#27710 = B_SPLINE_CURVE_WITH_KNOTS ( 'NONE', 3,
 ( #36362, #17241, #54487, #54180, #11944, #45753 ),
 .UNSPECIFIED., .F., .F.,
 ( 4, 2, 4 ),
 ( 3.576224061345498009E-18, 0.0002448709889506552593, 0.0004897419779013069407 ),
 .UNSPECIFIED. ) ;
#27711 = CARTESIAN_POINT ( 'NONE',  ( -1.321505333908964186, 3.855830693249140850, -0.03421028094653189716 ) ) ;
#27712 = CARTESIAN_POINT ( 'NONE',  ( 4.553261556744873317, -39.47791437445913942, 19.26223877088302672 ) ) ;
#27713 = CARTESIAN_POINT ( 'NONE',  ( 0.5848930533535030563, 22.37766167358058667, 41.21302391732886150 ) ) ;
#27714 = CARTESIAN_POINT ( 'NONE',  ( 3.660176727303390276, 40.62966184289491878, 25.63023984566660118 ) ) ;
#27715 = CARTESIAN_POINT ( 'NONE',  ( 4.962356264823608143, 0.000000000000000000, 0.000000000000000000 ) ) ;
#27716 = B_SPLINE_CURVE_WITH_KNOTS ( 'NONE', 3,
 ( #55753, #55446, #16640, #59847, #26036, #26961, #7840, #45171, #21643, #45780, #21958, #49519, #2197, #1899, #30403, #50450, #40167, #60447, #17567 ),
 .UNSPECIFIED., .F., .F.,
 ( 4, 3, 3, 3, 3, 3, 4 ),
 ( 9.813676791237319219E-18, 0.0002724573126191774360, 0.0004086839781548490193, 0.0005449106435901849557, 0.0006811373090491581800, 0.0008459866663933742533, 0.001010840725717204692 ),
 .UNSPECIFIED. ) ;
#27717 = VECTOR ( 'NONE', #14370, 1000.000000000000114 ) ;
#27718 = CARTESIAN_POINT ( 'NONE',  ( 0.9790850452238862855, -1.450985114059958114, -41.88355252914887217 ) ) ;
#27719 = B_SPLINE_CURVE_WITH_KNOTS ( 'NONE', 3,
 ( #5873, #15015, #34125, #49427 ),
 .UNSPECIFIED., .F., .F.,
 ( 4, 4 ),
 ( 2.061695315165020171E-17, 0.004444306975806114161 ),
 .UNSPECIFIED. ) ;
#27720 = CARTESIAN_POINT ( 'NONE',  ( 4.691466044806104740, -37.25818859570289732, -24.49380602310800370 ) ) ;
#27721 = ORIENTED_EDGE ( 'NONE', *, *, #24824, .F. ) ;
#27722 = AXIS2_PLACEMENT_3D ( 'NONE', #1153, #20289, #39407 ) ;
#27723 = FACE_OUTER_BOUND ( 'NONE', #22124, .T. ) ;
#27724 = CARTESIAN_POINT ( 'NONE',  ( 0.6252788684277219566, 32.50271218743920087, -36.81056956410968439 ) ) ;
#27725 = LINE ( 'NONE', #52132, #30832 ) ;
#27726 = CARTESIAN_POINT ( 'NONE',  ( 0.6008122571543326185, -39.61437304146983962, -29.02164707587397174 ) ) ;
#27727 = CARTESIAN_POINT ( 'NONE',  ( 3.050102900204245682, -24.33449941209498846, -36.65047595244580947 ) ) ;
#27728 = CARTESIAN_POINT ( 'NONE',  ( 5.960221823109900008, 0.005450390361438351740, 20.52559243573973546 ) ) ;
#27729 = CONTEXT_DEPENDENT_SHAPE_REPRESENTATION ( #47261, #36310 ) ;
#27730 = CARTESIAN_POINT ( 'NONE',  ( 0.5824935313925957425, -24.92613923739933313, 39.72311367165993801 ) ) ;
#27731 =( BOUNDED_SURFACE ( )  B_SPLINE_SURFACE ( 3, 1, ( 
 ( #61055, #37282 ),
 ( #42293, #32576 ),
 ( #51655, #8746 ),
 ( #56661, #4027 ) ),
 .UNSPECIFIED., .F., .F., .F. ) 
 B_SPLINE_SURFACE_WITH_KNOTS ( ( 4, 4 ),
 ( 2, 2 ),
 ( 0.000000000000000000, 1.000000000000000000 ),
 ( 0.000000000000000000, 1.000000000000000000 ),
 .UNSPECIFIED. ) 
 GEOMETRIC_REPRESENTATION_ITEM ( )  RATIONAL_B_SPLINE_SURFACE ( (
 ( 1.000000000000000000, 1.000000000000000000),
 ( 0.7269869731126821222, 0.9931720237060910339),
 ( 0.7269869731126821222, 0.9931720237060910339),
 ( 1.000000000000000000, 1.000000000000000000) ) ) 
 REPRESENTATION_ITEM ( '' )  SURFACE ( )  );
#27732 = EDGE_CURVE ( 'NONE', #19831, #376, #49585, .T. ) ;
#27733 = CIRCLE ( 'NONE', #6675, 47.91270532121795611 ) ;
#27734 = CARTESIAN_POINT ( 'NONE',  ( 3.782625744892853525, -42.02453477873416432, -1.084703058889718186 ) ) ;
#27736 = ORIENTED_EDGE ( 'NONE', *, *, #35443, .T. ) ;
#27735 = CARTESIAN_POINT ( 'NONE',  ( 0.6028618097248864549, -46.51318640245705183, -12.28244208173044250 ) ) ;
#27737 = ORIENTED_EDGE ( 'NONE', *, *, #44042, .T. ) ;
#27738 = CARTESIAN_POINT ( 'NONE',  ( 0.9972139404380298000, -42.90441115546387607, 0.6581143129158801841 ) ) ;
#27739 = CARTESIAN_POINT ( 'NONE',  ( 4.291220156522060236, -41.03139692541923722, 23.14764488353824134 ) ) ;
#27740 = ADVANCED_FACE ( 'NONE', ( #40236 ), #37825, .F. ) ;
#27741 = ORIENTED_EDGE ( 'NONE', *, *, #22354, .T. ) ;
#27742 = DIRECTION ( 'NONE',  ( 0.000000000000000000, 0.000000000000000000, 1.000000000000000000 ) ) ;
#27743 = CARTESIAN_POINT ( 'NONE',  ( 0.5817217712918340000, -46.04480998170284067, 8.894404294681674372 ) ) ;
#27744 = CARTESIAN_POINT ( 'NONE',  ( 0.1100053167205930493, 5.450899213259504883, -42.77858932361498745 ) ) ;
#27745 = EDGE_CURVE ( 'NONE', #42964, #55548, #38325, .T. ) ;
#27746 = ORIENTED_EDGE ( 'NONE', *, *, #49791, .F. ) ;
#27747 = VERTEX_POINT ( 'NONE', #3202 ) ;
#27748 = CIRCLE ( 'NONE', #36897, 5.453125000000000000 ) ;
#27749 = CARTESIAN_POINT ( 'NONE',  ( 2.185380717157383135, 37.66778067744588299, 22.80258980692837767 ) ) ;
#27750 = CARTESIAN_POINT ( 'NONE',  ( -4.915099999999998914, 12.80000000000000071, 3.000000000000000000 ) ) ;
#27751 = EDGE_CURVE ( 'NONE', #58674, #52304, #59914, .T. ) ;
#27752 = CARTESIAN_POINT ( 'NONE',  ( 0.5804410086790514622, -35.14691939471148885, -31.05179397260405239 ) ) ;
#27753 = CARTESIAN_POINT ( 'NONE',  ( 0.1158816050234199313, -42.68251980219233133, -11.18680225268246708 ) ) ;
#27754 = CARTESIAN_POINT ( 'NONE',  ( -6.015611763856276717, -7.216738110653404981, 17.40650793417841413 ) ) ;
#27755 = AXIS2_PLACEMENT_3D ( 'NONE', #16437, #11755, #34947 ) ;
#27756 = EDGE_LOOP ( 'NONE', ( #49468, #41650, #59303, #42478 ) ) ;
#27757 = CARTESIAN_POINT ( 'NONE',  ( 0.6000166863083090663, -31.02657807334566087, 38.06803035050591433 ) ) ;
#27758 = CARTESIAN_POINT ( 'NONE',  ( 0.7048096507298635682, 48.10291524268443197, -0.8437160066902310573 ) ) ;
#27759 = VECTOR ( 'NONE', #47424, 1000.000000000000000 ) ;
#27760 = ORIENTED_EDGE ( 'NONE', *, *, #21348, .T. ) ;
#27761 = CONICAL_SURFACE ( 'NONE', #31750, 42.08604991992415023, 1.569615340895231137 ) ;
#27762 = CARTESIAN_POINT ( 'NONE',  ( 0.6023142530420679819, -47.72938419887615424, -6.019593586345132863 ) ) ;
#27763 = CARTESIAN_POINT ( 'NONE',  ( 4.303969348037246512, -48.06163817123224646, -2.158280495710712454 ) ) ;
#27764 = CARTESIAN_POINT ( 'NONE',  ( 3.390910168358337362, 38.72858971300023967, -20.83730969620907203 ) ) ;
#27765 = DIRECTION ( 'NONE',  ( -1.000000000000000000, -0.000000000000000000, -0.000000000000000000 ) ) ;
#27766 = ORIENTED_EDGE ( 'NONE', *, *, #39779, .T. ) ;
#27767 = VERTEX_POINT ( 'NONE', #36140 ) ;
#27768 = CARTESIAN_POINT ( 'NONE',  ( 0.1147471544378677044, -44.12318868410672934, 0.3104976971916312833 ) ) ;
#27769 = CARTESIAN_POINT ( 'NONE',  ( 1.500000000000001332, 8.239576745513314221E-16, 6.728125000000023448 ) ) ;
#27770 = CARTESIAN_POINT ( 'NONE',  ( -2.739355103387248747, -0.7412303453947486354, -14.90966614401821388 ) ) ;
#27771 = VERTEX_POINT ( 'NONE', #54896 ) ;
#27772 = CARTESIAN_POINT ( 'NONE',  ( -6.017396004339687465, 7.209881890566553153, 17.40926186480781368 ) ) ;
#27773 = ORIENTED_EDGE ( 'NONE', *, *, #45156, .F. ) ;
#27774 = CARTESIAN_POINT ( 'NONE',  ( 1.088313998177379949, -4.827222641554953064, -42.64115081428568743 ) ) ;
#27775 = CARTESIAN_POINT ( 'NONE',  ( 4.975610109902397937, -11.44439439467527642, -47.55497076097196185 ) ) ;
#27776 = CARTESIAN_POINT ( 'NONE',  ( 0.6021448801613057400, -13.72177509508782833, -47.15139474996232849 ) ) ;
#27777 = ORIENTED_EDGE ( 'NONE', *, *, #36344, .F. ) ;
#27778 = CARTESIAN_POINT ( 'NONE',  ( 3.661921753701998128, 38.05323874046504784, 27.65107855392275837 ) ) ;
#27779 = EDGE_CURVE ( 'NONE', #41166, #24004, #33112, .T. ) ;
#27780 = CARTESIAN_POINT ( 'NONE',  ( 0.1152809850208375841, -27.68358432278522230, 34.35934285653605968 ) ) ;
#27781 = CARTESIAN_POINT ( 'NONE',  ( 4.975610109902397937, 45.11887670192763267, -18.88746601040027784 ) ) ;
#27782 = ADVANCED_FACE ( 'NONE', ( #18255 ), #42209, .F. ) ;
#27783 = VERTEX_POINT ( 'NONE', #22328 ) ;
#27784 = CARTESIAN_POINT ( 'NONE',  ( 0.5988103622719987973, 47.77151394449997213, -5.677495780220555233 ) ) ;
#27785 = CARTESIAN_POINT ( 'NONE',  ( 4.967162193818130511, 0.000000000000000000, 0.000000000000000000 ) ) ;
#27786 = CARTESIAN_POINT ( 'NONE',  ( -6.016489644550736315, 17.40716454747938968, -7.215050741357851294 ) ) ;
#27787 = CARTESIAN_POINT ( 'NONE',  ( 0.1087620492084205998, 26.53886348603002432, -33.99140154262277491 ) ) ;
#27788 = FACE_OUTER_BOUND ( 'NONE', #36640, .T. ) ;
#27789 = ORIENTED_EDGE ( 'NONE', *, *, #17200, .F. ) ;
#27790 = ADVANCED_FACE ( 'NONE', ( #55205 ), #33782, .F. ) ;
#27791 = CONICAL_SURFACE ( 'NONE', #9761, 42.08604991992415023, 1.569615340895231137 ) ;
#27792 = CARTESIAN_POINT ( 'NONE',  ( 5.896278296736517710, 19.70873670457416438, 4.011567913441704825 ) ) ;
#27793 = CARTESIAN_POINT ( 'NONE',  ( 4.967162193818130511, 24.30453456948110613, 35.57684288741985768 ) ) ;
#27794 = ORIENTED_EDGE ( 'NONE', *, *, #3313, .F. ) ;
#27795 = CARTESIAN_POINT ( 'NONE',  ( 0.8753041380234530822, -43.21430456406316978, -23.31656511833100964 ) ) ;
#27796 = CARTESIAN_POINT ( 'NONE',  ( -6.057079549204054558, -17.35362438320633771, 8.347631512370735862 ) ) ;
#27797 = CARTESIAN_POINT ( 'NONE',  ( 3.238931869106854489, 3.793313187126944097, -42.82436385108076138 ) ) ;
#27798 = CARTESIAN_POINT ( 'NONE',  ( 0.3676999524040366896, -31.10876963919527682, 31.27610965031171020 ) ) ;
#27799 = CARTESIAN_POINT ( 'NONE',  ( 5.960721111146673579, -10.26825948882913586, -17.77250458025988422 ) ) ;
#27800 = DIRECTION ( 'NONE',  ( 0.1024043820194936449, -0.1428674944016006809, -0.9844298967354730978 ) ) ;
#27801 = CARTESIAN_POINT ( 'NONE',  ( 50.84889841487235174, 15.27482646519414367, 2.632653459949275465 ) ) ;
#27802 = CARTESIAN_POINT ( 'NONE',  ( 0.08486401232817714080, 0.000000000000000000, -3.000000000000000000 ) ) ;
#27803 = CARTESIAN_POINT ( 'NONE',  ( 0.5786265663353153954, 41.11783955080273500, -24.57327059187355189 ) ) ;
#27804 = CARTESIAN_POINT ( 'NONE',  ( 4.960386119450151732, 32.76426482034242582, -28.99895542006316518 ) ) ;
#27805 = EDGE_CURVE ( 'NONE', #34886, #18589, #48877, .T. ) ;
#27806 =( BOUNDED_SURFACE ( )  B_SPLINE_SURFACE ( 3, 1, ( 
 ( #61935, #24368 ),
 ( #57858, #19676 ),
 ( #19072, #57228 ),
 ( #14365, #42883 ) ),
 .UNSPECIFIED., .F., .F., .F. ) 
 B_SPLINE_SURFACE_WITH_KNOTS ( ( 4, 4 ),
 ( 2, 2 ),
 ( 0.000000000000000000, 1.000000000000000000 ),
 ( 0.000000000000000000, 1.000000000000000000 ),
 .UNSPECIFIED. ) 
 GEOMETRIC_REPRESENTATION_ITEM ( )  RATIONAL_B_SPLINE_SURFACE ( (
 ( 1.000000000000000000, 1.000000000000000000),
 ( 0.9953040768229013402, 0.8617119497784988535),
 ( 0.9953040768229013402, 0.8617119497784988535),
 ( 1.000000000000000000, 1.000000000000000000) ) ) 
 REPRESENTATION_ITEM ( '' )  SURFACE ( )  );
#27807 = CARTESIAN_POINT ( 'NONE',  ( 0.7048096507298635682, 23.32077812596881827, -42.08020459959958970 ) ) ;
#27808 = ORIENTED_EDGE ( 'NONE', *, *, #15802, .T. ) ;
#27809 = AXIS2_PLACEMENT_3D ( 'NONE', #57850, #47869, #14665 ) ;
#27810 = CARTESIAN_POINT ( 'NONE',  ( 0.1129192098497455998, 39.96249028893973332, -18.70698152272436587 ) ) ;
#27811 = CARTESIAN_POINT ( 'NONE',  ( 0.8560838555295223751, -46.85553835019177882, -2.220666565569921591 ) ) ;
#27812 = CARTESIAN_POINT ( 'NONE',  ( 0.3676999524040323597, -43.84864779214683495, 4.821480075982420566 ) ) ;
#27813 = CYLINDRICAL_SURFACE ( 'NONE', #51513, 15.50000000000000000 ) ;
#27814 = CARTESIAN_POINT ( 'NONE',  ( 0.5835226383429296115, 46.50157772193422545, 6.070069514995094728 ) ) ;
#27815 = CARTESIAN_POINT ( 'NONE',  ( 0.6031356755773454870, -38.16618524502141696, 29.28597628606482317 ) ) ;
#27816 = ADVANCED_FACE ( 'NONE', ( #22638 ), #16200, .F. ) ;
#27817 = VERTEX_POINT ( 'NONE', #45533 ) ;
#27818 = CARTESIAN_POINT ( 'NONE',  ( 0.9747592971366234593, 10.79247637456177245, -41.52905920980973775 ) ) ;
#27819 = CARTESIAN_POINT ( 'NONE',  ( 4.335381028904201628, -15.96267600302313383, 46.31360299617006859 ) ) ;
#27821 = VECTOR ( 'NONE', #30243, 1000.000000000000000 ) ;
#27820 = CARTESIAN_POINT ( 'NONE',  ( 1.231276596079881047, 29.74482033789362134, -29.53849072116746655 ) ) ;
#27822 = CARTESIAN_POINT ( 'NONE',  ( 43.00000000000000000, 0.000000000000000000, 0.000000000000000000 ) ) ;
#27823 = ORIENTED_EDGE ( 'NONE', *, *, #44211, .T. ) ;
#27824 = CARTESIAN_POINT ( 'NONE',  ( 0.7245667037590776127, -46.24390958543283858, 13.24050682223013276 ) ) ;
#27825 = EDGE_CURVE ( 'NONE', #4461, #44643, #21107, .T. ) ;
#27826 = CARTESIAN_POINT ( 'NONE',  ( 4.956445790443996913, 2.113652668516264654, 47.04328350079860854 ) ) ;
#27827 = VERTEX_POINT ( 'NONE', #42082 ) ;
#27828 =( GEOMETRIC_REPRESENTATION_CONTEXT ( 3 ) GLOBAL_UNCERTAINTY_ASSIGNED_CONTEXT ( ( #47391 ) ) GLOBAL_UNIT_ASSIGNED_CONTEXT ( ( #10315, #9373, #52591 ) ) REPRESENTATION_CONTEXT ( 'NONE', 'WORKASPACE' ) );
#27829 = CARTESIAN_POINT ( 'NONE',  ( 2.533389852662419894, -26.18899039574286292, 35.37777994427159456 ) ) ;
#27830 = CIRCLE ( 'NONE', #51829, 47.09074272231896430 ) ;
#27831 = ORIENTED_EDGE ( 'NONE', *, *, #39069, .T. ) ;
#27832 = B_SPLINE_CURVE_WITH_KNOTS ( 'NONE', 3,
 ( #5704, #58963, #22315, #40834, #31092, #45832, #46139, #31401, #21384, #51106, #2569, #22008, #60815, #35810, #2254, #2876 ),
 .UNSPECIFIED., .F., .F.,
 ( 4, 3, 3, 3, 3, 4 ),
 ( 1.040890552917501732E-17, 0.0002724568934985567396, 0.0004086836638483815564, 0.0005449104342063605493, 0.0008173270854453664564, 0.001089761613562688141 ),
 .UNSPECIFIED. ) ;
#27833 = CARTESIAN_POINT ( 'NONE',  ( 2.281351352603287364, 47.95523304704249057, 1.314116150903620106 ) ) ;
#27834 = DIRECTION ( 'NONE',  ( -1.000000000000000000, -0.000000000000000000, -0.000000000000000000 ) ) ;
#27835 = EDGE_LOOP ( 'NONE', ( #28013, #31377, #22832, #56307 ) ) ;
#27836 = CARTESIAN_POINT ( 'NONE',  ( 4.335381028904216727, 38.64381571559575690, 30.10668288940879478 ) ) ;
#27837 = ORIENTED_EDGE ( 'NONE', *, *, #680, .T. ) ;
#27838 = CARTESIAN_POINT ( 'NONE',  ( 0.9756950546413940550, 21.53795086961263650, 37.11135009583534128 ) ) ;
#27839 = FACE_OUTER_BOUND ( 'NONE', #1084, .T. ) ;
#27840 = VERTEX_POINT ( 'NONE', #2586 ) ;
#27841 = DIRECTION ( 'NONE',  ( 1.000000000000000000, 0.000000000000000000, 0.000000000000000000 ) ) ;
#27842 = ORIENTED_EDGE ( 'NONE', *, *, #23018, .T. ) ;
#27843 = CARTESIAN_POINT ( 'NONE',  ( 0.5850706913938533704, 47.50996714391791187, -6.071602062250133436 ) ) ;
#27844 = ORIENTED_EDGE ( 'NONE', *, *, #30725, .T. ) ;
#27845 = VERTEX_POINT ( 'NONE', #22026 ) ;
#27846 = CARTESIAN_POINT ( 'NONE',  ( 0.1119899015040012186, 25.70258781475827803, -35.86555851812634899 ) ) ;
#27847 = CARTESIAN_POINT ( 'NONE',  ( 0.6017667736363750963, -34.26315558341214285, 33.76945004754856683 ) ) ;
#27848 = CIRCLE ( 'NONE', #7804, 42.92674063221959813 ) ;
#27849 = CIRCLE ( 'NONE', #25744, 5.000000000000000000 ) ;
#27850 = CARTESIAN_POINT ( 'NONE',  ( 0.1073791018717578927, 21.14095454447508615, 37.58707531572213156 ) ) ;
#27851 = CARTESIAN_POINT ( 'NONE',  ( 3.559346040607745287, -28.99128698353359823, -33.05957592862291250 ) ) ;
#27852 = EDGE_LOOP ( 'NONE', ( #24507, #60268, #11970, #15745 ) ) ;
#27853 = FACE_OUTER_BOUND ( 'NONE', #53339, .T. ) ;
#27854 = ADVANCED_FACE ( 'NONE', ( #56133 ), #46772, .T. ) ;
#27855 = CARTESIAN_POINT ( 'NONE',  ( 5.901463166500145796, 8.452982876530379386, 18.25006714589622803 ) ) ;
#27856 = CARTESIAN_POINT ( 'NONE',  ( 5.895596859100789899, 20.06821053248684805, -1.339816866691640129 ) ) ;
#27857 = EDGE_LOOP ( 'NONE', ( #552, #2772, #25513, #27202 ) ) ;
#27858 = EDGE_CURVE ( 'NONE', #15229, #1725, #55513, .T. ) ;
#27859 = VERTEX_POINT ( 'NONE', #7913 ) ;
#27860 = SURFACE_STYLE_FILL_AREA ( #43215 ) ;
#27861 = CARTESIAN_POINT ( 'NONE',  ( 3.782542959838397945, 23.52698454657985039, 34.83846798499559583 ) ) ;
#27862 = CARTESIAN_POINT ( 'NONE',  ( 0.1073791018717483448, -42.68962945260958008, 6.109314776651994627 ) ) ;
#27863 = CARTESIAN_POINT ( 'NONE',  ( -6.077587904424778920, -17.35179747939691808, -8.349320069797613542 ) ) ;
#27864 = CARTESIAN_POINT ( 'NONE',  ( 2.009741617377216460, -34.45716542851557307, 27.42640749815687329 ) ) ;
#27865 = ADVANCED_FACE ( 'NONE', ( #43306 ), #29004, .F. ) ;
#27866 = ADVANCED_FACE ( 'NONE', ( #19487 ), #28252, .F. ) ;
#27867 = CIRCLE ( 'NONE', #5829, 43.08621763946400307 ) ;
#27868 = VERTEX_POINT ( 'NONE', #23552 ) ;
#27869 = CARTESIAN_POINT ( 'NONE',  ( 4.999999999999997335, 5.204748896376250699E-16, -4.250000000000000000 ) ) ;
#27870 = EDGE_CURVE ( 'NONE', #36560, #31693, #45760, .T. ) ;
#27871 = DIRECTION ( 'NONE',  ( -1.000000000000000000, -0.000000000000000000, -0.000000000000000000 ) ) ;
#27872 = CARTESIAN_POINT ( 'NONE',  ( 0.9791128995231632715, -41.06788468137693826, 8.352621267798951976 ) ) ;
#27873 = DIRECTION ( 'NONE',  ( 0.000000000000000000, 1.000000000000000000, -1.287488025362403787E-15 ) ) ;
#27874 = CARTESIAN_POINT ( 'NONE',  ( 2.533389852662419894, -41.36703057798246164, -15.04058884797672313 ) ) ;
#27875 = AXIS2_PLACEMENT_3D ( 'NONE', #42538, #13720, #14647 ) ;
#27876 = EDGE_CURVE ( 'NONE', #36253, #19244, #4807, .T. ) ;
#27877 = ORIENTED_EDGE ( 'NONE', *, *, #5543, .T. ) ;
#27878 = CARTESIAN_POINT ( 'NONE',  ( 0.8557997880470606944, 47.37054680076706603, 7.156447707085862753 ) ) ;
#27879 = CARTESIAN_POINT ( 'NONE',  ( 0.9762797500689124330, 38.77779312671053447, -15.89363222827765831 ) ) ;
#27880 = EDGE_CURVE ( 'NONE', #7019, #54529, #18554, .T. ) ;
#27881 = CARTESIAN_POINT ( 'NONE',  ( 0.8557997880470599172, 46.50333260518575429, -11.51622788066409697 ) ) ;
#27882 = CARTESIAN_POINT ( 'NONE',  ( 0.1081432562775998391, -16.11101151263798670, -40.00205417854806456 ) ) ;
#27883 = B_SPLINE_CURVE_WITH_KNOTS ( 'NONE', 3,
 ( #56063, #7838, #31348, #41386, #22568, #46386 ),
 .UNSPECIFIED., .F., .F.,
 ( 4, 2, 4 ),
 ( 1.764953265579307567E-18, 0.0002450742804987322246, 0.0004901485609974626061 ),
 .UNSPECIFIED. ) ;
#27884 = AXIS2_PLACEMENT_3D ( 'NONE', #37689, #43008, #56140 ) ;
#27885 = LINE ( 'NONE', #39160, #32241 ) ;
#27886 = FACE_OUTER_BOUND ( 'NONE', #57796, .T. ) ;
#27887 = CARTESIAN_POINT ( 'NONE',  ( 5.960221823109900008, 19.82761049839334788, 5.307149561568152762 ) ) ;
#27888 = CARTESIAN_POINT ( 'NONE',  ( 0.8557997880470690211, -0.9121262075942833114, -47.89938907511595545 ) ) ;
#27889 = CARTESIAN_POINT ( 'NONE',  ( 4.967162193818130511, -38.83676580803754064, -18.65818244221298983 ) ) ;
#27890 = AXIS2_PLACEMENT_3D ( 'NONE', #11327, #30414, #47019 ) ;
#27891 = EDGE_LOOP ( 'NONE', ( #27503, #47617, #10656, #44166 ) ) ;
#27892 = VECTOR ( 'NONE', #53341, 1000.000000000000114 ) ;
#27893 = CARTESIAN_POINT ( 'NONE',  ( 4.962356264823608143, 18.10963840443066530, -37.99048031708887407 ) ) ;
#27894 = FACE_OUTER_BOUND ( 'NONE', #47151, .T. ) ;
#27895 = CARTESIAN_POINT ( 'NONE',  ( 0.8744876279028263033, -42.33402326122615733, -24.86323641237110493 ) ) ;
#27896 = CARTESIAN_POINT ( 'NONE',  ( 0.5797568665920721509, -45.82673094209771847, 9.956708279469337342 ) ) ;
#27897 = ORIENTED_EDGE ( 'NONE', *, *, #47368, .F. ) ;
#27898 = CARTESIAN_POINT ( 'NONE',  ( 0.7044674535453004927, -13.16383595884607871, 47.31295959522610417 ) ) ;
#27899 = CARTESIAN_POINT ( 'NONE',  ( 0.5809828226811617480, 18.83114015454759738, -44.03860873105676177 ) ) ;
#27900 = EDGE_CURVE ( 'NONE', #61413, #41443, #13871, .T. ) ;
#27901 = B_SPLINE_CURVE_WITH_KNOTS ( 'NONE', 3,
 ( #51638, #27846, #33490, #61641, #17841, #28454 ),
 .UNSPECIFIED., .F., .F.,
 ( 4, 2, 4 ),
 ( 1.964714961417949990E-17, 0.0002293755540694315353, 0.0004587511081388433924 ),
 .UNSPECIFIED. ) ;
#27902 =( BOUNDED_SURFACE ( )  B_SPLINE_SURFACE ( 3, 1, ( 
 ( #49968, #49650 ),
 ( #31798, #50271 ),
 ( #54328, #16453 ),
 ( #27090, #12388 ) ),
 .UNSPECIFIED., .F., .F., .F. ) 
 B_SPLINE_SURFACE_WITH_KNOTS ( ( 4, 4 ),
 ( 2, 2 ),
 ( 0.000000000000000000, 1.000000000000000000 ),
 ( 0.000000000000000000, 1.000000000000000000 ),
 .UNSPECIFIED. ) 
 GEOMETRIC_REPRESENTATION_ITEM ( )  RATIONAL_B_SPLINE_SURFACE ( (
 ( 1.000000000000000000, 1.000000000000000000),
 ( 0.9952954269826590483, 0.8620686068821339365),
 ( 0.9952954269826590483, 0.8620686068821339365),
 ( 1.000000000000000000, 1.000000000000000000) ) ) 
 REPRESENTATION_ITEM ( '' )  SURFACE ( )  );
#27903 =( LENGTH_UNIT ( ) NAMED_UNIT ( * ) SI_UNIT ( .MILLI., .METRE. ) );
#27904 = ORIENTED_EDGE ( 'NONE', *, *, #58044, .T. ) ;
#27905 = DIRECTION ( 'NONE',  ( 0.000000000000000000, 0.000000000000000000, 1.000000000000000000 ) ) ;
#27906 = EDGE_CURVE ( 'NONE', #17426, #48474, #36114, .T. ) ;
#27907 = CARTESIAN_POINT ( 'NONE',  ( -6.015611763856276717, 13.32857883366833462, 13.31979030221804017 ) ) ;
#27908 = CARTESIAN_POINT ( 'NONE',  ( 0.7048096507298579061, -5.442192462019134425, -47.80151517212784285 ) ) ;
#27909 = ORIENTED_EDGE ( 'NONE', *, *, #45929, .F. ) ;
#27910 = CARTESIAN_POINT ( 'NONE',  ( 0.8751705887134423323, 46.21789262997739201, 13.30665218149378504 ) ) ;
#27911 = VECTOR ( 'NONE', #35209, 1000.000000000000000 ) ;
#27912 = ORIENTED_EDGE ( 'NONE', *, *, #52261, .F. ) ;
#27913 = EDGE_LOOP ( 'NONE', ( #21266, #42601, #12926, #26839 ) ) ;
#27914 = CARTESIAN_POINT ( 'NONE',  ( 0.5819845901640494645, -5.801229454883635839, -47.54333976522122640 ) ) ;
#27915 = CARTESIAN_POINT ( 'NONE',  ( 0.7044674535452954967, -14.77841640690501457, 46.83376059334789687 ) ) ;
#27916 = ORIENTED_EDGE ( 'NONE', *, *, #56986, .T. ) ;
#27917 = CARTESIAN_POINT ( 'NONE',  ( 5.901463166500145796, -13.99254106127034625, 14.44737571288640865 ) ) ;
#27918 = VERTEX_POINT ( 'NONE', #9762 ) ;
#27919 = CARTESIAN_POINT ( 'NONE',  ( 5.894904586330512508, -19.39796360309176038, -5.314924281188778465 ) ) ;
#27920 =( BOUNDED_SURFACE ( )  B_SPLINE_SURFACE ( 3, 1, ( 
 ( #18923, #38046 ),
 ( #24211, #19532 ),
 ( #705, #32706 ),
 ( #51788, #8886 ) ),
 .UNSPECIFIED., .F., .F., .F. ) 
 B_SPLINE_SURFACE_WITH_KNOTS ( ( 4, 4 ),
 ( 2, 2 ),
 ( 0.000000000000000000, 1.000000000000000000 ),
 ( 0.000000000000000000, 1.000000000000000000 ),
 .UNSPECIFIED. ) 
 GEOMETRIC_REPRESENTATION_ITEM ( )  RATIONAL_B_SPLINE_SURFACE ( (
 ( 1.000000000000000000, 1.000000000000000000),
 ( 0.9754377213608244057, 0.9999580625633939235),
 ( 0.9754377213608244057, 0.9999580625633939235),
 ( 1.000000000000000000, 1.000000000000000000) ) ) 
 REPRESENTATION_ITEM ( '' )  SURFACE ( )  );
#27921 = CARTESIAN_POINT ( 'NONE',  ( 0.9968887458511638267, 0.6574002966414476123, -42.90440775986216693 ) ) ;
#27922 = CARTESIAN_POINT ( 'NONE',  ( 1.231276596079881047, -18.40965318903201364, 37.66113965983544887 ) ) ;
#27923 = ORIENTED_EDGE ( 'NONE', *, *, #17072, .F. ) ;
#27924 = CARTESIAN_POINT ( 'NONE',  ( 4.975610109902397937, 8.374023221151757568, 48.19050883970187016 ) ) ;
#27925 = B_SPLINE_CURVE_WITH_KNOTS ( 'NONE', 3,
 ( #55173, #2555, #40819, #22920, #37331, #12296 ),
 .UNSPECIFIED., .F., .F.,
 ( 4, 2, 4 ),
 ( 0.000000000000000000, 0.0002447195606305757761, 0.0004894391212611515522 ),
 .UNSPECIFIED. ) ;
#27926 = CARTESIAN_POINT ( 'NONE',  ( 0.8753041380234465318, -38.81339214172277963, -30.07754840950027031 ) ) ;
#27927 = ORIENTED_EDGE ( 'NONE', *, *, #39766, .F. ) ;
#27928 = ADVANCED_FACE ( 'NONE', ( #61743 ), #45910, .F. ) ;
#27929 = CARTESIAN_POINT ( 'NONE',  ( 5.960221823109900008, -5.307149561567947593, -19.82761049839340117 ) ) ;
#27930 = CARTESIAN_POINT ( 'NONE',  ( 0.5850706913938534814, -29.30134895053029709, -37.88789093229835458 ) ) ;
#27931 = VERTEX_POINT ( 'NONE', #9448 ) ;
#27932 = CARTESIAN_POINT ( 'NONE',  ( 2.301430502907646058, -1.287492012859730028, 48.01619648598871493 ) ) ;
#27933 = EDGE_CURVE ( 'NONE', #4978, #38949, #32978, .T. ) ;
#27934 = ORIENTED_EDGE ( 'NONE', *, *, #42109, .F. ) ;
#27935 = CARTESIAN_POINT ( 'NONE',  ( 0.7048096507298579061, -46.24547838151358548, -13.26491767067499161 ) ) ;
#27936 = CARTESIAN_POINT ( 'NONE',  ( 0.5830082357119554803, 11.13697854971562329, -45.55436031513902151 ) ) ;
#27937 = ORIENTED_EDGE ( 'NONE', *, *, #57139, .T. ) ;
#27938 = CARTESIAN_POINT ( 'NONE',  ( 0.6846871229502932144, -7.109010606687719225, 47.37786444808391906 ) ) ;
#27939 = CARTESIAN_POINT ( 'NONE',  ( 0.6039202388192953519, -1.399875120786322480, 49.08771804122896043 ) ) ;
#27940 = CARTESIAN_POINT ( 'NONE',  ( 0.5549461598389364703, 8.956512157940801799, -43.18562938561233011 ) ) ;
#27941 = DIRECTION ( 'NONE',  ( -0.1011922191286467460, 0.3909116750757886116, 0.9148487290679595541 ) ) ;
#27942 = EDGE_CURVE ( 'NONE', #40345, #59818, #47867, .T. ) ;
#27943 = EDGE_CURVE ( 'NONE', #47983, #46169, #42381, .T. ) ;
#27944 = AXIS2_PLACEMENT_3D ( 'NONE', #32149, #7698, #45958 ) ;
#27945 = EDGE_LOOP ( 'NONE', ( #21131, #54950, #30136, #56684 ) ) ;
#27946 = CARTESIAN_POINT ( 'NONE',  ( 3.376099380956842921, 12.51418204574263981, 4.806623696325688755 ) ) ;
#27947 = EDGE_CURVE ( 'NONE', #22992, #3856, #56928, .T. ) ;
#27948 = CARTESIAN_POINT ( 'NONE',  ( 0.5807400328401637335, -41.20655774452986719, 24.41979442053154870 ) ) ;
#27949 = CARTESIAN_POINT ( 'NONE',  ( -6.015611763856276717, 7.205255340944849429, -17.41126425312530301 ) ) ;
#27950 = CARTESIAN_POINT ( 'NONE',  ( 5.959547316686252039, -10.25972575517517704, -17.77749189599214219 ) ) ;
#27951 = CARTESIAN_POINT ( 'NONE',  ( 3.238741278300274029, -7.419593128524375913, 42.34697043723798515 ) ) ;
#27952 = DIRECTION ( 'NONE',  ( -0.07836865515943411409, -0.7956898808744429230, -0.6006129930017468643 ) ) ;
#27953 = CARTESIAN_POINT ( 'NONE',  ( 4.967162193818130511, 28.74031574030056646, -32.10009971360042158 ) ) ;
#27954 = CARTESIAN_POINT ( 'NONE',  ( 0.2940133293163028072, -41.18723740816950141, 15.80670820446579050 ) ) ;
#27955 = CARTESIAN_POINT ( 'NONE',  ( 0.9762797500689124330, -11.93232144563832975, 40.17392798947675914 ) ) ;
#27956 = FACE_OUTER_BOUND ( 'NONE', #33165, .T. ) ;
#27957 = DIRECTION ( 'NONE',  ( 0.09835009131224552170, -0.1222230102475082847, 0.9876177374393952935 ) ) ;
#27958 = CARTESIAN_POINT ( 'NONE',  ( 0.8760168074887090262, 17.58183840866401226, -44.77533136581864426 ) ) ;
#27959 = FACE_OUTER_BOUND ( 'NONE', #40420, .T. ) ;
#27960 = CARTESIAN_POINT ( 'NONE',  ( 0.9741495583595177754, 36.96045061395533793, 21.79582154536815608 ) ) ;
#27961 = CARTESIAN_POINT ( 'NONE',  ( 2.009741617377216460, -21.64669824990051694, 38.35263397083436843 ) ) ;
#27962 = SURFACE_STYLE_FILL_AREA ( #9156 ) ;
#27963 = CARTESIAN_POINT ( 'NONE',  ( 0.8560838555295158248, 16.00311602465144745, 44.09391240957503300 ) ) ;
#27965 = ORIENTED_EDGE ( 'NONE', *, *, #45481, .F. ) ;
#27964 = CARTESIAN_POINT ( 'NONE',  ( -90.00000000000000000, 0.000000000000000000, 0.000000000000000000 ) ) ;
#27966 = DIRECTION ( 'NONE',  ( 0.000000000000000000, 0.000000000000000000, 1.000000000000000000 ) ) ;
#27967 = LINE ( 'NONE', #46474, #11494 ) ;
#27968 = CARTESIAN_POINT ( 'NONE',  ( 0.5850706913938534814, -46.31100969101478881, -12.22095376872085382 ) ) ;
#27969 = ORIENTED_EDGE ( 'NONE', *, *, #3259, .T. ) ;
#27970 = ORIENTED_EDGE ( 'NONE', *, *, #659, .T. ) ;
#27971 = CARTESIAN_POINT ( 'NONE',  ( 4.960156602257180580, 26.21519897043481961, -38.31207700265922256 ) ) ;
#27973 = CARTESIAN_POINT ( 'NONE',  ( 0.6017666602106488405, 6.625262199740437730, 47.64919188470830846 ) ) ;
#27972 = B_SPLINE_CURVE_WITH_KNOTS ( 'NONE', 3,
 ( #53537, #29434, #39486, #15672, #24432, #14743 ),
 .UNSPECIFIED., .F., .F.,
 ( 4, 2, 4 ),
 ( 1.487699617223508360E-16, 0.0002445252820015211956, 0.0004890505640028936386 ),
 .UNSPECIFIED. ) ;
#27974 = B_SPLINE_CURVE_WITH_KNOTS ( 'NONE', 3,
 ( #40970, #11511, #30595, #16836, #21519, #45049 ),
 .UNSPECIFIED., .F., .F.,
 ( 4, 2, 4 ),
 ( 2.611104600503255956E-18, 0.0002447193893791691660, 0.0004894387787583357298 ),
 .UNSPECIFIED. ) ;
#27975 = ORIENTED_EDGE ( 'NONE', *, *, #18643, .F. ) ;
#27976 = VERTEX_POINT ( 'NONE', #38000 ) ;
#27977 = EDGE_CURVE ( 'NONE', #60297, #1954, #4114, .T. ) ;
#27978 = CARTESIAN_POINT ( 'NONE',  ( 0.6031356219577718170, -38.21934428970593700, -29.21669799774949539 ) ) ;
#27979 = AXIS2_PLACEMENT_3D ( 'NONE', #9885, #33091, #4845 ) ;
#27980 = DIRECTION ( 'NONE',  ( -1.000000000000000000, -1.836909530733573776E-16, 1.925929944387235853E-32 ) ) ;
#27981 = CARTESIAN_POINT ( 'NONE',  ( 0.9754402186311951217, -41.39745964575704562, 11.28658745892504456 ) ) ;
#27982 = ORIENTED_EDGE ( 'NONE', *, *, #7618, .F. ) ;
#27983 = ORIENTED_EDGE ( 'NONE', *, *, #3177, .T. ) ;
#27984 = CARTESIAN_POINT ( 'NONE',  ( -6.078726893082806448, -17.35055002122458490, 8.351793533709011896 ) ) ;
#27985 = ORIENTED_EDGE ( 'NONE', *, *, #7063, .T. ) ;
#27986 = LINE ( 'NONE', #5073, #18552 ) ;
#27987 = DIRECTION ( 'NONE',  ( -1.000000000000000000, -0.000000000000000000, -0.000000000000000000 ) ) ;
#27988 = CARTESIAN_POINT ( 'NONE',  ( -6.010958268070873523, 18.20513189769808804, 4.863021950010711691 ) ) ;
#27989 = ORIENTED_EDGE ( 'NONE', *, *, #5917, .F. ) ;
#27990 = B_SPLINE_CURVE_WITH_KNOTS ( 'NONE', 3,
 ( #49419, #25618, #30009, #35971 ),
 .UNSPECIFIED., .F., .F.,
 ( 4, 4 ),
 ( 0.000000000000000000, 0.005013413432710155451 ),
 .UNSPECIFIED. ) ;
#27991 = CARTESIAN_POINT ( 'NONE',  ( 2.282803330402966235, -45.75239485235542958, -10.64026657237235973 ) ) ;
#27992 = ORIENTED_EDGE ( 'NONE', *, *, #47889, .T. ) ;
#27993 = ORIENTED_EDGE ( 'NONE', *, *, #40002, .F. ) ;
#27994 = CARTESIAN_POINT ( 'NONE',  ( 5.200000000000002842, 0.000000000000000000, -2.700000000000000622 ) ) ;
#27995 = AXIS2_PLACEMENT_3D ( 'NONE', #10774, #12251, #7198 ) ;
#27996 = VERTEX_POINT ( 'NONE', #57052 ) ;
#27997 = CARTESIAN_POINT ( 'NONE',  ( 0.6021448801613057400, 46.52272187781679946, 15.72187926764014065 ) ) ;
#27998 = CARTESIAN_POINT ( 'NONE',  ( -6.016761891674564211, -13.32172022638601128, 13.32657647165350490 ) ) ;
#27999 = CARTESIAN_POINT ( 'NONE',  ( 5.974727161628369032, 2.663664384318509715, 20.35137732084677253 ) ) ;
#28000 = CARTESIAN_POINT ( 'NONE',  ( 0.5987334308729320709, 16.39078228288969186, -46.29152365957120452 ) ) ;
#28001 = CARTESIAN_POINT ( 'NONE',  ( 0.7948884756798505480, -2.440498779800571505, 49.03817503033675962 ) ) ;
#28002 = EDGE_CURVE ( 'NONE', #36997, #55413, #20341, .T. ) ;
#28003 = VERTEX_POINT ( 'NONE', #10394 ) ;
#28004 = CARTESIAN_POINT ( 'NONE',  ( -6.016761891674564211, 9.418621820384725396, -16.32039929810246903 ) ) ;
#28005 = CARTESIAN_POINT ( 'NONE',  ( 0.1064266418746773885, -10.61815661559970003, -41.79703894102866713 ) ) ;
#28006 = EDGE_CURVE ( 'NONE', #10306, #2188, #61465, .T. ) ;
#28007 = CARTESIAN_POINT ( 'NONE',  ( 0.1100247026804066219, 39.90641708963711665, -16.34612806822719122 ) ) ;
#28008 = ORIENTED_EDGE ( 'NONE', *, *, #47647, .T. ) ;
#28009 = CARTESIAN_POINT ( 'NONE',  ( 0.6252788684277214015, 41.52615316421481140, 26.21112234445213574 ) ) ;
#28010 = ADVANCED_FACE ( 'NONE', ( #6570 ), #35425, .F. ) ;
#28011 = CARTESIAN_POINT ( 'NONE',  ( 2.648799415243708655, -29.47778256948722131, 39.18644916390910993 ) ) ;
#28012 = CARTESIAN_POINT ( 'NONE',  ( 3.559346040607745287, -4.982408603749695963, 43.68759418928067362 ) ) ;
#28013 = ORIENTED_EDGE ( 'NONE', *, *, #50068, .F. ) ;
#28014 = EDGE_LOOP ( 'NONE', ( #20876, #4624, #33807, #57297 ) ) ;
#28015 = FACE_OUTER_BOUND ( 'NONE', #5827, .T. ) ;
#28016 = EDGE_CURVE ( 'NONE', #7742, #41497, #61859, .T. ) ;
#28017 = CARTESIAN_POINT ( 'NONE',  ( -6.016489644550737204, 14.95199950534963484, -11.46752133529369821 ) ) ;
#28018 = CARTESIAN_POINT ( 'NONE',  ( 4.962356264823609031, 31.50371261889155150, -27.90612278853226513 ) ) ;
#28019 = B_SPLINE_CURVE_WITH_KNOTS ( 'NONE', 3,
 ( #4395, #18236, #32642, #27936, #13228, #38282, #61726, #33269, #8822, #18862, #13537, #37347, #42984, #56731, #46441, #51727 ),
 .UNSPECIFIED., .F., .F.,
 ( 4, 3, 3, 3, 3, 4 ),
 ( 1.214354834101861570E-17, 0.0002732102107931902164, 0.0004098135523333812629, 0.0005464168938824976243, 0.0008195847345945407331, 0.001092771384553105699 ),
 .UNSPECIFIED. ) ;
#28020 = CARTESIAN_POINT ( 'NONE',  ( -2.708315649062910779, 13.41752550814502598, 5.842990691604645015 ) ) ;
#28021 = CARTESIAN_POINT ( 'NONE',  ( 0.5830081025819925378, -30.48545850581747985, -35.63521929317017367 ) ) ;
#28022 = CARTESIAN_POINT ( 'NONE',  ( 3.240649175237397372, -39.19469574595558470, 19.97600417449955401 ) ) ;
#28023 = B_SPLINE_CURVE_WITH_KNOTS ( 'NONE', 3,
 ( #10682, #34806, #30082, #20696, #39836, #7181, #51035, #17857, #36053, #55422, #2497, #51342, #50725, #3720, #7816, #21619, #8425, #35740, #41670 ),
 .UNSPECIFIED., .F., .F.,
 ( 4, 3, 3, 3, 3, 3, 4 ),
 ( 9.813676791237319219E-18, 0.0002724573126191667566, 0.0004086839781548390988, 0.0005449106435901880999, 0.0006811373090491526505, 0.0008459866663933667723, 0.001010840725717211197 ),
 .UNSPECIFIED. ) ;
#28024 = CARTESIAN_POINT ( 'NONE',  ( 4.956445790444002242, -37.28933980949966553, 28.75835855384135087 ) ) ;
#28025 = CARTESIAN_POINT ( 'NONE',  ( 5.959547316686252039, 12.49803383497749820, -16.28190225198605745 ) ) ;
#28026 =( BOUNDED_SURFACE ( )  B_SPLINE_SURFACE ( 3, 1, ( 
 ( #21149, #50267 ),
 ( #1706, #49964 ),
 ( #35880, #54952 ),
 ( #6702, #12084 ) ),
 .UNSPECIFIED., .F., .F., .F. ) 
 B_SPLINE_SURFACE_WITH_KNOTS ( ( 4, 4 ),
 ( 2, 2 ),
 ( 0.000000000000000000, 1.000000000000000000 ),
 ( 0.000000000000000000, 1.000000000000000000 ),
 .UNSPECIFIED. ) 
 GEOMETRIC_REPRESENTATION_ITEM ( )  RATIONAL_B_SPLINE_SURFACE ( (
 ( 1.000000000000000000, 1.000000000000000000),
 ( 0.7211978278499970862, 0.9934217856018976445),
 ( 0.7211978278499970862, 0.9934217856018976445),
 ( 1.000000000000000000, 1.000000000000000000) ) ) 
 REPRESENTATION_ITEM ( '' )  SURFACE ( )  );
#28027 = CARTESIAN_POINT ( 'NONE',  ( 0.2224561200757645130, 42.84309024201778726, -4.874377913226053849 ) ) ;
#28028 = CARTESIAN_POINT ( 'NONE',  ( 5.910764540655177868, -17.31247307865856300, 10.23618651500086330 ) ) ;
#28029 = CARTESIAN_POINT ( 'NONE',  ( 5.880360259849752858, -3.184717612778290796, 47.86623372148044808 ) ) ;
#28030 = CARTESIAN_POINT ( 'NONE',  ( 0.2285344041767070900, 40.07377575118545110, 18.45517995954402579 ) ) ;
#28032 = ORIENTED_EDGE ( 'NONE', *, *, #55439, .T. ) ;
#28031 = ADVANCED_FACE ( 'NONE', ( #5648 ), #40200, .F. ) ;
#28033 = CARTESIAN_POINT ( 'NONE',  ( 6.999999999999995559, 56.56854249492371878, 56.56854249492391062 ) ) ;
#28034 = CARTESIAN_POINT ( 'NONE',  ( 0.6000166863083106206, -2.096232480231295714, -49.06556115135418850 ) ) ;
#28036 = EDGE_CURVE ( 'NONE', #25685, #26377, #7868, .T. ) ;
#28035 = CARTESIAN_POINT ( 'NONE',  ( 0.6001305935487315502, 29.70149728382437004, -37.84751346122824600 ) ) ;
#28037 = CARTESIAN_POINT ( 'NONE',  ( -6.016489644550736315, 14.95199950534948030, 11.46752133529389717 ) ) ;
#28038 = LINE ( 'NONE', #23641, #19155 ) ;
#28039 = CARTESIAN_POINT ( 'NONE',  ( -6.016761891674564211, -17.41015286184797262, -7.207804629151495668 ) ) ;
#28040 = CARTESIAN_POINT ( 'NONE',  ( 0.5832655196449136881, -25.42549130248452371, 39.40532419611102455 ) ) ;
#28041 = CARTESIAN_POINT ( 'NONE',  ( 0.8554163680231816613, -39.19027442586699550, -25.79395013442212203 ) ) ;
#28042 = CARTESIAN_POINT ( 'NONE',  ( -2.601141883200662974, -1.938888835821362067, 14.79986951130705108 ) ) ;
#28044 = ORIENTED_EDGE ( 'NONE', *, *, #53307, .F. ) ;
#28043 = CARTESIAN_POINT ( 'NONE',  ( 2.281351352603211424, 32.98025003937418376, 34.83869092251570265 ) ) ;
#28045 = ORIENTED_EDGE ( 'NONE', *, *, #13443, .T. ) ;
#28046 = CARTESIAN_POINT ( 'NONE',  ( 0.7762783648524372859, -37.45705264446598193, 29.86325223096999082 ) ) ;
#28047 = CARTESIAN_POINT ( 'NONE',  ( 2.618530812446111078, -15.26631161698053418, 44.45971793445664133 ) ) ;
#28048 = CARTESIAN_POINT ( 'NONE',  ( 0.7762777257811896980, 17.50713318242637584, 44.59086130178256724 ) ) ;
#28049 = ORIENTED_EDGE ( 'NONE', *, *, #424, .F. ) ;
#28050 = CARTESIAN_POINT ( 'NONE',  ( 0.6016117650947689910, 10.58756707388382168, -47.95262743271228345 ) ) ;
#28051 = DIRECTION ( 'NONE',  ( -0.07906939808003035641, 0.9208896734047710142, 0.3817201064965217716 ) ) ;
#28052 = CARTESIAN_POINT ( 'NONE',  ( 0.1103310638050662151, 5.710544932888923952, -42.74468893497611788 ) ) ;
#28053 = ORIENTED_EDGE ( 'NONE', *, *, #40618, .F. ) ;
#28054 = ORIENTED_EDGE ( 'NONE', *, *, #50413, .F. ) ;
#28056 = EDGE_CURVE ( 'NONE', #1247, #26085, #57684, .T. ) ;
#28055 = B_SPLINE_CURVE_WITH_KNOTS ( 'NONE', 3,
 ( #1364, #1070, #20206, #11412 ),
 .UNSPECIFIED., .F., .F.,
 ( 4, 4 ),
 ( 6.254634441385501517E-18, 0.004566006591234644633 ),
 .UNSPECIFIED. ) ;
#28057 = CARTESIAN_POINT ( 'NONE',  ( 0.9785694773339237429, 25.03819957080264302, -33.60690357601148293 ) ) ;
#28058 = CARTESIAN_POINT ( 'NONE',  ( 4.060580049360325461, -39.81183563956297178, 18.61411930142365989 ) ) ;
#28059 = CARTESIAN_POINT ( 'NONE',  ( 5.272379999999998290, 0.000000000000000000, 0.000000000000000000 ) ) ;
#28060 = CARTESIAN_POINT ( 'NONE',  ( 0.5817217712918331118, 17.27887506707169152, -43.59673646530094970 ) ) ;
#28061 = DIRECTION ( 'NONE',  ( 0.000000000000000000, 0.000000000000000000, 1.000000000000000000 ) ) ;
#28062 = CARTESIAN_POINT ( 'NONE',  ( 4.999999999999997335, 9.184547653667864935E-16, -9.629649721936170507E-32 ) ) ;
#28063 = B_SPLINE_CURVE_WITH_KNOTS ( 'NONE', 3,
 ( #2984, #22107, #41235, #52447 ),
 .UNSPECIFIED., .F., .F.,
 ( 4, 4 ),
 ( 4.336808689942017736E-19, 0.004041751736740994277 ),
 .UNSPECIFIED. ) ;
#28064 = CARTESIAN_POINT ( 'NONE',  ( 0.9730545539215883499, 26.52009130076770305, 33.73144377768567637 ) ) ;
#28065 = ORIENTED_EDGE ( 'NONE', *, *, #6607, .T. ) ;
#28066 = AXIS2_PLACEMENT_3D ( 'NONE', #45628, #40950, #45027 ) ;
#28067 = B_SPLINE_CURVE_WITH_KNOTS ( 'NONE', 3,
 ( #53171, #34099, #10276, #29369, #28440, #28759 ),
 .UNSPECIFIED., .F., .F.,
 ( 4, 2, 4 ),
 ( 7.023086426956682172E-18, 0.0002445244328975374024, 0.0004890488657950677574 ),
 .UNSPECIFIED. ) ;
#28068 = CARTESIAN_POINT ( 'NONE',  ( 5.880360259849752858, 21.25991003419953174, -43.00389496650593912 ) ) ;
#28069 = ORIENTED_EDGE ( 'NONE', *, *, #2239, .F. ) ;
#28070 = CARTESIAN_POINT ( 'NONE',  ( 0.8751705887134423323, -47.55935879196466232, -7.160166390004136794 ) ) ;
#28071 = CARTESIAN_POINT ( 'NONE',  ( 5.896782393890504181, -9.671431223051156323, 17.63489452692596515 ) ) ;
#28072 = CARTESIAN_POINT ( 'NONE',  ( 5.910764540655177868, -13.97071922697925750, -14.46790388238998482 ) ) ;
#28073 = CARTESIAN_POINT ( 'NONE',  ( 0.5987334363312694085, 23.24905850218390313, -43.25556825697827890 ) ) ;
#28074 = ORIENTED_EDGE ( 'NONE', *, *, #40545, .F. ) ;
#28075 = ORIENTED_EDGE ( 'NONE', *, *, #26689, .T. ) ;
#28076 = CARTESIAN_POINT ( 'NONE',  ( 0.5806925824938499181, 46.54710689580866756, -5.708695295225145294 ) ) ;
#28077 = CARTESIAN_POINT ( 'NONE',  ( 0.8753041380234465318, 37.96023374381077531, -31.14737520222577771 ) ) ;
#28078 = CARTESIAN_POINT ( 'NONE',  ( 4.958415959904818315, -4.043245302073017022, 45.24219403665016159 ) ) ;
#28079 = CIRCLE ( 'NONE', #58061, 15.50000000000000000 ) ;
#28080 = ORIENTED_EDGE ( 'NONE', *, *, #26303, .T. ) ;
#28081 = CARTESIAN_POINT ( 'NONE',  ( 4.975610109902397937, -23.13264022976521161, -43.09675583078175265 ) ) ;
#28082 = EDGE_CURVE ( 'NONE', #14994, #12923, #40166, .T. ) ;
#28083 = ORIENTED_EDGE ( 'NONE', *, *, #51684, .F. ) ;
#28084 = CARTESIAN_POINT ( 'NONE',  ( 0.7413678028165009426, 43.45184631738121084, 7.511534023149208039 ) ) ;
#28085 = CARTESIAN_POINT ( 'NONE',  ( 0.5806925824938502512, 28.25565086187734920, 37.42780459384778879 ) ) ;
#28086 = CARTESIAN_POINT ( 'NONE',  ( 0.1157991065609916131, 37.02429157203778942, -24.00300396047191143 ) ) ;
#28087 = VERTEX_POINT ( 'NONE', #15719 ) ;
#28088 = CARTESIAN_POINT ( 'NONE',  ( 4.962356264823608143, -19.84272732133934269, -37.11471096901227185 ) ) ;
#28089 = EDGE_CURVE ( 'NONE', #13993, #38729, #27867, .T. ) ;
#28090 = CARTESIAN_POINT ( 'NONE',  ( 0.6000166863083106206, 11.43688157230965885, -47.76003791465640091 ) ) ;
#28091 = DIRECTION ( 'NONE',  ( -1.000000000000000000, 0.000000000000000000, 0.000000000000000000 ) ) ;
#28092 = CARTESIAN_POINT ( 'NONE',  ( 0.7246131072078539903, 47.79072675905340617, -5.464103862701012559 ) ) ;
#28093 =( BOUNDED_SURFACE ( )  B_SPLINE_SURFACE ( 3, 1, ( 
 ( #7918, #32051 ),
 ( #45854, #12332 ),
 ( #61137, #41153 ),
 ( #8846, #18258 ) ),
 .UNSPECIFIED., .F., .F., .F. ) 
 B_SPLINE_SURFACE_WITH_KNOTS ( ( 4, 4 ),
 ( 2, 2 ),
 ( 0.000000000000000000, 1.000000000000000000 ),
 ( 0.000000000000000000, 1.000000000000000000 ),
 .UNSPECIFIED. ) 
 GEOMETRIC_REPRESENTATION_ITEM ( )  RATIONAL_B_SPLINE_SURFACE ( (
 ( 1.000000000000000000, 1.000000000000000000),
 ( 0.9953390228620291325, 0.8624445117761032620),
 ( 0.9953390228620291325, 0.8624445117761032620),
 ( 1.000000000000000000, 1.000000000000000000) ) ) 
 REPRESENTATION_ITEM ( '' )  SURFACE ( )  );
#28094 = CARTESIAN_POINT ( 'NONE',  ( 0.1157506346131639274, 33.53794432182292695, -28.67310500223404546 ) ) ;
#28095 = CARTESIAN_POINT ( 'NONE',  ( 0.9762797500689124330, -40.96497924994823592, 8.842808390834631993 ) ) ;
#28096 = CARTESIAN_POINT ( 'NONE',  ( 0.1104177457020373149, 26.24862037251732616, -34.21590786699014330 ) ) ;
#28097 = DIRECTION ( 'NONE',  ( -1.000000000000000000, -0.000000000000000000, -0.000000000000000000 ) ) ;
#28098 = ORIENTED_EDGE ( 'NONE', *, *, #23663, .T. ) ;
#28099 = LINE ( 'NONE', #23100, #27669 ) ;
#28100 = ORIENTED_EDGE ( 'NONE', *, *, #49569, .T. ) ;
#28101 = CARTESIAN_POINT ( 'NONE',  ( -2.708315649062910779, -11.44805714186566270, -9.116606751444287227 ) ) ;
#28102 = CYLINDRICAL_SURFACE ( 'NONE', #36371, 5.000000000000000000 ) ;
#28104 = EDGE_CURVE ( 'NONE', #25364, #55454, #12919, .T. ) ;
#28103 = CARTESIAN_POINT ( 'NONE',  ( 4.956653778116975495, 20.77844580450561551, 43.37017594958062006 ) ) ;
#28105 = FACE_OUTER_BOUND ( 'NONE', #6924, .T. ) ;
#28106 = B_SPLINE_CURVE_WITH_KNOTS ( 'NONE', 3,
 ( #2721, #32175, #45667, #31239 ),
 .UNSPECIFIED., .F., .F.,
 ( 4, 4 ),
 ( 0.000000000000000000, 0.005004741218457420607 ),
 .UNSPECIFIED. ) ;
#28107 = CARTESIAN_POINT ( 'NONE',  ( -6.072942160501519915, 5.492864488351274943, 18.45623477314995853 ) ) ;
#28108 = CARTESIAN_POINT ( 'NONE',  ( 0.6254087463353913412, -41.31312313681428350, 24.64672211239892974 ) ) ;
#28109 = CARTESIAN_POINT ( 'NONE',  ( 51.67479428703781963, 15.31607246706614056, 2.381689993923809201 ) ) ;
#28110 = DIRECTION ( 'NONE',  ( -1.000000000000000000, 1.691355389077386917E-17, 5.551115123125782702E-17 ) ) ;
#28111 = CARTESIAN_POINT ( 'NONE',  ( 0.5817216825391109403, 11.31383544828560517, 45.51079080456168668 ) ) ;
#28112 = CARTESIAN_POINT ( 'NONE',  ( 4.322998006666165516, -46.85697641700715366, 10.36018990813231788 ) ) ;
#28113 = CARTESIAN_POINT ( 'NONE',  ( 0.5797568665920710407, 32.14649144340224041, -34.14422932914341402 ) ) ;
#28114 = CARTESIAN_POINT ( 'NONE',  ( 0.1097557419366048670, -5.407604117550024903, 42.78407272074148437 ) ) ;
#28115 = VERTEX_POINT ( 'NONE', #45168 ) ;
#28116 = CARTESIAN_POINT ( 'NONE',  ( 5.860006189529246790, 21.34829429597527550, -43.25137511473229068 ) ) ;
#28117 = CARTESIAN_POINT ( 'NONE',  ( 0.5997462898726536595, -48.76843890605300658, -5.761162800241320880 ) ) ;
#28118 = DIRECTION ( 'NONE',  ( 0.000000000000000000, -0.000000000000000000, 1.000000000000000000 ) ) ;
#28119 = CARTESIAN_POINT ( 'NONE',  ( 2.282816707992311400, -26.37306023955149570, -38.87105169671840343 ) ) ;
#28120 = CARTESIAN_POINT ( 'NONE',  ( 2.526464513654347321, -25.19161096467252747, 34.82216969498457360 ) ) ;
#28121 = VECTOR ( 'NONE', #22882, 1000.000000000000000 ) ;
#28122 = VERTEX_POINT ( 'NONE', #35447 ) ;
#28123 = DIRECTION ( 'NONE',  ( -0.000000000000000000, -0.000000000000000000, 1.000000000000000000 ) ) ;
#28124 = CARTESIAN_POINT ( 'NONE',  ( 0.9762797500689124330, 41.90547441298052433, 0.5059638413352746111 ) ) ;
#28125 = CARTESIAN_POINT ( 'NONE',  ( -20.07373396512872787, -8.000008915846105850, 0.1379583681271069062 ) ) ;
#28126 = EDGE_LOOP ( 'NONE', ( #3162, #13095 ) ) ;
#28127 = CARTESIAN_POINT ( 'NONE',  ( -4.554074483026735898, -10.53772250678246358, 5.913403440073379425E-14 ) ) ;
#28128 = B_SPLINE_CURVE_WITH_KNOTS ( 'NONE', 3,
 ( #58353, #52750, #38080, #28639 ),
 .UNSPECIFIED., .F., .F.,
 ( 4, 4 ),
 ( 0.000000000000000000, 0.004048833967417087357 ),
 .UNSPECIFIED. ) ;
#28129 = EDGE_CURVE ( 'NONE', #41690, #29140, #12143, .T. ) ;
#28130 = CARTESIAN_POINT ( 'NONE',  ( 4.963659409799330291, -29.14784479683135743, 33.96111158240236705 ) ) ;
#28131 = VERTEX_POINT ( 'NONE', #39534 ) ;
#28132 = ADVANCED_FACE ( 'NONE', ( #49518 ), #46890, .F. ) ;
#28133 = CARTESIAN_POINT ( 'NONE',  ( 4.060580049360325461, -25.55452198193345481, 35.75519683394414017 ) ) ;
#28134 = ORIENTED_EDGE ( 'NONE', *, *, #12781, .T. ) ;
#28135 = CARTESIAN_POINT ( 'NONE',  ( 3.678748215320120973, 36.06704015422782561, -33.13278480316439101 ) ) ;
#28136 = LINE ( 'NONE', #37563, #55546 ) ;
#28137 = VERTEX_POINT ( 'NONE', #26958 ) ;
#28138 = FACE_BOUND ( 'NONE', #28275, .T. ) ;
#28139 = CARTESIAN_POINT ( 'NONE',  ( -6.063463321072278589, -14.65282214633749192, -12.49460906260262050 ) ) ;
#28140 = CARTESIAN_POINT ( 'NONE',  ( 0.5830082357119560355, -7.530675664250292556, -46.28737364528480924 ) ) ;
#28141 = CARTESIAN_POINT ( 'NONE',  ( 0.7948884756798489937, -43.19977691860155034, 23.33405062956740750 ) ) ;
#28142 = VERTEX_POINT ( 'NONE', #13180 ) ;
#28143 = DIRECTION ( 'NONE',  ( -0.000000000000000000, -0.000000000000000000, 1.000000000000000000 ) ) ;
#28144 = ORIENTED_EDGE ( 'NONE', *, *, #59411, .F. ) ;
#28145 = CARTESIAN_POINT ( 'NONE',  ( 2.528100132419517365, 41.96176039463138352, -1.210141816325795316 ) ) ;
#28146 = ORIENTED_EDGE ( 'NONE', *, *, #58060, .F. ) ;
#28147 = EDGE_CURVE ( 'NONE', #9403, #20133, #42114, .T. ) ;
#28148 = EDGE_LOOP ( 'NONE', ( #34235, #19632 ) ) ;
#28149 = CARTESIAN_POINT ( 'NONE',  ( 1.154321713695928064, -42.43366804783610746, -6.418927679456075452 ) ) ;
#28150 = CARTESIAN_POINT ( 'NONE',  ( 0.6023142530420679819, -33.83147280953710379, 34.20176999054650224 ) ) ;
#28151 = CARTESIAN_POINT ( 'NONE',  ( 0.7056555295713290432, 46.47980662829232301, 11.58338207350417015 ) ) ;
#28152 = CARTESIAN_POINT ( 'NONE',  ( 4.962356264823608143, 41.32726869310149453, -7.955655864260332777 ) ) ;
#28153 = VERTEX_POINT ( 'NONE', #2514 ) ;
#28154 = CARTESIAN_POINT ( 'NONE',  ( 0.9756354156337461170, 0.1303083999672954851, -42.90827993934335893 ) ) ;
#28155 = EDGE_CURVE ( 'NONE', #17050, #39295, #27883, .T. ) ;
#28156 = LINE ( 'NONE', #47587, #1615 ) ;
#28157 = CARTESIAN_POINT ( 'NONE',  ( -6.078075953587585900, -18.89992925442663818, 3.686169885505006238 ) ) ;
#28158 = ORIENTED_EDGE ( 'NONE', *, *, #32973, .F. ) ;
#28159 = VECTOR ( 'NONE', #13089, 1000.000000000000000 ) ;
#28160 = EDGE_CURVE ( 'NONE', #43495, #31225, #18120, .T. ) ;
#28161 = ORIENTED_EDGE ( 'NONE', *, *, #9848, .T. ) ;
#28162 = CONICAL_SURFACE ( 'NONE', #52164, 4.000000000000000000, 1.047197551196595855 ) ;
#28163 = CARTESIAN_POINT ( 'NONE',  ( 4.956445790444038657, 44.30493387627053181, -15.95653108789415953 ) ) ;
#28164 = CARTESIAN_POINT ( 'NONE',  ( -6.063463321072276813, -6.665223333113386772, -18.06641221712797218 ) ) ;
#28165 = DIRECTION ( 'NONE',  ( 0.000000000000000000, 0.000000000000000000, -1.000000000000000000 ) ) ;
#28166 = CARTESIAN_POINT ( 'NONE',  ( 4.967162193818130511, -32.68434214048189546, 28.07411493385282242 ) ) ;
#28167 = CARTESIAN_POINT ( 'NONE',  ( 0.5807400328401637335, -29.58941477093042494, 37.66660715020854866 ) ) ;
#28168 =( BOUNDED_SURFACE ( )  B_SPLINE_SURFACE ( 3, 1, ( 
 ( #50465, #3451 ),
 ( #50766, #31676 ),
 ( #27588, #55154 ),
 ( #26661, #21975 ) ),
 .UNSPECIFIED., .F., .F., .F. ) 
 B_SPLINE_SURFACE_WITH_KNOTS ( ( 4, 4 ),
 ( 2, 2 ),
 ( 0.000000000000000000, 1.000000000000000000 ),
 ( 0.000000000000000000, 1.000000000000000000 ),
 .UNSPECIFIED. ) 
 GEOMETRIC_REPRESENTATION_ITEM ( )  RATIONAL_B_SPLINE_SURFACE ( (
 ( 1.000000000000000000, 1.000000000000000000),
 ( 0.7269869731126821222, 0.9931720237060910339),
 ( 0.7269869731126821222, 0.9931720237060910339),
 ( 1.000000000000000000, 1.000000000000000000) ) ) 
 REPRESENTATION_ITEM ( '' )  SURFACE ( )  );
#28169 = ORIENTED_EDGE ( 'NONE', *, *, #36719, .F. ) ;
#28170 = DIRECTION ( 'NONE',  ( 0.000000000000000000, 0.000000000000000000, -1.000000000000000000 ) ) ;
#28172 = EDGE_CURVE ( 'NONE', #8614, #35106, #43909, .T. ) ;
#28171 = CARTESIAN_POINT ( 'NONE',  ( 0.9787464366903576574, -41.10375767077415077, 8.174050295461709581 ) ) ;
#28173 = CARTESIAN_POINT ( 'NONE',  ( 0.3676999524040366896, -38.83470403830472151, -20.92406140260821346 ) ) ;
#28174 = CARTESIAN_POINT ( 'NONE',  ( 4.967162193818130511, 43.02067033766019932, -2.375726030842729486 ) ) ;
#28175 = SHAPE_REPRESENTATION_RELATIONSHIP ( 'NONE' , 'NONE' ,  #40484, #59429 ) ;
#28176 = CARTESIAN_POINT ( 'NONE',  ( 0.6031356755825967308, 1.709377914627507658E-05, 48.10744332413644031 ) ) ;
#28177 = VERTEX_POINT ( 'NONE', #41091 ) ;
#28178 = CARTESIAN_POINT ( 'NONE',  ( 0.1310142868023707330, 34.59629828998416912, -25.74368468368899343 ) ) ;
#28179 = CARTESIAN_POINT ( 'NONE',  ( 0.3622758884714730732, 4.808133778521878732, -42.84426538328727219 ) ) ;
#28180 = CARTESIAN_POINT ( 'NONE',  ( 5.974727161628367256, -20.35137732084674056, -2.663664384318710887 ) ) ;
#28181 = B_SPLINE_CURVE_WITH_KNOTS ( 'NONE', 3,
 ( #6249, #11302, #49200, #31025, #8351, #30088, #3645, #46597, #49820, #54813, #26319, #36903, #21626, #54492, #16624, #6881, #51266, #32183, #58895, #25391, #21012, #49507, #41910, #60977, #34814, #39842, #44538, #40765, #59830, #20702 ),
 .UNSPECIFIED., .F., .F.,
 ( 4, 2, 2, 2, 2, 2, 2, 2, 2, 2, 2, 2, 2, 2, 4 ),
 ( 0.006577215611807306177, 0.007399161751817349281, 0.007810134821822366062, 0.008221107891827382844, 0.008632080961832398758, 0.009043054031837416407, 0.009454027101842432321, 0.009865000171847449970, 0.01027597324185246588, 0.01068694631185748180, 0.01109791938186249771, 0.01150889245186751536, 0.01233083859187754892, 0.01274181166188256484, 0.01315278473188758249 ),
 .UNSPECIFIED. ) ;
#28182 = CARTESIAN_POINT ( 'NONE',  ( -6.078726893082806448, -8.909671472910916989, 17.07078778245215034 ) ) ;
#28183 = CARTESIAN_POINT ( 'NONE',  ( -6.078457390727109555, 0.6215653986401029618, 19.24599094597940052 ) ) ;
#28184 = CARTESIAN_POINT ( 'NONE',  ( 4.975801465491694664, -35.64402118370934147, -32.01766832630300286 ) ) ;
#28185 = CARTESIAN_POINT ( 'NONE',  ( 4.956653778116990594, -35.79382859084093127, -32.11725092155079864 ) ) ;
#28186 = CARTESIAN_POINT ( 'NONE',  ( 4.691466044806102076, 37.25818859570306785, -24.49380602310773725 ) ) ;
#28187 = ORIENTED_EDGE ( 'NONE', *, *, #18964, .F. ) ;
#28188 = EDGE_CURVE ( 'NONE', #51030, #39564, #12566, .T. ) ;
#28189 = DIRECTION ( 'NONE',  ( -1.000000000000000000, -0.000000000000000000, -0.000000000000000000 ) ) ;
#28190 = CARTESIAN_POINT ( 'NONE',  ( 3.894904216938897878, 23.29122489240411653, -37.27791806804204811 ) ) ;
#28191 = CARTESIAN_POINT ( 'NONE',  ( -6.016104459813374383, -4.871830707672929250, -18.20253432612971523 ) ) ;
#28192 = DIRECTION ( 'NONE',  ( 1.000000000000000000, 0.000000000000000000, 0.000000000000000000 ) ) ;
#28193 = VERTEX_POINT ( 'NONE', #40462 ) ;
#28194 = EDGE_CURVE ( 'NONE', #25747, #1919, #9847, .T. ) ;
#28195 = CARTESIAN_POINT ( 'NONE',  ( 5.895881250540457863, 19.71075194021744181, -4.001742065590352837 ) ) ;
#28196 = FACE_OUTER_BOUND ( 'NONE', #44820, .T. ) ;
#28197 = B_SPLINE_CURVE_WITH_KNOTS ( 'NONE', 3,
 ( #43838, #39129, #40068, #11528 ),
 .UNSPECIFIED., .F., .F.,
 ( 4, 4 ),
 ( 0.000000000000000000, 0.005014147105413707325 ),
 .UNSPECIFIED. ) ;
#28198 = AXIS2_PLACEMENT_3D ( 'NONE', #31742, #2907, #45248 ) ;
#28199 = EDGE_CURVE ( 'NONE', #30745, #37740, #33874, .T. ) ;
#28200 = B_SPLINE_CURVE_WITH_KNOTS ( 'NONE', 3,
 ( #10110, #61470, #43034, #42120 ),
 .UNSPECIFIED., .F., .F.,
 ( 4, 4 ),
 ( 0.000000000000000000, 0.005013413432710135502 ),
 .UNSPECIFIED. ) ;
#28201 = CIRCLE ( 'NONE', #24221, 48.91267123290010943 ) ;
#28202 = VERTEX_POINT ( 'NONE', #27568 ) ;
#28203 = CARTESIAN_POINT ( 'NONE',  ( 0.1139756605157203062, 3.841029851089543090, -43.95681641541004581 ) ) ;
#28204 = LINE ( 'NONE', #56391, #33547 ) ;
#28205 = EDGE_CURVE ( 'NONE', #24773, #4220, #48728, .T. ) ;
#28206 = CARTESIAN_POINT ( 'NONE',  ( -2.700785417809989042, -13.56184546075576769, -3.000000000000003997 ) ) ;
#28207 = ORIENTED_EDGE ( 'NONE', *, *, #34542, .T. ) ;
#28208 = CARTESIAN_POINT ( 'NONE',  ( 0.7242003506639982380, -31.25070601918658753, -37.87354020194578652 ) ) ;
#28209 = EDGE_LOOP ( 'NONE', ( #4950, #24000, #14144, #40488 ) ) ;
#28210 = VERTEX_POINT ( 'NONE', #40781 ) ;
#28211 = CARTESIAN_POINT ( 'NONE',  ( 0.5809828226811626362, -12.92184523170236510, 46.11980934799335330 ) ) ;
#28212 = CARTESIAN_POINT ( 'NONE',  ( -6.001507490154110336, 17.41542759839264320, 7.196845540359233517 ) ) ;
#28213 = ORIENTED_EDGE ( 'NONE', *, *, #55857, .F. ) ;
#28214 = CARTESIAN_POINT ( 'NONE',  ( 4.967162193818130511, -3.259922920617460029, -42.96271701169388280 ) ) ;
#28215 = ORIENTED_EDGE ( 'NONE', *, *, #46260, .T. ) ;
#28216 = CARTESIAN_POINT ( 'NONE',  ( 0.1119899015040012463, -43.83035649366780717, 5.085386694293604570 ) ) ;
#28217 = FACE_OUTER_BOUND ( 'NONE', #5933, .T. ) ;
#28218 = FACE_OUTER_BOUND ( 'NONE', #1083, .T. ) ;
#28219 = ADVANCED_FACE ( 'NONE', ( #26333 ), #50576, .F. ) ;
#28220 = VERTEX_POINT ( 'NONE', #31974 ) ;
#28221 = CARTESIAN_POINT ( 'NONE',  ( 5.895596859100789899, 20.06821053248684805, -1.339816866691640129 ) ) ;
#28222 = CARTESIAN_POINT ( 'NONE',  ( 5.917102823773431552, 19.71063251686273432, -3.997584750438137213 ) ) ;
#28223 = CARTESIAN_POINT ( 'NONE',  ( 0.8551540677456715978, 19.17641535420853671, 43.91216198251545677 ) ) ;
#28224 = LINE ( 'NONE', #23842, #21677 ) ;
#28225 = EDGE_LOOP ( 'NONE', ( #23968, #46330, #59085, #31097 ) ) ;
#28226 = ADVANCED_FACE ( 'NONE', ( #31656 ), #29361, .F. ) ;
#28227 = CARTESIAN_POINT ( 'NONE',  ( 5.960721111146673579, -5.306302591836445259, -19.82781442290496443 ) ) ;
#28228 = CARTESIAN_POINT ( 'NONE',  ( 0.1158816050234198619, -31.70051762657859840, -30.69233167278335728 ) ) ;
#28229 = ORIENTED_EDGE ( 'NONE', *, *, #50482, .F. ) ;
#28230 = CARTESIAN_POINT ( 'NONE',  ( 4.553261556744875094, -43.82122302957815663, -3.039733214544628748 ) ) ;
#28231 = ADVANCED_FACE ( 'NONE', ( #54827 ), #14571, .F. ) ;
#28232 = ORIENTED_EDGE ( 'NONE', *, *, #15088, .F. ) ;
#28233 = CARTESIAN_POINT ( 'NONE',  ( 1.227938101723748288, 11.92353943228006585, -41.23019537246697297 ) ) ;
#28234 = CARTESIAN_POINT ( 'NONE',  ( 0.6021447746440204973, 46.52271636273428612, -15.72189560202788527 ) ) ;
#28235 = VERTEX_POINT ( 'NONE', #42006 ) ;
#28236 = CARTESIAN_POINT ( 'NONE',  ( 0.9783242366443540838, -34.39878881041870073, -23.93862607968005207 ) ) ;
#28237 = CARTESIAN_POINT ( 'NONE',  ( 0.5980271706414734822, 33.53334604750687475, 35.88264128655829666 ) ) ;
#28238 = DIRECTION ( 'NONE',  ( 1.000000000000000000, 0.000000000000000000, 0.000000000000000000 ) ) ;
#28239 = FACE_BOUND ( 'NONE', #18911, .T. ) ;
#28240 = ORIENTED_EDGE ( 'NONE', *, *, #44142, .F. ) ;
#28241 = DIRECTION ( 'NONE',  ( 0.09722883295013595717, 0.1030875952483898822, -0.9899088350697040628 ) ) ;
#28242 = CARTESIAN_POINT ( 'NONE',  ( 0.5807400328401637335, 38.33001520688950592, 28.72484455891654065 ) ) ;
#28243 = CARTESIAN_POINT ( 'NONE',  ( -6.015611763856276717, -17.41126425312542736, 7.205255340944552778 ) ) ;
#28245 = ADVANCED_FACE ( 'NONE', ( #18182 ), #52957, .F. ) ;
#28244 = CARTESIAN_POINT ( 'NONE',  ( 0.5807400328401637335, 24.41979442053169436, 41.20655774452978193 ) ) ;
#28246 = CIRCLE ( 'NONE', #33280, 47.91270532121795611 ) ;
#28247 = FACE_OUTER_BOUND ( 'NONE', #60320, .T. ) ;
#28248 = CARTESIAN_POINT ( 'NONE',  ( 5.958863334805807099, -16.28483817244747556, 12.49425770716459994 ) ) ;
#28249 = EDGE_CURVE ( 'NONE', #56267, #37980, #56265, .T. ) ;
#28250 = B_SPLINE_CURVE_WITH_KNOTS ( 'NONE', 3,
 ( #61077, #51991, #22887, #9083, #52604, #28810 ),
 .UNSPECIFIED., .F., .F.,
 ( 4, 2, 4 ),
 ( 0.002336974151641576809, 0.003500975885716453226, 0.004664977619791330077 ),
 .UNSPECIFIED. ) ;
#28251 = FACE_OUTER_BOUND ( 'NONE', #22041, .T. ) ;
#28252 = PLANE ( 'NONE',  #38892 ) ;
#28253 = CARTESIAN_POINT ( 'NONE',  ( 0.9787284016396609054, -12.23755578274794509, 40.08214349798376475 ) ) ;
#28254 = DIRECTION ( 'NONE',  ( -0.1736481776669312471, 0.9848077530122077983, -5.551115123125779621E-17 ) ) ;
#28255 = CARTESIAN_POINT ( 'NONE',  ( 0.9756354156337452288, 30.43287766742290046, -30.24859376089789009 ) ) ;
#28256 = CARTESIAN_POINT ( 'NONE',  ( 0.1100247026804066219, -21.70899701554550276, 37.26174279786175703 ) ) ;
#28257 = CARTESIAN_POINT ( 'NONE',  ( 1.227938101723748288, -34.55893248994524214, 25.45152231597044690 ) ) ;
#28258 = LINE ( 'NONE', #33292, #15674 ) ;
#28259 = CARTESIAN_POINT ( 'NONE',  ( 0.2279481005628781476, -31.16006227558741770, -31.23385992884048079 ) ) ;
#28260 =( BOUNDED_SURFACE ( )  B_SPLINE_SURFACE ( 3, 1, ( 
 ( #31587, #50674 ),
 ( #40097, #49450 ),
 ( #7763, #17187 ),
 ( #26888, #58836 ) ),
 .UNSPECIFIED., .F., .F., .F. ) 
 B_SPLINE_SURFACE_WITH_KNOTS ( ( 4, 4 ),
 ( 2, 2 ),
 ( 0.000000000000000000, 1.000000000000000000 ),
 ( 0.000000000000000000, 1.000000000000000000 ),
 .UNSPECIFIED. ) 
 GEOMETRIC_REPRESENTATION_ITEM ( )  RATIONAL_B_SPLINE_SURFACE ( (
 ( 1.000000000000000000, 1.000000000000000000),
 ( 0.7223157951917480446, 0.9931996967497186413),
 ( 0.7223157951917480446, 0.9931996967497186413),
 ( 1.000000000000000000, 1.000000000000000000) ) ) 
 REPRESENTATION_ITEM ( '' )  SURFACE ( )  );
#28261 = CARTESIAN_POINT ( 'NONE',  ( 0.9754642270333709897, -37.07163437210430601, -21.60621846558674974 ) ) ;
#28262 = CARTESIAN_POINT ( 'NONE',  ( 0.5832655196449135770, 45.28935891855852702, -12.17001034179147645 ) ) ;
#28263 = CARTESIAN_POINT ( 'NONE',  ( 0.5997462898726536595, -39.66574928371219499, -28.95133786038212875 ) ) ;
#28265 = ORIENTED_EDGE ( 'NONE', *, *, #27880, .F. ) ;
#28264 = CARTESIAN_POINT ( 'NONE',  ( 0.5806925824938502512, -8.338382001837375768, -46.14860504863607105 ) ) ;
#28266 = CARTESIAN_POINT ( 'NONE',  ( 0.6028777368367060907, -39.40737854605714574, 29.30184883994229850 ) ) ;
#28267 = CARTESIAN_POINT ( 'NONE',  ( 0.5839879327111934249, 24.02664985973703793, 41.43370681949784995 ) ) ;
#28268 = ORIENTED_EDGE ( 'NONE', *, *, #35890, .F. ) ;
#28269 = EDGE_CURVE ( 'NONE', #21652, #32480, #21895, .T. ) ;
#28270 = CARTESIAN_POINT ( 'NONE',  ( 3.221118495291109163, -30.25413894314359453, 31.92880355526516567 ) ) ;
#28271 = CARTESIAN_POINT ( 'NONE',  ( 5.960721111146673579, -16.28787783074235662, 12.49016043756443750 ) ) ;
#28272 = EDGE_CURVE ( 'NONE', #20804, #44257, #56987, .T. ) ;
#28273 =( BOUNDED_SURFACE ( )  B_SPLINE_SURFACE ( 3, 1, ( 
 ( #35535, #40555 ),
 ( #21110, #60538 ),
 ( #1985, #7932 ),
 ( #11727, #45255 ) ),
 .UNSPECIFIED., .F., .F., .F. ) 
 B_SPLINE_SURFACE_WITH_KNOTS ( ( 4, 4 ),
 ( 2, 2 ),
 ( 0.000000000000000000, 1.000000000000000000 ),
 ( 0.000000000000000000, 1.000000000000000000 ),
 .UNSPECIFIED. ) 
 GEOMETRIC_REPRESENTATION_ITEM ( )  RATIONAL_B_SPLINE_SURFACE ( (
 ( 1.000000000000000000, 1.000000000000000000),
 ( 0.9953040768229013402, 0.8617119497784988535),
 ( 0.9953040768229013402, 0.8617119497784988535),
 ( 1.000000000000000000, 1.000000000000000000) ) ) 
 REPRESENTATION_ITEM ( '' )  SURFACE ( )  );
#28274 = EDGE_LOOP ( 'NONE', ( #5267, #5020, #38961, #26771 ) ) ;
#28275 = EDGE_LOOP ( 'NONE', ( #55890, #27831 ) ) ;
#28276 = CARTESIAN_POINT ( 'NONE',  ( 0.6009453534118439633, -37.89911869481712614, -29.63106322864171105 ) ) ;
#28277 = ADVANCED_FACE ( 'NONE', ( #4043 ), #41836, .F. ) ;
#28278 = ORIENTED_EDGE ( 'NONE', *, *, #35199, .T. ) ;
#28279 = EDGE_CURVE ( 'NONE', #45339, #17051, #7664, .T. ) ;
#28280 = CARTESIAN_POINT ( 'NONE',  ( 0.5807400328401574052, -18.83234461715150587, -44.04145271122585115 ) ) ;
#28281 = CARTESIAN_POINT ( 'NONE',  ( 4.691466044806103852, -8.371234562542175794, 43.79545162262294156 ) ) ;
#28282 = EDGE_CURVE ( 'NONE', #1725, #14527, #19121, .T. ) ;
#28283 = ORIENTED_EDGE ( 'NONE', *, *, #37365, .T. ) ;
#28284 = VERTEX_POINT ( 'NONE', #27881 ) ;
#28285 = DIRECTION ( 'NONE',  ( 1.000000000000000000, 0.000000000000000000, 0.000000000000000000 ) ) ;
#28286 = VERTEX_POINT ( 'NONE', #10015 ) ;
#28287 = CARTESIAN_POINT ( 'NONE',  ( 5.896782393890504181, -4.668739246792056541, -19.56345983519980081 ) ) ;
#28288 = DIRECTION ( 'NONE',  ( 1.000000000000000000, 0.000000000000000000, 0.000000000000000000 ) ) ;
#28289 = CIRCLE ( 'NONE', #3274, 4.000000000000000888 ) ;
#28290 = CARTESIAN_POINT ( 'NONE',  ( 0.1098349054025746369, -30.34240357440814861, -30.64407294528938053 ) ) ;
#28291 = ORIENTED_EDGE ( 'NONE', *, *, #17560, .T. ) ;
#28292 = CARTESIAN_POINT ( 'NONE',  ( 0.1368894036331280151, -7.670678564336283145, -43.45137530948780835 ) ) ;
#28293 = EDGE_CURVE ( 'NONE', #2081, #26311, #37609, .T. ) ;
#28294 = CARTESIAN_POINT ( 'NONE',  ( 0.9756354156337452288, -33.96210048825357575, -26.22428641656288306 ) ) ;
#28295 = ORIENTED_EDGE ( 'NONE', *, *, #12127, .T. ) ;
#28296 = ORIENTED_EDGE ( 'NONE', *, *, #46186, .T. ) ;
#28297 = CARTESIAN_POINT ( 'NONE',  ( 0.5850706913938533704, -44.31965802246118358, 18.16120156791865270 ) ) ;
#28298 = ORIENTED_EDGE ( 'NONE', *, *, #2108, .T. ) ;
#28299 = CARTESIAN_POINT ( 'NONE',  ( 3.221118495291108719, 34.68635812792123119, 27.04843765327941441 ) ) ;
#28300 = CARTESIAN_POINT ( 'NONE',  ( 0.6000166863083090663, 37.05402083933936552, 32.23077754796270966 ) ) ;
#28301 = DIRECTION ( 'NONE',  ( -1.000000000000000000, -0.000000000000000000, -0.000000000000000000 ) ) ;
#28302 = DIRECTION ( 'NONE',  ( 0.000000000000000000, 0.000000000000000000, 1.000000000000000000 ) ) ;
#28303 = CARTESIAN_POINT ( 'NONE',  ( 1.827119703190780653, 29.55676396270184725, -31.30004882613811290 ) ) ;
#28304 = B_SPLINE_CURVE_WITH_KNOTS ( 'NONE', 3,
 ( #50145, #36377, #55442, #1577 ),
 .UNSPECIFIED., .F., .F.,
 ( 4, 4 ),
 ( 4.336808689942017736E-19, 0.004041751736740997747 ),
 .UNSPECIFIED. ) ;
#28305 = EDGE_LOOP ( 'NONE', ( #9423, #59525, #54610, #28835 ) ) ;
#28306 = CARTESIAN_POINT ( 'NONE',  ( 0.6001305935487422083, -23.60027211631858179, 41.92422178329128712 ) ) ;
#28307 = CARTESIAN_POINT ( 'NONE',  ( 0.8560838555295158248, 46.60258007729424889, -5.345312359545362213 ) ) ;
#28308 = B_SPLINE_CURVE_WITH_KNOTS ( 'NONE', 3,
 ( #58664, #47766, #43078, #115 ),
 .UNSPECIFIED., .F., .F.,
 ( 4, 4 ),
 ( 2.927345865710861972E-18, 0.004444878191957672177 ),
 .UNSPECIFIED. ) ;
#28309 = CARTESIAN_POINT ( 'NONE',  ( 2.618530812446115519, -44.84885430744860457, -14.08215383055621572 ) ) ;
#28310 = VECTOR ( 'NONE', #54211, 999.9999999999998863 ) ;
#28311 = EDGE_LOOP ( 'NONE', ( #32739, #13127, #51961, #60118 ) ) ;
#28312 = CARTESIAN_POINT ( 'NONE',  ( 0.5800708119828336118, -38.37709857409249992, -28.65679933661834511 ) ) ;
#28313 = CARTESIAN_POINT ( 'NONE',  ( 0.9741495583595173313, 30.05988007970395870, 30.61921547032163815 ) ) ;
#28314 = LINE ( 'NONE', #22695, #45462 ) ;
#28315 = EDGE_LOOP ( 'NONE', ( #18045, #11894, #14814, #17986 ) ) ;
#28316 = ORIENTED_EDGE ( 'NONE', *, *, #12552, .T. ) ;
#28317 = FACE_OUTER_BOUND ( 'NONE', #26312, .T. ) ;
#28318 = LINE ( 'NONE', #41518, #7658 ) ;
#28319 = CARTESIAN_POINT ( 'NONE',  ( 4.975610109902397937, 38.85236532789244279, 29.71435874397685595 ) ) ;
#28320 = CARTESIAN_POINT ( 'NONE',  ( -4.915099999999998914, 0.000000000000000000, 0.000000000000000000 ) ) ;
#28321 = CARTESIAN_POINT ( 'NONE',  ( 3.680974057930773036, -14.19449211152969781, 45.82782223000849342 ) ) ;
#28322 = B_SPLINE_CURVE_WITH_KNOTS ( 'NONE', 3,
 ( #42046, #18221, #13839, #61706 ),
 .UNSPECIFIED., .F., .F.,
 ( 4, 4 ),
 ( 1.951563910473907981E-18, 0.004048833967417086489 ),
 .UNSPECIFIED. ) ;
#28323 = CARTESIAN_POINT ( 'NONE',  ( 0.1155031312995260795, -17.70651496066106034, -40.41560293351683697 ) ) ;
#28324 = CARTESIAN_POINT ( 'NONE',  ( 5.860006189529246790, -21.34829429597497708, 43.25137511473244700 ) ) ;
#28325 = DIRECTION ( 'NONE',  ( -2.168404344971009361E-16, 1.000000000000000000, 0.000000000000000000 ) ) ;
#28326 = ADVANCED_FACE ( 'NONE', ( #56675 ), #20589, .F. ) ;
#28327 = CARTESIAN_POINT ( 'NONE',  ( 4.975610109902397937, 2.142807115709095100, 48.86571174967821918 ) ) ;
#28328 = CARTESIAN_POINT ( 'NONE',  ( 5.910764540655177868, 3.360528482495168223, -19.82947520201938829 ) ) ;
#28329 = CARTESIAN_POINT ( 'NONE',  ( 0.9789889208857698311, 41.90853909528808430, -0.09617141507911233789 ) ) ;
#28330 = CARTESIAN_POINT ( 'NONE',  ( 5.958863334805807099, -5.311251202228716828, -19.82657410201440840 ) ) ;
#28331 = VERTEX_POINT ( 'NONE', #15952 ) ;
#28332 = DIRECTION ( 'NONE',  ( 0.1011922191286468153, -0.2707140367832097105, 0.9573265091265147353 ) ) ;
#28333 = CARTESIAN_POINT ( 'NONE',  ( 0.6000166863083106206, -1.051715750663621884, -49.09905676984293876 ) ) ;
#28334 = CARTESIAN_POINT ( 'NONE',  ( 0.1158403557922069033, -35.33903139989523368, -26.42145277801803971 ) ) ;
#28335 = LINE ( 'NONE', #57743, #19033 ) ;
#28336 = B_SPLINE_CURVE_WITH_KNOTS ( 'NONE', 3,
 ( #46797, #3836, #4742, #37388, #56461, #8863 ),
 .UNSPECIFIED., .F., .F.,
 ( 4, 2, 4 ),
 ( 8.131516293641283255E-19, 0.0002293801035737058755, 0.0004587602071474109378 ),
 .UNSPECIFIED. ) ;
#28337 = LINE ( 'NONE', #18342, #1096 ) ;
#28338 = AXIS2_PLACEMENT_3D ( 'NONE', #39450, #9679, #33202 ) ;
#28339 = CARTESIAN_POINT ( 'NONE',  ( 0.1084644655670278651, 42.80575641816240307, 5.234391617064142466 ) ) ;
#28340 = DIRECTION ( 'NONE',  ( 1.000000000000000000, 0.000000000000000000, 0.000000000000000000 ) ) ;
#28341 = CARTESIAN_POINT ( 'NONE',  ( 0.6064515330803582627, 10.17911311372881755, -45.77903441811543672 ) ) ;
#28342 = CARTESIAN_POINT ( 'NONE',  ( -6.077587904424778920, 3.067159685105589784, -19.01022232536993783 ) ) ;
#28344 = EDGE_LOOP ( 'NONE', ( #34810, #10194, #33021, #48769 ) ) ;
#28343 = CARTESIAN_POINT ( 'NONE',  ( 0.8751705887134423323, 5.393078191592057813, 47.79200036674281904 ) ) ;
#28345 = ORIENTED_EDGE ( 'NONE', *, *, #9339, .T. ) ;
#28346 = CARTESIAN_POINT ( 'NONE',  ( 1.399999999999998579, 0.000000000000000000, 0.000000000000000000 ) ) ;
#28347 = CARTESIAN_POINT ( 'NONE',  ( 0.8557997880470606944, 43.90420959842181503, 19.17299735372024827 ) ) ;
#28348 = CARTESIAN_POINT ( 'NONE',  ( 5.965394784446458765, -14.52385693118993082, -14.50338846149128358 ) ) ;
#28349 = VERTEX_POINT ( 'NONE', #15030 ) ;
#28351 = DIRECTION ( 'NONE',  ( 0.09722883295013597105, -0.03945211390408235458, 0.9944798061055105665 ) ) ;
#28350 = VECTOR ( 'NONE', #27115, 1000.000000000000000 ) ;
#28352 = CARTESIAN_POINT ( 'NONE',  ( 0.1102847568649952675, 5.537466591275668648, -42.76743495471824019 ) ) ;
#28353 = EDGE_CURVE ( 'NONE', #45831, #57398, #61354, .T. ) ;
#28354 = ORIENTED_EDGE ( 'NONE', *, *, #53261, .F. ) ;
#28355 = ORIENTED_EDGE ( 'NONE', *, *, #36461, .T. ) ;
#28356 = ADVANCED_FACE ( 'NONE', ( #43543 ), #24615, .F. ) ;
#28357 = CARTESIAN_POINT ( 'NONE',  ( 0.9757402383260933565, 41.42435672089872867, 11.18751708556325397 ) ) ;
#28358 = EDGE_CURVE ( 'NONE', #18917, #55928, #46414, .T. ) ;
#28359 = CARTESIAN_POINT ( 'NONE',  ( 5.960721111146673579, 7.860635756377621242, 18.96073515164551537 ) ) ;
#28360 = CARTESIAN_POINT ( 'NONE',  ( 1.088908134280557105, -34.51503525510833015, -25.50067491870075287 ) ) ;
#28361 = EDGE_CURVE ( 'NONE', #16193, #16923, #6093, .T. ) ;
#28362 = CARTESIAN_POINT ( 'NONE',  ( 4.960386119450144626, -43.42409617054088500, -5.365103581847961323 ) ) ;
#28363 = CARTESIAN_POINT ( 'NONE',  ( 0.5980894510889457338, 19.05812566676443254, 44.17723055703957868 ) ) ;
#28364 = CARTESIAN_POINT ( 'NONE',  ( 0.5819845079324661441, 37.72030202710114821, -29.51613512130344574 ) ) ;
#28365 = EDGE_LOOP ( 'NONE', ( #13789, #59399, #42339, #26620 ) ) ;
#28366 = B_SPLINE_CURVE_WITH_KNOTS ( 'NONE', 3,
 ( #46934, #56294, #51908, #47531, #33442, #9939 ),
 .UNSPECIFIED., .F., .F.,
 ( 4, 2, 4 ),
 ( 5.421010862427522170E-19, 0.0002293801035737090468, 0.0004587602071474175514 ),
 .UNSPECIFIED. ) ;
#28367 = CARTESIAN_POINT ( 'NONE',  ( 2.643462169533613793, 22.81120928486495458, -42.27470921730917297 ) ) ;
#28368 = ADVANCED_FACE ( 'NONE', ( #54434 ), #54585, .F. ) ;
#28369 = CARTESIAN_POINT ( 'NONE',  ( 0.9968887458511668243, 42.45154664631704833, 6.251925120321585538 ) ) ;
#28370 = ORIENTED_EDGE ( 'NONE', *, *, #36977, .F. ) ;
#28371 = CARTESIAN_POINT ( 'NONE',  ( 0.9762797500689124330, -37.17323042682959766, -19.35137526946170183 ) ) ;
#28372 = CARTESIAN_POINT ( 'NONE',  ( 0.7762777257811900311, -47.89627391089017294, -0.8897018348891000405 ) ) ;
#28373 = CARTESIAN_POINT ( 'NONE',  ( 0.6064515330803572635, -13.21408419773141496, 44.99691450368958101 ) ) ;
#28374 = CARTESIAN_POINT ( 'NONE',  ( 0.9730545539215883499, 15.95224156741828914, 39.83279466599044838 ) ) ;
#28375 = ADVANCED_FACE ( 'NONE', ( #34443 ), #56982, .F. ) ;
#28376 = ORIENTED_EDGE ( 'NONE', *, *, #34026, .F. ) ;
#28377 = EDGE_LOOP ( 'NONE', ( #45750, #41722, #43183, #53633 ) ) ;
#28378 = CARTESIAN_POINT ( 'NONE',  ( 0.5786265663353153954, -17.66171603226112197, 44.52624106864138298 ) ) ;
#28379 = CARTESIAN_POINT ( 'NONE',  ( 4.967162193818130511, 0.000000000000000000, 0.000000000000000000 ) ) ;
#28380 = CARTESIAN_POINT ( 'NONE',  ( 0.7056313189692712262, -2.409529526766163610, -46.83954324518119705 ) ) ;
#28381 =( REPRESENTATION_RELATIONSHIP ('NONE','NONE', #44881, #19619 ) REPRESENTATION_RELATIONSHIP_WITH_TRANSFORMATION ( #39933 )SHAPE_REPRESENTATION_RELATIONSHIP( ) );
#28382 =( BOUNDED_SURFACE ( )  B_SPLINE_SURFACE ( 3, 1, ( 
 ( #20275, #58444 ),
 ( #39393, #15572 ),
 ( #34678, #10876 ),
 ( #29966, #49075 ) ),
 .UNSPECIFIED., .F., .F., .F. ) 
 B_SPLINE_SURFACE_WITH_KNOTS ( ( 4, 4 ),
 ( 2, 2 ),
 ( 0.000000000000000000, 1.000000000000000000 ),
 ( 0.000000000000000000, 1.000000000000000000 ),
 .UNSPECIFIED. ) 
 GEOMETRIC_REPRESENTATION_ITEM ( )  RATIONAL_B_SPLINE_SURFACE ( (
 ( 1.000000000000000000, 1.000000000000000000),
 ( 0.7269869731126817891, 0.9931720237060910339),
 ( 0.7269869731126817891, 0.9931720237060910339),
 ( 1.000000000000000000, 1.000000000000000000) ) ) 
 REPRESENTATION_ITEM ( '' )  SURFACE ( )  );
#28383 = ORIENTED_EDGE ( 'NONE', *, *, #7778, .T. ) ;
#28384 = CARTESIAN_POINT ( 'NONE',  ( 0.6041374136657475802, -34.14050483116160706, 33.89363087702989219 ) ) ;
#28385 = EDGE_LOOP ( 'NONE', ( #22915, #34849, #60342, #60203 ) ) ;
#28386 = CARTESIAN_POINT ( 'NONE',  ( -69.95594261585601714, 0.000000000000000000, 8.000000000000000000 ) ) ;
#28387 = CARTESIAN_POINT ( 'NONE',  ( 0.5835871038041845482, 27.70768690911332399, 37.83541382155152633 ) ) ;
#28388 = ORIENTED_EDGE ( 'NONE', *, *, #41588, .F. ) ;
#28389 = CARTESIAN_POINT ( 'NONE',  ( 1.231276596079881935, -40.90292846002442673, -9.177538581351248226 ) ) ;
#28390 = CARTESIAN_POINT ( 'NONE',  ( 0.5980271706414734822, -49.10762822256506865, 0.7000665654016514639 ) ) ;
#28391 = CARTESIAN_POINT ( 'NONE',  ( 0.9754402186311941225, 25.97197377940605989, -34.15542855230911101 ) ) ;
#28392 = ORIENTED_EDGE ( 'NONE', *, *, #51209, .F. ) ;
#28393 = CARTESIAN_POINT ( 'NONE',  ( 0.1119898979215349644, 24.78191822507562847, -36.50777776498444638 ) ) ;
#28394 = CARTESIAN_POINT ( 'NONE',  ( 0.1119898979215348533, -43.68681028663498722, 6.198702705517695755 ) ) ;
#28395 = FACE_OUTER_BOUND ( 'NONE', #35407, .T. ) ;
#28396 = CARTESIAN_POINT ( 'NONE',  ( 0.6017666602106490625, 29.00829887116070438, -38.37783452831175879 ) ) ;
#28397 = EDGE_CURVE ( 'NONE', #7149, #56267, #24766, .T. ) ;
#28398 = CARTESIAN_POINT ( 'NONE',  ( 0.1103744047535531458, 16.53879706351773393, -39.82693656558416961 ) ) ;
#28399 = EDGE_LOOP ( 'NONE', ( #48644, #18500, #23774, #54386 ) ) ;
#28400 = CARTESIAN_POINT ( 'NONE',  ( 2.643462169533600914, 22.81120928486436483, 42.27470921730947140 ) ) ;
#28401 = ORIENTED_EDGE ( 'NONE', *, *, #25673, .T. ) ;
#28402 = DIRECTION ( 'NONE',  ( 0.1024043820194936172, 0.4859385467930459335, -0.8679729669084563781 ) ) ;
#28403 = CARTESIAN_POINT ( 'NONE',  ( 5.880360259849752858, 26.69116321728570540, -39.86101557989643140 ) ) ;
#28404 = CARTESIAN_POINT ( 'NONE',  ( 5.974727161628367256, -2.694421823322779019, -20.34732802718246703 ) ) ;
#28405 = CARTESIAN_POINT ( 'NONE',  ( 4.999999999999986677, 54.69470952477936976, 58.44237546506825964 ) ) ;
#28406 = B_SPLINE_CURVE_WITH_KNOTS ( 'NONE', 3,
 ( #51707, #37033, #52318, #42043, #52629, #3774 ),
 .UNSPECIFIED., .F., .F.,
 ( 4, 2, 4 ),
 ( 9.948699630566631321E-18, 0.0002291472222819947516, 0.0004582944445639795827 ),
 .UNSPECIFIED. ) ;
#28407 = CARTESIAN_POINT ( 'NONE',  ( 4.000000000000003553, 2.309401076758480720, -5.599999999999999645 ) ) ;
#28408 = DIRECTION ( 'NONE',  ( 1.000000000000000000, 1.836909530733573776E-16, 0.000000000000000000 ) ) ;
#28409 = CARTESIAN_POINT ( 'NONE',  ( 0.5838002273316411639, -47.89576566046789452, -0.1361971433783075169 ) ) ;
#28410 = CARTESIAN_POINT ( 'NONE',  ( 0.8744876279028263033, -29.90976330662845939, -38.93271258621668096 ) ) ;
#28411 = CARTESIAN_POINT ( 'NONE',  ( 0.9789233960466698914, 29.22897439703389466, -30.03337780753075492 ) ) ;
#28412 = CARTESIAN_POINT ( 'NONE',  ( 0.2224561200757591284, 22.21411683958052308, -36.95704201588769422 ) ) ;
#28413 = ORIENTED_EDGE ( 'NONE', *, *, #55853, .F. ) ;
#28414 = DIRECTION ( 'NONE',  ( 0.1024043820194936311, -0.9139094329506659564, 0.3927886084231538288 ) ) ;
#28415 = FACE_OUTER_BOUND ( 'NONE', #28839, .T. ) ;
#28416 = VECTOR ( 'NONE', #38160, 1000.000000000000000 ) ;
#28417 = CARTESIAN_POINT ( 'NONE',  ( 4.553261556744875094, 0.000000000000000000, 0.000000000000000000 ) ) ;
#28418 = CARTESIAN_POINT ( 'NONE',  ( 0.9730545539215883499, 42.47233286818625686, -6.101350888304211573 ) ) ;
#28419 = CARTESIAN_POINT ( 'NONE',  ( -4.214292481396491930, -11.25702090725073035, -1.199999999999999956 ) ) ;
#28420 = B_SPLINE_CURVE_WITH_KNOTS ( 'NONE', 3,
 ( #32295, #46106, #51692, #17898, #3154, #31366, #22280, #61085, #17582, #22898, #36704, #37021, #8785, #55770, #13195, #8459, #18199, #56387, #13502 ),
 .UNSPECIFIED., .F., .F.,
 ( 4, 3, 3, 3, 3, 3, 4 ),
 ( 9.541595121948227273E-18, 0.0002732106629380621609, 0.0004098138914053778715, 0.0005464171197651488581, 0.0006830203481512578259, 0.0008196235766963648256, 0.001011968216111141594 ),
 .UNSPECIFIED. ) ;
#28421 = VERTEX_POINT ( 'NONE', #59772 ) ;
#28422 = EDGE_CURVE ( 'NONE', #52129, #1361, #13569, .T. ) ;
#28423 = CARTESIAN_POINT ( 'NONE',  ( 0.9758171775293909000, 11.09981579996865264, -41.44794628856068641 ) ) ;
#28424 = DIRECTION ( 'NONE',  ( -1.000000000000000000, -0.000000000000000000, -0.000000000000000000 ) ) ;
#28425 = DIRECTION ( 'NONE',  ( -0.1011922191286467182, 0.8730847945189542658, -0.4769518595913168069 ) ) ;
#28426 = ORIENTED_EDGE ( 'NONE', *, *, #55433, .F. ) ;
#28427 = EDGE_CURVE ( 'NONE', #60972, #14899, #55370, .T. ) ;
#28428 = CARTESIAN_POINT ( 'NONE',  ( 0.9730545539215883499, -25.71816799638755668, -34.34678117142582465 ) ) ;
#28429 = VECTOR ( 'NONE', #22233, 999.9999999999998863 ) ;
#28430 = B_SPLINE_CURVE_WITH_KNOTS ( 'NONE', 3,
 ( #51087, #32314, #51391, #18219 ),
 .UNSPECIFIED., .F., .F.,
 ( 4, 4 ),
 ( 1.388456241783856658E-17, 0.005004948556313818311 ),
 .UNSPECIFIED. ) ;
#28431 = B_SPLINE_CURVE_WITH_KNOTS ( 'NONE', 3,
 ( #39109, #1770, #35323, #39726, #6765, #20899 ),
 .UNSPECIFIED., .F., .F.,
 ( 4, 2, 4 ),
 ( 1.870693080156664505E-17, 0.0002293319059085104962, 0.0004586638118170022899 ),
 .UNSPECIFIED. ) ;
#28432 = CARTESIAN_POINT ( 'NONE',  ( 0.5832655196449133550, 43.08542359691993795, 18.51705852578387379 ) ) ;
#28433 = DIRECTION ( 'NONE',  ( 1.000000000000000000, 1.836909530733573776E-16, -1.925929944387235853E-32 ) ) ;
#28434 = ORIENTED_EDGE ( 'NONE', *, *, #30352, .T. ) ;
#28435 = EDGE_LOOP ( 'NONE', ( #43602, #8933, #32166, #10766 ) ) ;
#28436 = CARTESIAN_POINT ( 'NONE',  ( 50.50000000000000000, 15.27178771460631168, -2.649999999999992806 ) ) ;
#28437 = EDGE_CURVE ( 'NONE', #59248, #44953, #13888, .T. ) ;
#28438 = CARTESIAN_POINT ( 'NONE',  ( 1.088908134280556661, 42.90644581410506220, -0.7803765577543299026 ) ) ;
#28439 = ORIENTED_EDGE ( 'NONE', *, *, #39697, .T. ) ;
#28440 = CARTESIAN_POINT ( 'NONE',  ( 0.7762783648524360647, -24.71864151483687166, -41.03453896757969943 ) ) ;
#28441 = CARTESIAN_POINT ( 'NONE',  ( 50.50000000000000000, 15.27178771460631168, 2.649999999999992806 ) ) ;
#28442 = CARTESIAN_POINT ( 'NONE',  ( 0.5806925824938502512, -8.338382001837375768, -46.14860504863607105 ) ) ;
#28443 = CARTESIAN_POINT ( 'NONE',  ( 4.975610109902397937, 38.85236532789286201, -29.71435874397630528 ) ) ;
#28444 = EDGE_CURVE ( 'NONE', #21051, #42119, #2333, .T. ) ;
#28445 = B_SPLINE_CURVE_WITH_KNOTS ( 'NONE', 3,
 ( #48387, #39315, #29890, #24269, #34298, #34002, #53986, #1671, #11112, #44632, #29582, #5448, #29272, #25193, #20812, #15499, #48692, #6358, #10178 ),
 .UNSPECIFIED., .F., .F.,
 ( 4, 3, 3, 3, 3, 3, 4 ),
 ( 1.144439277862597989E-16, 0.0002618519381806278684, 0.0003927759815485985773, 0.0005237000248299448395, 0.0006546240681325003188, 0.0007855481115631340102, 0.0009699050456655093156 ),
 .UNSPECIFIED. ) ;
#28446 = ORIENTED_EDGE ( 'NONE', *, *, #12560, .F. ) ;
#28447 = DIRECTION ( 'NONE',  ( 0.000000000000000000, 0.000000000000000000, 1.000000000000000000 ) ) ;
#28448 = EDGE_LOOP ( 'NONE', ( #50862, #51777, #52008, #40728 ) ) ;
#28449 = CARTESIAN_POINT ( 'NONE',  ( 0.8560838555295158248, -44.00447048317951726, -16.24744323198929052 ) ) ;
#28450 =( BOUNDED_SURFACE ( )  B_SPLINE_SURFACE ( 3, 1, ( 
 ( #35370, #54427 ),
 ( #10943, #30024 ),
 ( #25636, #6811 ),
 ( #25029, #49136 ) ),
 .UNSPECIFIED., .F., .F., .F. ) 
 B_SPLINE_SURFACE_WITH_KNOTS ( ( 4, 4 ),
 ( 2, 2 ),
 ( 0.000000000000000000, 1.000000000000000000 ),
 ( 0.000000000000000000, 1.000000000000000000 ),
 .UNSPECIFIED. ) 
 GEOMETRIC_REPRESENTATION_ITEM ( )  RATIONAL_B_SPLINE_SURFACE ( (
 ( 1.000000000000000000, 1.000000000000000000),
 ( 0.9732289882329797637, 0.9999525324661233672),
 ( 0.9732289882329797637, 0.9999525324661233672),
 ( 1.000000000000000000, 1.000000000000000000) ) ) 
 REPRESENTATION_ITEM ( '' )  SURFACE ( )  );
#28451 = VECTOR ( 'NONE', #46322, 1000.000000000000227 ) ;
#28452 = ORIENTED_EDGE ( 'NONE', *, *, #16102, .F. ) ;
#28453 = ORIENTED_EDGE ( 'NONE', *, *, #29300, .T. ) ;
#28454 = CARTESIAN_POINT ( 'NONE',  ( 0.3676999524040323597, 25.91024933382809436, -35.70167450949183774 ) ) ;
#28455 = CARTESIAN_POINT ( 'NONE',  ( 5.960721111146673579, -20.34914600876577140, 2.685391721745692628 ) ) ;
#28456 = CARTESIAN_POINT ( 'NONE',  ( 4.834790513006553603, -31.42367164492852893, -35.28657253511732961 ) ) ;
#28457 = CARTESIAN_POINT ( 'NONE',  ( 4.975801465491694664, 3.702618843597456522, -47.76942479135481534 ) ) ;
#28458 = ORIENTED_EDGE ( 'NONE', *, *, #42254, .F. ) ;
#28459 = CARTESIAN_POINT ( 'NONE',  ( 0.9757787079277446818, 0.03949005143961138026, -42.90844198810273014 ) ) ;
#28460 = CARTESIAN_POINT ( 'NONE',  ( 0.8560838555295223751, -46.14148336882287538, -8.446084690930739214 ) ) ;
#28461 = CARTESIAN_POINT ( 'NONE',  ( 0.1152809850208375980, -38.55430589558707766, 21.45951489198335338 ) ) ;
#28462 = VERTEX_POINT ( 'NONE', #22493 ) ;
#28463 = ORIENTED_EDGE ( 'NONE', *, *, #13335, .F. ) ;
#28464 = CARTESIAN_POINT ( 'NONE',  ( 0.1102847568649952675, -21.64199720113217040, -37.30068345220683312 ) ) ;
#28465 = CARTESIAN_POINT ( 'NONE',  ( 5.860006189529234355, 45.67886430272030651, 15.48781697582063366 ) ) ;
#28466 = CARTESIAN_POINT ( 'NONE',  ( 5.901764892641307547, 30.49809846213652520, 38.31262791343741014 ) ) ;
#28467 = EDGE_CURVE ( 'NONE', #20535, #5623, #50934, .T. ) ;
#28468 = CARTESIAN_POINT ( 'NONE',  ( 0.2885697896453110478, -42.63514065501010464, -6.424755442172452646 ) ) ;
#28470 = AXIS2_PLACEMENT_3D ( 'NONE', #34864, #25439, #15138 ) ;
#28469 = CARTESIAN_POINT ( 'NONE',  ( -6.015611763856276717, -16.31561949997069405, -9.427003116184344833 ) ) ;
#28471 = VERTEX_POINT ( 'NONE', #27191 ) ;
#28472 = ORIENTED_EDGE ( 'NONE', *, *, #59404, .F. ) ;
#28473 = AXIS2_PLACEMENT_3D ( 'NONE', #41617, #32214, #17186 ) ;
#28474 = CARTESIAN_POINT ( 'NONE',  ( 4.335381028904216727, -46.80143676542533626, 14.47005059964335771 ) ) ;
#28475 = CARTESIAN_POINT ( 'NONE',  ( -6.016104459813371719, -14.95258000663124243, -11.46679299034596156 ) ) ;
#28476 = CARTESIAN_POINT ( 'NONE',  ( 2.500000000000000000, -1.178949249685214307, 2.042000000000001592 ) ) ;
#28477 = CARTESIAN_POINT ( 'NONE',  ( 0.9756008150404614776, -21.33101788548756161, 37.23069985082535993 ) ) ;
#28478 = CARTESIAN_POINT ( 'NONE',  ( 3.238018933889920792, 13.30865154331494438, 1.512377752505517092 ) ) ;
#28479 = VERTEX_POINT ( 'NONE', #7130 ) ;
#28480 = CARTESIAN_POINT ( 'NONE',  ( 0.1147471544378675379, 20.13337721096016608, -39.26320555627666664 ) ) ;
#28481 = CARTESIAN_POINT ( 'NONE',  ( 0.1073791018717483448, 26.63563652260123149, 33.91564619577815165 ) ) ;
#28482 = DIRECTION ( 'NONE',  ( 0.09835009131224552170, -0.9592125346408738595, 0.2650256080583596185 ) ) ;
#28483 = CARTESIAN_POINT ( 'NONE',  ( 5.959547316686252039, 17.77749189599217416, -10.25972575517511487 ) ) ;
#28484 = CARTESIAN_POINT ( 'NONE',  ( -6.078726893082806448, 0.6205993875982012131, 19.24600991553399254 ) ) ;
#28485 = CARTESIAN_POINT ( 'NONE',  ( -2.708315649062910779, -0.2635547933244546392, 14.63219292706382468 ) ) ;
#28486 = CARTESIAN_POINT ( 'NONE',  ( 0.8560838555295223751, 37.37287335782406217, 28.34856559090382078 ) ) ;
#28487 = VECTOR ( 'NONE', #31831, 999.9999999999998863 ) ;
#28488 = EDGE_CURVE ( 'NONE', #243, #8457, #19877, .T. ) ;
#28489 = CARTESIAN_POINT ( 'NONE',  ( 4.549368137175248350, -42.84816078363928682, 2.596185425821780246 ) ) ;
#28490 = ORIENTED_EDGE ( 'NONE', *, *, #55071, .F. ) ;
#28491 = CARTESIAN_POINT ( 'NONE',  ( 0.1103878639767399555, 37.37111717125843313, 21.52017980327911317 ) ) ;
#28492 = CARTESIAN_POINT ( 'NONE',  ( 0.9784957157296378938, 20.34434192463124091, 36.63933417307226392 ) ) ;
#28493 = CARTESIAN_POINT ( 'NONE',  ( 2.282803330402962239, -15.16644679234350690, 44.45757302363679742 ) ) ;
#28494 = CARTESIAN_POINT ( 'NONE',  ( 0.5806925824938511393, 42.95845041307772050, -18.80940989108128747 ) ) ;
#28495 = VERTEX_POINT ( 'NONE', #60081 ) ;
#28496 = EDGE_CURVE ( 'NONE', #3952, #217, #36772, .T. ) ;
#28497 = CARTESIAN_POINT ( 'NONE',  ( 0.5804410086790514622, -45.84731009780865918, 9.876437042312852910 ) ) ;
#28498 = DIRECTION ( 'NONE',  ( 0.07500201931887537365, -0.8510178133412981127, -0.5197531899602795269 ) ) ;
#28499 = EDGE_CURVE ( 'NONE', #5464, #61588, #16561, .T. ) ;
#28500 = PLANE ( 'NONE',  #38561 ) ;
#28501 = ORIENTED_EDGE ( 'NONE', *, *, #46928, .F. ) ;
#28502 = CARTESIAN_POINT ( 'NONE',  ( 0.1152809850208375286, 4.457062010796396301, -43.89851797864788097 ) ) ;
#28503 = CARTESIAN_POINT ( 'NONE',  ( 4.960156602257184133, -26.21519897043405223, -38.31207700265980520 ) ) ;
#28504 = AXIS2_PLACEMENT_3D ( 'NONE', #11942, #12240, #27246 ) ;
#28505 = CARTESIAN_POINT ( 'NONE',  ( 0.9730545539215883499, -33.73144377768576874, 26.52009130076758225 ) ) ;
#28506 = ORIENTED_EDGE ( 'NONE', *, *, #51058, .F. ) ;
#28507 = CARTESIAN_POINT ( 'NONE',  ( 0.1365634738349425503, 41.67041550752998091, 14.50651891575141406 ) ) ;
#28508 = VECTOR ( 'NONE', #44108, 1000.000000000000114 ) ;
#28509 = ORIENTED_EDGE ( 'NONE', *, *, #43024, .T. ) ;
#28510 = CARTESIAN_POINT ( 'NONE',  ( 4.553261556744875094, 0.000000000000000000, 0.000000000000000000 ) ) ;
#28511 = VERTEX_POINT ( 'NONE', #45396 ) ;
#28512 = CARTESIAN_POINT ( 'NONE',  ( 0.5839879882012694035, -6.251708210201749161, -47.48620708510745914 ) ) ;
#28513 = LINE ( 'NONE', #5002, #57468 ) ;
#28514 = ORIENTED_EDGE ( 'NONE', *, *, #34450, .F. ) ;
#28515 = CARTESIAN_POINT ( 'NONE',  ( 0.8760168074887076939, -13.30888447662048968, -46.22580377597780910 ) ) ;
#28516 = EDGE_CURVE ( 'NONE', #57370, #47719, #26986, .T. ) ;
#28517 = AXIS2_PLACEMENT_3D ( 'NONE', #35575, #39982, #45287 ) ;
#28518 = B_SPLINE_CURVE_WITH_KNOTS ( 'NONE', 3,
 ( #12361, #2933, #2303, #55544 ),
 .UNSPECIFIED., .F., .F.,
 ( 4, 4 ),
 ( 0.000000000000000000, 0.005014147105413691713 ),
 .UNSPECIFIED. ) ;
#28519 = ORIENTED_EDGE ( 'NONE', *, *, #8669, .T. ) ;
#28520 = CARTESIAN_POINT ( 'NONE',  ( 4.967162193818129623, -13.42934394584134949, -40.93989340068622340 ) ) ;
#28521 = CARTESIAN_POINT ( 'NONE',  ( 0.5830082357119563685, 40.20946850652512694, 24.13360058841410449 ) ) ;
#28522 =( BOUNDED_SURFACE ( )  B_SPLINE_SURFACE ( 3, 1, ( 
 ( #5220, #9952 ),
 ( #48164, #24351 ),
 ( #10881, #53148 ),
 ( #38783, #29350 ) ),
 .UNSPECIFIED., .F., .F., .F. ) 
 B_SPLINE_SURFACE_WITH_KNOTS ( ( 4, 4 ),
 ( 2, 2 ),
 ( 0.000000000000000000, 1.000000000000000000 ),
 ( 0.000000000000000000, 1.000000000000000000 ),
 .UNSPECIFIED. ) 
 GEOMETRIC_REPRESENTATION_ITEM ( )  RATIONAL_B_SPLINE_SURFACE ( (
 ( 1.000000000000000000, 1.000000000000000000),
 ( 0.9729067724841187204, 0.9999501103223794596),
 ( 0.9729067724841187204, 0.9999501103223794596),
 ( 1.000000000000000000, 1.000000000000000000) ) ) 
 REPRESENTATION_ITEM ( '' )  SURFACE ( )  );
#28523 = ORIENTED_EDGE ( 'NONE', *, *, #23113, .T. ) ;
#28524 = CARTESIAN_POINT ( 'NONE',  ( 0.5804410086790514622, -46.75463715370017326, 3.677466040799799440 ) ) ;
#28525 = CARTESIAN_POINT ( 'NONE',  ( 5.960721111146673579, -7.848955554238384202, -18.96557324978284242 ) ) ;
#28526 = CARTESIAN_POINT ( 'NONE',  ( -6.078075953587585900, 15.43522972334799093, 11.51298647765255900 ) ) ;
#28527 = ORIENTED_EDGE ( 'NONE', *, *, #6086, .F. ) ;
#28528 = CARTESIAN_POINT ( 'NONE',  ( 0.5848930533535030563, -1.384993715960175509, 46.87595198813895792 ) ) ;
#28529 = CARTESIAN_POINT ( 'NONE',  ( 2.643462169533600914, -42.27470921730956377, 22.81120928486421917 ) ) ;
#28530 = ORIENTED_EDGE ( 'NONE', *, *, #21788, .F. ) ;
#28531 = FACE_OUTER_BOUND ( 'NONE', #18860, .T. ) ;
#28532 = VERTEX_POINT ( 'NONE', #2125 ) ;
#28533 = CARTESIAN_POINT ( 'NONE',  ( 2.500000000000000000, 2.500728763858895382E-16, -2.041999999999999815 ) ) ;
#28534 = CARTESIAN_POINT ( 'NONE',  ( 0.9730545539215883499, 30.69604515769650632, 29.98130006528872826 ) ) ;
#28535 = EDGE_LOOP ( 'NONE', ( #6989, #40651, #3311, #30733 ) ) ;
#28536 = CARTESIAN_POINT ( 'NONE',  ( 3.680974057930773480, 14.19449211152937806, -45.82782223000860711 ) ) ;
#28537 = CARTESIAN_POINT ( 'NONE',  ( 0.1152339509894530906, 25.06061834086574081, -36.31677434504207724 ) ) ;
#28538 = CARTESIAN_POINT ( 'NONE',  ( 0.1129192098497447394, -0.9297496242502409913, 44.11448008785053077 ) ) ;
#28539 = CARTESIAN_POINT ( 'NONE',  ( 0.9790850452238870627, -22.59298530334723765, -35.29722857882659781 ) ) ;
#28540 =( BOUNDED_SURFACE ( )  B_SPLINE_SURFACE ( 3, 1, ( 
 ( #24296, #10826 ),
 ( #19613, #1388 ),
 ( #43747, #14609 ),
 ( #34631, #53696 ) ),
 .UNSPECIFIED., .F., .F., .F. ) 
 B_SPLINE_SURFACE_WITH_KNOTS ( ( 4, 4 ),
 ( 2, 2 ),
 ( 0.000000000000000000, 1.000000000000000000 ),
 ( 0.000000000000000000, 1.000000000000000000 ),
 .UNSPECIFIED. ) 
 GEOMETRIC_REPRESENTATION_ITEM ( )  RATIONAL_B_SPLINE_SURFACE ( (
 ( 1.000000000000000000, 1.000000000000000000),
 ( 0.9952954269826590483, 0.8620686068821307169),
 ( 0.9952954269826590483, 0.8620686068821307169),
 ( 1.000000000000000000, 1.000000000000000000) ) ) 
 REPRESENTATION_ITEM ( '' )  SURFACE ( )  );
#28541 = ORIENTED_EDGE ( 'NONE', *, *, #42518, .F. ) ;
#28542 = CARTESIAN_POINT ( 'NONE',  ( 0.9972139404380298000, 41.61281131482461859, 10.46878911444690452 ) ) ;
#28543 = ADVANCED_FACE ( 'NONE', ( #2441 ), #11825, .F. ) ;
#28544 =( BOUNDED_SURFACE ( )  B_SPLINE_SURFACE ( 3, 1, ( 
 ( #19099, #57259 ),
 ( #14395, #61350 ),
 ( #28164, #51343 ),
 ( #56043, #23167 ) ),
 .UNSPECIFIED., .F., .F., .F. ) 
 B_SPLINE_SURFACE_WITH_KNOTS ( ( 4, 4 ),
 ( 2, 2 ),
 ( 0.000000000000000000, 1.000000000000000000 ),
 ( 0.000000000000000000, 1.000000000000000000 ),
 .UNSPECIFIED. ) 
 GEOMETRIC_REPRESENTATION_ITEM ( )  RATIONAL_B_SPLINE_SURFACE ( (
 ( 1.000000000000000000, 1.000000000000000000),
 ( 0.7211978278499970862, 0.9934217856018976445),
 ( 0.7211978278499970862, 0.9934217856018976445),
 ( 1.000000000000000000, 1.000000000000000000) ) ) 
 REPRESENTATION_ITEM ( '' )  SURFACE ( )  );
#28545 = CARTESIAN_POINT ( 'NONE',  ( 4.322998006666165516, -20.30542865297677935, 43.48102276965666135 ) ) ;
#28546 = CARTESIAN_POINT ( 'NONE',  ( -6.016489644550736315, -18.84320342686341121, 0.004404229197709936920 ) ) ;
#28547 = B_SPLINE_CURVE_WITH_KNOTS ( 'NONE', 3,
 ( #6319, #59896, #25773, #30772, #35500, #26082 ),
 .UNSPECIFIED., .F., .F.,
 ( 4, 2, 4 ),
 ( 1.951563910473907981E-18, 0.0002447193893791694912, 0.0004894387787583370309 ),
 .UNSPECIFIED. ) ;
#28548 = EDGE_CURVE ( 'NONE', #34766, #15927, #47962, .T. ) ;
#28549 = B_SPLINE_CURVE_WITH_KNOTS ( 'NONE', 3,
 ( #42996, #28551, #47672, #29478, #13868, #5646 ),
 .UNSPECIFIED., .F., .F.,
 ( 4, 2, 4 ),
 ( 1.499559393730840704E-16, 0.0002445252820015210871, 0.0004890505640028922291 ),
 .UNSPECIFIED. ) ;
#28550 = DIRECTION ( 'NONE',  ( 1.000000000000000000, 1.836909530733573776E-16, 0.000000000000000000 ) ) ;
#28551 = CARTESIAN_POINT ( 'NONE',  ( 0.7762777257811892540, 46.49451973287617790, -11.53708189756892466 ) ) ;
#28552 = B_SPLINE_CURVE_WITH_KNOTS ( 'NONE', 3,
 ( #22725, #36848, #46238, #55595 ),
 .UNSPECIFIED., .F., .F.,
 ( 4, 4 ),
 ( 2.318323674163820247E-17, 0.004564976165746189446 ),
 .UNSPECIFIED. ) ;
#28553 = CIRCLE ( 'NONE', #61546, 18.99999999999999645 ) ;
#28554 = CARTESIAN_POINT ( 'NONE',  ( 1.157644175074337367, -13.20506553587984477, 39.78226388319673390 ) ) ;
#28555 = EDGE_CURVE ( 'NONE', #54380, #26593, #43425, .T. ) ;
#28556 = CARTESIAN_POINT ( 'NONE',  ( 0.8760168074887076939, 7.161346975773065893, 47.56749362999715913 ) ) ;
#28557 = CIRCLE ( 'NONE', #32564, 13.50000000000000178 ) ;
#28558 = DIRECTION ( 'NONE',  ( 0.07439287786467665975, -0.3693942911085648095, -0.9262902123089783446 ) ) ;
#28559 = DIRECTION ( 'NONE',  ( -0.1024043820194934645, -0.8548216096550925736, -0.5087173657443611052 ) ) ;
#28560 = CARTESIAN_POINT ( 'NONE',  ( 0.5998501479064708430, 48.10473956285918717, 0.5236536531316605680 ) ) ;
#28561 = VECTOR ( 'NONE', #52414, 1000.000000000000000 ) ;
#28562 = CARTESIAN_POINT ( 'NONE',  ( -4.908599999999998964, 0.000000000000000000, 0.000000000000000000 ) ) ;
#28563 = CARTESIAN_POINT ( 'NONE',  ( 0.1147471544378676767, 39.88833925880920361, 18.86458532932503473 ) ) ;
#28564 = CARTESIAN_POINT ( 'NONE',  ( 5.959547316686252039, -7.851524054666280783, -18.96456592444097922 ) ) ;
#28565 = CARTESIAN_POINT ( 'NONE',  ( 0.5848930533535030563, 16.68483824254287384, -43.82795061610497811 ) ) ;
#28566 = CARTESIAN_POINT ( 'NONE',  ( 50.00005079999999680, 0.000000000000000000, 10.00000000000000000 ) ) ;
#28567 = EDGE_CURVE ( 'NONE', #44340, #22451, #4816, .T. ) ;
#28568 = CARTESIAN_POINT ( 'NONE',  ( 0.3676999524040366896, 21.13209774130265473, 38.72189339863005841 ) ) ;
#28569 = VERTEX_POINT ( 'NONE', #13111 ) ;
#28570 = CARTESIAN_POINT ( 'NONE',  ( 0.8554163680231708922, 43.54276151446883603, -17.47092993535007466 ) ) ;
#28571 = DIRECTION ( 'NONE',  ( -0.07439287786467650709, -0.1170659376278904151, 0.9903339163990669824 ) ) ;
#28573 = EDGE_CURVE ( 'NONE', #16242, #60250, #59145, .T. ) ;
#28572 = LINE ( 'NONE', #19204, #24732 ) ;
#28574 = VERTEX_POINT ( 'NONE', #55991 ) ;
#28575 = CARTESIAN_POINT ( 'NONE',  ( -2.708315649062910779, -14.54141329178163389, 1.648584381066805049 ) ) ;
#28576 = CARTESIAN_POINT ( 'NONE',  ( 1.657374760986086271, 26.21018067049697109, 35.41068873196552858 ) ) ;
#28577 = EDGE_CURVE ( 'NONE', #60250, #3477, #17339, .T. ) ;
#28578 = UNCERTAINTY_MEASURE_WITH_UNIT (LENGTH_MEASURE( 1.000000000000000082E-05 ), #40801, 'distance_accuracy_value', 'NONE');
#28579 = EDGE_LOOP ( 'NONE', ( #54206, #26009, #42268, #26193 ) ) ;
#28580 = ORIENTED_EDGE ( 'NONE', *, *, #51052, .T. ) ;
#28581 = CARTESIAN_POINT ( 'NONE',  ( 0.5998501479064699549, 18.89267974119604077, 44.24259072156093708 ) ) ;
#28582 = EDGE_LOOP ( 'NONE', ( #32473, #43037, #45024, #38045 ) ) ;
#28583 = CARTESIAN_POINT ( 'NONE',  ( 0.6064515330803588178, 3.986541738855695183, -46.72731343659132364 ) ) ;
#28584 = CARTESIAN_POINT ( 'NONE',  ( 3.270143674763207553, -9.870732238228589139, 9.482922169187926187 ) ) ;
#28585 = ORIENTED_EDGE ( 'NONE', *, *, #53849, .T. ) ;
#28586 = ORIENTED_EDGE ( 'NONE', *, *, #53724, .F. ) ;
#28587 = DIRECTION ( 'NONE',  ( -0.07906939808003035641, 0.7773121955653319315, -0.6241264142084236299 ) ) ;
#28588 = EDGE_LOOP ( 'NONE', ( #46292, #55082, #6915, #771 ) ) ;
#28589 = CARTESIAN_POINT ( 'NONE',  ( 0.3622758884714730732, 15.73321244754854753, -40.13994584881767480 ) ) ;
#28590 = CARTESIAN_POINT ( 'NONE',  ( 4.975610109902397937, 19.27143522741655701, 44.95621415792550124 ) ) ;
#28591 = EDGE_CURVE ( 'NONE', #32404, #40072, #38385, .T. ) ;
#28592 = B_SPLINE_CURVE_WITH_KNOTS ( 'NONE', 3,
 ( #21865, #16241, #2426, #16547 ),
 .UNSPECIFIED., .F., .F.,
 ( 4, 4 ),
 ( 0.000000000000000000, 0.005014147105413713397 ),
 .UNSPECIFIED. ) ;
#28593 = CARTESIAN_POINT ( 'NONE',  ( -6.078726893082806448, 17.85000270430350611, 7.222980321520863001 ) ) ;
#28594 = VERTEX_POINT ( 'NONE', #52755 ) ;
#28595 = CARTESIAN_POINT ( 'NONE',  ( -6.077587904424778920, -11.02178778841116547, -15.78975032548523139 ) ) ;
#28596 = CARTESIAN_POINT ( 'NONE',  ( 0.9757787079277435716, -34.01751575780804870, -26.15233402543304919 ) ) ;
#28597 = ORIENTED_EDGE ( 'NONE', *, *, #49160, .T. ) ;
#28598 = ORIENTED_EDGE ( 'NONE', *, *, #50017, .F. ) ;
#28599 = CARTESIAN_POINT ( 'NONE',  ( 0.5807400328401574052, -44.45848844984454473, 17.82553128098393103 ) ) ;
#28600 = CONICAL_SURFACE ( 'NONE', #24593, 43.08621763946400307, 1.568696531533066763 ) ;
#28601 = VERTEX_POINT ( 'NONE', #5126 ) ;
#28602 = CARTESIAN_POINT ( 'NONE',  ( 0.6029443449137434907, 46.59195503072400157, 15.51545243936909557 ) ) ;
#28603 = CARTESIAN_POINT ( 'NONE',  ( 0.5806925824938494740, -46.75147433417404841, 3.677228565731047283 ) ) ;
#28604 = CARTESIAN_POINT ( 'NONE',  ( 0.9745511491811756910, -0.3405614984923568400, 42.90705396078542577 ) ) ;
#28605 = CARTESIAN_POINT ( 'NONE',  ( 4.967162193818129623, 32.68434214048168940, 28.07411493385305334 ) ) ;
#28606 = AXIS2_PLACEMENT_3D ( 'NONE', #29955, #29641, #6116 ) ;
#28607 = VERTEX_POINT ( 'NONE', #432 ) ;
#28608 = CARTESIAN_POINT ( 'NONE',  ( 2.648799415243696664, -31.64453936086654906, 37.45851828260384764 ) ) ;
#28609 = LINE ( 'NONE', #33342, #27759 ) ;
#28610 = CARTESIAN_POINT ( 'NONE',  ( 5.896278296736517710, 19.70873670457421767, -4.011567913441433042 ) ) ;
#28611 = EDGE_LOOP ( 'NONE', ( #9794, #33242, #12066, #56478 ) ) ;
#28612 = CARTESIAN_POINT ( 'NONE',  ( -6.078726893082806448, 12.00859800336337280, 15.05282748397580406 ) ) ;
#28613 = CARTESIAN_POINT ( 'NONE',  ( 4.963659409799330291, -9.199077662858595517, -43.79875484948457398 ) ) ;
#28614 = CARTESIAN_POINT ( 'NONE',  ( 2.706805983486680223, -5.384497782719996906, 43.67817872745656871 ) ) ;
#28615 = CIRCLE ( 'NONE', #11643, 6.887500000000022382 ) ;
#28616 = VERTEX_POINT ( 'NONE', #24256 ) ;
#28617 = ORIENTED_EDGE ( 'NONE', *, *, #34521, .T. ) ;
#28618 = CARTESIAN_POINT ( 'NONE',  ( 4.956445790444035104, 35.28522167764516837, -31.18479086508480691 ) ) ;
#28619 = ADVANCED_FACE ( 'NONE', ( #43393 ), #31759, .F. ) ;
#28620 = CARTESIAN_POINT ( 'NONE',  ( 0.5807400328401574052, 23.47602859900714733, 41.75144119563893952 ) ) ;
#28621 = CARTESIAN_POINT ( 'NONE',  ( -6.077587904424778920, 16.77513308702641837, -9.454677747363051665 ) ) ;
#28622 = DIRECTION ( 'NONE',  ( 0.09835009131224564660, 0.3736726418952187601, 0.9223318362920801539 ) ) ;
#28623 = EDGE_CURVE ( 'NONE', #17224, #61039, #39782, .T. ) ;
#28624 = CARTESIAN_POINT ( 'NONE',  ( 0.9730545539215883499, -42.47233286818622133, 6.101350888304490461 ) ) ;
#28625 =( BOUNDED_SURFACE ( )  B_SPLINE_SURFACE ( 3, 1, ( 
 ( #25799, #60843 ),
 ( #7282, #12962 ),
 ( #27342, #22649 ),
 ( #8223, #45862 ) ),
 .UNSPECIFIED., .F., .F., .F. ) 
 B_SPLINE_SURFACE_WITH_KNOTS ( ( 4, 4 ),
 ( 2, 2 ),
 ( 0.000000000000000000, 1.000000000000000000 ),
 ( 0.000000000000000000, 1.000000000000000000 ),
 .UNSPECIFIED. ) 
 GEOMETRIC_REPRESENTATION_ITEM ( )  RATIONAL_B_SPLINE_SURFACE ( (
 ( 1.000000000000000000, 1.000000000000000000),
 ( 0.7223157951917480446, 0.9931996967497186413),
 ( 0.7223157951917480446, 0.9931996967497186413),
 ( 1.000000000000000000, 1.000000000000000000) ) ) 
 REPRESENTATION_ITEM ( '' )  SURFACE ( )  );
#28626 = CARTESIAN_POINT ( 'NONE',  ( 4.963659409799330291, 8.262218268420474132, 43.98510776953411749 ) ) ;
#28627 = CARTESIAN_POINT ( 'NONE',  ( 0.5806925824938502512, -41.60618895332704170, 21.63671424046659908 ) ) ;
#28628 = CARTESIAN_POINT ( 'NONE',  ( 4.834790513006555379, 1.975078679465946951, 47.20898648704820744 ) ) ;
#28629 = FACE_OUTER_BOUND ( 'NONE', #42962, .T. ) ;
#28630 = EDGE_CURVE ( 'NONE', #37726, #46057, #44987, .T. ) ;
#28631 = CARTESIAN_POINT ( 'NONE',  ( 0.9788927965476030835, 41.90843032204052321, -0.1417059435968782144 ) ) ;
#28632 = ADVANCED_FACE ( 'NONE', ( #40588 ), #35795, .F. ) ;
#28633 = CARTESIAN_POINT ( 'NONE',  ( 0.3676999524040366896, 40.09552319080398775, 18.39292264373822405 ) ) ;
#28634 = VERTEX_POINT ( 'NONE', #14157 ) ;
#28635 = EDGE_CURVE ( 'NONE', #37784, #15622, #10569, .T. ) ;
#28636 = CARTESIAN_POINT ( 'NONE',  ( 0.5786265663353153954, 23.32245830379087081, -41.83999636203295580 ) ) ;
#28637 = CARTESIAN_POINT ( 'NONE',  ( 0.6021448801613057400, 41.01326314309687859, 27.00839471316351137 ) ) ;
#28638 = CARTESIAN_POINT ( 'NONE',  ( 0.1158516988532803521, -35.39112975881853629, -26.35166205815612273 ) ) ;
#28639 = CARTESIAN_POINT ( 'NONE',  ( 4.967162193818130511, 24.30453456948110613, 35.57684288741985768 ) ) ;
#28640 = CARTESIAN_POINT ( 'NONE',  ( 0.5998501479064708430, -34.38546660123321175, 33.64490850298784608 ) ) ;
#28641 = CARTESIAN_POINT ( 'NONE',  ( 0.8554163680231816613, -13.02474486562579870, 45.07284652978080430 ) ) ;
#28642 = ITEM_DEFINED_TRANSFORMATION ( 'NONE', 'NONE', #8865,  #14677 ) ;
#28643 = CARTESIAN_POINT ( 'NONE',  ( -6.015611763856276717, 18.84324252354755203, -0.006214430185207123029 ) ) ;
#28644 = CARTESIAN_POINT ( 'NONE',  ( 0.6029443199889047422, 22.71403544353044524, -43.53860626759250607 ) ) ;
#28645 = EDGE_CURVE ( 'NONE', #27021, #55166, #35883, .T. ) ;
#28646 = CARTESIAN_POINT ( 'NONE',  ( 4.291220156522060236, 8.814262783203506757, -46.27848062430671661 ) ) ;
#28647 = AXIS2_PLACEMENT_3D ( 'NONE', #41068, #31632, #16935 ) ;
#28648 = ADVANCED_FACE ( 'NONE', ( #16764 ), #13937, .F. ) ;
#28649 = CARTESIAN_POINT ( 'NONE',  ( 4.975801465491695552, 0.000000000000000000, 0.000000000000000000 ) ) ;
#28651 = ORIENTED_EDGE ( 'NONE', *, *, #40419, .F. ) ;
#28650 = CARTESIAN_POINT ( 'NONE',  ( -0.2111111111111110827, -9.497654031326126400, -1.199999999999999956 ) ) ;
#28652 = ORIENTED_EDGE ( 'NONE', *, *, #3196, .F. ) ;
#28653 = AXIS2_PLACEMENT_3D ( 'NONE', #54311, #11754, #26140 ) ;
#28654 = B_SPLINE_CURVE_WITH_KNOTS ( 'NONE', 3,
 ( #51942, #47259, #23445, #56947, #55706, #17831 ),
 .UNSPECIFIED., .F., .F.,
 ( 4, 2, 4 ),
 ( 0.000000000000000000, 0.0002447195606305753424, 0.0004894391212611506848 ),
 .UNSPECIFIED. ) ;
#28655 = CARTESIAN_POINT ( 'NONE',  ( 4.967162193818130511, -32.10009971360091896, 28.74031574030002645 ) ) ;
#28656 = CARTESIAN_POINT ( 'NONE',  ( 0.1102847568649952675, 39.87696813145905850, 16.41780866919057047 ) ) ;
#28657 = AXIS2_PLACEMENT_3D ( 'NONE', #2571, #49891, #6625 ) ;
#28658 = CARTESIAN_POINT ( 'NONE',  ( 0.8551540677456834771, 11.51835730326545004, -46.51172240253108470 ) ) ;
#28659 = ORIENTED_EDGE ( 'NONE', *, *, #50141, .F. ) ;
#28660 = CARTESIAN_POINT ( 'NONE',  ( 0.5824935313925941882, 22.85613393777071423, 40.94917970451332678 ) ) ;
#28661 = CARTESIAN_POINT ( 'NONE',  ( 0.5817216825391123836, -45.86342747968472366, 9.786775363885668710 ) ) ;
#28662 = CARTESIAN_POINT ( 'NONE',  ( -6.016761891674565099, 17.40752468084782834, 7.214149619366422961 ) ) ;
#28663 = ORIENTED_EDGE ( 'NONE', *, *, #38983, .F. ) ;
#28664 = VERTEX_POINT ( 'NONE', #2638 ) ;
#28665 = CARTESIAN_POINT ( 'NONE',  ( -5.995132425357893702, 11.46484027925389348, -14.95525565067262797 ) ) ;
#28666 = AXIS2_PLACEMENT_3D ( 'NONE', #33839, #24728, #10324 ) ;
#28667 = CARTESIAN_POINT ( 'NONE',  ( 4.960156602257181468, -45.42786611289307075, -9.558288641082238968 ) ) ;
#28668 = CARTESIAN_POINT ( 'NONE',  ( 5.901764892641307547, 42.64666365787686431, 24.06768676652583849 ) ) ;
#28669 = CARTESIAN_POINT ( 'NONE',  ( 42.00000000000000711, -15.99999999999998934, 1.959434878635763159E-15 ) ) ;
#28670 = EDGE_CURVE ( 'NONE', #42065, #35170, #32213, .T. ) ;
#28671 = B_SPLINE_CURVE_WITH_KNOTS ( 'NONE', 3,
 ( #19014, #23692, #38130, #31869 ),
 .UNSPECIFIED., .F., .F.,
 ( 4, 4 ),
 ( 0.000000000000000000, 0.005013413432710149380 ),
 .UNSPECIFIED. ) ;
#28672 = CARTESIAN_POINT ( 'NONE',  ( 0.7948878604505659196, 48.02008979560216062, -10.23570336228642219 ) ) ;
#28673 = B_SPLINE_CURVE_WITH_KNOTS ( 'NONE', 3,
 ( #3040, #50963, #46294, #17164 ),
 .UNSPECIFIED., .F., .F.,
 ( 4, 4 ),
 ( 0.000000000000000000, 0.005013413432710145043 ),
 .UNSPECIFIED. ) ;
#28674 = ADVANCED_FACE ( 'NONE', ( #18530 ), #14916, .T. ) ;
#28675 = B_SPLINE_CURVE_WITH_KNOTS ( 'NONE', 3,
 ( #27482, #60670, #51903, #60069 ),
 .UNSPECIFIED., .F., .F.,
 ( 4, 4 ),
 ( 0.000000000000000000, 0.005004741218457404994 ),
 .UNSPECIFIED. ) ;
#28676 = CARTESIAN_POINT ( 'NONE',  ( 0.5819845901640493535, 38.27312528999471652, -28.79568196372230204 ) ) ;
#28677 = ORIENTED_EDGE ( 'NONE', *, *, #2905, .T. ) ;
#28678 = DIRECTION ( 'NONE',  ( -0.1024043820194934368, 0.4859385467930398272, 0.8679729669084597088 ) ) ;
#28679 = CARTESIAN_POINT ( 'NONE',  ( 0.3676999524040366896, 44.06746933160592050, 2.002181318165502599 ) ) ;
#28680 = EDGE_LOOP ( 'NONE', ( #55630, #16870, #48575, #35577 ) ) ;
#28681 = CARTESIAN_POINT ( 'NONE',  ( 1.227938101723756947, -37.58536632582764980, -20.72293514920789903 ) ) ;
#28682 = DIRECTION ( 'NONE',  ( -0.000000000000000000, 1.000000000000000000, 1.224646799147353207E-16 ) ) ;
#28683 = CARTESIAN_POINT ( 'NONE',  ( 0.8744876279028263033, -20.68330519280349122, 44.52584571550372061 ) ) ;
#28684 = CARTESIAN_POINT ( 'NONE',  ( 1.830465331921977912, -5.808636319045533902, -43.66504093655992591 ) ) ;
#28685 = ORIENTED_EDGE ( 'NONE', *, *, #47655, .T. ) ;
#28686 = ORIENTED_EDGE ( 'NONE', *, *, #51571, .F. ) ;
#28687 = CARTESIAN_POINT ( 'NONE',  ( 0.8551540677456715978, -17.49081417858818455, 44.61036085020945308 ) ) ;
#28688 = CARTESIAN_POINT ( 'NONE',  ( -6.017396004339687465, 17.40836349643167580, 7.212050743684241816 ) ) ;
#28689 = CARTESIAN_POINT ( 'NONE',  ( 4.956445790444036881, 42.27038699792232279, -20.75457619864872783 ) ) ;
#28690 = LINE ( 'NONE', #53408, #26455 ) ;
#28691 = VERTEX_POINT ( 'NONE', #8817 ) ;
#28692 = FACE_OUTER_BOUND ( 'NONE', #11208, .T. ) ;
#28693 = CIRCLE ( 'NONE', #58670, 42.92674063221959813 ) ;
#28694 = ORIENTED_EDGE ( 'NONE', *, *, #60517, .F. ) ;
#28695 = CARTESIAN_POINT ( 'NONE',  ( 5.880360259849739535, 45.44137230084860590, 15.37531919565251748 ) ) ;
#28696 = DIRECTION ( 'NONE',  ( 0.1011922191286468153, 0.08272061902647194487, -0.9914219253051130831 ) ) ;
#28697 = AXIS2_PLACEMENT_3D ( 'NONE', #26933, #2488, #36046 ) ;
#28698 = ORIENTED_EDGE ( 'NONE', *, *, #56199, .F. ) ;
#28699 = B_SPLINE_CURVE_WITH_KNOTS ( 'NONE', 3,
 ( #5233, #5837, #34392, #5534 ),
 .UNSPECIFIED., .F., .F.,
 ( 4, 4 ),
 ( 2.061695315165020171E-17, 0.004444306975806115029 ),
 .UNSPECIFIED. ) ;
#28700 = CARTESIAN_POINT ( 'NONE',  ( 0.1129192098497447394, 44.06201484046244587, 2.343210614524684487 ) ) ;
#28701 = AXIS2_PLACEMENT_3D ( 'NONE', #29, #14470, #10069 ) ;
#28702 = CARTESIAN_POINT ( 'NONE',  ( 0.6039202388192953519, 10.75760111029238786, -47.91490093072120260 ) ) ;
#28703 = CARTESIAN_POINT ( 'NONE',  ( 0.9756950546413942771, 26.04419981250937610, -34.10037081504532352 ) ) ;
#28704 = ORIENTED_EDGE ( 'NONE', *, *, #17684, .T. ) ;
#28705 = ADVANCED_FACE ( 'NONE', ( #47055 ), #48574, .F. ) ;
#28706 = CARTESIAN_POINT ( 'NONE',  ( 0.5838002273316436064, -18.20308624554797916, -44.30203797796956877 ) ) ;
#28707 = DIRECTION ( 'NONE',  ( 0.000000000000000000, 0.000000000000000000, 1.000000000000000000 ) ) ;
#28708 = CARTESIAN_POINT ( 'NONE',  ( 4.833616638992205949, 46.11947910922903304, 3.476827473558036008 ) ) ;
#28709 = CARTESIAN_POINT ( 'NONE',  ( 0.9730545539215883499, -36.90443313492345823, 21.89037132892422832 ) ) ;
#28710 = B_SPLINE_CURVE_WITH_KNOTS ( 'NONE', 3,
 ( #42680, #18553, #56131, #37681, #37064, #52355, #51121, #51425, #46457, #61431, #61741, #13869, #32976, #27639, #22951, #9447 ),
 .UNSPECIFIED., .F., .F.,
 ( 4, 3, 3, 3, 3, 4 ),
 ( 1.040890552917501732E-17, 0.0002724568934985535954, 0.0004086836638483777617, 0.0005449104342063600072, 0.0008173270854453693838, 0.001089761613562689659 ),
 .UNSPECIFIED. ) ;
#28711 = CARTESIAN_POINT ( 'NONE',  ( 0.8760168074887090262, 7.161346975773060564, 47.56749362999715913 ) ) ;
#28712 = VERTEX_POINT ( 'NONE', #9739 ) ;
#28713 = CIRCLE ( 'NONE', #5689, 47.91270532121795611 ) ;
#28714 = CARTESIAN_POINT ( 'NONE',  ( -6.078726893082806448, 5.482141236672210205, -18.45914864585846260 ) ) ;
#28715 = EDGE_CURVE ( 'NONE', #27427, #30264, #56151, .T. ) ;
#28716 = CARTESIAN_POINT ( 'NONE',  ( 2.009741617377216460, -16.56455318118139175, 40.80587770812996240 ) ) ;
#28717 = ORIENTED_EDGE ( 'NONE', *, *, #15938, .T. ) ;
#28718 = B_SPLINE_CURVE_WITH_KNOTS ( 'NONE', 3,
 ( #35061, #54116, #26876, #12482, #16876, #7433 ),
 .UNSPECIFIED., .F., .F.,
 ( 4, 2, 4 ),
 ( 6.149443329761888550E-18, 0.0002445244328975374566, 0.0004890488657950688416 ),
 .UNSPECIFIED. ) ;
#28719 = EDGE_CURVE ( 'NONE', #39423, #43333, #9777, .T. ) ;
#28720 = CARTESIAN_POINT ( 'NONE',  ( 3.238018933889920792, 6.194554405862312763, -11.87581525961332751 ) ) ;
#28721 = CARTESIAN_POINT ( 'NONE',  ( 0.3622758884714600280, 29.89648521331588071, 31.06363466427737663 ) ) ;
#28722 = CARTESIAN_POINT ( 'NONE',  ( 0.6067099128993260759, 18.98236771638461562, 43.97493306231469745 ) ) ;
#28723 = DIRECTION ( 'NONE',  ( -0.1011922191286467598, 0.9882612224441083004, -0.1144547552576855587 ) ) ;
#28724 = CARTESIAN_POINT ( 'NONE',  ( 1.231276596079887264, -6.136529359146732254, 41.46829847537028257 ) ) ;
#28725 = CARTESIAN_POINT ( 'NONE',  ( 0.1119898979215351448, -40.68569781727580903, 17.07733297014341645 ) ) ;
#28726 = VECTOR ( 'NONE', #53440, 1000.000000000000114 ) ;
#28727 = CARTESIAN_POINT ( 'NONE',  ( 0.5819845079324655890, -47.89381220525412175, 0.4540594263151432886 ) ) ;
#28728 = CARTESIAN_POINT ( 'NONE',  ( 36.00000000000000711, 9.192007254758536529E-15, 1.647756707073945522E-16 ) ) ;
#28729 = DIRECTION ( 'NONE',  ( 0.000000000000000000, 0.000000000000000000, -1.000000000000000000 ) ) ;
#28730 = CARTESIAN_POINT ( 'NONE',  ( 0.8760168074886960365, -46.68716261866184425, 11.58706983520244904 ) ) ;
#28731 = B_SPLINE_CURVE_WITH_KNOTS ( 'NONE', 3,
 ( #61529, #52143, #3903, #13338, #51831, #13968 ),
 .UNSPECIFIED., .F., .F.,
 ( 4, 2, 4 ),
 ( 0.000000000000000000, 0.0002293801035737094262, 0.0004587602071474188524 ),
 .UNSPECIFIED. ) ;
#28732 = DIRECTION ( 'NONE',  ( 0.07836865515943411409, -0.7860872967108184506, -0.6131273243286252672 ) ) ;
#28734 = VERTEX_POINT ( 'NONE', #19 ) ;
#28733 = DIRECTION ( 'NONE',  ( -1.000000000000000000, -0.000000000000000000, -0.000000000000000000 ) ) ;
#28735 = ORIENTED_EDGE ( 'NONE', *, *, #8085, .F. ) ;
#28736 = FACE_OUTER_BOUND ( 'NONE', #61478, .T. ) ;
#28737 = CARTESIAN_POINT ( 'NONE',  ( 0.3676999524040323597, 5.056646555325726489, -43.82215089355327109 ) ) ;
#28738 = LINE ( 'NONE', #9011, #1471 ) ;
#28739 = DIRECTION ( 'NONE',  ( -1.000000000000000000, -0.000000000000000000, -0.000000000000000000 ) ) ;
#28740 = CARTESIAN_POINT ( 'NONE',  ( 0.9762797500689124330, 10.20671408566037286, -40.64662068068250278 ) ) ;
#28741 = ORIENTED_EDGE ( 'NONE', *, *, #53858, .T. ) ;
#28742 = VECTOR ( 'NONE', #53847, 1000.000000000000114 ) ;
#28743 = AXIS2_PLACEMENT_3D ( 'NONE', #15390, #30080, #11610 ) ;
#28744 = CIRCLE ( 'NONE', #39783, 4.250000000000000000 ) ;
#28745 = CARTESIAN_POINT ( 'NONE',  ( 50.00005079999999680, 9.539392014169456147, 3.000000000000000000 ) ) ;
#28746 = ORIENTED_EDGE ( 'NONE', *, *, #53017, .F. ) ;
#28747 = B_SPLINE_CURVE_WITH_KNOTS ( 'NONE', 3,
 ( #13355, #32453, #61246, #47481, #34013, #53083, #38405, #24594, #9560, #57773, #19289, #61549, #56855, #43730, #18669, #779 ),
 .UNSPECIFIED., .F., .F.,
 ( 4, 3, 3, 3, 3, 4 ),
 ( 1.105939361823508950E-17, 0.0002732102107931894033, 0.0004098135523333801787, 0.0005464168938824981664, 0.0008195847345945439857, 0.001092771384553107867 ),
 .UNSPECIFIED. ) ;
#28748 = B_SPLINE_CURVE_WITH_KNOTS ( 'NONE', 3,
 ( #4781, #24532, #9505, #43358, #89, #29533 ),
 .UNSPECIFIED., .F., .F.,
 ( 4, 2, 4 ),
 ( 1.985955348410164766E-17, 0.0002448709889506577530, 0.0004897419779012956650 ),
 .UNSPECIFIED. ) ;
#28749 = CARTESIAN_POINT ( 'NONE',  ( 0.5830082357119567016, -25.00320994349359438, -39.67457028702288113 ) ) ;
#28750 = ORIENTED_EDGE ( 'NONE', *, *, #22794, .F. ) ;
#28751 = B_SPLINE_CURVE_WITH_KNOTS ( 'NONE', 3,
 ( #41963, #44134, #58169, #38489 ),
 .UNSPECIFIED., .F., .F.,
 ( 4, 4 ),
 ( 2.168404344971008868E-19, 0.004446298630425049407 ),
 .UNSPECIFIED. ) ;
#28752 =( BOUNDED_SURFACE ( )  B_SPLINE_SURFACE ( 3, 1, ( 
 ( #26510, #18368 ),
 ( #7382, #31846 ),
 ( #36867, #46261 ),
 ( #60945, #13358 ) ),
 .UNSPECIFIED., .F., .F., .F. ) 
 B_SPLINE_SURFACE_WITH_KNOTS ( ( 4, 4 ),
 ( 2, 2 ),
 ( 0.000000000000000000, 1.000000000000000000 ),
 ( 0.000000000000000000, 1.000000000000000000 ),
 .UNSPECIFIED. ) 
 GEOMETRIC_REPRESENTATION_ITEM ( )  RATIONAL_B_SPLINE_SURFACE ( (
 ( 1.000000000000000000, 1.000000000000000000),
 ( 0.9729067724841187204, 0.9999501103223794596),
 ( 0.9729067724841187204, 0.9999501103223794596),
 ( 1.000000000000000000, 1.000000000000000000) ) ) 
 REPRESENTATION_ITEM ( '' )  SURFACE ( )  );
#28753 = ADVANCED_FACE ( 'NONE', ( #953 ), #61007, .F. ) ;
#28754 = DIRECTION ( 'NONE',  ( 0.000000000000000000, 0.000000000000000000, -1.000000000000000000 ) ) ;
#28755 = VERTEX_POINT ( 'NONE', #29771 ) ;
#28756 = CARTESIAN_POINT ( 'NONE',  ( 4.975610109902397937, 35.53430708602585497, -33.61193875773584949 ) ) ;
#28757 = CARTESIAN_POINT ( 'NONE',  ( 0.6001305935487315502, -18.89378601236093758, 44.24520387813796418 ) ) ;
#28758 = ORIENTED_EDGE ( 'NONE', *, *, #19809, .F. ) ;
#28759 = CARTESIAN_POINT ( 'NONE',  ( 0.8557997880470690211, -24.73961900479222820, -41.02602466100805145 ) ) ;
#28760 = CARTESIAN_POINT ( 'NONE',  ( 3.240649175237396040, 2.400950397866095987, 43.92607829734675562 ) ) ;
#28761 = CARTESIAN_POINT ( 'NONE',  ( 1.827119703190779321, 27.17434071502558268, 33.38937793923695807 ) ) ;
#28762 = DIRECTION ( 'NONE',  ( 0.09835009131224567436, 0.9223318362920787106, -0.3736726418952223683 ) ) ;
#28763 = ORIENTED_EDGE ( 'NONE', *, *, #53666, .T. ) ;
#28764 = CARTESIAN_POINT ( 'NONE',  ( 0.6008122571543326185, -8.267105668410495767, -48.40670939376742865 ) ) ;
#28765 = ORIENTED_EDGE ( 'NONE', *, *, #29151, .F. ) ;
#28766 = LINE ( 'NONE', #18147, #17179 ) ;
#28767 = ORIENTED_EDGE ( 'NONE', *, *, #35153, .T. ) ;
#28768 = ORIENTED_EDGE ( 'NONE', *, *, #6330, .F. ) ;
#28769 = CARTESIAN_POINT ( 'NONE',  ( 4.553261556744875094, 0.000000000000000000, 0.000000000000000000 ) ) ;
#28770 = CARTESIAN_POINT ( 'NONE',  ( 0.5786265663353196143, 47.58023467411546648, -5.535668456753460198 ) ) ;
#28771 = CARTESIAN_POINT ( 'NONE',  ( 0.9756950546413930558, 34.10037081504560064, 26.04419981250898886 ) ) ;
#28772 = ORIENTED_EDGE ( 'NONE', *, *, #10926, .T. ) ;
#28773 = CARTESIAN_POINT ( 'NONE',  ( 0.5809828226811617480, -46.11980934799329646, -12.92184523170252497 ) ) ;
#28774 = CARTESIAN_POINT ( 'NONE',  ( 0.9730545539215883499, 10.61654491617622398, -41.57420493492374192 ) ) ;
#28775 = EDGE_CURVE ( 'NONE', #17561, #42072, #14459, .T. ) ;
#28776 = CARTESIAN_POINT ( 'NONE',  ( 0.6846871229502899947, -38.52803883689281150, -28.47437962186167582 ) ) ;
#28777 = ORIENTED_EDGE ( 'NONE', *, *, #42492, .F. ) ;
#28778 = EDGE_CURVE ( 'NONE', #42119, #10980, #58349, .T. ) ;
#28779 = ORIENTED_EDGE ( 'NONE', *, *, #19673, .T. ) ;
#28780 = CARTESIAN_POINT ( 'NONE',  ( 4.960386119450145515, 41.17653976845473096, -14.79625078758826895 ) ) ;
#28781 = DIRECTION ( 'NONE',  ( -1.000000000000000000, -1.836970198721027715E-16, 2.218671295934095703E-31 ) ) ;
#28782 = CARTESIAN_POINT ( 'NONE',  ( 0.9762797500689124330, 38.77779312671053447, -15.89363222827765831 ) ) ;
#28783 = CARTESIAN_POINT ( 'NONE',  ( 0.1092355843206037486, -34.39511076960621239, 26.01340835034354271 ) ) ;
#28784 = CARTESIAN_POINT ( 'NONE',  ( 0.7048096507298635682, 42.08020459959950443, 23.32077812596896393 ) ) ;
#28785 = ORIENTED_EDGE ( 'NONE', *, *, #21013, .F. ) ;
#28786 = EDGE_CURVE ( 'NONE', #22536, #55130, #5322, .T. ) ;
#28787 = ORIENTED_EDGE ( 'NONE', *, *, #53430, .T. ) ;
#28788 = CIRCLE ( 'NONE', #7760, 47.91270532121795611 ) ;
#28789 = CIRCLE ( 'NONE', #60646, 12.50000000000000000 ) ;
#28790 = EDGE_CURVE ( 'NONE', #31225, #51844, #53918, .T. ) ;
#28791 = CARTESIAN_POINT ( 'NONE',  ( 1.140000000000009006, 0.000000000000000000, 0.000000000000000000 ) ) ;
#28792 = CARTESIAN_POINT ( 'NONE',  ( 0.9780106845699496620, -41.13015066261051800, 8.040021948128993401 ) ) ;
#28793 = DIRECTION ( 'NONE',  ( 0.000000000000000000, 0.000000000000000000, 1.000000000000000000 ) ) ;
#28794 = CARTESIAN_POINT ( 'NONE',  ( 0.9745511491811764682, -21.74846188963803684, 36.98831798234368762 ) ) ;
#28795 = DIRECTION ( 'NONE',  ( 1.000000000000000000, 0.000000000000000000, 0.000000000000000000 ) ) ;
#28796 = DIRECTION ( 'NONE',  ( 0.09835009131224567436, -0.3736726418952255879, -0.9223318362920773783 ) ) ;
#28797 = ORIENTED_EDGE ( 'NONE', *, *, #39532, .T. ) ;
#28798 = CARTESIAN_POINT ( 'NONE',  ( -6.077587904424778920, -11.02178778841116547, -15.78975032548523139 ) ) ;
#28799 = CARTESIAN_POINT ( 'NONE',  ( 0.6000166863083106206, -8.353387137038740917, 48.39467331274394013 ) ) ;
#28801 = ADVANCED_FACE ( 'NONE', ( #20385 ), #21616, .T. ) ;
#28800 = CARTESIAN_POINT ( 'NONE',  ( 5.958863334805807099, 17.77634700750928687, -10.26176968287926528 ) ) ;
#28802 = TOROIDAL_SURFACE ( 'NONE', #60799, 15.38217999999999996, 0.05882000000000109363 ) ;
#28803 = DIRECTION ( 'NONE',  ( 0.000000000000000000, 0.000000000000000000, 1.000000000000000000 ) ) ;
#28804 = EDGE_CURVE ( 'NONE', #23782, #23477, #4852, .T. ) ;
#28805 = CARTESIAN_POINT ( 'NONE',  ( 4.975610109902397937, 0.000000000000000000, 0.000000000000000000 ) ) ;
#28806 = CARTESIAN_POINT ( 'NONE',  ( 5.896782393890504181, -7.222780579330736472, 18.77118876312459150 ) ) ;
#28807 =( BOUNDED_SURFACE ( )  B_SPLINE_SURFACE ( 3, 1, ( 
 ( #41651, #17221 ),
 ( #55712, #59810 ),
 ( #7165, #31619 ),
 ( #36039, #22534 ) ),
 .UNSPECIFIED., .F., .F., .F. ) 
 B_SPLINE_SURFACE_WITH_KNOTS ( ( 4, 4 ),
 ( 2, 2 ),
 ( 0.000000000000000000, 1.000000000000000000 ),
 ( 0.000000000000000000, 1.000000000000000000 ),
 .UNSPECIFIED. ) 
 GEOMETRIC_REPRESENTATION_ITEM ( )  RATIONAL_B_SPLINE_SURFACE ( (
 ( 1.000000000000000000, 1.000000000000000000),
 ( 0.7223157951917476005, 0.9931996967497186413),
 ( 0.7223157951917476005, 0.9931996967497186413),
 ( 1.000000000000000000, 1.000000000000000000) ) ) 
 REPRESENTATION_ITEM ( '' )  SURFACE ( )  );
#28808 = VERTEX_POINT ( 'NONE', #59502 ) ;
#28809 = CONICAL_SURFACE ( 'NONE', #44855, 42.92674063221959813, 1.485477209440487556 ) ;
#28810 = CARTESIAN_POINT ( 'NONE',  ( 4.000000000000003553, 2.309401076758524685, -0.3572655899081733644 ) ) ;
#28811 = CARTESIAN_POINT ( 'NONE',  ( 6.999999999999995559, 56.56854249492371878, 56.56854249492391062 ) ) ;
#28812 = CARTESIAN_POINT ( 'NONE',  ( 2.648799415243708655, 33.97949776740066596, 35.35408314134042485 ) ) ;
#28813 = CARTESIAN_POINT ( 'NONE',  ( 3.894904216938898323, 40.51735868841397092, 17.04312111646823880 ) ) ;
#28814 = CARTESIAN_POINT ( 'NONE',  ( 0.8751705887134553219, -23.27176129838455054, 42.09020928323333521 ) ) ;
#28815 = ORIENTED_EDGE ( 'NONE', *, *, #41326, .F. ) ;
#28816 = CARTESIAN_POINT ( 'NONE',  ( 4.958415959904820092, 8.053194174019305152, -44.70290837762330938 ) ) ;
#28817 = FACE_OUTER_BOUND ( 'NONE', #47056, .T. ) ;
#28818 = CARTESIAN_POINT ( 'NONE',  ( 5.901764892641307547, 19.78248028302040495, 44.79559064563818538 ) ) ;
#28819 =( BOUNDED_SURFACE ( )  B_SPLINE_SURFACE ( 3, 1, ( 
 ( #58200, #54418 ),
 ( #20628, #58815 ),
 ( #54109, #15324 ),
 ( #20030, #58500 ) ),
 .UNSPECIFIED., .F., .F., .F. ) 
 B_SPLINE_SURFACE_WITH_KNOTS ( ( 4, 4 ),
 ( 2, 2 ),
 ( 0.000000000000000000, 1.000000000000000000 ),
 ( 0.000000000000000000, 1.000000000000000000 ),
 .UNSPECIFIED. ) 
 GEOMETRIC_REPRESENTATION_ITEM ( )  RATIONAL_B_SPLINE_SURFACE ( (
 ( 1.000000000000000000, 1.000000000000000000),
 ( 0.9751682680413298332, 0.9999560080971552356),
 ( 0.9751682680413298332, 0.9999560080971552356),
 ( 1.000000000000000000, 1.000000000000000000) ) ) 
 REPRESENTATION_ITEM ( '' )  SURFACE ( )  );
#28820 = ORIENTED_EDGE ( 'NONE', *, *, #10090, .F. ) ;
#28821 = ADVANCED_FACE ( 'NONE', ( #44834 ), #20692, .T. ) ;
#28822 = DIRECTION ( 'NONE',  ( 0.07500201931887537365, 0.8838330717251207114, 0.4617507968840214860 ) ) ;
#28823 = ORIENTED_EDGE ( 'NONE', *, *, #54028, .T. ) ;
#28824 = CARTESIAN_POINT ( 'NONE',  ( 4.967162193818130511, -28.07411493385273715, -32.68434214048198072 ) ) ;
#28825 = CIRCLE ( 'NONE', #8842, 85.00000000000001421 ) ;
#28826 = ORIENTED_EDGE ( 'NONE', *, *, #51249, .T. ) ;
#28827 = CARTESIAN_POINT ( 'NONE',  ( 0.7057020205114981071, -17.55108080125414460, -44.57024707370732841 ) ) ;
#28828 = EDGE_LOOP ( 'NONE', ( #42173, #21731, #42711, #43202 ) ) ;
#28829 = CARTESIAN_POINT ( 'NONE',  ( 4.967162193818130511, 0.000000000000000000, 0.000000000000000000 ) ) ;
#28830 = CARTESIAN_POINT ( 'NONE',  ( 4.975610109902397937, 47.45567470742089000, 11.84940273605495520 ) ) ;
#28831 = EDGE_CURVE ( 'NONE', #16995, #29392, #60896, .T. ) ;
#28832 = VERTEX_POINT ( 'NONE', #21309 ) ;
#28833 = CARTESIAN_POINT ( 'NONE',  ( 4.963659409799331179, -20.22157859941701830, -39.92545197189572548 ) ) ;
#28834 = PRODUCT_DEFINITION_SHAPE ( 'NONE', 'NONE',  #61991 ) ;
#28835 = ORIENTED_EDGE ( 'NONE', *, *, #8594, .F. ) ;
#28836 = DIRECTION ( 'NONE',  ( 0.000000000000000000, 0.000000000000000000, 1.000000000000000000 ) ) ;
#28837 = CARTESIAN_POINT ( 'NONE',  ( 3.407937589446174087, -0.4592810312472936363, 13.69123696618924235 ) ) ;
#28838 = B_SPLINE_CURVE_WITH_KNOTS ( 'NONE', 3,
 ( #10319, #6195, #44480, #20642 ),
 .UNSPECIFIED., .F., .F.,
 ( 4, 4 ),
 ( 1.301042606982605128E-18, 0.004446298630425060683 ),
 .UNSPECIFIED. ) ;
#28839 = EDGE_LOOP ( 'NONE', ( #47508, #60966, #61401, #27982 ) ) ;
#28840 = FACE_OUTER_BOUND ( 'NONE', #37550, .T. ) ;
#28841 = AXIS2_PLACEMENT_3D ( 'NONE', #53891, #44240, #59214 ) ;
#28842 = CARTESIAN_POINT ( 'NONE',  ( 0.8551540677456739292, -7.157691013574685179, 47.37911285756618440 ) ) ;
#28843 = CARTESIAN_POINT ( 'NONE',  ( 0.7242003506639991262, 27.41645750814208427, -40.73511423612637827 ) ) ;
#28844 = ORIENTED_EDGE ( 'NONE', *, *, #23229, .T. ) ;
#28845 = CARTESIAN_POINT ( 'NONE',  ( 0.5839880159502346402, -33.83547574026603399, -33.89965136132180845 ) ) ;
#28846 = CARTESIAN_POINT ( 'NONE',  ( 0.1149546198390367924, -18.11085549359680158, 40.23609670822052209 ) ) ;
#28847 = VERTEX_POINT ( 'NONE', #30378 ) ;
#28848 = DIRECTION ( 'NONE',  ( 0.09835009131224552170, -0.9876177374393967368, -0.1222230102474975155 ) ) ;
#28849 = ORIENTED_EDGE ( 'NONE', *, *, #57668, .T. ) ;
#28850 = PRESENTATION_LAYER_ASSIGNMENT (  '', '', ( #48840 ) ) ;
#28851 = CARTESIAN_POINT ( 'NONE',  ( 1.231276596079887264, 25.54232633153331733, 33.23952972879620660 ) ) ;
#28852 = CARTESIAN_POINT ( 'NONE',  ( 5.960721111146673579, 0.006321279846820317821, -20.52557019979492026 ) ) ;
#28853 = EDGE_LOOP ( 'NONE', ( #13886, #46651, #54681, #30274 ) ) ;
#28854 = CARTESIAN_POINT ( 'NONE',  ( 0.9780303403264780648, -34.73352412603711770, -23.45041396609195772 ) ) ;
#28855 = CARTESIAN_POINT ( 'NONE',  ( 0.1156495703730067576, 25.13225202099905786, -36.26724226604579826 ) ) ;
#28856 = CARTESIAN_POINT ( 'NONE',  ( 0.6001305935487422083, 47.76436356026960084, 5.760103278698182727 ) ) ;
#28857 = CARTESIAN_POINT ( 'NONE',  ( 0.1310142868023672913, -40.08041389954892253, 15.91230901232153627 ) ) ;
#28858 = ADVANCED_FACE ( 'NONE', ( #30693 ), #31385, .F. ) ;
#28859 = ORIENTED_EDGE ( 'NONE', *, *, #2519, .T. ) ;
#28860 = CARTESIAN_POINT ( 'NONE',  ( 0.6017666602106489515, 18.08695057064592859, -44.57804174182703605 ) ) ;
#28861 = EDGE_CURVE ( 'NONE', #59386, #34059, #16001, .T. ) ;
#28862 = CARTESIAN_POINT ( 'NONE',  ( 0.5987334363312690755, -25.97268459165310261, 41.67712276026960438 ) ) ;
#28863 = CARTESIAN_POINT ( 'NONE',  ( 0.5827359174754822568, -44.10985444762171426, -18.66406616558025888 ) ) ;
#28864 = CARTESIAN_POINT ( 'NONE',  ( 0.5850706913938533704, 38.10903744847180974, -29.01314519953759685 ) ) ;
#28865 = B_SPLINE_CURVE_WITH_KNOTS ( 'NONE', 3,
 ( #58610, #14813, #6594, #33925 ),
 .UNSPECIFIED., .F., .F.,
 ( 4, 4 ),
 ( 6.938893903907228378E-18, 0.005013413432710140706 ),
 .UNSPECIFIED. ) ;
#28866 = CARTESIAN_POINT ( 'NONE',  ( 2.185380717157383579, -8.443826973212180675, -43.21483066163343523 ) ) ;
#28867 = CIRCLE ( 'NONE', #41917, 2.649999999999997691 ) ;
#28868 = DIRECTION ( 'NONE',  ( 1.000000000000000000, 0.000000000000000000, 0.000000000000000000 ) ) ;
#28869 = VECTOR ( 'NONE', #87, 1000.000000000000114 ) ;
#28870 = CARTESIAN_POINT ( 'NONE',  ( 2.282816707992309624, -33.94297373141591123, 32.47108714959165354 ) ) ;
#28871 = LINE ( 'NONE', #47996, #13416 ) ;
#28872 = CARTESIAN_POINT ( 'NONE',  ( 0.9757787079277441267, 30.36877398309943388, -30.31292661677461098 ) ) ;
#28873 = EDGE_CURVE ( 'NONE', #36274, #48937, #55112, .T. ) ;
#28874 = CARTESIAN_POINT ( 'NONE',  ( 0.1092355843206037486, -21.82203846347354670, 37.19569459163097491 ) ) ;
#28875 = CARTESIAN_POINT ( 'NONE',  ( 4.553261556744875094, 0.000000000000000000, 0.000000000000000000 ) ) ;
#28876 = CARTESIAN_POINT ( 'NONE',  ( 4.553261556744875094, 0.000000000000000000, 0.000000000000000000 ) ) ;
#28877 = CARTESIAN_POINT ( 'NONE',  ( 0.7413678028165012757, -22.05608674998674701, 38.18396429192890196 ) ) ;
#28878 = CARTESIAN_POINT ( 'NONE',  ( 0.7242003506639991262, -45.81453560520021995, -17.66465401319446116 ) ) ;
#28879 = CARTESIAN_POINT ( 'NONE',  ( 0.5806925824938494740, 45.08220210717442455, -12.91578164539189721 ) ) ;
#28880 = LINE ( 'NONE', #23265, #36187 ) ;
#28881 = ORIENTED_EDGE ( 'NONE', *, *, #54993, .T. ) ;
#28882 = AXIS2_PLACEMENT_3D ( 'NONE', #54948, #7324, #26452 ) ;
#28883 = DIRECTION ( 'NONE',  ( -1.000000000000000000, -1.836909530733573776E-16, -1.361838123766432833E-32 ) ) ;
#28884 = CARTESIAN_POINT ( 'NONE',  ( 4.691466044806103852, -40.13652286047880580, -19.42108863068366631 ) ) ;
#28885 = FACE_OUTER_BOUND ( 'NONE', #48639, .T. ) ;
#28886 = ORIENTED_EDGE ( 'NONE', *, *, #40061, .T. ) ;
#28887 = CARTESIAN_POINT ( 'NONE',  ( 0.9756354156337447847, 5.471460801653407202, 42.55820231551292920 ) ) ;
#28888 = CARTESIAN_POINT ( 'NONE',  ( 5.959828726073459926, -16.28681682518072549, 12.49160845136007580 ) ) ;
#28889 =( GEOMETRIC_REPRESENTATION_CONTEXT ( 3 ) GLOBAL_UNCERTAINTY_ASSIGNED_CONTEXT ( ( #27357 ) ) GLOBAL_UNIT_ASSIGNED_CONTEXT ( ( #24648, #52837, #48443 ) ) REPRESENTATION_CONTEXT ( 'NONE', 'WORKASPACE' ) );
#28890 = ORIENTED_EDGE ( 'NONE', *, *, #52462, .T. ) ;
#28891 = ORIENTED_EDGE ( 'NONE', *, *, #46428, .T. ) ;
#28892 = CARTESIAN_POINT ( 'NONE',  ( -31.75000000000000000, 16.00000000000000000, 0.000000000000000000 ) ) ;
#28894 = EDGE_LOOP ( 'NONE', ( #12679, #50678, #43128, #53152 ) ) ;
#28893 =( BOUNDED_SURFACE ( )  B_SPLINE_SURFACE ( 3, 1, ( 
 ( #24646, #52834 ),
 ( #29333, #38455 ),
 ( #43785, #15558 ),
 ( #24958, #44095 ) ),
 .UNSPECIFIED., .F., .F., .F. ) 
 B_SPLINE_SURFACE_WITH_KNOTS ( ( 4, 4 ),
 ( 2, 2 ),
 ( 0.000000000000000000, 1.000000000000000000 ),
 ( 0.000000000000000000, 1.000000000000000000 ),
 .UNSPECIFIED. ) 
 GEOMETRIC_REPRESENTATION_ITEM ( )  RATIONAL_B_SPLINE_SURFACE ( (
 ( 1.000000000000000000, 1.000000000000000000),
 ( 0.9953040768229005630, 0.8617119497784937465),
 ( 0.9953040768229005630, 0.8617119497784937465),
 ( 1.000000000000000000, 1.000000000000000000) ) ) 
 REPRESENTATION_ITEM ( '' )  SURFACE ( )  );
#28895 = CARTESIAN_POINT ( 'NONE',  ( -6.016104459813371719, -9.416989654584419611, 16.32137543786079803 ) ) ;
#28896 = ORIENTED_EDGE ( 'NONE', *, *, #44101, .F. ) ;
#28897 = ADVANCED_FACE ( 'NONE', ( #12237 ), #18220, .F. ) ;
#28898 = EDGE_LOOP ( 'NONE', ( #15977, #54422, #5410, #40001 ) ) ;
#28899 = CARTESIAN_POINT ( 'NONE',  ( 0.6000166863083106206, 44.47108027094632376, -20.83618250168447972 ) ) ;
#28900 = ORIENTED_EDGE ( 'NONE', *, *, #14823, .T. ) ;
#28901 = CARTESIAN_POINT ( 'NONE',  ( 4.291220156522059348, 8.814262783202863716, 46.27848062430680898 ) ) ;
#28902 = CARTESIAN_POINT ( 'NONE',  ( 4.975610109902397937, 38.85236532789286201, -29.71435874397630528 ) ) ;
#28903 = ADVANCED_FACE ( 'NONE', ( #54803 ), #44222, .F. ) ;
#28904 = CARTESIAN_POINT ( 'NONE',  ( 0.1103878639767399417, -30.52789484587433222, -30.45925431905102698 ) ) ;
#28905 = ORIENTED_EDGE ( 'NONE', *, *, #23967, .F. ) ;
#28906 = CARTESIAN_POINT ( 'NONE',  ( 0.6000166863083090663, 27.66667954482571545, 40.57558779207488442 ) ) ;
#28907 = B_SPLINE_CURVE_WITH_KNOTS ( 'NONE', 3,
 ( #38403, #47790, #4835, #57449 ),
 .UNSPECIFIED., .F., .F.,
 ( 4, 4 ),
 ( 2.365306999241824718E-17, 0.004564976165746187711 ),
 .UNSPECIFIED. ) ;
#28908 = CARTESIAN_POINT ( 'NONE',  ( 0.9790320750461911636, -39.61794717384558595, 13.66584773340351688 ) ) ;
#28909 = ORIENTED_EDGE ( 'NONE', *, *, #20307, .F. ) ;
#28910 = EDGE_CURVE ( 'NONE', #24624, #45383, #41992, .T. ) ;
#28911 = ORIENTED_EDGE ( 'NONE', *, *, #17167, .F. ) ;
#28912 =( BOUNDED_SURFACE ( )  B_SPLINE_SURFACE ( 3, 1, ( 
 ( #5888, #40096 ),
 ( #907, #54125 ),
 ( #10949, #20043 ),
 ( #59144, #45095 ) ),
 .UNSPECIFIED., .F., .F., .F. ) 
 B_SPLINE_SURFACE_WITH_KNOTS ( ( 4, 4 ),
 ( 2, 2 ),
 ( 0.000000000000000000, 1.000000000000000000 ),
 ( 0.000000000000000000, 1.000000000000000000 ),
 .UNSPECIFIED. ) 
 GEOMETRIC_REPRESENTATION_ITEM ( )  RATIONAL_B_SPLINE_SURFACE ( (
 ( 1.000000000000000000, 1.000000000000000000),
 ( 0.9953040768229005630, 0.8617119497784937465),
 ( 0.9953040768229005630, 0.8617119497784937465),
 ( 1.000000000000000000, 1.000000000000000000) ) ) 
 REPRESENTATION_ITEM ( '' )  SURFACE ( )  );
#28913 = CARTESIAN_POINT ( 'NONE',  ( -2.708315649062916552, -5.356004933109549171, 13.61924161399624822 ) ) ;
#28914 = CIRCLE ( 'NONE', #22943, 43.92652462719577500 ) ;
#28915 = VERTEX_POINT ( 'NONE', #14477 ) ;
#28916 = CARTESIAN_POINT ( 'NONE',  ( 2.281448460670567613, 34.83871297539704415, 32.98023336626246049 ) ) ;
#28917 = CARTESIAN_POINT ( 'NONE',  ( 3.270143674763207553, 8.548517033725413938, -10.69018354892878264 ) ) ;
#28918 = CARTESIAN_POINT ( 'NONE',  ( 0.5850706913938534814, -38.10903744847121288, -29.01314519953837845 ) ) ;
#28919 = DIRECTION ( 'NONE',  ( -1.000000000000000000, -1.836909530733573776E-16, 2.465190328815682145E-32 ) ) ;
#28920 =( BOUNDED_SURFACE ( )  B_SPLINE_SURFACE ( 3, 1, ( 
 ( #27754, #45964 ),
 ( #60947, #18370 ),
 ( #8026, #41259 ),
 ( #3008, #12751 ) ),
 .UNSPECIFIED., .F., .F., .F. ) 
 B_SPLINE_SURFACE_WITH_KNOTS ( ( 4, 4 ),
 ( 2, 2 ),
 ( 0.000000000000000000, 1.000000000000000000 ),
 ( 0.000000000000000000, 1.000000000000000000 ),
 .UNSPECIFIED. ) 
 GEOMETRIC_REPRESENTATION_ITEM ( )  RATIONAL_B_SPLINE_SURFACE ( (
 ( 1.000000000000000000, 1.000000000000000000),
 ( 0.9953040768229005630, 0.8617119497784937465),
 ( 0.9953040768229005630, 0.8617119497784937465),
 ( 1.000000000000000000, 1.000000000000000000) ) ) 
 REPRESENTATION_ITEM ( '' )  SURFACE ( )  );
#28921 = ORIENTED_EDGE ( 'NONE', *, *, #61075, .T. ) ;
#28922 = CARTESIAN_POINT ( 'NONE',  ( 0.6027935024548037868, -12.61964268015589141, 46.42277558035020490 ) ) ;
#28923 = CARTESIAN_POINT ( 'NONE',  ( 3.270143674763207553, 8.113405361969672214, -11.02405647745161410 ) ) ;
#28924 = CARTESIAN_POINT ( 'NONE',  ( 4.291220156522059348, -23.50705364442096013, -40.82655295593802691 ) ) ;
#28925 = ORIENTED_EDGE ( 'NONE', *, *, #45565, .F. ) ;
#28926 = CARTESIAN_POINT ( 'NONE',  ( 4.956445790444004018, -45.27177431812791042, 12.96165499572219737 ) ) ;
#28927 = CARTESIAN_POINT ( 'NONE',  ( 4.335381028904216727, -32.17603896083203807, -36.93858909670704094 ) ) ;
#28928 = DIRECTION ( 'NONE',  ( 0.1736481776669315802, -0.9848077530122079093, 5.551115123125782702E-17 ) ) ;
#28929 = ADVANCED_FACE ( 'NONE', ( #43930, #970 ), #33584, .F. ) ;
#28930 = VECTOR ( 'NONE', #3842, 1000.000000000000000 ) ;
#28931 = ORIENTED_EDGE ( 'NONE', *, *, #61718, .F. ) ;
#28932 = VERTEX_POINT ( 'NONE', #53574 ) ;
#28933 = DIRECTION ( 'NONE',  ( 0.000000000000000000, 0.000000000000000000, -1.000000000000000000 ) ) ;
#28934 = DIRECTION ( 'NONE',  ( 0.000000000000000000, 0.000000000000000000, -1.000000000000000000 ) ) ;
#28935 = EDGE_CURVE ( 'NONE', #37380, #16660, #53154, .T. ) ;
#28936 = CARTESIAN_POINT ( 'NONE',  ( 4.956653778116999476, 43.37017594958085454, -20.77844580450516077 ) ) ;
#28937 = B_SPLINE_CURVE_WITH_KNOTS ( 'NONE', 3,
 ( #25321, #49744, #11546, #35055, #15020, #20631 ),
 .UNSPECIFIED., .F., .F.,
 ( 4, 2, 4 ),
 ( 5.275955480050202716E-18, 0.0002445244328975366434, 0.0004890488657950680827 ),
 .UNSPECIFIED. ) ;
#28938 = CARTESIAN_POINT ( 'NONE',  ( 0.8554163680231720024, 27.08908797599197982, -38.30648490452740162 ) ) ;
#28939 = CARTESIAN_POINT ( 'NONE',  ( 4.549368137175248350, 0.000000000000000000, 0.000000000000000000 ) ) ;
#28940 = EDGE_CURVE ( 'NONE', #22273, #5676, #25092, .T. ) ;
#28941 = CARTESIAN_POINT ( 'NONE',  ( 0.1156867017252034557, -31.78337558606124347, 30.60653269533405663 ) ) ;
#28942 = VECTOR ( 'NONE', #56667, 1000.000000000000114 ) ;
#28943 =( NAMED_UNIT ( * ) PLANE_ANGLE_UNIT ( ) SI_UNIT ( $, .RADIAN. ) );
#28944 = CARTESIAN_POINT ( 'NONE',  ( 0.8753041380234471980, 37.96023374381077531, -31.14737520222577416 ) ) ;
#28945 = CARTESIAN_POINT ( 'NONE',  ( 4.553261556744873317, -39.47791437445913942, 19.26223877088302672 ) ) ;
#28946 = CARTESIAN_POINT ( 'NONE',  ( 5.901764892641307547, -48.07448765165377580, 9.318535532510814789 ) ) ;
#28947 = CARTESIAN_POINT ( 'NONE',  ( 4.962356264823608143, 6.570263404306589727, 41.57002810511892221 ) ) ;
#28948 = PLANE ( 'NONE',  #51861 ) ;
#28949 = VERTEX_POINT ( 'NONE', #47990 ) ;
#28950 = CARTESIAN_POINT ( 'NONE',  ( 0.8560838555295223751, -46.73345513967318965, 4.044379407262076676 ) ) ;
#28951 = CARTESIAN_POINT ( 'NONE',  ( 0.1103878639767399694, -34.24245495763003788, -26.21398130517505365 ) ) ;
#28952 = CARTESIAN_POINT ( 'NONE',  ( 0.5806925824938499181, -45.84420715090598009, -9.875780123533834498 ) ) ;
#28953 = FACE_OUTER_BOUND ( 'NONE', #31882, .T. ) ;
#28954 = ADVANCED_FACE ( 'NONE', ( #11874 ), #44927, .F. ) ;
#28955 = CARTESIAN_POINT ( 'NONE',  ( 4.322998006666179727, -16.38761975793238790, 45.10383234877005521 ) ) ;
#28956 = CARTESIAN_POINT ( 'NONE',  ( 0.6023143664670691511, -46.53533348215000132, 12.19804739160180951 ) ) ;
#28957 = LINE ( 'NONE', #51590, #15632 ) ;
#28958 = FACE_OUTER_BOUND ( 'NONE', #35752, .T. ) ;
#28959 = CIRCLE ( 'NONE', #1933, 48.91267123290010943 ) ;
#28960 = CARTESIAN_POINT ( 'NONE',  ( 0.6026112563231247332, 48.23484943966749228, -9.216305899698413739 ) ) ;
#28961 = CARTESIAN_POINT ( 'NONE',  ( 0.9757402383260965761, -11.18751708556339253, 41.42435672089863630 ) ) ;
#28962 = CARTESIAN_POINT ( 'NONE',  ( 0.000000000000000000, 0.000000000000000000, -25.03750572909317285 ) ) ;
#28963 = CARTESIAN_POINT ( 'NONE',  ( 4.549368137175248350, -42.14271863032827525, -8.166781970325585505 ) ) ;
#28965 = ORIENTED_EDGE ( 'NONE', *, *, #29706, .F. ) ;
#28964 = CARTESIAN_POINT ( 'NONE',  ( 0.8751705887134553219, -19.22545746485630502, -44.08562551107074512 ) ) ;
#28966 = ORIENTED_EDGE ( 'NONE', *, *, #7899, .T. ) ;
#28967 = CIRCLE ( 'NONE', #17982, 2.649999999999999467 ) ;
#28968 = CARTESIAN_POINT ( 'NONE',  ( 0.1087620492084205998, -43.12302841504342155, -0.3620418170785275058 ) ) ;
#28969 = CARTESIAN_POINT ( 'NONE',  ( 0.5806925824938502512, 46.40146083665138832, -6.791670970259978013 ) ) ;
#28970 = CARTESIAN_POINT ( 'NONE',  ( 0.1073791018717483448, -11.62916352156123168, -41.52698815987163528 ) ) ;
#28971 = B_SPLINE_CURVE_WITH_KNOTS ( 'NONE', 3,
 ( #13490, #37302, #28186, #23188 ),
 .UNSPECIFIED., .F., .F.,
 ( 4, 4 ),
 ( 0.000000000000000000, 0.005014147105413699519 ),
 .UNSPECIFIED. ) ;
#28972 = ORIENTED_EDGE ( 'NONE', *, *, #50146, .F. ) ;
#28973 = CARTESIAN_POINT ( 'NONE',  ( 4.967162193818130511, 40.65506779172185503, -14.26841313271238221 ) ) ;
#28974 = CARTESIAN_POINT ( 'NONE',  ( 4.999999999999998224, -2.649999999999153921, -80.00000000000004263 ) ) ;
#28975 = CARTESIAN_POINT ( 'NONE',  ( 0.8557997880470697982, 24.73961900479251952, 41.02602466100786671 ) ) ;
#28976 = ORIENTED_EDGE ( 'NONE', *, *, #29594, .F. ) ;
#28977 = ORIENTED_EDGE ( 'NONE', *, *, #60740, .T. ) ;
#28978 = CARTESIAN_POINT ( 'NONE',  ( -2.601141883200662974, 10.36212650428623228, 10.74345204199085302 ) ) ;
#28979 = EDGE_CURVE ( 'NONE', #4433, #51079, #57969, .T. ) ;
#28980 = CIRCLE ( 'NONE', #38047, 42.08604991992415023 ) ;
#28981 = CARTESIAN_POINT ( 'NONE',  ( 4.967162193818130511, 0.000000000000000000, 0.000000000000000000 ) ) ;
#28982 = CARTESIAN_POINT ( 'NONE',  ( 0.5835226383429285013, 16.68471544554396147, -43.82764818065410140 ) ) ;
#28983 = ADVANCED_FACE ( 'NONE', ( #20103 ), #1351, .F. ) ;
#28984 = ADVANCED_FACE ( 'NONE', ( #45384 ), #7768, .F. ) ;
#28985 = CARTESIAN_POINT ( 'NONE',  ( 2.282816707992308292, -12.65678178881115734, 45.23607897639210762 ) ) ;
#28986 = B_SPLINE_CURVE_WITH_KNOTS ( 'NONE', 3,
 ( #38545, #57597, #14730, #33846, #52922, #10026, #29120, #5589, #24734, #48239, #43875, #917, #48845, #16898, #31287, #12504 ),
 .UNSPECIFIED., .F., .F.,
 ( 4, 3, 3, 3, 3, 4 ),
 ( 2.194378057379452319E-17, 0.0002612764279487753854, 0.0003919131003184781609, 0.0005225497727000660148, 0.0007837925190632443785, 0.001045051706266714783 ),
 .UNSPECIFIED. ) ;
#28987 = CARTESIAN_POINT ( 'NONE',  ( 0.9754402186311934564, 42.56545569314712907, 5.414674803233914702 ) ) ;
#28988 = ORIENTED_EDGE ( 'NONE', *, *, #11385, .T. ) ;
#28989 = EDGE_CURVE ( 'NONE', #54909, #7563, #22504, .T. ) ;
#28990 = EDGE_CURVE ( 'NONE', #3915, #37874, #14786, .T. ) ;
#28991 = ORIENTED_EDGE ( 'NONE', *, *, #13986, .T. ) ;
#28992 = CARTESIAN_POINT ( 'NONE',  ( 4.962356264823600149, -32.75738977283805298, 26.42326651140453109 ) ) ;
#28993 = CARTESIAN_POINT ( 'NONE',  ( 1.657374760986086271, 44.02697161945633297, 1.586258891804838367 ) ) ;
#28994 = ORIENTED_EDGE ( 'NONE', *, *, #26094, .F. ) ;
#28995 = CARTESIAN_POINT ( 'NONE',  ( 0.9772918015221174759, -37.58957372490684179, -18.52999738074653635 ) ) ;
#28996 = DIRECTION ( 'NONE',  ( 0.09835009131224553558, 0.5996571005210405980, -0.7941905447268757801 ) ) ;
#28997 = CARTESIAN_POINT ( 'NONE',  ( 0.6025881611877911270, 46.41131722377291169, 12.66175293297418492 ) ) ;
#28998 = CARTESIAN_POINT ( 'NONE',  ( 3.782625744892853970, -8.686979669181580377, -41.13118632281627640 ) ) ;
#28999 = ORIENTED_EDGE ( 'NONE', *, *, #52664, .T. ) ;
#29000 = ORIENTED_EDGE ( 'NONE', *, *, #43914, .T. ) ;
#29001 = CARTESIAN_POINT ( 'NONE',  ( 0.5837800304671227902, 46.48363954360758754, -6.205528741328782516 ) ) ;
#29002 = CARTESIAN_POINT ( 'NONE',  ( 0.9745511491811751359, -42.49552597049454761, -5.938142320543777330 ) ) ;
#29003 = CARTESIAN_POINT ( 'NONE',  ( 0.3622758884714730732, 41.85013935980087751, 10.35929834645937397 ) ) ;
#29004 =( BOUNDED_SURFACE ( )  B_SPLINE_SURFACE ( 3, 1, ( 
 ( #23869, #28556 ),
 ( #19185, #29177 ),
 ( #10080, #4414 ),
 ( #42999, #341 ) ),
 .UNSPECIFIED., .F., .F., .F. ) 
 B_SPLINE_SURFACE_WITH_KNOTS ( ( 4, 4 ),
 ( 2, 2 ),
 ( 0.000000000000000000, 1.000000000000000000 ),
 ( 0.000000000000000000, 1.000000000000000000 ),
 .UNSPECIFIED. ) 
 GEOMETRIC_REPRESENTATION_ITEM ( )  RATIONAL_B_SPLINE_SURFACE ( (
 ( 1.000000000000000000, 1.000000000000000000),
 ( 0.9953040768229005630, 0.8617119497784937465),
 ( 0.9953040768229005630, 0.8617119497784937465),
 ( 1.000000000000000000, 1.000000000000000000) ) ) 
 REPRESENTATION_ITEM ( '' )  SURFACE ( )  );
#29005 = CARTESIAN_POINT ( 'NONE',  ( 0.5839880159502331969, 29.12121614504463096, 38.02605095487687947 ) ) ;
#29006 = ORIENTED_EDGE ( 'NONE', *, *, #32836, .F. ) ;
#29007 = CARTESIAN_POINT ( 'NONE',  ( 0.6026112563231248442, 4.888769112786662596, -48.86349282916715708 ) ) ;
#29008 = ORIENTED_EDGE ( 'NONE', *, *, #60609, .F. ) ;
#29009 = CARTESIAN_POINT ( 'NONE',  ( 1.231276596079881935, 38.91607545535268997, -15.58254928345689017 ) ) ;
#29010 = CARTESIAN_POINT ( 'NONE',  ( 0.1157991065609915715, 9.739164777550831431, 43.03592725820383436 ) ) ;
#29011 = EDGE_CURVE ( 'NONE', #19785, #57948, #19795, .T. ) ;
#29012 = CIRCLE ( 'NONE', #7991, 2.041999999999999815 ) ;
#29013 = ORIENTED_EDGE ( 'NONE', *, *, #4062, .F. ) ;
#29014 = CARTESIAN_POINT ( 'NONE',  ( 50.50000000000000000, 0.000000000000000000, 2.649999999999992806 ) ) ;
#29015 = LINE ( 'NONE', #15540, #48776 ) ;
#29016 = B_SPLINE_CURVE_WITH_KNOTS ( 'NONE', 3,
 ( #58249, #58876, #25069, #44213 ),
 .UNSPECIFIED., .F., .F.,
 ( 4, 4 ),
 ( 7.919159918457849946E-17, 0.005004741218457501271 ),
 .UNSPECIFIED. ) ;
#29017 = CARTESIAN_POINT ( 'NONE',  ( 4.833616638992205949, -25.31740731790869248, -38.70560126501854370 ) ) ;
#29018 = ORIENTED_EDGE ( 'NONE', *, *, #56798, .T. ) ;
#29019 = ADVANCED_FACE ( 'NONE', ( #38296 ), #44579, .F. ) ;
#29020 = CARTESIAN_POINT ( 'NONE',  ( 0.8751705887134423323, 47.79200036674280483, -5.393078191592203474 ) ) ;
#29021 = CARTESIAN_POINT ( 'NONE',  ( 0.1313383488274133815, 26.75504982351763061, 33.82021892231554716 ) ) ;
#29022 = CARTESIAN_POINT ( 'NONE',  ( 2.648799415243696664, -36.17482712903065334, 33.10437048902073798 ) ) ;
#29023 = CARTESIAN_POINT ( 'NONE',  ( 2.301529144917015213, 11.18385659262678189, -46.71331407887427645 ) ) ;
#29024 = ORIENTED_EDGE ( 'NONE', *, *, #687, .T. ) ;
#29025 = CARTESIAN_POINT ( 'NONE',  ( 0.9749527285493297946, 39.75066842359309760, -16.15611883305602703 ) ) ;
#29026 = CARTESIAN_POINT ( 'NONE',  ( 0.5782707292762423457, -46.10024953908492762, -8.631532085424908018 ) ) ;
#29027 = CARTESIAN_POINT ( 'NONE',  ( 0.5832655196449155754, 28.00069848097898273, -37.61909179593025954 ) ) ;
#29028 = CIRCLE ( 'NONE', #55030, 5.633200000000004870 ) ;
#29029 = ORIENTED_EDGE ( 'NONE', *, *, #22923, .T. ) ;
#29030 = DIRECTION ( 'NONE',  ( 1.000000000000000000, 0.000000000000000000, 0.000000000000000000 ) ) ;
#29031 = DIRECTION ( 'NONE',  ( 0.000000000000000000, 0.000000000000000000, -1.000000000000000000 ) ) ;
#29032 = DIRECTION ( 'NONE',  ( -1.000000000000000000, 0.000000000000000000, 0.000000000000000000 ) ) ;
#29033 = CARTESIAN_POINT ( 'NONE',  ( 5.960721111146673579, 2.685391721745764571, 20.34914600876576074 ) ) ;
#29034 = ADVANCED_FACE ( 'NONE', ( #35987 ), #26993, .F. ) ;
#29035 = B_SPLINE_CURVE_WITH_KNOTS ( 'NONE', 3,
 ( #20176, #40774, #31650, #55129 ),
 .UNSPECIFIED., .F., .F.,
 ( 4, 4 ),
 ( 0.000000000000000000, 0.004442905043737216571 ),
 .UNSPECIFIED. ) ;
#29036 = CARTESIAN_POINT ( 'NONE',  ( 0.8753041380234471980, -13.11588273819783268, -47.31925557181583741 ) ) ;
#29037 = CARTESIAN_POINT ( 'NONE',  ( 0.6026777506516368677, -19.71849354655656228, 44.97474183240662171 ) ) ;
#29038 = CARTESIAN_POINT ( 'NONE',  ( 0.7048096507298635682, -11.63498350884368904, 46.68221792389220326 ) ) ;
#29039 = DIRECTION ( 'NONE',  ( -2.775557570403182199E-17, -0.6377407717913610163, 0.7702510681556756778 ) ) ;
#29040 = CARTESIAN_POINT ( 'NONE',  ( 0.3676999524040366896, 39.37931578713023839, -19.88014264185028068 ) ) ;
#29041 = ADVANCED_FACE ( 'NONE', ( #8068 ), #12176, .F. ) ;
#29042 = CARTESIAN_POINT ( 'NONE',  ( 4.553261556744875094, 0.000000000000000000, 0.000000000000000000 ) ) ;
#29043 = CARTESIAN_POINT ( 'NONE',  ( 0.1064266418746778187, -26.69589626339737265, 33.86837517279499821 ) ) ;
#29045 = EDGE_LOOP ( 'NONE', ( #24443, #20726, #59866, #18309 ) ) ;
#29044 = CARTESIAN_POINT ( 'NONE',  ( 3.238931869106854045, 19.89273896137483533, -38.11291514434422822 ) ) ;
#29046 = ORIENTED_EDGE ( 'NONE', *, *, #56062, .T. ) ;
#29047 = LINE ( 'NONE', #48159, #34526 ) ;
#29048 = CARTESIAN_POINT ( 'NONE',  ( -2.739355103387248747, 8.323596231104431808, -12.39214722041991834 ) ) ;
#29049 = FACE_OUTER_BOUND ( 'NONE', #20629, .T. ) ;
#29050 = FACE_OUTER_BOUND ( 'NONE', #26004, .T. ) ;
#29051 = ORIENTED_EDGE ( 'NONE', *, *, #21251, .T. ) ;
#29052 = CARTESIAN_POINT ( 'NONE',  ( 5.894904586330512508, 5.957793302349398523, 19.21026056637763091 ) ) ;
#29053 = CARTESIAN_POINT ( 'NONE',  ( -6.010958268070873523, 11.48268200989218890, -14.94067681728537522 ) ) ;
#29054 = FACE_OUTER_BOUND ( 'NONE', #21554, .T. ) ;
#29055 = VERTEX_POINT ( 'NONE', #36914 ) ;
#29056 = EDGE_CURVE ( 'NONE', #15399, #7691, #50883, .T. ) ;
#29057 = B_SPLINE_CURVE_WITH_KNOTS ( 'NONE', 3,
 ( #42148, #61205, #32726, #22387 ),
 .UNSPECIFIED., .F., .F.,
 ( 4, 4 ),
 ( 1.734723475976807094E-17, 0.005004741218457424944 ),
 .UNSPECIFIED. ) ;
#29058 = ADVANCED_FACE ( 'NONE', ( #18095 ), #31016, .F. ) ;
#29059 = FACE_OUTER_BOUND ( 'NONE', #58003, .T. ) ;
#29060 = DIRECTION ( 'NONE',  ( -1.000000000000000000, -0.000000000000000000, -0.000000000000000000 ) ) ;
#29061 = VERTEX_POINT ( 'NONE', #56287 ) ;
#29062 = AXIS2_PLACEMENT_3D ( 'NONE', #13718, #28408, #32510 ) ;
#29063 = CARTESIAN_POINT ( 'NONE',  ( 0.9730545539215883499, -5.099196237955184507, 42.60426903087352457 ) ) ;
#29064 = ORIENTED_EDGE ( 'NONE', *, *, #35946, .T. ) ;
#29065 = ADVANCED_FACE ( 'NONE', ( #22787 ), #61723, .F. ) ;
#29066 = ADVANCED_FACE ( 'NONE', ( #13402 ), #40955, .F. ) ;
#29067 = CARTESIAN_POINT ( 'NONE',  ( 52.11657354882707693, 15.35644106150795807, -2.106932783932539799 ) ) ;
#29068 = CARTESIAN_POINT ( 'NONE',  ( 2.648799415243696664, 3.327403256648802987, 48.92285611917237986 ) ) ;
#29069 = EDGE_LOOP ( 'NONE', ( #1068, #35300, #48630, #57681 ) ) ;
#29070 = CARTESIAN_POINT ( 'NONE',  ( -6.001507490154111224, -16.32705935667514296, 9.408444979392264429 ) ) ;
#29071 = EDGE_CURVE ( 'NONE', #929, #23349, #40502, .T. ) ;
#29072 = CARTESIAN_POINT ( 'NONE',  ( 0.5804410086790514622, -44.48029469925780433, -14.86685021524651162 ) ) ;
#29073 = CARTESIAN_POINT ( 'NONE',  ( 4.956653778116970166, 43.37017594958054900, 20.77844580450576117 ) ) ;
#29074 = CARTESIAN_POINT ( 'NONE',  ( -2.739355103387247858, 8.754959582419541420, -12.09124681996101103 ) ) ;
#29075 = ORIENTED_EDGE ( 'NONE', *, *, #11372, .F. ) ;
#29076 = DIRECTION ( 'NONE',  ( 0.000000000000000000, 0.000000000000000000, -1.000000000000000000 ) ) ;
#29077 = VERTEX_POINT ( 'NONE', #14028 ) ;
#29078 = CARTESIAN_POINT ( 'NONE',  ( 0.3622758884714730732, -36.91764744403337062, 22.26738722580103413 ) ) ;
#29079 = EDGE_CURVE ( 'NONE', #44331, #27918, #3070, .T. ) ;
#29080 = VERTEX_POINT ( 'NONE', #8993 ) ;
#29081 = ORIENTED_EDGE ( 'NONE', *, *, #20097, .F. ) ;
#29082 = CARTESIAN_POINT ( 'NONE',  ( 0.9769922540276050338, -37.60142665668843875, 18.50579013357184621 ) ) ;
#29083 = CARTESIAN_POINT ( 'NONE',  ( 0.3676999524040323597, 36.51379593394458567, 24.75264207750540635 ) ) ;
#29084 = EDGE_LOOP ( 'NONE', ( #53739, #55584, #10533, #44529 ) ) ;
#29085 = CARTESIAN_POINT ( 'NONE',  ( 0.7762777257811889209, -46.03397617421218513, -13.25585385760155432 ) ) ;
#29086 = DIRECTION ( 'NONE',  ( -1.000000000000000000, 0.000000000000000000, 0.000000000000000000 ) ) ;
#29087 = CARTESIAN_POINT ( 'NONE',  ( 2.648799415243708655, -49.01629645596155171, 1.385692978581188006 ) ) ;
#29089 = ORIENTED_EDGE ( 'NONE', *, *, #40707, .T. ) ;
#29088 = B_SPLINE_CURVE_WITH_KNOTS ( 'NONE', 3,
 ( #43391, #10162, #429, #38689, #53657, #29257 ),
 .UNSPECIFIED., .F., .F.,
 ( 4, 2, 4 ),
 ( 3.496446946337351263E-18, 0.0002450742804987349893, 0.0004901485609974665092 ),
 .UNSPECIFIED. ) ;
#29090 = B_SPLINE_CURVE_WITH_KNOTS ( 'NONE', 3,
 ( #13876, #41460, #50826, #61138, #4119, #17955, #56137, #47081, #32984, #60523, #32357, #52058, #28256, #33594, #5046, #28874, #38004, #34210, #48297 ),
 .UNSPECIFIED., .F., .F.,
 ( 4, 3, 3, 3, 3, 3, 4 ),
 ( 1.149162571898268292E-16, 0.0002618519381806242905, 0.0003927759815485965715, 0.0005237000248299455984, 0.0006546240681324996683, 0.0007855481115631327092, 0.0009699050456655110503 ),
 .UNSPECIFIED. ) ;
#29091 = ORIENTED_EDGE ( 'NONE', *, *, #5349, .T. ) ;
#29092 = CARTESIAN_POINT ( 'NONE',  ( 0.3622758884714730732, 10.35929834645922831, -41.85013935980092015 ) ) ;
#29093 = CARTESIAN_POINT ( 'NONE',  ( 2.500000000000000000, -2.357898499370432166, 3.035766082959412415E-15 ) ) ;
#29094 = DIRECTION ( 'NONE',  ( -1.000000000000000000, -0.000000000000000000, -0.000000000000000000 ) ) ;
#29095 = CARTESIAN_POINT ( 'NONE',  ( 5.960221823109900008, 12.49086489703227798, -16.28736530777577585 ) ) ;
#29096 = VERTEX_POINT ( 'NONE', #42842 ) ;
#29097 = VERTEX_POINT ( 'NONE', #4888 ) ;
#29098 = CARTESIAN_POINT ( 'NONE',  ( 0.5998501479064708430, 11.94461217097404493, 46.60114184914321811 ) ) ;
#29099 = CARTESIAN_POINT ( 'NONE',  ( 0.6008122571543325074, -20.27531257495885342, -44.72657208475775548 ) ) ;
#29100 = CARTESIAN_POINT ( 'NONE',  ( 0.5830081025819942031, -41.97804134881273086, -20.90636455483389611 ) ) ;
#29101 = B_SPLINE_CURVE_WITH_KNOTS ( 'NONE', 3,
 ( #20229, #29304, #52797, #39345 ),
 .UNSPECIFIED., .F., .F.,
 ( 4, 4 ),
 ( 0.000000000000000000, 0.004442905043737216571 ),
 .UNSPECIFIED. ) ;
#29102 = CARTESIAN_POINT ( 'NONE',  ( 4.553261556744875094, 0.000000000000000000, 0.000000000000000000 ) ) ;
#29103 = CARTESIAN_POINT ( 'NONE',  ( 0.9268187852002115479, 10.77474991967946849, 42.75112977544562654 ) ) ;
#29104 =( LENGTH_UNIT ( ) NAMED_UNIT ( * ) SI_UNIT ( .MILLI., .METRE. ) );
#29105 = CARTESIAN_POINT ( 'NONE',  ( 4.549368137175248350, -32.13400537129904677, -28.46244473166662559 ) ) ;
#29106 = CIRCLE ( 'NONE', #2069, 15.14599999999999369 ) ;
#29107 = EDGE_CURVE ( 'NONE', #15738, #371, #24021, .T. ) ;
#29108 = ORIENTED_EDGE ( 'NONE', *, *, #6830, .T. ) ;
#29109 = CARTESIAN_POINT ( 'NONE',  ( -6.057079549204054558, -19.21795591696650618, -1.225316886878888401 ) ) ;
#29110 = CARTESIAN_POINT ( 'NONE',  ( 4.335381028904201628, -23.55321997556108471, -42.95349434501429897 ) ) ;
#29111 = CARTESIAN_POINT ( 'NONE',  ( 0.1100247026804066219, -16.34612806822732978, -39.90641708963705980 ) ) ;
#29112 = CARTESIAN_POINT ( 'NONE',  ( 4.975610109902397937, -5.269241389990889424, -48.62802178077758697 ) ) ;
#29113 = DIRECTION ( 'NONE',  ( -1.000000000000000000, -0.000000000000000000, -0.000000000000000000 ) ) ;
#29114 = CARTESIAN_POINT ( 'NONE',  ( 5.960721111146673579, 20.52557019979492026, -0.006321279846608376246 ) ) ;
#29115 =( BOUNDED_SURFACE ( )  B_SPLINE_SURFACE ( 3, 1, ( 
 ( #20458, #53629 ),
 ( #45219, #24851 ),
 ( #6316, #19857 ),
 ( #38971, #53335 ) ),
 .UNSPECIFIED., .F., .F., .F. ) 
 B_SPLINE_SURFACE_WITH_KNOTS ( ( 4, 4 ),
 ( 2, 2 ),
 ( 0.000000000000000000, 1.000000000000000000 ),
 ( 0.000000000000000000, 1.000000000000000000 ),
 .UNSPECIFIED. ) 
 GEOMETRIC_REPRESENTATION_ITEM ( )  RATIONAL_B_SPLINE_SURFACE ( (
 ( 1.000000000000000000, 1.000000000000000000),
 ( 0.7269869731126821222, 0.9931720237060910339),
 ( 0.7269869731126821222, 0.9931720237060910339),
 ( 1.000000000000000000, 1.000000000000000000) ) ) 
 REPRESENTATION_ITEM ( '' )  SURFACE ( )  );
#29116 = EDGE_LOOP ( 'NONE', ( #43949, #3220, #35650, #27912 ) ) ;
#29117 = CARTESIAN_POINT ( 'NONE',  ( 4.962356264823608143, -4.645793755591040686, 41.82884409403227011 ) ) ;
#29118 = CARTESIAN_POINT ( 'NONE',  ( 0.1103744047535531458, 37.32746539760790228, 21.59576373962429940 ) ) ;
#29119 = B_SPLINE_CURVE_WITH_KNOTS ( 'NONE', 3,
 ( #43216, #37593, #27861, #46992 ),
 .UNSPECIFIED., .F., .F.,
 ( 4, 4 ),
 ( 2.168404344971008868E-18, 0.004041751736740980400 ),
 .UNSPECIFIED. ) ;
#29120 = CARTESIAN_POINT ( 'NONE',  ( 0.6027444965799114707, -47.46805475837615518, -12.58261869974789171 ) ) ;
#29121 = CARTESIAN_POINT ( 'NONE',  ( 4.226256110419179812, 40.57295234433516384, 16.87195270416243886 ) ) ;
#29122 = CARTESIAN_POINT ( 'NONE',  ( 1.227938101723756947, -36.73927144310528092, 22.18841447410706635 ) ) ;
#29123 = ORIENTED_EDGE ( 'NONE', *, *, #27095, .T. ) ;
#29124 = B_SPLINE_CURVE_WITH_KNOTS ( 'NONE', 3,
 ( #15220, #1091, #5473, #15834 ),
 .UNSPECIFIED., .F., .F.,
 ( 4, 4 ),
 ( 0.000000000000000000, 0.005014147105413706458 ),
 .UNSPECIFIED. ) ;
#29125 = ADVANCED_FACE ( 'NONE', ( #23103 ), #48918, .T. ) ;
#29126 = DIRECTION ( 'NONE',  ( -1.000000000000000000, -0.000000000000000000, -0.000000000000000000 ) ) ;
#29127 = CARTESIAN_POINT ( 'NONE',  ( 5.901463166500146684, -15.79333916981796726, -12.45344563595674714 ) ) ;
#29128 = ADVANCED_FACE ( 'NONE', ( #42231 ), #50946, .F. ) ;
#29129 = CARTESIAN_POINT ( 'NONE',  ( 0.9762797500689124330, -39.75277516423506086, -13.26806888463731227 ) ) ;
#29130 = ORIENTED_EDGE ( 'NONE', *, *, #58378, .F. ) ;
#29131 = CARTESIAN_POINT ( 'NONE',  ( -6.015611763856276717, -18.68122482568278286, -2.465697960551244350 ) ) ;
#29132 = EDGE_CURVE ( 'NONE', #46173, #15504, #10936, .T. ) ;
#29133 = CARTESIAN_POINT ( 'NONE',  ( 5.959547316686252039, -2.675599016784394379, -20.35048796920736081 ) ) ;
#29134 = EDGE_LOOP ( 'NONE', ( #43642, #18693, #10481, #300 ) ) ;
#29135 = EDGE_CURVE ( 'NONE', #31646, #8175, #45956, .T. ) ;
#29136 = CARTESIAN_POINT ( 'NONE',  ( 0.3622758884714600280, -17.25816669465019615, 39.50828911766968332 ) ) ;
#29137 = ORIENTED_EDGE ( 'NONE', *, *, #51930, .F. ) ;
#29138 = CARTESIAN_POINT ( 'NONE',  ( 3.376099380956842921, -13.22083125066026099, -2.217657474370683612 ) ) ;
#29139 = ADVANCED_FACE ( 'NONE', ( #38763, #47842 ), #57499, .F. ) ;
#29140 = VERTEX_POINT ( 'NONE', #37526 ) ;
#29141 = CARTESIAN_POINT ( 'NONE',  ( 0.3622758884714730732, 36.91764744403321430, -22.26738722580129348 ) ) ;
#29142 = VERTEX_POINT ( 'NONE', #14639 ) ;
#29143 = CARTESIAN_POINT ( 'NONE',  ( 10.00000000000001599, -58.44237546506767700, -54.69470952477997372 ) ) ;
#29144 = ORIENTED_EDGE ( 'NONE', *, *, #40664, .T. ) ;
#29145 = FACE_OUTER_BOUND ( 'NONE', #47357, .T. ) ;
#29146 = CARTESIAN_POINT ( 'NONE',  ( 5.959547316686252039, 5.315863417546330183, -19.82530672674356964 ) ) ;
#29147 = AXIS2_PLACEMENT_3D ( 'NONE', #54974, #45008, #12406 ) ;
#29148 = CARTESIAN_POINT ( 'NONE',  ( 0.5806925824938499181, 40.06810415365472977, 24.36738377166168235 ) ) ;
#29149 = EDGE_LOOP ( 'NONE', ( #60058, #27609, #34565, #57149 ) ) ;
#29150 = CARTESIAN_POINT ( 'NONE',  ( 0.9754642270333679921, -16.25787253057904991, -39.70914670678651959 ) ) ;
#29151 = EDGE_CURVE ( 'NONE', #58288, #15929, #47924, .T. ) ;
#29152 = CARTESIAN_POINT ( 'NONE',  ( 1.154321485836934169, 36.74718014677598887, -22.16897757994436802 ) ) ;
#29153 = CARTESIAN_POINT ( 'NONE',  ( -6.078726893082806448, 15.43407385306362301, 11.51448676958282391 ) ) ;
#29154 = VERTEX_POINT ( 'NONE', #18713 ) ;
#29155 = CARTESIAN_POINT ( 'NONE',  ( 0.5806925824938502512, -13.37132486740698134, 44.94919391528425479 ) ) ;
#29156 = EDGE_CURVE ( 'NONE', #30940, #9945, #32822, .T. ) ;
#29157 = CARTESIAN_POINT ( 'NONE',  ( 1.827326673878743479, -39.28486782721054738, -17.60663982372524217 ) ) ;
#29158 = ORIENTED_EDGE ( 'NONE', *, *, #48542, .F. ) ;
#29159 = CARTESIAN_POINT ( 'NONE',  ( 2.528100132419516477, 25.86511525564304037, 33.06432505653756238 ) ) ;
#29160 = VERTEX_POINT ( 'NONE', #14329 ) ;
#29161 = CARTESIAN_POINT ( 'NONE',  ( 2.618530812446115519, -29.26021975733438651, 36.79084572214530624 ) ) ;
#29162 = CYLINDRICAL_SURFACE ( 'NONE', #61951, 9.500000000000000000 ) ;
#29163 = ORIENTED_EDGE ( 'NONE', *, *, #34446, .F. ) ;
#29164 = CARTESIAN_POINT ( 'NONE',  ( 6.566016632682842413, -8.528786624275486616, 3.000000000000020872 ) ) ;
#29165 = CARTESIAN_POINT ( 'NONE',  ( 0.1145239942831223490, 25.51135876117968593, -36.00161183701438006 ) ) ;
#29166 = CARTESIAN_POINT ( 'NONE',  ( -6.016761891674564211, -18.68243340030201338, -2.456125503350905959 ) ) ;
#29167 = DIRECTION ( 'NONE',  ( 1.000000000000000000, 0.000000000000000000, 0.000000000000000000 ) ) ;
#29168 = ORIENTED_EDGE ( 'NONE', *, *, #34671, .F. ) ;
#29169 = CARTESIAN_POINT ( 'NONE',  ( 4.834790513006553603, 43.62201989944812652, 18.15788315901754757 ) ) ;
#29170 = CARTESIAN_POINT ( 'NONE',  ( 0.8751705887134553219, 13.30665218149297857, 46.21789262997761938 ) ) ;
#29171 = CARTESIAN_POINT ( 'NONE',  ( 2.881901170002227897, 8.474399077991585715E-12, -49.00591519830774700 ) ) ;
#29173 = DIRECTION ( 'NONE',  ( 1.000000000000000000, 0.000000000000000000, 0.000000000000000000 ) ) ;
#29172 =( BOUNDED_SURFACE ( )  B_SPLINE_SURFACE ( 3, 1, ( 
 ( #51865, #8963 ),
 ( #28072, #34325 ),
 ( #53400, #33404 ),
 ( #1090, #10509 ) ),
 .UNSPECIFIED., .F., .F., .F. ) 
 B_SPLINE_SURFACE_WITH_KNOTS ( ( 4, 4 ),
 ( 2, 2 ),
 ( 0.000000000000000000, 1.000000000000000000 ),
 ( 0.000000000000000000, 1.000000000000000000 ),
 .UNSPECIFIED. ) 
 GEOMETRIC_REPRESENTATION_ITEM ( )  RATIONAL_B_SPLINE_SURFACE ( (
 ( 1.000000000000000000, 1.000000000000000000),
 ( 0.7282232189291693025, 0.9929344683865674037),
 ( 0.7282232189291693025, 0.9929344683865674037),
 ( 1.000000000000000000, 1.000000000000000000) ) ) 
 REPRESENTATION_ITEM ( '' )  SURFACE ( )  );
#29174 = DIRECTION ( 'NONE',  ( -0.07906939808003034253, 0.6871887087747716727, -0.7221632148065447732 ) ) ;
#29175 = EDGE_CURVE ( 'NONE', #31234, #20011, #9296, .T. ) ;
#29176 = CARTESIAN_POINT ( 'NONE',  ( 4.060580049360325461, -9.288457618609966104, -42.95570101193199264 ) ) ;
#29177 = CARTESIAN_POINT ( 'NONE',  ( 0.7048096507298635682, 7.115188260603208192, 47.58126109679103877 ) ) ;
#29178 = CARTESIAN_POINT ( 'NONE',  ( 0.6067375320500697500, 38.42671567536892496, -28.59217831626977357 ) ) ;
#29179 = CARTESIAN_POINT ( 'NONE',  ( 3.240649175237395152, 13.46447809955735586, 41.88045781631560516 ) ) ;
#29180 = CARTESIAN_POINT ( 'NONE',  ( 0.9752570700956796346, 30.50353876750672910, -30.17732761204907277 ) ) ;
#29181 = DIRECTION ( 'NONE',  ( 0.000000000000000000, 0.000000000000000000, -1.000000000000000000 ) ) ;
#29182 = CARTESIAN_POINT ( 'NONE',  ( -6.017396004339686577, -17.40926186480773907, -7.209881890566737006 ) ) ;
#29183 = VECTOR ( 'NONE', #29805, 1000.000000000000114 ) ;
#29184 = CARTESIAN_POINT ( 'NONE',  ( 0.5835226383429310548, -1.384976919776544912, 46.87562600624814024 ) ) ;
#29185 =( BOUNDED_SURFACE ( )  B_SPLINE_SURFACE ( 3, 1, ( 
 ( #3242, #56487 ),
 ( #36803, #17674 ),
 ( #50867, #17068 ),
 ( #46196, #4164 ) ),
 .UNSPECIFIED., .F., .F., .F. ) 
 B_SPLINE_SURFACE_WITH_KNOTS ( ( 4, 4 ),
 ( 2, 2 ),
 ( 0.000000000000000000, 1.000000000000000000 ),
 ( 0.000000000000000000, 1.000000000000000000 ),
 .UNSPECIFIED. ) 
 GEOMETRIC_REPRESENTATION_ITEM ( )  RATIONAL_B_SPLINE_SURFACE ( (
 ( 1.000000000000000000, 1.000000000000000000),
 ( 0.7223157951917480446, 0.9931996967497186413),
 ( 0.7223157951917480446, 0.9931996967497186413),
 ( 1.000000000000000000, 1.000000000000000000) ) ) 
 REPRESENTATION_ITEM ( '' )  SURFACE ( )  );
#29186 = CIRCLE ( 'NONE', #5208, 47.09074272231896430 ) ;
#29187 = DIRECTION ( 'NONE',  ( 0.000000000000000000, 0.000000000000000000, -1.000000000000000000 ) ) ;
#29188 = DIRECTION ( 'NONE',  ( 0.07500201931887538753, 0.6540624036680682263, -0.7527131387228735981 ) ) ;
#29189 = EDGE_LOOP ( 'NONE', ( #27737, #8282, #23843, #47902 ) ) ;
#29190 = CARTESIAN_POINT ( 'NONE',  ( 0.000000000000000000, 1.178949249685217415, 2.041999999999998483 ) ) ;
#29191 = CARTESIAN_POINT ( 'NONE',  ( 0.8560838555295223751, -35.39593983670150124, -30.78149244527203621 ) ) ;
#29192 = CARTESIAN_POINT ( 'NONE',  ( -6.015611763856276717, 9.416239407363534042, -16.32183393015586503 ) ) ;
#29193 = ORIENTED_EDGE ( 'NONE', *, *, #6835, .F. ) ;
#29194 = CARTESIAN_POINT ( 'NONE',  ( 4.553261556744873317, -20.51767157960462384, -38.84024612145397981 ) ) ;
#29195 = DIRECTION ( 'NONE',  ( 0.000000000000000000, -1.224646799147353454E-16, 1.000000000000000000 ) ) ;
#29196 = B_SPLINE_CURVE_WITH_KNOTS ( 'NONE', 3,
 ( #22423, #8014, #4521, #41552, #27744, #31832, #28352, #60614, #47473, #23661, #28052, #60305, #50918, #22735, #41867, #17731, #32448, #46875, #27125 ),
 .UNSPECIFIED., .F., .F.,
 ( 4, 3, 3, 3, 3, 3, 4 ),
 ( 1.153344816771540786E-16, 0.0002618519381806256457, 0.0003927759815485972221, 0.0005237000248299425627, 0.0006546240681324985841, 0.0007855481115631309744, 0.0009699050456655101829 ),
 .UNSPECIFIED. ) ;
#29197 = ORIENTED_EDGE ( 'NONE', *, *, #28645, .T. ) ;
#29198 = ORIENTED_EDGE ( 'NONE', *, *, #29412, .F. ) ;
#29199 = CARTESIAN_POINT ( 'NONE',  ( 0.5807400328401637335, -12.92266817606048335, 46.12278621143492785 ) ) ;
#29200 = EDGE_CURVE ( 'NONE', #10336, #23991, #33436, .T. ) ;
#29201 = ORIENTED_EDGE ( 'NONE', *, *, #1888, .T. ) ;
#29202 = CARTESIAN_POINT ( 'NONE',  ( 4.553261556744873317, 42.43205150231990075, -11.36048287389704292 ) ) ;
#29203 = VERTEX_POINT ( 'NONE', #19036 ) ;
#29204 = EDGE_CURVE ( 'NONE', #4680, #46648, #44936, .T. ) ;
#29205 = ORIENTED_EDGE ( 'NONE', *, *, #10253, .F. ) ;
#29206 = CARTESIAN_POINT ( 'NONE',  ( 0.9730545539215883499, 25.71816799638778406, 34.34678117142565412 ) ) ;
#29207 = ORIENTED_EDGE ( 'NONE', *, *, #58830, .F. ) ;
#29208 = CARTESIAN_POINT ( 'NONE',  ( 4.291220156522060236, -9.951772474098369514, -46.04727160136066288 ) ) ;
#29209 = CARTESIAN_POINT ( 'NONE',  ( 1.227938101723748288, 39.32113113558966688, 17.20315230597858047 ) ) ;
#29210 = DIRECTION ( 'NONE',  ( 0.000000000000000000, 0.000000000000000000, 1.000000000000000000 ) ) ;
#29211 = ORIENTED_EDGE ( 'NONE', *, *, #43546, .T. ) ;
#29213 = B_SPLINE_CURVE_WITH_KNOTS ( 'NONE', 3,
 ( #17356, #59320, #49617, #21431 ),
 .UNSPECIFIED., .F., .F.,
 ( 4, 4 ),
 ( 0.000000000000000000, 0.004445488388166993383 ),
 .UNSPECIFIED. ) ;
#29212 = CARTESIAN_POINT ( 'NONE',  ( -2.739355103387247858, 6.670587007382158262, 13.35480572408154920 ) ) ;
#29214 = CARTESIAN_POINT ( 'NONE',  ( 0.6017666602106489515, -48.10631669010027878, 0.3491145841137135442 ) ) ;
#29215 = ORIENTED_EDGE ( 'NONE', *, *, #30042, .T. ) ;
#29216 = ORIENTED_EDGE ( 'NONE', *, *, #48457, .F. ) ;
#29217 = ORIENTED_EDGE ( 'NONE', *, *, #22567, .T. ) ;
#29218 = CARTESIAN_POINT ( 'NONE',  ( 3.270143674763207553, 13.53222904135357041, -2.058141141425458454 ) ) ;
#29219 = CARTESIAN_POINT ( 'NONE',  ( 1.154321713695928286, -30.92445811446669168, 29.75729669971099156 ) ) ;
#29220 = FACE_OUTER_BOUND ( 'NONE', #25422, .T. ) ;
#29221 = CARTESIAN_POINT ( 'NONE',  ( 0.1081432562775998946, 5.208748643066120287, 42.80885385101083784 ) ) ;
#29222 = EDGE_CURVE ( 'NONE', #8039, #3160, #15084, .T. ) ;
#29223 = EDGE_LOOP ( 'NONE', ( #48423, #55425, #59706, #50634 ) ) ;
#29224 = CARTESIAN_POINT ( 'NONE',  ( 3.238741278300275805, 19.89284324544641436, 38.11287256318068728 ) ) ;
#29225 = AXIS2_PLACEMENT_3D ( 'NONE', #28962, #48077, #24259 ) ;
#29226 = DIRECTION ( 'NONE',  ( 1.000000000000000000, 0.000000000000000000, 0.000000000000000000 ) ) ;
#29227 = VECTOR ( 'NONE', #7097, 1000.000000000000114 ) ;
#29228 = CARTESIAN_POINT ( 'NONE',  ( 5.895881250540457863, 19.70893872444552386, -4.010662783674629139 ) ) ;
#29229 = CARTESIAN_POINT ( 'NONE',  ( -6.016761891674564211, -2.456125503350841566, 18.68243340030202049 ) ) ;
#29230 = EDGE_LOOP ( 'NONE', ( #45617, #2795, #53077, #25023 ) ) ;
#29231 = CARTESIAN_POINT ( 'NONE',  ( 4.975801465491695552, -47.84403947906842092, -2.564218696447329027 ) ) ;
#29232 = CARTESIAN_POINT ( 'NONE',  ( 0.6008122571543325074, -14.38934544891279188, -46.95211697056022615 ) ) ;
#29233 = CARTESIAN_POINT ( 'NONE',  ( 4.967162193818130511, 0.000000000000000000, 0.000000000000000000 ) ) ;
#29234 = CARTESIAN_POINT ( 'NONE',  ( -17.97369999999976642, -12.32233744059949210, 2.099999999999994760 ) ) ;
#29235 = ORIENTED_EDGE ( 'NONE', *, *, #14476, .F. ) ;
#29236 = ORIENTED_EDGE ( 'NONE', *, *, #8594, .T. ) ;
#29237 = CARTESIAN_POINT ( 'NONE',  ( 0.9788927965476014181, -39.63608187503911040, -13.61314167365405403 ) ) ;
#29238 = CARTESIAN_POINT ( 'NONE',  ( 0.7048096507298579061, -34.61049487267082014, 33.41730025321693631 ) ) ;
#29239 = CARTESIAN_POINT ( 'NONE',  ( 4.553261556744875094, -15.38244134641827898, 41.14510984366961566 ) ) ;
#29240 = CARTESIAN_POINT ( 'NONE',  ( -6.072942160501519915, 16.77122109808136230, -9.462045506564152220 ) ) ;
#29241 = LINE ( 'NONE', #48358, #23558 ) ;
#29242 = CARTESIAN_POINT ( 'NONE',  ( 3.783198216974390515, 35.16829104054202304, -24.80909581868404956 ) ) ;
#29243 = CARTESIAN_POINT ( 'NONE',  ( 0.5809828226811617480, 47.55412398569215071, -5.711058609464832792 ) ) ;
#29244 = CARTESIAN_POINT ( 'NONE',  ( 3.782625744892852637, 8.059507167186435339, -41.25872572337967625 ) ) ;
#29245 = ADVANCED_FACE ( 'NONE', ( #39376 ), #57329, .F. ) ;
#29246 = FACE_OUTER_BOUND ( 'NONE', #11480, .T. ) ;
#29247 = CARTESIAN_POINT ( 'NONE',  ( -6.010958268070873523, -13.33459572764767032, 13.31406649671957787 ) ) ;
#29248 = CARTESIAN_POINT ( 'NONE',  ( 0.2940135542859017570, 40.08987455701127800, 18.41310692671174820 ) ) ;
#29249 = ORIENTED_EDGE ( 'NONE', *, *, #61810, .T. ) ;
#29250 = DIRECTION ( 'NONE',  ( 0.000000000000000000, 0.000000000000000000, 1.000000000000000000 ) ) ;
#29251 = DIRECTION ( 'NONE',  ( 0.000000000000000000, 0.000000000000000000, 1.000000000000000000 ) ) ;
#29252 = CARTESIAN_POINT ( 'NONE',  ( -6.078075953587585900, -8.901949479773122675, 17.07484903906043172 ) ) ;
#29253 = CARTESIAN_POINT ( 'NONE',  ( 1.227938101723748288, 36.73927144310511750, 22.18841447410732215 ) ) ;
#29254 = CARTESIAN_POINT ( 'NONE',  ( 0.6000166863083106206, -20.35571918921451484, 44.69304395538860319 ) ) ;
#29255 = CARTESIAN_POINT ( 'NONE',  ( 0.6031356219577719280, -46.44562759437263111, 12.53544563195218764 ) ) ;
#29256 = EDGE_CURVE ( 'NONE', #40254, #48086, #45707, .T. ) ;
#29257 = CARTESIAN_POINT ( 'NONE',  ( 0.8751705887134553219, 23.27176129838425922, -42.09020928323351995 ) ) ;
#29258 = CARTESIAN_POINT ( 'NONE',  ( 0.9730545539215883499, 6.101350888304637010, 42.47233286818619291 ) ) ;
#29259 = CARTESIAN_POINT ( 'NONE',  ( 0.6026777506516368677, 48.16831407909742069, -9.558237777678705527 ) ) ;
#29260 = CARTESIAN_POINT ( 'NONE',  ( 0.5997462898726536595, -31.02483596213057737, 38.06587952047342327 ) ) ;
#29261 = EDGE_CURVE ( 'NONE', #45029, #9871, #33723, .T. ) ;
#29263 =( BOUNDED_SURFACE ( )  B_SPLINE_SURFACE ( 3, 1, ( 
 ( #58553, #53852 ),
 ( #25062, #20371 ),
 ( #57621, #58240 ),
 ( #14752, #10354 ) ),
 .UNSPECIFIED., .F., .F., .F. ) 
 B_SPLINE_SURFACE_WITH_KNOTS ( ( 4, 4 ),
 ( 2, 2 ),
 ( 0.000000000000000000, 1.000000000000000000 ),
 ( 0.000000000000000000, 1.000000000000000000 ),
 .UNSPECIFIED. ) 
 GEOMETRIC_REPRESENTATION_ITEM ( )  RATIONAL_B_SPLINE_SURFACE ( (
 ( 1.000000000000000000, 1.000000000000000000),
 ( 0.9952954269826590483, 0.8620686068821307169),
 ( 0.9952954269826590483, 0.8620686068821307169),
 ( 1.000000000000000000, 1.000000000000000000) ) ) 
 REPRESENTATION_ITEM ( '' )  SURFACE ( )  );
#29262 = CARTESIAN_POINT ( 'NONE',  ( 0.6029442701453591180, -1.661030530721965937, -49.07938673959044706 ) ) ;
#29264 = CARTESIAN_POINT ( 'NONE',  ( 0.5980271706414711508, -8.528665270202141713, 48.36642545765100465 ) ) ;
#29266 = VERTEX_POINT ( 'NONE', #35283 ) ;
#29265 = CARTESIAN_POINT ( 'NONE',  ( 4.975801465491695552, 0.000000000000000000, 0.000000000000000000 ) ) ;
#29267 = ORIENTED_EDGE ( 'NONE', *, *, #7985, .T. ) ;
#29268 = CARTESIAN_POINT ( 'NONE',  ( 0.1313383488274125765, -33.82021892231565374, 26.75504982351751693 ) ) ;
#29269 = CARTESIAN_POINT ( 'NONE',  ( 5.895596859100789899, -13.98490190264574196, 14.45512718677573538 ) ) ;
#29270 = CARTESIAN_POINT ( 'NONE',  ( 0.1152809850208375564, 41.80610087945574094, 14.11365338055760787 ) ) ;
#29271 = EDGE_LOOP ( 'NONE', ( #37842, #28976, #22305, #59227 ) ) ;
#29272 = CARTESIAN_POINT ( 'NONE',  ( 0.1100247026804066219, -11.32523219034937156, 41.61078157869232541 ) ) ;
#29273 = CARTESIAN_POINT ( 'NONE',  ( 3.601691676948239884, 0.2777746788518056786, 42.02545230802814302 ) ) ;
#29274 = CARTESIAN_POINT ( 'NONE',  ( 0.5980894510889457338, -44.71414919659894593, -17.76188940524932747 ) ) ;
#29275 = TOROIDAL_SURFACE ( 'NONE', #14280, 6.866799999999992465, 0.02570000000000187065 ) ;
#29276 = VECTOR ( 'NONE', #57877, 1000.000000000000227 ) ;
#29277 = EDGE_LOOP ( 'NONE', ( #31825, #44589, #721, #28911 ) ) ;
#29278 = ORIENTED_EDGE ( 'NONE', *, *, #57942, .F. ) ;
#29279 = CARTESIAN_POINT ( 'NONE',  ( 0.6027935024548037868, -23.90242449907784916, -41.74929432965609521 ) ) ;
#29280 = CARTESIAN_POINT ( 'NONE',  ( 0.9762797500689124330, 33.20096159360316790, 25.57383300261796677 ) ) ;
#29281 = EDGE_CURVE ( 'NONE', #38098, #38419, #6043, .T. ) ;
#29282 = CARTESIAN_POINT ( 'NONE',  ( 0.9968887458511636046, -39.38692798189855182, -17.02616470386922032 ) ) ;
#29283 = CARTESIAN_POINT ( 'NONE',  ( 0.2940133293163010308, 14.47847103911990985, 41.67270600701866812 ) ) ;
#29284 = ADVANCED_FACE ( 'NONE', ( #34357 ), #56244, .F. ) ;
#29285 =( BOUNDED_SURFACE ( )  B_SPLINE_SURFACE ( 3, 1, ( 
 ( #47336, #32944 ),
 ( #48797, #49107 ),
 ( #39425, #5851 ),
 ( #37969, #37648 ) ),
 .UNSPECIFIED., .F., .F., .F. ) 
 B_SPLINE_SURFACE_WITH_KNOTS ( ( 4, 4 ),
 ( 2, 2 ),
 ( 0.000000000000000000, 1.000000000000000000 ),
 ( 0.000000000000000000, 1.000000000000000000 ),
 .UNSPECIFIED. ) 
 GEOMETRIC_REPRESENTATION_ITEM ( )  RATIONAL_B_SPLINE_SURFACE ( (
 ( 1.000000000000000000, 1.000000000000000000),
 ( 0.7282232189291694135, 0.9929344683865672927),
 ( 0.7282232189291694135, 0.9929344683865672927),
 ( 1.000000000000000000, 1.000000000000000000) ) ) 
 REPRESENTATION_ITEM ( '' )  SURFACE ( )  );
#29286 = CARTESIAN_POINT ( 'NONE',  ( 1.088313998177382835, -10.35171213034662330, -41.64627086748864571 ) ) ;
#29287 = B_SPLINE_CURVE_WITH_KNOTS ( 'NONE', 3,
 ( #49292, #39617, #15490, #30184, #20801, #39938, #6348, #58672, #15798, #58995, #16106, #35218, #54277, #6655, #44939, #1977 ),
 .UNSPECIFIED., .F., .F.,
 ( 4, 3, 3, 3, 3, 4 ),
 ( 2.081781105835003463E-17, 0.0002612764279487747349, 0.0003919131003184788114, 0.0005225497727000652558, 0.0007837925190632463301, 0.001045051706266715650 ),
 .UNSPECIFIED. ) ;
#29288 = CARTESIAN_POINT ( 'NONE',  ( 2.299652685299200972, -42.07683617587559155, -25.17581343843097841 ) ) ;
#29289 = EDGE_CURVE ( 'NONE', #5948, #38470, #25482, .T. ) ;
#29290 = CARTESIAN_POINT ( 'NONE',  ( 0.5838002273316426072, 38.08117724016846495, -29.04904228829574109 ) ) ;
#29291 = ORIENTED_EDGE ( 'NONE', *, *, #35275, .F. ) ;
#29292 = VERTEX_POINT ( 'NONE', #39687 ) ;
#29293 = CARTESIAN_POINT ( 'NONE',  ( -6.077587904424778920, 7.800189710370847074, -17.60548385805273242 ) ) ;
#29294 = CARTESIAN_POINT ( 'NONE',  ( -2.708315649062910779, -1.648584381066950488, -14.54141329178161612 ) ) ;
#29295 = EDGE_LOOP ( 'NONE', ( #51101, #52084, #54597, #51298 ) ) ;
#29296 = CARTESIAN_POINT ( 'NONE',  ( 4.956653778116970166, 45.35992544608529187, 15.97476558431900884 ) ) ;
#29297 = CARTESIAN_POINT ( 'NONE',  ( 7.999999999999986677, 56.56854249492450037, -56.56854249492312192 ) ) ;
#29298 = CARTESIAN_POINT ( 'NONE',  ( 0.3622758884714730732, -34.70015533914812522, -25.58609868863756276 ) ) ;
#29299 = CARTESIAN_POINT ( 'NONE',  ( -2.681483223904233881, 3.070647092368428588, -5.600000000000003197 ) ) ;
#29300 = EDGE_CURVE ( 'NONE', #52413, #33451, #56102, .T. ) ;
#29301 = ORIENTED_EDGE ( 'NONE', *, *, #7201, .F. ) ;
#29302 = B_SPLINE_CURVE_WITH_KNOTS ( 'NONE', 3,
 ( #28590, #37402, #23291, #51779 ),
 .UNSPECIFIED., .F., .F.,
 ( 4, 4 ),
 ( 6.938893903907228378E-18, 0.005013413432710138104 ),
 .UNSPECIFIED. ) ;
#29303 = ORIENTED_EDGE ( 'NONE', *, *, #6430, .T. ) ;
#29304 = CARTESIAN_POINT ( 'NONE',  ( 2.299746137290199943, 48.83328922304266939, -4.426194905876138286 ) ) ;
#29305 = CARTESIAN_POINT ( 'NONE',  ( 5.895596859100789899, 0.6684898708304538584, -20.10177366565161350 ) ) ;
#29306 = CARTESIAN_POINT ( 'NONE',  ( 0.7242486021783793859, 28.75996529048175887, -39.79793787200863164 ) ) ;
#29307 = CARTESIAN_POINT ( 'NONE',  ( 0.5834872094924183905, 28.97678700412181740, 38.13619618345218498 ) ) ;
#29308 = ORIENTED_EDGE ( 'NONE', *, *, #33550, .T. ) ;
#29309 = CARTESIAN_POINT ( 'NONE',  ( 0.5809828226811553087, 41.74875432577648837, 23.47450554821725532 ) ) ;
#29310 = VERTEX_POINT ( 'NONE', #7348 ) ;
#29311 = CARTESIAN_POINT ( 'NONE',  ( 4.549368137175248350, -35.80950303116117794, 23.67244292351576718 ) ) ;
#29312 = CARTESIAN_POINT ( 'NONE',  ( 0.1152339509894530906, 10.03623295132059567, 42.96762407443620191 ) ) ;
#29313 = VERTEX_POINT ( 'NONE', #12401 ) ;
#29314 = CARTESIAN_POINT ( 'NONE',  ( 0.5804410086790514622, -1.020940616195406880, -46.88792522722240363 ) ) ;
#29315 = DIRECTION ( 'NONE',  ( 0.1024043820194936449, -0.8548216096551033427, 0.5087173657443432306 ) ) ;
#29316 = CARTESIAN_POINT ( 'NONE',  ( 0.9740398440564321803, 25.79088785829030428, -34.29238484271503040 ) ) ;
#29317 = CARTESIAN_POINT ( 'NONE',  ( 0.7762783648524405056, -19.15108798908280718, -43.90991295203441780 ) ) ;
#29318 = CARTESIAN_POINT ( 'NONE',  ( 2.000000000000010658, -3.464101615137748169, -5.600000000000000533 ) ) ;
#29319 = CARTESIAN_POINT ( 'NONE',  ( 1.000433927950262980, -40.93358531992097227, 8.992233899849193079 ) ) ;
#29320 = CARTESIAN_POINT ( 'NONE',  ( 2.281351352603299798, 46.66131639318016511, -11.14238889600236426 ) ) ;
#29321 = CARTESIAN_POINT ( 'NONE',  ( 0.3676999524040323597, 30.26295534861902681, -32.09523511193413725 ) ) ;
#29322 = ORIENTED_EDGE ( 'NONE', *, *, #16894, .F. ) ;
#29323 = CARTESIAN_POINT ( 'NONE',  ( 2.618530812446115519, 46.98662296661649407, -1.408563591474231602 ) ) ;
#29324 = FACE_OUTER_BOUND ( 'NONE', #45905, .T. ) ;
#29325 = CARTESIAN_POINT ( 'NONE',  ( 0.5800708057587411481, -24.48933404430286842, 41.16170989303191874 ) ) ;
#29326 = ORIENTED_EDGE ( 'NONE', *, *, #6740, .T. ) ;
#29327 = ADVANCED_FACE ( 'NONE', ( #27103 ), #43109, .F. ) ;
#29328 = CARTESIAN_POINT ( 'NONE',  ( -17.42928676736936922, -12.33362675552796084, 2.032827274293960151 ) ) ;
#29329 = FACE_OUTER_BOUND ( 'NONE', #17838, .T. ) ;
#29330 = CARTESIAN_POINT ( 'NONE',  ( 2.281448460670567613, -11.14236343022405151, 46.66132715497960248 ) ) ;
#29331 = CARTESIAN_POINT ( 'NONE',  ( 0.5806925824938502512, -44.47729014209954101, -14.86583411581937320 ) ) ;
#29332 = VECTOR ( 'NONE', #48866, 1000.000000000000114 ) ;
#29333 = CARTESIAN_POINT ( 'NONE',  ( -6.016104459813374383, -17.40682403289243396, -7.215917642689251288 ) ) ;
#29334 = CARTESIAN_POINT ( 'NONE',  ( 0.6009453534118439633, 38.43042294376915180, -28.93865405070907926 ) ) ;
#29335 = EDGE_CURVE ( 'NONE', #34780, #42042, #62, .T. ) ;
#29336 = CARTESIAN_POINT ( 'NONE',  ( -0.5000000000002493561, -8.043653582563827727E-15, -3.653067726541008255E-16 ) ) ;
#29337 = CARTESIAN_POINT ( 'NONE',  ( 5.901463166500145796, 20.06674442072659303, 1.357806574544058398 ) ) ;
#29338 = B_SPLINE_CURVE_WITH_KNOTS ( 'NONE', 3,
 ( #46936, #42851, #47229, #4582, #61297, #42539, #60995, #9940, #56912, #18415, #37534, #19046, #13721, #8682, #52521, #9305 ),
 .UNSPECIFIED., .F., .F.,
 ( 4, 3, 3, 3, 3, 4 ),
 ( 2.081781105835003463E-17, 0.0002618515315864420310, 0.0003927756766341996717, 0.0005236998216950579984, 0.0007855159896329915251, 0.001047349442285929171 ),
 .UNSPECIFIED. ) ;
#29339 = CARTESIAN_POINT ( 'NONE',  ( 0.9787284016396609054, -6.785939174618667913, 41.35561664934046178 ) ) ;
#29340 = EDGE_CURVE ( 'NONE', #44468, #34503, #52898, .T. ) ;
#29341 = CARTESIAN_POINT ( 'NONE',  ( -3.514385190458188646, -13.03453477240703862, -1.199999999999999956 ) ) ;
#29343 = VERTEX_POINT ( 'NONE', #26171 ) ;
#29342 = DIRECTION ( 'NONE',  ( 0.09722883295013594329, -0.3959434903494651881, 0.9131129757554853343 ) ) ;
#29344 = ORIENTED_EDGE ( 'NONE', *, *, #49698, .F. ) ;
#29345 = CARTESIAN_POINT ( 'NONE',  ( 3.680882792899936362, -35.20667105325194512, -32.59085259319675743 ) ) ;
#29346 = CARTESIAN_POINT ( 'NONE',  ( 7.000000000000016875, -58.44237546506844438, 54.69470952477915660 ) ) ;
#29347 = CARTESIAN_POINT ( 'NONE',  ( 0.3622758884714600280, -29.89648521331609743, -31.06363466427717412 ) ) ;
#29348 = CARTESIAN_POINT ( 'NONE',  ( 0.1152809850208375564, -23.06252723633350143, 37.61735131509301766 ) ) ;
#29349 = CARTESIAN_POINT ( 'NONE',  ( 0.2885700199627502793, 17.24062365614539516, 39.51953436244181006 ) ) ;
#29350 = CARTESIAN_POINT ( 'NONE',  ( 0.5804410086790514622, 28.25755288515122388, -37.43034272883804192 ) ) ;
#29351 = VERTEX_POINT ( 'NONE', #22399 ) ;
#29352 = CARTESIAN_POINT ( 'NONE',  ( 4.956653778116982600, -43.37017594958069111, 20.77844580450546985 ) ) ;
#29353 = ADVANCED_FACE ( 'NONE', ( #45307 ), #15467, .F. ) ;
#29354 = CARTESIAN_POINT ( 'NONE',  ( -19.96574584685826537, -7.972179581716115848, 0.6786367118085059325 ) ) ;
#29355 = DIRECTION ( 'NONE',  ( 1.000000000000000000, -0.000000000000000000, -0.000000000000000000 ) ) ;
#29356 = EDGE_CURVE ( 'NONE', #22114, #4359, #60284, .T. ) ;
#29357 = EDGE_LOOP ( 'NONE', ( #52697, #53005, #43998, #24502 ) ) ;
#29358 = CARTESIAN_POINT ( 'NONE',  ( 0.9972139404380291339, -30.80335716430295889, -29.87264297738558483 ) ) ;
#29359 = EDGE_CURVE ( 'NONE', #31306, #39564, #37499, .T. ) ;
#29360 = CARTESIAN_POINT ( 'NONE',  ( 0.5839879327111934249, 47.47435452316582172, -6.341736898931451982 ) ) ;
#29361 =( BOUNDED_SURFACE ( )  B_SPLINE_SURFACE ( 3, 1, ( 
 ( #59528, #17565 ),
 ( #36681, #16636 ),
 ( #12876, #60756 ),
 ( #17877, #37000 ) ),
 .UNSPECIFIED., .F., .F., .F. ) 
 B_SPLINE_SURFACE_WITH_KNOTS ( ( 4, 4 ),
 ( 2, 2 ),
 ( 0.000000000000000000, 1.000000000000000000 ),
 ( 0.000000000000000000, 1.000000000000000000 ),
 .UNSPECIFIED. ) 
 GEOMETRIC_REPRESENTATION_ITEM ( )  RATIONAL_B_SPLINE_SURFACE ( (
 ( 1.000000000000000000, 1.000000000000000000),
 ( 0.9953390228620291325, 0.8624445117761032620),
 ( 0.9953390228620291325, 0.8624445117761032620),
 ( 1.000000000000000000, 1.000000000000000000) ) ) 
 REPRESENTATION_ITEM ( '' )  SURFACE ( )  );
#29362 = VERTEX_POINT ( 'NONE', #31178 ) ;
#29363 = DIRECTION ( 'NONE',  ( 0.000000000000000000, 0.000000000000000000, -1.000000000000000000 ) ) ;
#29364 = EDGE_LOOP ( 'NONE', ( #40557, #34676, #13601, #39100 ) ) ;
#29365 = LINE ( 'NONE', #24675, #41872 ) ;
#29366 = CARTESIAN_POINT ( 'NONE',  ( 0.8753041380234471980, 3.828530797420656384, 48.95386276695825956 ) ) ;
#29367 = B_SPLINE_CURVE_WITH_KNOTS ( 'NONE', 3,
 ( #45393, #16881, #35998, #55059 ),
 .UNSPECIFIED., .F., .F.,
 ( 4, 4 ),
 ( 8.673617379884035472E-19, 0.004041751736740998614 ),
 .UNSPECIFIED. ) ;
#29368 = ORIENTED_EDGE ( 'NONE', *, *, #38292, .T. ) ;
#29369 = CARTESIAN_POINT ( 'NONE',  ( 0.7056555295713305975, -24.67549844185508334, -41.05687446835462850 ) ) ;
#29370 = CARTESIAN_POINT ( 'NONE',  ( -2.739355103387247858, 12.65256472621583406, -7.922131834294089181 ) ) ;
#29371 = CARTESIAN_POINT ( 'NONE',  ( 0.9789233960466705575, 40.38468033015125513, 11.19885357810509952 ) ) ;
#29372 = CARTESIAN_POINT ( 'NONE',  ( 0.8744876279028306332, 28.81338721758086052, 39.75095932715638014 ) ) ;
#29373 = ADVANCED_FACE ( 'NONE', ( #17099 ), #15839, .F. ) ;
#29374 = VECTOR ( 'NONE', #48564, 1000.000000000000227 ) ;
#29375 = ORIENTED_EDGE ( 'NONE', *, *, #52542, .F. ) ;
#29376 = CARTESIAN_POINT ( 'NONE',  ( 5.896782393890504181, 16.58545041924871910, -11.37756218478521930 ) ) ;
#29377 = CARTESIAN_POINT ( 'NONE',  ( 5.860006189529234355, -36.27483683749414922, -31.78942168514599942 ) ) ;
#29378 = ORIENTED_EDGE ( 'NONE', *, *, #25562, .F. ) ;
#29379 = CARTESIAN_POINT ( 'NONE',  ( 1.827119703190781097, -36.65069040194725147, 22.58367210012827186 ) ) ;
#29380 = EDGE_CURVE ( 'NONE', #33929, #12652, #49907, .T. ) ;
#29381 = B_SPLINE_CURVE_WITH_KNOTS ( 'NONE', 3,
 ( #35643, #37489, #32469, #23072, #36879, #56867 ),
 .UNSPECIFIED., .F., .F.,
 ( 4, 2, 4 ),
 ( 1.208501758069982961E-16, 0.0002448718616795920121, 0.0004897437233590632441 ),
 .UNSPECIFIED. ) ;
#29382 = VERTEX_POINT ( 'NONE', #52433 ) ;
#29383 = ORIENTED_EDGE ( 'NONE', *, *, #2144, .T. ) ;
#29384 = DIRECTION ( 'NONE',  ( -1.000000000000000000, -0.000000000000000000, -0.000000000000000000 ) ) ;
#29385 = CARTESIAN_POINT ( 'NONE',  ( 0.9780303403264780648, 35.89220515824327151, -21.63536970503760060 ) ) ;
#29386 = CARTESIAN_POINT ( 'NONE',  ( 2.526552050251862358, -41.81191169914602312, 9.948123361606700854 ) ) ;
#29387 = ORIENTED_EDGE ( 'NONE', *, *, #50841, .F. ) ;
#29388 = CARTESIAN_POINT ( 'NONE',  ( 4.956653778116975495, -8.845409907521238679, 47.27023054223749909 ) ) ;
#29389 = FACE_OUTER_BOUND ( 'NONE', #24093, .T. ) ;
#29390 = CARTESIAN_POINT ( 'NONE',  ( 0.8551540677456715978, -38.56334384152412298, -28.44084013485158025 ) ) ;
#29391 = ORIENTED_EDGE ( 'NONE', *, *, #60624, .T. ) ;
#29392 = VERTEX_POINT ( 'NONE', #46851 ) ;
#29393 = DIRECTION ( 'NONE',  ( 0.000000000000000000, 0.000000000000000000, 1.000000000000000000 ) ) ;
#29394 = CARTESIAN_POINT ( 'NONE',  ( 0.5980271706414734822, 48.06821839532983631, -10.07450361757529045 ) ) ;
#29395 = PRODUCT_DEFINITION_SHAPE ( 'NONE', 'NONE',  #744 ) ;
#29396 = CARTESIAN_POINT ( 'NONE',  ( 1.000110580585050979, 38.83619784128909203, -15.75332409379547016 ) ) ;
#29397 = CARTESIAN_POINT ( 'NONE',  ( 0.000000000000000000, 0.000000000000000000, 0.000000000000000000 ) ) ;
#29398 = EDGE_LOOP ( 'NONE', ( #33716, #51939, #55927, #57515 ) ) ;
#29399 = DIRECTION ( 'NONE',  ( 0.000000000000000000, 0.000000000000000000, 1.000000000000000000 ) ) ;
#29400 = ORIENTED_EDGE ( 'NONE', *, *, #39412, .F. ) ;
#29401 = ADVANCED_FACE ( 'NONE', ( #32429 ), #24238, .F. ) ;
#29402 = CARTESIAN_POINT ( 'NONE',  ( 4.549368137175248350, 0.000000000000000000, 0.000000000000000000 ) ) ;
#29403 = CARTESIAN_POINT ( 'NONE',  ( 0.6021448801613057400, -19.63870604132753783, -45.00958079841749537 ) ) ;
#29404 = CARTESIAN_POINT ( 'NONE',  ( 0.5817216825391129387, -42.05894263787597964, -20.74319879843310233 ) ) ;
#29405 = AXIS2_PLACEMENT_3D ( 'NONE', #18026, #50285, #7349 ) ;
#29406 = DIRECTION ( 'NONE',  ( -1.000000000000000000, -0.000000000000000000, -0.000000000000000000 ) ) ;
#29407 = CARTESIAN_POINT ( 'NONE',  ( -6.016761891674564211, 16.31696541414285306, -9.424569481870079812 ) ) ;
#29408 = EDGE_CURVE ( 'NONE', #16773, #7089, #42703, .T. ) ;
#29409 = B_SPLINE_CURVE_WITH_KNOTS ( 'NONE', 3,
 ( #12072, #25519, #26445, #40580, #25834, #44656 ),
 .UNSPECIFIED., .F., .F.,
 ( 4, 2, 4 ),
 ( 0.000000000000000000, 0.0002293801035737085318, 0.0004587602071474170635 ),
 .UNSPECIFIED. ) ;
#29410 = CARTESIAN_POINT ( 'NONE',  ( 0.7048096507298579061, -7.115188260604195847, 47.58126109679088245 ) ) ;
#29411 = CARTESIAN_POINT ( 'NONE',  ( 0.8557997880470690211, 43.90420959842208504, -19.17299735371961944 ) ) ;
#29412 = EDGE_CURVE ( 'NONE', #41724, #14140, #26267, .T. ) ;
#29413 = CARTESIAN_POINT ( 'NONE',  ( 2.301529144917014325, 19.56451384728982035, 43.86846428170467505 ) ) ;
#29414 = EDGE_CURVE ( 'NONE', #8183, #31776, #11299, .T. ) ;
#29415 = DIRECTION ( 'NONE',  ( 0.000000000000000000, 0.000000000000000000, 1.000000000000000000 ) ) ;
#29416 = ADVANCED_FACE ( 'NONE', ( #61821 ), #43384, .F. ) ;
#29417 = CARTESIAN_POINT ( 'NONE',  ( 0.6064782688330854210, 40.70787696428524782, -23.28525712719063279 ) ) ;
#29418 = CARTESIAN_POINT ( 'NONE',  ( -99.50001199999974233, 5.000000000000001776, 1.500000000000000222 ) ) ;
#29419 = MECHANICAL_DESIGN_GEOMETRIC_PRESENTATION_REPRESENTATION (  '', ( #56416 ), #40456 ) ;
#29420 = CARTESIAN_POINT ( 'NONE',  ( 5.895596859100789899, 3.348897116308330091, 19.83212220910483481 ) ) ;
#29421 = EDGE_CURVE ( 'NONE', #2222, #41260, #18958, .T. ) ;
#29422 = ORIENTED_EDGE ( 'NONE', *, *, #256, .F. ) ;
#29423 = CARTESIAN_POINT ( 'NONE',  ( 3.376099380956842921, 11.76186387009555290, 6.431713763329955036 ) ) ;
#29424 = CARTESIAN_POINT ( 'NONE',  ( 3.376099380956838925, 3.553490516825327017, -12.92598502161052565 ) ) ;
#29425 = CARTESIAN_POINT ( 'NONE',  ( 0.5819845901640494645, 18.74765780149888172, -44.07435474487826355 ) ) ;
#29426 = CARTESIAN_POINT ( 'NONE',  ( 0.1064266379913941102, -30.09411261783711922, 30.88821943652560265 ) ) ;
#29427 = CARTESIAN_POINT ( 'NONE',  ( 4.963659409799330291, 39.92545197189578232, -20.22157859941687263 ) ) ;
#29428 = VERTEX_POINT ( 'NONE', #4808 ) ;
#29429 = CARTESIAN_POINT ( 'NONE',  ( 0.9741495583595167762, -37.35596046161881389, 21.11077839432123326 ) ) ;
#29430 = FACE_BOUND ( 'NONE', #39313, .T. ) ;
#29431 = CARTESIAN_POINT ( 'NONE',  ( 2.648799415243708655, 18.22894499609817132, 45.52167645879077185 ) ) ;
#29432 = ORIENTED_EDGE ( 'NONE', *, *, #37599, .T. ) ;
#29433 = CARTESIAN_POINT ( 'NONE',  ( 0.5797568665920711517, -35.19933622554232500, -30.98761103865694011 ) ) ;
#29434 = CARTESIAN_POINT ( 'NONE',  ( 0.7762777257811890319, 23.17763256463769395, 41.92424087089318618 ) ) ;
#29435 = ORIENTED_EDGE ( 'NONE', *, *, #52324, .F. ) ;
#29436 = CARTESIAN_POINT ( 'NONE',  ( 0.1073791018717578927, -16.95003405440338895, 39.65380858626186722 ) ) ;
#29437 = ORIENTED_EDGE ( 'NONE', *, *, #41588, .T. ) ;
#29438 = DIRECTION ( 'NONE',  ( 1.000000000000000000, 0.000000000000000000, 0.000000000000000000 ) ) ;
#29439 = ORIENTED_EDGE ( 'NONE', *, *, #5279, .T. ) ;
#29440 = CARTESIAN_POINT ( 'NONE',  ( 0.5998501479064708430, -41.92175333043635987, 23.59887241503281174 ) ) ;
#29441 = FACE_OUTER_BOUND ( 'NONE', #47089, .T. ) ;
#29442 = ORIENTED_EDGE ( 'NONE', *, *, #46972, .F. ) ;
#29443 = CARTESIAN_POINT ( 'NONE',  ( 0.8751705887134423323, -46.21789262997747727, -13.30665218149346529 ) ) ;
#29444 = EDGE_CURVE ( 'NONE', #24101, #3387, #25895, .T. ) ;
#29445 = ORIENTED_EDGE ( 'NONE', *, *, #54814, .F. ) ;
#29446 = DIRECTION ( 'NONE',  ( 0.000000000000000000, 0.000000000000000000, 1.000000000000000000 ) ) ;
#29447 = DIRECTION ( 'NONE',  ( -1.000000000000000000, -0.000000000000000000, -0.000000000000000000 ) ) ;
#29448 = ADVANCED_FACE ( 'NONE', ( #27723 ), #992, .F. ) ;
#29449 = CARTESIAN_POINT ( 'NONE',  ( 0.5834584762367748256, 40.25629450370218620, 24.05549296614785604 ) ) ;
#29450 = B_SPLINE_CURVE_WITH_KNOTS ( 'NONE', 3,
 ( #25325, #58506, #1498, #12177, #15943, #35057 ),
 .UNSPECIFIED., .F., .F.,
 ( 4, 2, 4 ),
 ( 0.000000000000000000, 0.0002293801035737090739, 0.0004587602071474181477 ),
 .UNSPECIFIED. ) ;
#29451 = VECTOR ( 'NONE', #20534, 1000.000000000000000 ) ;
#29452 = ORIENTED_EDGE ( 'NONE', *, *, #31851, .T. ) ;
#29453 = CARTESIAN_POINT ( 'NONE',  ( 5.895596859100789899, 3.348897116308330091, 19.83212220910483481 ) ) ;
#29454 = CARTESIAN_POINT ( 'NONE',  ( 0.5827359174754809246, 34.12345922495658357, -33.60976280407613359 ) ) ;
#29455 = CARTESIAN_POINT ( 'NONE',  ( 0.5817216825391131607, 32.27291863391528892, -34.02489786988552112 ) ) ;
#29456 = CARTESIAN_POINT ( 'NONE',  ( 0.3622758884714730732, 34.70015533914794759, 25.58609868863780434 ) ) ;
#29457 = ORIENTED_EDGE ( 'NONE', *, *, #56632, .T. ) ;
#29458 = PRODUCT_RELATED_PRODUCT_CATEGORY ( 'part', '', ( #16779 ) ) ;
#29459 = CARTESIAN_POINT ( 'NONE',  ( 4.691466044806103852, -14.01607102724572584, 42.32811009116530698 ) ) ;
#29460 = CARTESIAN_POINT ( 'NONE',  ( 0.1157506346131639274, -17.77584971692775184, 40.38514363777890281 ) ) ;
#29461 = AXIS2_PLACEMENT_3D ( 'NONE', #20175, #34578, #730 ) ;
#29462 = EDGE_LOOP ( 'NONE', ( #23896, #8945, #34005, #22001 ) ) ;
#29463 = CARTESIAN_POINT ( 'NONE',  ( 0.5807400328401637335, -18.83234461715215247, 44.04145271122558825 ) ) ;
#29464 = VERTEX_POINT ( 'NONE', #111 ) ;
#29465 = CARTESIAN_POINT ( 'NONE',  ( 4.322998006666165516, -32.40067585697774888, -35.39923696759002070 ) ) ;
#29466 = ORIENTED_EDGE ( 'NONE', *, *, #52231, .T. ) ;
#29467 = CARTESIAN_POINT ( 'NONE',  ( -6.016489644550736315, -4.872725758886318204, 18.20227673842142480 ) ) ;
#29468 = CARTESIAN_POINT ( 'NONE',  ( 1.227938101723747621, 22.18841447410770940, -36.73927144310489012 ) ) ;
#29469 = CARTESIAN_POINT ( 'NONE',  ( 3.661933894777899212, 46.83251759290548932, -4.398461192491206262 ) ) ;
#29470 = CARTESIAN_POINT ( 'NONE',  ( 0.7764139734771263734, -39.16768475757491075, 25.80567653905045944 ) ) ;
#29471 = ORIENTED_EDGE ( 'NONE', *, *, #1538, .F. ) ;
#29472 = DIRECTION ( 'NONE',  ( 0.000000000000000000, 0.000000000000000000, 1.000000000000000000 ) ) ;
#29473 = B_SPLINE_CURVE_WITH_KNOTS ( 'NONE', 3,
 ( #22746, #8955, #55938, #42194, #3612, #17433 ),
 .UNSPECIFIED., .F., .F.,
 ( 4, 2, 4 ),
 ( 0.000000000000000000, 0.0002447195606305751256, 0.0004894391212611502512 ),
 .UNSPECIFIED. ) ;
#29474 = DIRECTION ( 'NONE',  ( -1.000000000000000000, -0.000000000000000000, -0.000000000000000000 ) ) ;
#29475 = B_SPLINE_CURVE_WITH_KNOTS ( 'NONE', 3,
 ( #6389, #16448, #25532, #35576, #54634, #30846 ),
 .UNSPECIFIED., .F., .F.,
 ( 4, 2, 4 ),
 ( 1.053462964043502403E-17, 0.0002448709889506573193, 0.0004897419779013041218 ),
 .UNSPECIFIED. ) ;
#29476 = EDGE_CURVE ( 'NONE', #60067, #2855, #56919, .T. ) ;
#29477 = CARTESIAN_POINT ( 'NONE',  ( 0.8744876279028263033, 41.62483489565955352, -26.03311679934954626 ) ) ;
#29478 = CARTESIAN_POINT ( 'NONE',  ( 0.6067375320500736358, 46.44340905096879624, -11.71046088714702904 ) ) ;
#29479 = CIRCLE ( 'NONE', #19485, 46.67105333295396719 ) ;
#29480 =( BOUNDED_SURFACE ( )  B_SPLINE_SURFACE ( 3, 1, ( 
 ( #32621, #19443 ),
 ( #52010, #38262 ),
 ( #302, #27915 ),
 ( #8, #57306 ) ),
 .UNSPECIFIED., .F., .F., .F. ) 
 B_SPLINE_SURFACE_WITH_KNOTS ( ( 4, 4 ),
 ( 2, 2 ),
 ( 0.000000000000000000, 1.000000000000000000 ),
 ( 0.000000000000000000, 1.000000000000000000 ),
 .UNSPECIFIED. ) 
 GEOMETRIC_REPRESENTATION_ITEM ( )  RATIONAL_B_SPLINE_SURFACE ( (
 ( 1.000000000000000000, 1.000000000000000000),
 ( 0.9953485035131437453, 0.8621029689291523912),
 ( 0.9953485035131437453, 0.8621029689291523912),
 ( 1.000000000000000000, 1.000000000000000000) ) ) 
 REPRESENTATION_ITEM ( '' )  SURFACE ( )  );
#29481 = CARTESIAN_POINT ( 'NONE',  ( 2.282816707992306959, 23.71786607569137217, 40.54577407355216678 ) ) ;
#29482 = ADVANCED_FACE ( 'NONE', ( #13325 ), #23033, .T. ) ;
#29483 = CARTESIAN_POINT ( 'NONE',  ( 0.8753041380234530822, -47.71532843791157319, -11.59248721954040917 ) ) ;
#29484 = EDGE_CURVE ( 'NONE', #147, #52535, #4193, .T. ) ;
#29485 = EDGE_CURVE ( 'NONE', #226, #3592, #48679, .T. ) ;
#29486 = CARTESIAN_POINT ( 'NONE',  ( 0.8551540677456715978, -47.37911285756625546, 7.157691013574198458 ) ) ;
#29487 = CARTESIAN_POINT ( 'NONE',  ( 5.917102823773431552, -17.29995091781586325, 10.25677416602822767 ) ) ;
#29488 = CARTESIAN_POINT ( 'NONE',  ( 0.9745511491811736926, 30.58068216140377871, -30.09905547141324433 ) ) ;
#29489 = CARTESIAN_POINT ( 'NONE',  ( 0.1158403557922069033, -43.75702967194915516, -5.680023016853070317 ) ) ;
#29490 = CARTESIAN_POINT ( 'NONE',  ( 0.6041374136657475802, 44.37863742124641675, 18.57118264377553629 ) ) ;
#29491 = CARTESIAN_POINT ( 'NONE',  ( 5.960721111146673579, 12.50019045452716426, 16.28018152803696950 ) ) ;
#29492 = B_SPLINE_CURVE_WITH_KNOTS ( 'NONE', 3,
 ( #17537, #12542, #46363, #13459, #50721, #12858 ),
 .UNSPECIFIED., .F., .F.,
 ( 4, 2, 4 ),
 ( 9.929776742050823831E-18, 0.0002448709889506595419, 0.0004897419779013092176 ),
 .UNSPECIFIED. ) ;
#29493 = AXIS2_PLACEMENT_3D ( 'NONE', #59265, #16372, #8496 ) ;
#29494 = CARTESIAN_POINT ( 'NONE',  ( 0.5834872094924170582, 33.70665904794288537, 34.02770606800772413 ) ) ;
#29495 = CARTESIAN_POINT ( 'NONE',  ( 0.5997462898726536595, 23.17609050332929854, -43.29457771044543080 ) ) ;
#29496 = EDGE_LOOP ( 'NONE', ( #13052, #16205, #10817, #46638 ) ) ;
#29497 = B_SPLINE_CURVE_WITH_KNOTS ( 'NONE', 3,
 ( #8324, #46574, #35951, #32466, #21832, #31226, #26835, #41569, #60953, #46892, #18063, #8637, #27762, #7393, #3928, #50623 ),
 .UNSPECIFIED., .F., .F.,
 ( 4, 3, 3, 3, 3, 4 ),
 ( 1.995049841954898532E-17, 0.0002618515315864418684, 0.0003927756766341984791, 0.0005236998216950566973, 0.0007855159896329908745, 0.001047349442285928304 ),
 .UNSPECIFIED. ) ;
#29498 = LINE ( 'NONE', #24182, #50861 ) ;
#29499 = CIRCLE ( 'NONE', #16499, 47.09074272231896430 ) ;
#29500 = CARTESIAN_POINT ( 'NONE',  ( 0.9787464366903554369, -1.577301036837284176, 41.87894595533244768 ) ) ;
#29501 = CARTESIAN_POINT ( 'NONE',  ( 0.5988103622719990193, 28.80261254779987112, 38.53259676306930714 ) ) ;
#29502 = EDGE_LOOP ( 'NONE', ( #34115, #60114, #44262, #27148 ) ) ;
#29503 = CARTESIAN_POINT ( 'NONE',  ( 0.8744876279028263033, -14.81965677138014037, 46.80521149998127584 ) ) ;
#29504 = CONICAL_SURFACE ( 'NONE', #14551, 4.000000000000000000, 1.047197551196595855 ) ;
#29505 = CARTESIAN_POINT ( 'NONE',  ( 5.895596859100789899, -15.78680134203104579, -12.46214614742317295 ) ) ;
#29506 = ORIENTED_EDGE ( 'NONE', *, *, #24479, .T. ) ;
#29507 = VERTEX_POINT ( 'NONE', #19878 ) ;
#29508 = DIRECTION ( 'NONE',  ( 0.09722883295013597105, 0.9421506058508642978, 0.3207784125186792790 ) ) ;
#29509 = ORIENTED_EDGE ( 'NONE', *, *, #30816, .T. ) ;
#29510 = CARTESIAN_POINT ( 'NONE',  ( 0.5807400328401637335, 28.72484455891639854, 38.33001520688960539 ) ) ;
#29511 = ORIENTED_EDGE ( 'NONE', *, *, #23807, .T. ) ;
#29512 = ORIENTED_EDGE ( 'NONE', *, *, #31371, .F. ) ;
#29513 = CARTESIAN_POINT ( 'NONE',  ( -6.078726893082806448, 7.791390017580090088, 17.60932374802262146 ) ) ;
#29514 = ORIENTED_EDGE ( 'NONE', *, *, #39380, .F. ) ;
#29515 = CARTESIAN_POINT ( 'NONE',  ( 0.5848930533535030563, -46.80349522319535538, -2.950579143132510129 ) ) ;
#29516 = CARTESIAN_POINT ( 'NONE',  ( 4.956445790443991584, 25.79263028817558023, 39.39896284113483915 ) ) ;
#29517 = CARTESIAN_POINT ( 'NONE',  ( 0.9791128995231611620, -17.64544790140575614, -38.01283470888404992 ) ) ;
#29518 = ORIENTED_EDGE ( 'NONE', *, *, #2713, .T. ) ;
#29519 = CARTESIAN_POINT ( 'NONE',  ( -6.078075953587585900, -11.02105682227004024, -15.79023371478177218 ) ) ;
#29520 = EDGE_CURVE ( 'NONE', #19228, #6747, #58984, .T. ) ;
#29521 = CARTESIAN_POINT ( 'NONE',  ( 0.9789889208857696090, -39.55815494300130553, 13.83789274231708966 ) ) ;
#29522 = ORIENTED_EDGE ( 'NONE', *, *, #55338, .F. ) ;
#29523 = VERTEX_POINT ( 'NONE', #54265 ) ;
#29524 = CARTESIAN_POINT ( 'NONE',  ( 0.6027935024548037868, -18.57106801640327731, 44.37842839362943437 ) ) ;
#29525 = CARTESIAN_POINT ( 'NONE',  ( 2.643462169533613793, 44.89050350746127549, 17.09809940585677168 ) ) ;
#29526 = LINE ( 'NONE', #47418, #39273 ) ;
#29527 = CARTESIAN_POINT ( 'NONE',  ( 0.1310142868023692897, 0.6370537502136495167, -43.11885108606331585 ) ) ;
#29528 = FACE_OUTER_BOUND ( 'NONE', #32086, .T. ) ;
#29529 = EDGE_LOOP ( 'NONE', ( #25590, #50282, #18406, #48207 ) ) ;
#29530 = CARTESIAN_POINT ( 'NONE',  ( 0.5998501479064708430, -33.64490850298820845, -34.38546660123286358 ) ) ;
#29531 = CARTESIAN_POINT ( 'NONE',  ( 0.8760168074886960365, 0.8912768426706220160, -48.09529047980637273 ) ) ;
#29532 =( BOUNDED_SURFACE ( )  B_SPLINE_SURFACE ( 3, 1, ( 
 ( #41451, #61126 ),
 ( #22321, #42074 ),
 ( #51416, #4105 ),
 ( #60506, #3807 ) ),
 .UNSPECIFIED., .F., .F., .F. ) 
 B_SPLINE_SURFACE_WITH_KNOTS ( ( 4, 4 ),
 ( 2, 2 ),
 ( 0.000000000000000000, 1.000000000000000000 ),
 ( 0.000000000000000000, 1.000000000000000000 ),
 .UNSPECIFIED. ) 
 GEOMETRIC_REPRESENTATION_ITEM ( )  RATIONAL_B_SPLINE_SURFACE ( (
 ( 1.000000000000000000, 1.000000000000000000),
 ( 0.7269869731126817891, 0.9931720237060910339),
 ( 0.7269869731126817891, 0.9931720237060910339),
 ( 1.000000000000000000, 1.000000000000000000) ) ) 
 REPRESENTATION_ITEM ( '' )  SURFACE ( )  );
#29533 = CARTESIAN_POINT ( 'NONE',  ( 0.8560838555295223751, -30.97734773434455491, -35.22466126774295248 ) ) ;
#29534 = CARTESIAN_POINT ( 'NONE',  ( 4.975610109902397937, 7.237810502494091303, 48.37420290059321104 ) ) ;
#29535 = AXIS2_PLACEMENT_3D ( 'NONE', #35717, #40731, #1004 ) ;
#29536 = EDGE_LOOP ( 'NONE', ( #24406, #4595, #61774, #22615 ) ) ;
#29537 = CARTESIAN_POINT ( 'NONE',  ( 5.960221823109900008, -17.77840967225713698, -10.25807604135615136 ) ) ;
#29538 = CARTESIAN_POINT ( 'NONE',  ( 0.6026777506516367566, -14.13933751125005678, -47.02792282655249068 ) ) ;
#29539 = CARTESIAN_POINT ( 'NONE',  ( 1.479689385636123067, -5.869565535353596708, 43.67072298112183404 ) ) ;
#29541 = ORIENTED_EDGE ( 'NONE', *, *, #1619, .T. ) ;
#29540 = AXIS2_PLACEMENT_3D ( 'NONE', #5229, #43811, #43490 ) ;
#29542 = B_SPLINE_CURVE_WITH_KNOTS ( 'NONE', 3,
 ( #39193, #48871, #25066, #1241, #15686, #34789, #8114, #41353, #6857, #60405, #54467, #2159, #26604, #12225, #26924, #21917, #12529, #26296, #46352 ),
 .UNSPECIFIED., .F., .F.,
 ( 4, 3, 3, 3, 3, 3, 4 ),
 ( 1.517943542627326963E-18, 0.0002612768053151708417, 0.0003919133833142907628, 0.0005225499612322602114, 0.0006531865391693355248, 0.0008112755173415186647, 0.0009693688056799723562 ),
 .UNSPECIFIED. ) ;
#29543 = ORIENTED_EDGE ( 'NONE', *, *, #13123, .F. ) ;
#29544 = CARTESIAN_POINT ( 'NONE',  ( 0.5998501479064699549, 44.24259072156085182, -18.89267974119621485 ) ) ;
#29545 = LINE ( 'NONE', #15159, #54653 ) ;
#29546 = CARTESIAN_POINT ( 'NONE',  ( 0.9791128995231598298, 15.05754411609824928, -39.11020070822854677 ) ) ;
#29547 = DIRECTION ( 'NONE',  ( 0.000000000000000000, 0.000000000000000000, 1.000000000000000000 ) ) ;
#29548 = CARTESIAN_POINT ( 'NONE',  ( 0.6001305935487422083, 29.70149728382435228, -37.84751346122826021 ) ) ;
#29549 = CARTESIAN_POINT ( 'NONE',  ( 0.1135584504625007929, -31.99564635880365771, 30.38471106029520996 ) ) ;
#29550 = EDGE_CURVE ( 'NONE', #1001, #30413, #894, .T. ) ;
#29551 =( BOUNDED_SURFACE ( )  B_SPLINE_SURFACE ( 3, 1, ( 
 ( #28564, #47686 ),
 ( #32986, #18261 ),
 ( #4730, #17957 ),
 ( #52060, #13255 ) ),
 .UNSPECIFIED., .F., .F., .F. ) 
 B_SPLINE_SURFACE_WITH_KNOTS ( ( 4, 4 ),
 ( 2, 2 ),
 ( 0.000000000000000000, 1.000000000000000000 ),
 ( 0.000000000000000000, 1.000000000000000000 ),
 .UNSPECIFIED. ) 
 GEOMETRIC_REPRESENTATION_ITEM ( )  RATIONAL_B_SPLINE_SURFACE ( (
 ( 1.000000000000000000, 1.000000000000000000),
 ( 0.9732289882329797637, 0.9999525324661233672),
 ( 0.9732289882329797637, 0.9999525324661233672),
 ( 1.000000000000000000, 1.000000000000000000) ) ) 
 REPRESENTATION_ITEM ( '' )  SURFACE ( )  );
#29552 = FACE_OUTER_BOUND ( 'NONE', #2302, .T. ) ;
#29553 = CARTESIAN_POINT ( 'NONE',  ( 3.407937589446178528, -11.62731850632889241, 7.243367523630984017 ) ) ;
#29554 = CARTESIAN_POINT ( 'NONE',  ( 0.5804410086790514622, -29.86002002114359755, -36.16488706179379875 ) ) ;
#29555 = EDGE_CURVE ( 'NONE', #19642, #20940, #35278, .T. ) ;
#29556 = CARTESIAN_POINT ( 'NONE',  ( 0.1084644655670280733, 30.21121552070997751, -30.77359411724695093 ) ) ;
#29557 = CARTESIAN_POINT ( 'NONE',  ( 0.7954196712028460681, 38.68220069891169999, -28.58653687859125725 ) ) ;
#29558 = VERTEX_POINT ( 'NONE', #20185 ) ;
#29559 = ADVANCED_FACE ( 'NONE', ( #24874 ), #25791, .T. ) ;
#29560 = CARTESIAN_POINT ( 'NONE',  ( 0.1156495703730067576, -7.176750697220416697, -43.53661910002907831 ) ) ;
#29561 = CARTESIAN_POINT ( 'NONE',  ( 5.901463166500146684, -17.31230476672924112, -10.23728352662563879 ) ) ;
#29562 = CARTESIAN_POINT ( 'NONE',  ( 5.901764892641307547, -44.10106349910979162, -21.28585600080873164 ) ) ;
#29563 = FACE_OUTER_BOUND ( 'NONE', #58028, .T. ) ;
#29564 = B_SPLINE_CURVE_WITH_KNOTS ( 'NONE', 3,
 ( #37612, #13804, #29345, #28184 ),
 .UNSPECIFIED., .F., .F.,
 ( 4, 4 ),
 ( 2.165040709395311930E-17, 0.004444306975806114161 ),
 .UNSPECIFIED. ) ;
#29565 = CARTESIAN_POINT ( 'NONE',  ( 4.553261556744875094, 0.000000000000000000, 0.000000000000000000 ) ) ;
#29566 = CARTESIAN_POINT ( 'NONE',  ( 0.5806925824938499181, -13.37132486740634540, -44.94919391528445374 ) ) ;
#29567 = CARTESIAN_POINT ( 'NONE',  ( 4.960386119450143738, -37.40422633003237962, 22.70154878690114941 ) ) ;
#29568 = CARTESIAN_POINT ( 'NONE',  ( 0.9745511491811738036, -26.39034508612560259, 33.83313387735780964 ) ) ;
#29569 =( REPRESENTATION_RELATIONSHIP ('NONE','NONE', #44881, #19619 ) REPRESENTATION_RELATIONSHIP_WITH_TRANSFORMATION ( #4200 )SHAPE_REPRESENTATION_RELATIONSHIP( ) );
#29570 = CARTESIAN_POINT ( 'NONE',  ( 5.960221823109900008, -16.28736530777582558, -12.49086489703221936 ) ) ;
#29571 = CARTESIAN_POINT ( 'NONE',  ( 0.8751705887134423323, 46.21789262997739201, 13.30665218149378504 ) ) ;
#29572 = DIRECTION ( 'NONE',  ( -1.000000000000000000, -1.836909530733580185E-16, 1.836909530733574022E-16 ) ) ;
#29574 = ORIENTED_EDGE ( 'NONE', *, *, #56988, .F. ) ;
#29573 = CARTESIAN_POINT ( 'NONE',  ( 5.981074661064941900, -16.27808421740017764, -12.50143471347275614 ) ) ;
#29575 = ORIENTED_EDGE ( 'NONE', *, *, #54148, .F. ) ;
#29576 = EDGE_CURVE ( 'NONE', #13746, #44371, #6826, .T. ) ;
#29577 = CARTESIAN_POINT ( 'NONE',  ( 0.7764146366350265227, -24.48247828494958611, 40.00810831189270544 ) ) ;
#29578 = CARTESIAN_POINT ( 'NONE',  ( 0.5549461598389364703, 43.94904939407230415, -3.701182625080478683 ) ) ;
#29579 = CARTESIAN_POINT ( 'NONE',  ( 1.827326673878742813, -34.89023127623437404, 25.21837361081529849 ) ) ;
#29580 = EDGE_CURVE ( 'NONE', #57526, #37539, #1967, .T. ) ;
#29581 = ORIENTED_EDGE ( 'NONE', *, *, #25063, .F. ) ;
#29582 = CARTESIAN_POINT ( 'NONE',  ( 0.1103310638050662013, -11.24099191367028183, 41.63362651001246206 ) ) ;
#29583 = DIRECTION ( 'NONE',  ( -1.000000000000000000, -0.000000000000000000, -0.000000000000000000 ) ) ;
#29584 = CARTESIAN_POINT ( 'NONE',  ( 5.896278296736517710, -19.39678151694244690, 5.319008027666769500 ) ) ;
#29585 = ORIENTED_EDGE ( 'NONE', *, *, #35275, .T. ) ;
#29586 = ORIENTED_EDGE ( 'NONE', *, *, #1687, .F. ) ;
#29587 = CARTESIAN_POINT ( 'NONE',  ( 0.6030672727741701600, -23.97812608463503992, -41.70584815505880272 ) ) ;
#29588 = FACE_OUTER_BOUND ( 'NONE', #14447, .T. ) ;
#29589 = CARTESIAN_POINT ( 'NONE',  ( 4.549368137175248350, -13.99871866169391765, 40.58005590356665948 ) ) ;
#29590 = CARTESIAN_POINT ( 'NONE',  ( 1.479689385636123067, -11.40586458698099648, 42.56160356813574452 ) ) ;
#29592 = CARTESIAN_POINT ( 'NONE',  ( 0.2940135542859015905, 5.036457902034579881, 43.82778388753477827 ) ) ;
#29591 = AXIS2_PLACEMENT_3D ( 'NONE', #13559, #37372, #13254 ) ;
#29593 = CARTESIAN_POINT ( 'NONE',  ( 0.7056759521544987424, -29.63218968554087240, -36.35494689250850797 ) ) ;
#29594 = EDGE_CURVE ( 'NONE', #4682, #3337, #23281, .T. ) ;
#29595 = CARTESIAN_POINT ( 'NONE',  ( 4.975610109902397937, -33.30777373088901072, 35.81957029655259817 ) ) ;
#29596 = EDGE_LOOP ( 'NONE', ( #801, #44766 ) ) ;
#29597 = AXIS2_PLACEMENT_3D ( 'NONE', #19797, #34510, #5647 ) ;
#29598 = ORIENTED_EDGE ( 'NONE', *, *, #32587, .T. ) ;
#29599 = CARTESIAN_POINT ( 'NONE',  ( -6.078075953587585900, 7.799379819826517846, -17.60581860275797439 ) ) ;
#29600 = CARTESIAN_POINT ( 'NONE',  ( 4.390527457369401532, 43.93270324789031633, 0.3208145280799595822 ) ) ;
#29601 = ORIENTED_EDGE ( 'NONE', *, *, #31336, .F. ) ;
#29602 = DIRECTION ( 'NONE',  ( 0.000000000000000000, 0.000000000000000000, 1.000000000000000000 ) ) ;
#29603 = CARTESIAN_POINT ( 'NONE',  ( 0.5782707292762423457, -2.290569157858090676, -46.84538020595721264 ) ) ;
#29604 = CARTESIAN_POINT ( 'NONE',  ( 4.956653778116992370, 31.29546495791903027, -36.51451553856384180 ) ) ;
#29605 = CARTESIAN_POINT ( 'NONE',  ( 0.1158403557922069033, -40.88518614858649869, -16.59342824069968003 ) ) ;
#29606 = ORIENTED_EDGE ( 'NONE', *, *, #27370, .F. ) ;
#29607 = CARTESIAN_POINT ( 'NONE',  ( 1.231276596079881047, -23.26513148155264332, 34.87134107206281186 ) ) ;
#29608 = CARTESIAN_POINT ( 'NONE',  ( 0.9757892942422806692, -42.54806590760156126, -5.549787678908827182 ) ) ;
#29609 = CARTESIAN_POINT ( 'NONE',  ( 0.5807400328401574052, -6.791881299635910807, 47.41494605191441281 ) ) ;
#29610 = CARTESIAN_POINT ( 'NONE',  ( 0.8551540677456834771, 41.03346287276463045, -24.74404575822732255 ) ) ;
#29611 = B_SPLINE_CURVE_WITH_KNOTS ( 'NONE', 3,
 ( #18485, #19418, #38850, #24411 ),
 .UNSPECIFIED., .F., .F.,
 ( 4, 4 ),
 ( 0.000000000000000000, 0.004445488388166991649 ),
 .UNSPECIFIED. ) ;
#29612 = ORIENTED_EDGE ( 'NONE', *, *, #2465, .T. ) ;
#29613 = CARTESIAN_POINT ( 'NONE',  ( 0.8551540677456715978, 46.51172240253137602, -11.51835730326430962 ) ) ;
#29614 = ORIENTED_EDGE ( 'NONE', *, *, #29715, .F. ) ;
#29615 = CARTESIAN_POINT ( 'NONE',  ( 3.240649175237395152, 41.13842520339412800, 15.58508547241233444 ) ) ;
#29616 = B_SPLINE_CURVE_WITH_KNOTS ( 'NONE', 3,
 ( #32864, #61027, #60707, #7468 ),
 .UNSPECIFIED., .F., .F.,
 ( 4, 4 ),
 ( 1.192622389734054877E-18, 0.004444878191957686922 ),
 .UNSPECIFIED. ) ;
#29617 = ORIENTED_EDGE ( 'NONE', *, *, #55857, .T. ) ;
#29618 = CARTESIAN_POINT ( 'NONE',  ( 0.6001305935487422083, 12.95698906763808900, -46.33281397023051795 ) ) ;
#29619 = CARTESIAN_POINT ( 'NONE',  ( 0.5806925824938499181, 42.95845041307745760, 18.80940989108190209 ) ) ;
#29620 = CARTESIAN_POINT ( 'NONE',  ( 0.3676999524040323597, -42.45338881270421894, -11.98584004733086061 ) ) ;
#29621 = CARTESIAN_POINT ( 'NONE',  ( 1.231276596079881047, 41.91134057782998212, 0.8463462572780127147 ) ) ;
#29622 = CARTESIAN_POINT ( 'NONE',  ( 5.917102823773431552, -7.220356195166569790, 18.77115272077508124 ) ) ;
#29623 = DIRECTION ( 'NONE',  ( -1.000000000000000000, -0.000000000000000000, -0.000000000000000000 ) ) ;
#29624 = FACE_OUTER_BOUND ( 'NONE', #42265, .T. ) ;
#29625 = CARTESIAN_POINT ( 'NONE',  ( 1.154321713695927398, 34.54400171733340130, -25.46626713715426149 ) ) ;
#29626 = ORIENTED_EDGE ( 'NONE', *, *, #27414, .F. ) ;
#29628 = EDGE_CURVE ( 'NONE', #31436, #61473, #9074, .T. ) ;
#29627 = CARTESIAN_POINT ( 'NONE',  ( 0.9730545539215883499, 39.83279466599061891, -15.95224156741785393 ) ) ;
#29629 = CARTESIAN_POINT ( 'NONE',  ( 4.549368137175248350, -40.58005590356681580, -13.99871866169351442 ) ) ;
#29630 = CARTESIAN_POINT ( 'NONE',  ( 4.060580049360325461, -15.64928826502552006, 41.06783986475723225 ) ) ;
#29631 = ORIENTED_EDGE ( 'NONE', *, *, #21358, .F. ) ;
#29632 = CONICAL_SURFACE ( 'NONE', #51624, 43.08621763946400307, 1.568696531533066763 ) ;
#29633 = CIRCLE ( 'NONE', #55647, 12.49999999999999822 ) ;
#29634 = EDGE_CURVE ( 'NONE', #52990, #46812, #31484, .T. ) ;
#29635 = CARTESIAN_POINT ( 'NONE',  ( 0.8751705887134553219, 34.63284514348538323, 33.37254303619566542 ) ) ;
#29636 = CARTESIAN_POINT ( 'NONE',  ( 2.643462169533613793, 28.13401304854720308, -38.93558293168510431 ) ) ;
#29637 = FACE_OUTER_BOUND ( 'NONE', #52477, .T. ) ;
#29638 = CARTESIAN_POINT ( 'NONE',  ( 5.860006189529234355, -3.171667470662203669, -48.12869875779312423 ) ) ;
#29639 = B_SPLINE_CURVE_WITH_KNOTS ( 'NONE', 3,
 ( #42746, #60898, #42147, #13940, #33351, #37129 ),
 .UNSPECIFIED., .F., .F.,
 ( 4, 2, 4 ),
 ( 1.870693080156664505E-17, 0.0002293755540694324298, 0.0004587511081388461571 ),
 .UNSPECIFIED. ) ;
#29640 = CARTESIAN_POINT ( 'NONE',  ( 0.6028777368367060907, -19.95745447572438636, 44.86914129065165469 ) ) ;
#29641 = DIRECTION ( 'NONE',  ( -1.000000000000000000, -0.000000000000000000, -0.000000000000000000 ) ) ;
#29642 = ADVANCED_FACE ( 'NONE', ( #39927 ), #45859, .F. ) ;
#29643 = CARTESIAN_POINT ( 'NONE',  ( 15.00000000000001776, -80.00000000000001421, 2.037316199841804408E-13 ) ) ;
#29644 = CARTESIAN_POINT ( 'NONE',  ( 0.3622758884714730732, -41.85013935980095567, -10.35929834645908265 ) ) ;
#29645 = B_SPLINE_CURVE_WITH_KNOTS ( 'NONE', 3,
 ( #60859, #55230, #7944, #22353, #17979, #3226 ),
 .UNSPECIFIED., .F., .F.,
 ( 4, 2, 4 ),
 ( 7.757919228897728493E-18, 0.0002291472222819922579, 0.0004582944445639767638 ),
 .UNSPECIFIED. ) ;
#29646 = CARTESIAN_POINT ( 'NONE',  ( 0.9968887458511638267, 29.87314546208230226, 30.80284987750020775 ) ) ;
#29647 = VECTOR ( 'NONE', #6648, 999.9999999999998863 ) ;
#29648 = CARTESIAN_POINT ( 'NONE',  ( 0.9788927965476029724, 29.03256182720962641, -30.22328516857536940 ) ) ;
#29650 = EDGE_LOOP ( 'NONE', ( #61230, #16932, #61772, #37820 ) ) ;
#29649 = DIRECTION ( 'NONE',  ( 0.000000000000000000, 0.000000000000000000, 1.000000000000000000 ) ) ;
#29651 = ORIENTED_EDGE ( 'NONE', *, *, #45996, .T. ) ;
#29652 = CARTESIAN_POINT ( 'NONE',  ( 0.5832366564991512403, -12.13301812590381346, 46.33368520589910844 ) ) ;
#29653 = DIRECTION ( 'NONE',  ( -1.000000000000000000, -1.836909530733573776E-16, 1.925929944387235853E-32 ) ) ;
#29654 = CARTESIAN_POINT ( 'NONE',  ( 0.1100247026804066219, 16.34612806822703490, 39.90641708963718060 ) ) ;
#29655 = EDGE_CURVE ( 'NONE', #6741, #58555, #43950, .T. ) ;
#29656 = CARTESIAN_POINT ( 'NONE',  ( 4.962356264823596597, 39.89814050050772920, 13.39305724859313429 ) ) ;
#29657 = CARTESIAN_POINT ( 'NONE',  ( 0.1129192098497447394, 41.72114954716796120, -14.36305915353690743 ) ) ;
#29658 = CARTESIAN_POINT ( 'NONE',  ( 0.1158403557922069033, 9.855458665879178071, -43.00942038285294444 ) ) ;
#29659 = ORIENTED_EDGE ( 'NONE', *, *, #24762, .F. ) ;
#29660 = ORIENTED_EDGE ( 'NONE', *, *, #39686, .T. ) ;
#29661 = DIRECTION ( 'NONE',  ( 0.000000000000000000, 0.000000000000000000, -1.000000000000000000 ) ) ;
#29662 = CARTESIAN_POINT ( 'NONE',  ( 0.3622758884714730732, -10.35929834645951964, 41.85013935980084199 ) ) ;
#29663 = DIRECTION ( 'NONE',  ( 0.000000000000000000, 0.000000000000000000, 1.000000000000000000 ) ) ;
#29664 = VERTEX_POINT ( 'NONE', #36141 ) ;
#29665 = CARTESIAN_POINT ( 'NONE',  ( 3.376099380956838925, -3.529868236344142929, -12.93245583275333743 ) ) ;
#29666 = CARTESIAN_POINT ( 'NONE',  ( 0.5837799406558230597, -25.31068968778611250, -39.47926718045562211 ) ) ;
#29667 = ORIENTED_EDGE ( 'NONE', *, *, #44754, .F. ) ;
#29668 = LINE ( 'NONE', #216, #26960 ) ;
#29669 = AXIS2_PLACEMENT_3D ( 'NONE', #33053, #52125, #4495 ) ;
#29670 = VERTEX_POINT ( 'NONE', #7592 ) ;
#29671 = DIRECTION ( 'NONE',  ( -1.000000000000000000, -3.135800716341471541E-16, -1.298891185607920445E-16 ) ) ;
#29672 = CARTESIAN_POINT ( 'NONE',  ( -6.063463321072276813, -1.864608017455207767, -19.16621218239826518 ) ) ;
#29673 = VERTEX_POINT ( 'NONE', #11708 ) ;
#29674 = CONICAL_SURFACE ( 'NONE', #33733, 43.08621763946400307, 1.568696531533066763 ) ;
#29675 = CARTESIAN_POINT ( 'NONE',  ( 5.901463166500145796, -17.29756286482720284, -10.26217273670579466 ) ) ;
#29676 = CARTESIAN_POINT ( 'NONE',  ( 3.680882792899936362, -27.71664061799177503, 39.15943299201938999 ) ) ;
#29677 = CARTESIAN_POINT ( 'NONE',  ( 4.975801465491695552, -45.18341283946470099, 15.94009207552969620 ) ) ;
#29678 = DIRECTION ( 'NONE',  ( 0.000000000000000000, 0.000000000000000000, 1.000000000000000000 ) ) ;
#29679 = EDGE_CURVE ( 'NONE', #7082, #7098, #36446, .T. ) ;
#29680 = ORIENTED_EDGE ( 'NONE', *, *, #61302, .T. ) ;
#29681 = EDGE_CURVE ( 'NONE', #14441, #2552, #26711, .T. ) ;
#29682 = CARTESIAN_POINT ( 'NONE',  ( 2.282816707992308736, -46.27578434998796553, -8.065280478779142115 ) ) ;
#29683 = ORIENTED_EDGE ( 'NONE', *, *, #47185, .F. ) ;
#29684 = CARTESIAN_POINT ( 'NONE',  ( 4.975801465491695552, -47.84403947906842092, -2.564218696447329027 ) ) ;
#29685 = ORIENTED_EDGE ( 'NONE', *, *, #48374, .T. ) ;
#29686 = CARTESIAN_POINT ( 'NONE',  ( -6.072942160501519027, 18.62280723096618118, 4.898490903053114742 ) ) ;
#29687 = EDGE_CURVE ( 'NONE', #43286, #31957, #49334, .T. ) ;
#29688 = EDGE_LOOP ( 'NONE', ( #7452, #44705, #20223, #47006 ) ) ;
#29689 = CARTESIAN_POINT ( 'NONE',  ( 4.975610109902397937, 13.36434394399761949, -47.05150069959838532 ) ) ;
#29691 = AXIS2_PLACEMENT_3D ( 'NONE', #20730, #35147, #54209 ) ;
#29690 = CARTESIAN_POINT ( 'NONE',  ( 5.965394784446458765, 17.78272165951786832, 10.25014670152121177 ) ) ;
#29692 = LINE ( 'NONE', #48807, #59264 ) ;
#29693 = ORIENTED_EDGE ( 'NONE', *, *, #47986, .T. ) ;
#29694 = CARTESIAN_POINT ( 'NONE',  ( 0.6001305935487422083, -17.92615948558569272, 44.64600790884025372 ) ) ;
#29695 = CARTESIAN_POINT ( 'NONE',  ( 0.5819845901640494645, -6.701564444318020897, 47.42480841519687118 ) ) ;
#29696 = CARTESIAN_POINT ( 'NONE',  ( 0.1140933569871964703, -38.63098921247078010, 21.32127159786375614 ) ) ;
#29697 = ORIENTED_EDGE ( 'NONE', *, *, #23432, .T. ) ;
#29698 = ORIENTED_EDGE ( 'NONE', *, *, #28269, .T. ) ;
#29699 = CARTESIAN_POINT ( 'NONE',  ( 4.553261556744875094, 22.57774691820428714, 37.68003330573307608 ) ) ;
#29700 = CARTESIAN_POINT ( 'NONE',  ( 1.227938101723748288, -42.91134962331486946, -0.8460948827229646252 ) ) ;
#29701 = CARTESIAN_POINT ( 'NONE',  ( 4.549368137175248350, 8.582197505784431968, -42.06008734272388239 ) ) ;
#29702 = DIRECTION ( 'NONE',  ( 0.09835009131224552170, -0.9164135549743811504, 0.3879606369183475900 ) ) ;
#29703 = CARTESIAN_POINT ( 'NONE',  ( 1.827326673878743701, -27.17438009792357434, 33.38933471001428899 ) ) ;
#29704 = LINE ( 'NONE', #30321, #36842 ) ;
#29705 = ORIENTED_EDGE ( 'NONE', *, *, #15648, .T. ) ;
#29706 = EDGE_CURVE ( 'NONE', #46812, #28087, #32049, .T. ) ;
#29707 = CARTESIAN_POINT ( 'NONE',  ( 5.896782393890504181, -11.92541098582113612, -16.19600752337651883 ) ) ;
#29708 = ORIENTED_EDGE ( 'NONE', *, *, #57658, .F. ) ;
#29709 = EDGE_CURVE ( 'NONE', #45591, #53833, #29926, .T. ) ;
#29710 = CARTESIAN_POINT ( 'NONE',  ( 0.3622758884714600280, -25.58609868863743841, -34.70015533914819628 ) ) ;
#29711 = FACE_OUTER_BOUND ( 'NONE', #21316, .T. ) ;
#29712 = CARTESIAN_POINT ( 'NONE',  ( 0.6000166863083090663, 41.44150143800037966, 26.35195325346236928 ) ) ;
#29713 = FACE_OUTER_BOUND ( 'NONE', #7722, .T. ) ;
#29714 = CARTESIAN_POINT ( 'NONE',  ( -6.017396004339686577, 16.31807101179383679, -9.422598049764452810 ) ) ;
#29715 = EDGE_CURVE ( 'NONE', #41352, #7929, #41151, .T. ) ;
#29716 = CARTESIAN_POINT ( 'NONE',  ( 0.8554163680231708922, 31.95314001164559059, 34.35407277904604229 ) ) ;
#29717 = LINE ( 'NONE', #15644, #37742 ) ;
#29718 = CARTESIAN_POINT ( 'NONE',  ( 4.834790513006553603, 46.91907382339847032, -5.584787594785217912 ) ) ;
#29719 = AXIS2_PLACEMENT_3D ( 'NONE', #11282, #30369, #25373 ) ;
#29720 = CARTESIAN_POINT ( 'NONE',  ( 0.8554163680231720024, -41.45413358837884488, 21.97180651536554308 ) ) ;
#29721 = FACE_OUTER_BOUND ( 'NONE', #50848, .T. ) ;
#29722 = AXIS2_PLACEMENT_3D ( 'NONE', #30695, #44836, #59195 ) ;
#29723 = AXIS2_PLACEMENT_3D ( 'NONE', #24444, #51709, #28836 ) ;
#29724 = DIRECTION ( 'NONE',  ( 0.09835009131224564660, -0.6119264800004838856, 0.7847759187265433978 ) ) ;
#29725 = EDGE_CURVE ( 'NONE', #13345, #26826, #43377, .T. ) ;
#29726 = CARTESIAN_POINT ( 'NONE',  ( 4.060580049360325461, -19.88058780675999415, -39.19476907467264226 ) ) ;
#29727 = CARTESIAN_POINT ( 'NONE',  ( 0.5997462898726536595, 4.195097405482933972, 48.92803682862026449 ) ) ;
#29728 =( BOUNDED_SURFACE ( )  B_SPLINE_SURFACE ( 3, 1, ( 
 ( #28852, #43288 ),
 ( #25080, #25386 ),
 ( #57957, #47975 ),
 ( #15081, #34497 ) ),
 .UNSPECIFIED., .F., .F., .F. ) 
 B_SPLINE_SURFACE_WITH_KNOTS ( ( 4, 4 ),
 ( 2, 2 ),
 ( 0.000000000000000000, 1.000000000000000000 ),
 ( 0.000000000000000000, 1.000000000000000000 ),
 .UNSPECIFIED. ) 
 GEOMETRIC_REPRESENTATION_ITEM ( )  RATIONAL_B_SPLINE_SURFACE ( (
 ( 1.000000000000000000, 1.000000000000000000),
 ( 0.9953390228620291325, 0.8624445117760984880),
 ( 0.9953390228620291325, 0.8624445117760984880),
 ( 1.000000000000000000, 1.000000000000000000) ) ) 
 REPRESENTATION_ITEM ( '' )  SURFACE ( )  );
#29729 = ORIENTED_EDGE ( 'NONE', *, *, #24112, .T. ) ;
#29730 = CARTESIAN_POINT ( 'NONE',  ( 4.960386119450151732, -4.847629508247444541, 43.48490488460461023 ) ) ;
#29731 = AXIS2_PLACEMENT_3D ( 'NONE', #19429, #57599, #1219 ) ;
#29732 = CARTESIAN_POINT ( 'NONE',  ( 0.8554163680231708922, -39.19027442586736498, 25.79395013442155005 ) ) ;
#29733 = CARTESIAN_POINT ( 'NONE',  ( 0.5549461598389366923, 24.50808299993816419, -36.66840006238268046 ) ) ;
#29734 = CARTESIAN_POINT ( 'NONE',  ( 5.910764540655177868, 12.97317151014736503, 15.36873642943569251 ) ) ;
#29735 = DIRECTION ( 'NONE',  ( 0.000000000000000000, 0.000000000000000000, 1.000000000000000000 ) ) ;
#29736 = ORIENTED_EDGE ( 'NONE', *, *, #34146, .T. ) ;
#29737 = DIRECTION ( 'NONE',  ( 0.1024043820194936449, 0.9641676559171069583, 0.2447326578667362307 ) ) ;
#29738 = LINE ( 'NONE', #44494, #49972 ) ;
#29739 = PLANE ( 'NONE',  #46560 ) ;
#29740 = VERTEX_POINT ( 'NONE', #3203 ) ;
#29741 = CARTESIAN_POINT ( 'NONE',  ( 0.1073791018717483448, -30.83464511437118816, -30.14884492832378626 ) ) ;
#29742 = CARTESIAN_POINT ( 'NONE',  ( 1.000110580585050979, 25.38656982076186353, -33.34575768381163385 ) ) ;
#29743 = CONICAL_SURFACE ( 'NONE', #2733, 43.92652462719577500, 1.486293639869522343 ) ;
#29744 = ORIENTED_EDGE ( 'NONE', *, *, #29755, .F. ) ;
#29745 = CARTESIAN_POINT ( 'NONE',  ( 4.694002226626921015, 32.50760209236046450, -31.96154842386231820 ) ) ;
#29746 = VERTEX_POINT ( 'NONE', #26401 ) ;
#29747 = CARTESIAN_POINT ( 'NONE',  ( 3.678748215320119197, -38.11576136296564243, 30.75388674657139276 ) ) ;
#29748 = ORIENTED_EDGE ( 'NONE', *, *, #56427, .F. ) ;
#29749 = CARTESIAN_POINT ( 'NONE',  ( -7.853389858698435866, 8.173624800449486472, 5.691590806814991163E-14 ) ) ;
#29750 = CARTESIAN_POINT ( 'NONE',  ( 0.1129192098497447394, 20.83764143887560749, 38.89401608281161060 ) ) ;
#29751 = EDGE_CURVE ( 'NONE', #42659, #13798, #30208, .T. ) ;
#29752 = ORIENTED_EDGE ( 'NONE', *, *, #47183, .T. ) ;
#29753 = CARTESIAN_POINT ( 'NONE',  ( 0.8744876279028263033, -35.88078294188978390, 33.50999053799454686 ) ) ;
#29754 = EDGE_LOOP ( 'NONE', ( #16296, #46730, #31149, #20492 ) ) ;
#29755 = EDGE_CURVE ( 'NONE', #35032, #42568, #51223, .T. ) ;
#29757 = B_SPLINE_CURVE_WITH_KNOTS ( 'NONE', 3,
 ( #56634, #36951, #23138, #46646, #32234, #51313 ),
 .UNSPECIFIED., .F., .F.,
 ( 4, 2, 4 ),
 ( 8.541065402288459803E-17, 0.0002293366620881456082, 0.0004586733241762058354 ),
 .UNSPECIFIED. ) ;
#29756 = CARTESIAN_POINT ( 'NONE',  ( 0.3622758884714600280, 4.808133778521302304, 42.84426538328732903 ) ) ;
#29758 = CARTESIAN_POINT ( 'NONE',  ( 0.6039202388192952409, -45.58380534490273561, 18.26692100839678545 ) ) ;
#29759 = B_SPLINE_CURVE_WITH_KNOTS ( 'NONE', 3,
 ( #27820, #46952, #41329, #14901 ),
 .UNSPECIFIED., .F., .F.,
 ( 4, 4 ),
 ( 0.000000000000000000, 0.004041751736741002084 ),
 .UNSPECIFIED. ) ;
#29760 = EDGE_CURVE ( 'NONE', #45115, #55224, #24721, .T. ) ;
#29761 = VERTEX_POINT ( 'NONE', #16709 ) ;
#29762 = CARTESIAN_POINT ( 'NONE',  ( 0.5980271706414734822, 43.94069670602981859, -21.93773953328744852 ) ) ;
#29763 = CARTESIAN_POINT ( 'NONE',  ( 4.060580049360325461, -36.55588913668041329, -24.39538201762661629 ) ) ;
#29764 = AXIS2_PLACEMENT_3D ( 'NONE', #4633, #4957, #48502 ) ;
#29765 = CARTESIAN_POINT ( 'NONE',  ( 0.5837800304671207918, 32.63445599095994965, -33.67832558714280111 ) ) ;
#29766 = VECTOR ( 'NONE', #11937, 1000.000000000000000 ) ;
#29767 = CARTESIAN_POINT ( 'NONE',  ( 0.1129192098497455998, -6.563350895508677674, -43.63340707310831590 ) ) ;
#29769 = EDGE_CURVE ( 'NONE', #30886, #18069, #35942, .T. ) ;
#29768 = VERTEX_POINT ( 'NONE', #35829 ) ;
#29770 = CARTESIAN_POINT ( 'NONE',  ( 0.5988103564986361205, 6.880138274944319399, 47.61318305157298170 ) ) ;
#29771 = CARTESIAN_POINT ( 'NONE',  ( 0.8560838555295223751, 27.08392101972057731, -38.29926965725677235 ) ) ;
#29772 = B_SPLINE_CURVE_WITH_KNOTS ( 'NONE', 3,
 ( #56386, #13501, #18502, #37627 ),
 .UNSPECIFIED., .F., .F.,
 ( 4, 4 ),
 ( 0.000000000000000000, 0.005014147105413715132 ),
 .UNSPECIFIED. ) ;
#29773 = VERTEX_POINT ( 'NONE', #9145 ) ;
#29774 = CARTESIAN_POINT ( 'NONE',  ( 0.5824935313925976299, -46.81422942724466196, -2.768772324900471649 ) ) ;
#29775 = CONICAL_SURFACE ( 'NONE', #4277, 5.612499999999999822, 0.4883339510564123076 ) ;
#29776 = VERTEX_POINT ( 'NONE', #47680 ) ;
#29777 = CARTESIAN_POINT ( 'NONE',  ( 2.299746137290197723, 38.15858813809509087, 30.79291296700212044 ) ) ;
#29778 = EDGE_CURVE ( 'NONE', #54614, #4627, #13522, .T. ) ;
#29779 = CARTESIAN_POINT ( 'NONE',  ( 0.1154773475650540393, 25.39148992311906028, 36.08622825303670112 ) ) ;
#29780 = ORIENTED_EDGE ( 'NONE', *, *, #39792, .F. ) ;
#29781 = CARTESIAN_POINT ( 'NONE',  ( 0.9789233960466698914, -12.29085669408485160, -40.06584041996139689 ) ) ;
#29782 = CARTESIAN_POINT ( 'NONE',  ( 0.8751705887134553219, 37.60752970653828697, -29.98056538504921065 ) ) ;
#29783 = CARTESIAN_POINT ( 'NONE',  ( 50.67563028805193426, 12.21587082446438011, -2.649999999999992362 ) ) ;
#29784 = DIRECTION ( 'NONE',  ( 0.000000000000000000, 0.000000000000000000, -1.000000000000000000 ) ) ;
#29785 = EDGE_CURVE ( 'NONE', #51706, #9752, #23254, .T. ) ;
#29786 = B_SPLINE_CURVE_WITH_KNOTS ( 'NONE', 3,
 ( #6886, #11953, #12558, #54821, #8435, #16629 ),
 .UNSPECIFIED., .F., .F.,
 ( 4, 2, 4 ),
 ( 0.000000000000000000, 0.0002447195606305759387, 0.0004894391212611518775 ),
 .UNSPECIFIED. ) ;
#29787 = ORIENTED_EDGE ( 'NONE', *, *, #54100, .F. ) ;
#29788 = CARTESIAN_POINT ( 'NONE',  ( 4.553261556744875094, 40.63093864075490558, 16.69330377710913993 ) ) ;
#29789 = CARTESIAN_POINT ( 'NONE',  ( -2.708315649062916552, 5.842990691604414977, 13.41752550814512546 ) ) ;
#29790 = CIRCLE ( 'NONE', #16797, 0.09999999999999939493 ) ;
#29791 = CARTESIAN_POINT ( 'NONE',  ( 3.376099380956842921, 1.798919266859354327, 13.28428669908133486 ) ) ;
#29792 = CARTESIAN_POINT ( 'NONE',  ( 5.981074661064941900, -7.862380442164009331, -18.95903134304786519 ) ) ;
#29793 = CARTESIAN_POINT ( 'NONE',  ( 0.5997462898726536595, -35.63787911784795170, 33.78599121123970406 ) ) ;
#29794 = CARTESIAN_POINT ( 'NONE',  ( 0.5786265663353196143, 41.83999636203351713, -23.32245830378984408 ) ) ;
#29795 = CARTESIAN_POINT ( 'NONE',  ( -15.87364305917332530, -8.000014946965743334, -0.1367906320862119773 ) ) ;
#29796 = CARTESIAN_POINT ( 'NONE',  ( 0.5998501479064708430, -41.92175333043635987, 23.59887241503281174 ) ) ;
#29797 = CARTESIAN_POINT ( 'NONE',  ( 4.975801465491694664, -43.22084481528235500, 20.67815041659062913 ) ) ;
#29798 = EDGE_CURVE ( 'NONE', #59869, #26853, #41160, .T. ) ;
#29799 = CARTESIAN_POINT ( 'NONE',  ( 0.1156867017252034835, -43.74576137695434852, -5.766382646491231334 ) ) ;
#29800 = CARTESIAN_POINT ( 'NONE',  ( 4.291220156522059348, 34.26497439135438583, -32.33110773335063470 ) ) ;
#29801 = CARTESIAN_POINT ( 'NONE',  ( 3.270143674763207553, 2.058141141425593901, 13.53222904135354909 ) ) ;
#29802 = EDGE_CURVE ( 'NONE', #18712, #61, #58297, .T. ) ;
#29803 = B_SPLINE_CURVE_WITH_KNOTS ( 'NONE', 3,
 ( #18109, #36612, #37232, #9861 ),
 .UNSPECIFIED., .F., .F.,
 ( 4, 4 ),
 ( 0.000000000000000000, 0.004444878191956872469 ),
 .UNSPECIFIED. ) ;
#29804 = DIRECTION ( 'NONE',  ( 0.000000000000000000, 0.000000000000000000, 1.000000000000000000 ) ) ;
#29805 = DIRECTION ( 'NONE',  ( 0.09835009131224552170, 0.9164135549743782638, -0.3879606369183544179 ) ) ;
#29806 = ORIENTED_EDGE ( 'NONE', *, *, #10753, .T. ) ;
#29807 = AXIS2_PLACEMENT_3D ( 'NONE', #38765, #44395, #43462 ) ;
#29808 = DIRECTION ( 'NONE',  ( -0.000000000000000000, 1.000000000000000000, 0.000000000000000000 ) ) ;
#29809 = CARTESIAN_POINT ( 'NONE',  ( 4.833616638992208614, -41.67905425467692737, -20.04871863793795228 ) ) ;
#29810 = CARTESIAN_POINT ( 'NONE',  ( 1.227938101723748288, -34.55893248994524214, 25.45152231597044690 ) ) ;
#29811 = VERTEX_POINT ( 'NONE', #18880 ) ;
#29812 = CARTESIAN_POINT ( 'NONE',  ( 0.7242486021783840489, -14.75415305889595885, 46.83296306970812140 ) ) ;
#29813 = CARTESIAN_POINT ( 'NONE',  ( 4.691466044806102076, 14.01607102724483056, 42.32811009116559831 ) ) ;
#29814 = ORIENTED_EDGE ( 'NONE', *, *, #26434, .F. ) ;
#29815 = EDGE_LOOP ( 'NONE', ( #55610, #39122, #35402, #13287 ) ) ;
#29816 = CARTESIAN_POINT ( 'NONE',  ( -6.015611763856276717, 4.870987357968176390, 18.20278301740938431 ) ) ;
#29817 = ORIENTED_EDGE ( 'NONE', *, *, #32191, .F. ) ;
#29818 = FACE_OUTER_BOUND ( 'NONE', #51174, .T. ) ;
#29819 = VECTOR ( 'NONE', #54889, 1000.000000000000114 ) ;
#29820 = ORIENTED_EDGE ( 'NONE', *, *, #47827, .F. ) ;
#29821 = VERTEX_POINT ( 'NONE', #19188 ) ;
#29822 = CARTESIAN_POINT ( 'NONE',  ( 0.1103744047535531458, 11.12399292196378831, 41.66501489234567401 ) ) ;
#29823 = EDGE_CURVE ( 'NONE', #25579, #35927, #23248, .T. ) ;
#29824 = VERTEX_POINT ( 'NONE', #61434 ) ;
#29825 = CYLINDRICAL_SURFACE ( 'NONE', #47097, 6.887500000000022382 ) ;
#29826 = DIRECTION ( 'NONE',  ( 0.1736481776669314969, -0.9848077530122079093, -4.496403249731880833E-15 ) ) ;
#29827 = VERTEX_POINT ( 'NONE', #17952 ) ;
#29828 = EDGE_CURVE ( 'NONE', #9811, #53201, #37066, .T. ) ;
#29829 = DIRECTION ( 'NONE',  ( 0.000000000000000000, 0.000000000000000000, 1.000000000000000000 ) ) ;
#29830 =( GEOMETRIC_REPRESENTATION_CONTEXT ( 3 ) GLOBAL_UNCERTAINTY_ASSIGNED_CONTEXT ( ( #61161 ) ) GLOBAL_UNIT_ASSIGNED_CONTEXT ( ( #39456, #15642, #30026 ) ) REPRESENTATION_CONTEXT ( 'NONE', 'WORKASPACE' ) );
#29831 = CARTESIAN_POINT ( 'NONE',  ( 1.227938101723757836, 39.96870412324336996, 15.63977281655856366 ) ) ;
#29832 = VERTEX_POINT ( 'NONE', #18555 ) ;
#29833 = VECTOR ( 'NONE', #15715, 1000.000000000000000 ) ;
#29834 = ADVANCED_FACE ( 'NONE', ( #32981 ), #51856, .F. ) ;
#29835 = ORIENTED_EDGE ( 'NONE', *, *, #6269, .F. ) ;
#29836 = EDGE_CURVE ( 'NONE', #27817, #47199, #7500, .T. ) ;
#29837 = CARTESIAN_POINT ( 'NONE',  ( 0.6031357023905875581, -18.45021748202310974, 44.42879114414625974 ) ) ;
#29838 = CARTESIAN_POINT ( 'NONE',  ( -4.000000000000000000, 0.000000000000000000, 0.000000000000000000 ) ) ;
#29839 = CARTESIAN_POINT ( 'NONE',  ( 5.974727161628367256, -16.29297756969640076, -12.48248968439922990 ) ) ;
#29840 = EDGE_CURVE ( 'NONE', #536, #35413, #25205, .T. ) ;
#29841 = ORIENTED_EDGE ( 'NONE', *, *, #10650, .F. ) ;
#29842 = CARTESIAN_POINT ( 'NONE',  ( 0.6000166863083106206, -19.40010892967622169, -45.11606427011503939 ) ) ;
#29843 = CARTESIAN_POINT ( 'NONE',  ( 0.6067375320500688618, -37.56348932307244581, -29.71715680108774293 ) ) ;
#29844 = CARTESIAN_POINT ( 'NONE',  ( 0.5980271706414711508, 48.06821839532968710, 10.07450361757597967 ) ) ;
#29845 = EDGE_CURVE ( 'NONE', #43658, #56839, #32156, .T. ) ;
#29846 = CARTESIAN_POINT ( 'NONE',  ( 0.6039202388192952409, -25.30794220682896878, -42.08410357967478177 ) ) ;
#29847 = ORIENTED_EDGE ( 'NONE', *, *, #27156, .T. ) ;
#29848 = CARTESIAN_POINT ( 'NONE',  ( 3.783278058412224976, 42.86118820526429829, 3.901118461246968927 ) ) ;
#29849 = CARTESIAN_POINT ( 'NONE',  ( 0.3622758884714600280, 42.62881903538200845, 6.444611261694737081 ) ) ;
#29850 = CARTESIAN_POINT ( 'NONE',  ( -6.016761891674564211, 18.20023637398605842, -4.880293656734773222 ) ) ;
#29851 = CARTESIAN_POINT ( 'NONE',  ( 2.185380717157383579, -5.603685766289446590, 43.67400266634471251 ) ) ;
#29852 = AXIS2_PLACEMENT_3D ( 'NONE', #15901, #48786, #11199 ) ;
#29853 = ORIENTED_EDGE ( 'NONE', *, *, #46312, .F. ) ;
#29854 = ORIENTED_EDGE ( 'NONE', *, *, #35542, .F. ) ;
#29855 = CARTESIAN_POINT ( 'NONE',  ( 4.549368137175248350, 0.000000000000000000, 0.000000000000000000 ) ) ;
#29856 = CYLINDRICAL_SURFACE ( 'NONE', #31697, 75.00000000000001421 ) ;
#29857 = CARTESIAN_POINT ( 'NONE',  ( 0.1102847568649952675, -39.80641842112257933, 16.58813073670638261 ) ) ;
#29858 = CARTESIAN_POINT ( 'NONE',  ( -6.079354080745853928, -12.94667982361282554, -14.25399722158730498 ) ) ;
#29859 = CARTESIAN_POINT ( 'NONE',  ( 0.9730545539215883499, 42.47233286818625686, -6.101350888304211573 ) ) ;
#29860 = CARTESIAN_POINT ( 'NONE',  ( 4.975610109902397937, 13.36434394399692316, 47.05150069959858428 ) ) ;
#29861 = B_SPLINE_CURVE_WITH_KNOTS ( 'NONE', 3,
 ( #4668, #15048, #37629, #19432 ),
 .UNSPECIFIED., .F., .F.,
 ( 4, 4 ),
 ( 1.734723475976807094E-18, 0.004050076154993000749 ),
 .UNSPECIFIED. ) ;
#29862 = CARTESIAN_POINT ( 'NONE',  ( -2.569797478183783568, 1.464172661884163285, -14.55946937464482360 ) ) ;
#29863 = CARTESIAN_POINT ( 'NONE',  ( -6.079354080745853928, -17.34853647870671622, -8.355910321152581588 ) ) ;
#29864 = CARTESIAN_POINT ( 'NONE',  ( -6.057079549204054558, 19.09996424292742745, -2.454098005099244251 ) ) ;
#29865 = CARTESIAN_POINT ( 'NONE',  ( 0.1098349054025746785, 30.64407294528948356, -30.34240357440803848 ) ) ;
#29866 = DIRECTION ( 'NONE',  ( -0.07439287786467650709, 0.9868880006907410074, -0.1432402660415122431 ) ) ;
#29867 = AXIS2_PLACEMENT_3D ( 'NONE', #41456, #3502, #36755 ) ;
#29868 = CARTESIAN_POINT ( 'NONE',  ( 0.1156867017252034280, -6.918830238422117418, -43.57835007669613248 ) ) ;
#29869 = LINE ( 'NONE', #48984, #35423 ) ;
#29870 = CARTESIAN_POINT ( 'NONE',  ( 0.1156867017252034557, -35.43631104193246273, 26.29088562628884418 ) ) ;
#29871 = CARTESIAN_POINT ( 'NONE',  ( -99.49999999999975842, 4.769696007084727185, 1.499999999999998446 ) ) ;
#29872 = CARTESIAN_POINT ( 'NONE',  ( 0.6009452777970413218, -23.67489783211123111, 41.87890062805995228 ) ) ;
#29873 = CARTESIAN_POINT ( 'NONE',  ( -7.632783294297951215E-14, -4.618802153517020948, -0.3572655899081733644 ) ) ;
#29874 = CARTESIAN_POINT ( 'NONE',  ( 0.5786265663353196143, 47.39171391660391208, 6.967625775955879064 ) ) ;
#29875 = ITEM_DEFINED_TRANSFORMATION ( 'NONE', 'NONE', #51872,  #14677 ) ;
#29876 = CARTESIAN_POINT ( 'NONE',  ( 0.9756354156337443406, -26.22428641656280135, 33.96210048825368233 ) ) ;
#29877 = PRODUCT_DEFINITION_FORMATION_WITH_SPECIFIED_SOURCE ( 'ANY', '', #7765, .NOT_KNOWN. ) ;
#29878 = EDGE_CURVE ( 'NONE', #28421, #28462, #60528, .T. ) ;
#29879 = CARTESIAN_POINT ( 'NONE',  ( 0.6024113833632039894, -30.78790221898711010, 38.25763905489927907 ) ) ;
#29880 = CARTESIAN_POINT ( 'NONE',  ( 0.8744876279028306332, 23.49358985382604459, 43.10917867646859492 ) ) ;
#29881 = CARTESIAN_POINT ( 'NONE',  ( 0.6029442701453591180, 48.21847811021937957, 9.301805947909977945 ) ) ;
#29883 = ORIENTED_EDGE ( 'NONE', *, *, #31249, .T. ) ;
#29882 = CARTESIAN_POINT ( 'NONE',  ( 0.7954190325252785687, -7.138712176115113550, -47.56618055754173469 ) ) ;
#29884 = EDGE_LOOP ( 'NONE', ( #60492, #29835, #39391, #27721 ) ) ;
#29885 = CARTESIAN_POINT ( 'NONE',  ( 0.1103878639767399694, -43.12442673975421314, 0.04853618198105230652 ) ) ;
#29886 = CARTESIAN_POINT ( 'NONE',  ( 5.000000000000002665, 3.306546357697854226E-16, 2.700000000000000622 ) ) ;
#29887 = CARTESIAN_POINT ( 'NONE',  ( 0.9762797500689124330, -34.26226594605947895, 24.13341909939818564 ) ) ;
#29888 = ORIENTED_EDGE ( 'NONE', *, *, #56300, .T. ) ;
#29889 = VERTEX_POINT ( 'NONE', #5353 ) ;
#29890 = CARTESIAN_POINT ( 'NONE',  ( 0.1092565886968783623, -10.86136484717998663, 41.73439049602432505 ) ) ;
#29891 = CARTESIAN_POINT ( 'NONE',  ( 0.5800708119828333897, 34.30831427709752290, 33.42085299104031293 ) ) ;
#29892 = CARTESIAN_POINT ( 'NONE',  ( 0.5837374860065634996, -41.56971235019468480, -23.79054246378012749 ) ) ;
#29893 = ORIENTED_EDGE ( 'NONE', *, *, #37473, .T. ) ;
#29894 = ORIENTED_EDGE ( 'NONE', *, *, #23480, .F. ) ;
#29895 = CARTESIAN_POINT ( 'NONE',  ( 5.896278296736517710, 18.99819559441558070, -6.602692160831987955 ) ) ;
#29896 = VECTOR ( 'NONE', #58220, 1000.000000000000000 ) ;
#29897 = AXIS2_PLACEMENT_3D ( 'NONE', #56654, #57879, #38506 ) ;
#29898 = CARTESIAN_POINT ( 'NONE',  ( 5.959828726073459926, -12.49160845136047193, 16.28681682518042706 ) ) ;
#29899 = CARTESIAN_POINT ( 'NONE',  ( 0.9730545539215883499, -11.59290486963477562, -41.31259007387244253 ) ) ;
#29900 = CARTESIAN_POINT ( 'NONE',  ( 0.6000166863083090663, 49.04012132094733545, 2.624877622903674990 ) ) ;
#29901 = CARTESIAN_POINT ( 'NONE',  ( 0.5998501479064699549, 18.89267974119604077, 44.24259072156093708 ) ) ;
#29902 = EDGE_CURVE ( 'NONE', #40335, #59254, #31372, .T. ) ;
#29903 =( BOUNDED_SURFACE ( )  B_SPLINE_SURFACE ( 3, 1, ( 
 ( #51816, #28029 ),
 ( #47148, #9220 ),
 ( #23633, #4190 ),
 ( #18954, #13631 ) ),
 .UNSPECIFIED., .F., .F., .F. ) 
 B_SPLINE_SURFACE_WITH_KNOTS ( ( 4, 4 ),
 ( 2, 2 ),
 ( 0.000000000000000000, 1.000000000000000000 ),
 ( 0.000000000000000000, 1.000000000000000000 ),
 .UNSPECIFIED. ) 
 GEOMETRIC_REPRESENTATION_ITEM ( )  RATIONAL_B_SPLINE_SURFACE ( (
 ( 1.000000000000000000, 1.000000000000000000),
 ( 0.7223157951917476005, 0.9931996967497186413),
 ( 0.7223157951917476005, 0.9931996967497186413),
 ( 1.000000000000000000, 1.000000000000000000) ) ) 
 REPRESENTATION_ITEM ( '' )  SURFACE ( )  );
#29904 = VECTOR ( 'NONE', #58803, 1000.000000000000000 ) ;
#29905 = CARTESIAN_POINT ( 'NONE',  ( 0.1140933569871964287, 15.59435692983238653, -41.27670023183653569 ) ) ;
#29906 = EDGE_CURVE ( 'NONE', #25113, #55904, #9730, .T. ) ;
#29907 = ORIENTED_EDGE ( 'NONE', *, *, #47607, .T. ) ;
#29908 = ORIENTED_EDGE ( 'NONE', *, *, #10696, .F. ) ;
#29909 = EDGE_CURVE ( 'NONE', #16942, #10591, #663, .T. ) ;
#29910 = CARTESIAN_POINT ( 'NONE',  ( 0.1119898979215347840, 33.95944467168810377, 28.17299107021446503 ) ) ;
#29911 = CARTESIAN_POINT ( 'NONE',  ( -6.010958268070873523, 9.434296419346436480, -16.31164801516932528 ) ) ;
#29912 = VECTOR ( 'NONE', #5951, 1000.000000000000114 ) ;
#29913 = VERTEX_POINT ( 'NONE', #15098 ) ;
#29914 = CARTESIAN_POINT ( 'NONE',  ( 0.5998501479064708430, 46.60114184914316837, -11.94461217097420658 ) ) ;
#29915 = CARTESIAN_POINT ( 'NONE',  ( 2.282803330402962239, 3.392772187570622044, 46.85067773618895615 ) ) ;
#29916 = ADVANCED_FACE ( 'NONE', ( #34207 ), #58244, .F. ) ;
#29917 = CARTESIAN_POINT ( 'NONE',  ( 5.895596859100789899, 8.462961974658767872, -18.24572437114973056 ) ) ;
#29918 = CARTESIAN_POINT ( 'NONE',  ( 0.1155031312995260795, -40.83589324745333471, -16.71440861096808206 ) ) ;
#29919 = ORIENTED_EDGE ( 'NONE', *, *, #12964, .F. ) ;
#29920 = CARTESIAN_POINT ( 'NONE',  ( 0.5806925824938499181, -14.41498975133639426, 44.62544602368059543 ) ) ;
#29921 = CARTESIAN_POINT ( 'NONE',  ( 0.9752132459055864455, -42.57112816680946565, -5.369621847648042845 ) ) ;
#29922 = CARTESIAN_POINT ( 'NONE',  ( 0.5807400328401574052, -5.711437504336299043, 47.55718917606841956 ) ) ;
#29923 = EDGE_CURVE ( 'NONE', #34686, #35128, #16658, .T. ) ;
#29924 =( BOUNDED_SURFACE ( )  B_SPLINE_SURFACE ( 3, 1, ( 
 ( #9193, #10436 ),
 ( #14532, #33944 ),
 ( #42729, #61789 ),
 ( #9497, #38964 ) ),
 .UNSPECIFIED., .F., .F., .F. ) 
 B_SPLINE_SURFACE_WITH_KNOTS ( ( 4, 4 ),
 ( 2, 2 ),
 ( 0.000000000000000000, 1.000000000000000000 ),
 ( 0.000000000000000000, 1.000000000000000000 ),
 .UNSPECIFIED. ) 
 GEOMETRIC_REPRESENTATION_ITEM ( )  RATIONAL_B_SPLINE_SURFACE ( (
 ( 1.000000000000000000, 1.000000000000000000),
 ( 0.9953040768229005630, 0.8617119497784937465),
 ( 0.9953040768229005630, 0.8617119497784937465),
 ( 1.000000000000000000, 1.000000000000000000) ) ) 
 REPRESENTATION_ITEM ( '' )  SURFACE ( )  );
#29925 = CARTESIAN_POINT ( 'NONE',  ( 0.9747592971366240144, -21.73404615330592549, -36.99691261380228013 ) ) ;
#29926 = B_SPLINE_CURVE_WITH_KNOTS ( 'NONE', 3,
 ( #6963, #21401, #8214, #40851, #45852, #27333 ),
 .UNSPECIFIED., .F., .F.,
 ( 4, 2, 4 ),
 ( 6.256513556477135401E-18, 0.0002445244328975374024, 0.0004890488657950686248 ),
 .UNSPECIFIED. ) ;
#29927 = ORIENTED_EDGE ( 'NONE', *, *, #8754, .T. ) ;
#29928 = CARTESIAN_POINT ( 'NONE',  ( 0.2940133293162999761, 42.11535308342802608, -13.13535626605661122 ) ) ;
#29929 = DIRECTION ( 'NONE',  ( -1.000000000000000000, -0.000000000000000000, -0.000000000000000000 ) ) ;
#29930 = VERTEX_POINT ( 'NONE', #35762 ) ;
#29931 = CARTESIAN_POINT ( 'NONE',  ( 4.833616638992205949, -38.70560126501880660, 25.31740731790829102 ) ) ;
#29932 = CARTESIAN_POINT ( 'NONE',  ( 4.691466044806103852, 14.64802401911168062, 42.11359095667496177 ) ) ;
#29933 = EDGE_CURVE ( 'NONE', #23932, #43343, #30718, .T. ) ;
#29934 = EDGE_LOOP ( 'NONE', ( #22311, #30587, #58708, #19376 ) ) ;
#29935 = CARTESIAN_POINT ( 'NONE',  ( 3.783198216974388295, -40.39102707215867127, 14.86152287314668463 ) ) ;
#29936 = CARTESIAN_POINT ( 'NONE',  ( 2.643462169533600914, -40.89244134039093836, -25.20536747735765104 ) ) ;
#29937 = EDGE_CURVE ( 'NONE', #7789, #52714, #3198, .T. ) ;
#29938 = CARTESIAN_POINT ( 'NONE',  ( 0.1073791018717483448, -21.98088480513640874, -37.10214135362880228 ) ) ;
#29939 = CARTESIAN_POINT ( 'NONE',  ( 4.553261556744875094, -29.69864478935419072, 32.36556910513705532 ) ) ;
#29940 = CARTESIAN_POINT ( 'NONE',  ( 3.238018933889920792, -7.437505510344910142, -11.13961418323103558 ) ) ;
#29941 = CARTESIAN_POINT ( 'NONE',  ( 0.1119898979215351031, -31.30369549611587132, 31.09726606212005962 ) ) ;
#29942 = CARTESIAN_POINT ( 'NONE',  ( 0.5832367798473397924, 46.33367954572898384, -12.13303976268012363 ) ) ;
#29943 = DIRECTION ( 'NONE',  ( 0.000000000000000000, 1.224646799147353947E-16, 1.000000000000000000 ) ) ;
#29944 = EDGE_LOOP ( 'NONE', ( #1953, #4160, #45052, #14119 ) ) ;
#29945 = DIRECTION ( 'NONE',  ( -1.000000000000000000, -5.380183451256491399E-17, -1.298891185607892835E-16 ) ) ;
#29946 = CARTESIAN_POINT ( 'NONE',  ( 1.231276596079887264, 14.27346765619334512, -39.41503383336959132 ) ) ;
#29947 = CARTESIAN_POINT ( 'NONE',  ( -4.473699999999997345, 0.000000000000000000, 0.000000000000000000 ) ) ;
#29948 = EDGE_LOOP ( 'NONE', ( #58940, #58682, #47666, #37102 ) ) ;
#29949 = CONICAL_SURFACE ( 'NONE', #18977, 43.08621763946400307, 1.568696531533066763 ) ;
#29950 = CARTESIAN_POINT ( 'NONE',  ( 3.680882792899936362, 35.20667105325171775, 32.59085259319700612 ) ) ;
#29951 = CARTESIAN_POINT ( 'NONE',  ( 4.834790513006555379, 7.995814508775468177, 46.56883390493727859 ) ) ;
#29952 = CARTESIAN_POINT ( 'NONE',  ( 0.6029443449137434907, 22.67547108931568189, 43.55872528967004342 ) ) ;
#29953 = CARTESIAN_POINT ( 'NONE',  ( -6.016761891674564211, -7.214149619366230226, -17.40752468084790650 ) ) ;
#29954 = CARTESIAN_POINT ( 'NONE',  ( 0.5804410086790514622, 32.99440095574045273, -33.33000686209395269 ) ) ;
#29955 = CARTESIAN_POINT ( 'NONE',  ( 4.967162193818130511, 0.000000000000000000, 0.000000000000000000 ) ) ;
#29956 = DIRECTION ( 'NONE',  ( -1.000000000000000000, -3.135800716341488305E-16, -1.298891185607925622E-16 ) ) ;
#29957 = CARTESIAN_POINT ( 'NONE',  ( 5.901463166500145796, -11.91875711499639934, -16.20065119599700765 ) ) ;
#29958 = EDGE_CURVE ( 'NONE', #60202, #7602, #3136, .T. ) ;
#29959 = CARTESIAN_POINT ( 'NONE',  ( 0.6254087463353934506, 46.64065386173398053, 11.78492518233826125 ) ) ;
#29960 = CARTESIAN_POINT ( 'NONE',  ( 4.549368137175248350, 38.40568845698250300, 19.17571786012337753 ) ) ;
#29962 = ORIENTED_EDGE ( 'NONE', *, *, #52182, .T. ) ;
#29961 = CARTESIAN_POINT ( 'NONE',  ( 4.975801465491695552, -39.51822597168514051, 27.09127437476313816 ) ) ;
#29963 = ORIENTED_EDGE ( 'NONE', *, *, #19960, .F. ) ;
#29965 = VECTOR ( 'NONE', #24089, 1000.000000000000114 ) ;
#29964 = CARTESIAN_POINT ( 'NONE',  ( 2.281448460670567613, -28.15071835136424383, 38.84544723616133410 ) ) ;
#29966 = CARTESIAN_POINT ( 'NONE',  ( 5.960721111146673579, 20.34914600876571456, 2.685391721746106963 ) ) ;
#29967 = CARTESIAN_POINT ( 'NONE',  ( 0.1097557419366048670, 16.70891382096314004, 39.75589591229793029 ) ) ;
#29968 = EDGE_CURVE ( 'NONE', #46035, #4359, #27716, .T. ) ;
#29969 = CARTESIAN_POINT ( 'NONE',  ( -31.75000000000000000, 0.000000000000000000, 0.000000000000000000 ) ) ;
#29970 = CARTESIAN_POINT ( 'NONE',  ( 5.960221823109900008, -18.96108896995709969, -7.859839668735147278 ) ) ;
#29971 = CARTESIAN_POINT ( 'NONE',  ( 0.1129192098497447394, 9.345467776859020859, -43.12324222292247811 ) ) ;
#29972 = ORIENTED_EDGE ( 'NONE', *, *, #47607, .F. ) ;
#29973 = VERTEX_POINT ( 'NONE', #6572 ) ;
#29974 = CARTESIAN_POINT ( 'NONE',  ( 0.5804410086790514622, -13.37224000219836917, -44.95223074752801296 ) ) ;
#29975 = CARTESIAN_POINT ( 'NONE',  ( -5.995132425357893702, 11.47834865841117491, -14.94489030678139230 ) ) ;
#29976 = CARTESIAN_POINT ( 'NONE',  ( 120.0000507999999968, 0.000000000000000000, 0.000000000000000000 ) ) ;
#29977 = EDGE_LOOP ( 'NONE', ( #59428, #22291, #36786, #30935 ) ) ;
#29978 = CARTESIAN_POINT ( 'NONE',  ( 4.967162193818130511, 0.000000000000000000, 0.000000000000000000 ) ) ;
#29979 = DIRECTION ( 'NONE',  ( -1.000000000000000000, -0.000000000000000000, -0.000000000000000000 ) ) ;
#29980 = B_SPLINE_CURVE_WITH_KNOTS ( 'NONE', 3,
 ( #3294, #3601, #36542, #3913, #18047, #17419 ),
 .UNSPECIFIED., .F., .F.,
 ( 4, 2, 4 ),
 ( 1.250788275041438294E-16, 0.0002450741128632354863, 0.0004901482257263459642 ),
 .UNSPECIFIED. ) ;
#29981 = VERTEX_POINT ( 'NONE', #25719 ) ;
#29982 = CARTESIAN_POINT ( 'NONE',  ( -6.078726893082806448, -8.903615017412294108, -17.07394743140643456 ) ) ;
#29983 = EDGE_CURVE ( 'NONE', #50438, #33616, #46372, .T. ) ;
#29984 = ORIENTED_EDGE ( 'NONE', *, *, #48528, .T. ) ;
#29985 = CARTESIAN_POINT ( 'NONE',  ( 4.958415959904820980, 18.66009313387939628, 41.41261737752859773 ) ) ;
#29987 = CARTESIAN_POINT ( 'NONE',  ( 4.958415959904820092, 13.93965400761620366, -43.23066041561927619 ) ) ;
#29986 = TOROIDAL_SURFACE ( 'NONE', #23963, 7.400000000000022560, 0.09999999999999961697 ) ;
#29988 = ORIENTED_EDGE ( 'NONE', *, *, #35391, .F. ) ;
#29989 = CARTESIAN_POINT ( 'NONE',  ( 0.5809828226811560858, -41.74875432577632495, -23.47450554821754309 ) ) ;
#29990 = CARTESIAN_POINT ( 'NONE',  ( 0.6039202388192952409, 46.55074123944880427, 15.63944381705665165 ) ) ;
#29991 = ADVANCED_FACE ( 'NONE', ( #35448 ), #2637, .F. ) ;
#29992 = CARTESIAN_POINT ( 'NONE',  ( 3.270143674763207553, 7.080034332678427411, -11.71453292426871684 ) ) ;
#29993 = CARTESIAN_POINT ( 'NONE',  ( 0.6000166863083106206, 4.195342255946718169, 48.93079383234981350 ) ) ;
#29994 = VERTEX_POINT ( 'NONE', #59530 ) ;
#29995 = CARTESIAN_POINT ( 'NONE',  ( 2.648799415243696664, -26.59464913125750485, 41.19759824158324335 ) ) ;
#29996 = CARTESIAN_POINT ( 'NONE',  ( 0.6028618097248862329, -0.1745704727162494252, -48.10721794025128162 ) ) ;
#29997 = ORIENTED_EDGE ( 'NONE', *, *, #26320, .T. ) ;
#29998 = CARTESIAN_POINT ( 'NONE',  ( -1.399999999999998579, 0.000000000000000000, 0.000000000000000000 ) ) ;
#29999 = VERTEX_POINT ( 'NONE', #31041 ) ;
#30000 = CARTESIAN_POINT ( 'NONE',  ( 5.960221823109900008, -14.50993159119820852, 14.51763960716753132 ) ) ;
#30001 = VERTEX_POINT ( 'NONE', #60150 ) ;
#30002 = CARTESIAN_POINT ( 'NONE',  ( 0.9762797500689124330, -31.41867615533366376, -27.73430319715951242 ) ) ;
#30003 = CIRCLE ( 'NONE', #57975, 5.453125000000000000 ) ;
#30004 = CARTESIAN_POINT ( 'NONE',  ( 0.7762777257811881437, 41.03453903600433961, 24.71864134625245057 ) ) ;
#30005 = VERTEX_POINT ( 'NONE', #17259 ) ;
#30006 = CARTESIAN_POINT ( 'NONE',  ( 0.5839879327111916485, 6.341736898931933375, 47.47435452316580040 ) ) ;
#30007 = CARTESIAN_POINT ( 'NONE',  ( 0.5819845079324660331, -5.801222053075409946, 47.54334065046002422 ) ) ;
#30008 = EDGE_CURVE ( 'NONE', #39735, #22660, #11982, .T. ) ;
#30009 = CARTESIAN_POINT ( 'NONE',  ( 4.834790513006555379, 43.62201989944838232, -18.15788315901691874 ) ) ;
#30010 = ORIENTED_EDGE ( 'NONE', *, *, #40400, .T. ) ;
#30011 = VERTEX_POINT ( 'NONE', #45469 ) ;
#30012 = CARTESIAN_POINT ( 'NONE',  ( 0.000000000000000000, 0.000000000000000000, -1.199999999999999956 ) ) ;
#30013 = CARTESIAN_POINT ( 'NONE',  ( 4.226256110419179812, 31.27626226520831310, 30.86458599600995356 ) ) ;
#30014 = DIRECTION ( 'NONE',  ( -0.000000000000000000, -0.000000000000000000, 1.000000000000000000 ) ) ;
#30015 = DIRECTION ( 'NONE',  ( 0.000000000000000000, 0.000000000000000000, 1.000000000000000000 ) ) ;
#30016 = CARTESIAN_POINT ( 'NONE',  ( 0.9790724872846766624, -27.02650450976093310, -32.02972469387346166 ) ) ;
#30017 = CARTESIAN_POINT ( 'NONE',  ( 0.9785694773339250752, 38.49576580281336646, 16.56536812055855634 ) ) ;
#30018 = ORIENTED_EDGE ( 'NONE', *, *, #30946, .T. ) ;
#30019 = DIRECTION ( 'NONE',  ( 0.000000000000000000, 0.000000000000000000, -1.000000000000000000 ) ) ;
#30020 = VERTEX_POINT ( 'NONE', #2517 ) ;
#30021 = CARTESIAN_POINT ( 'NONE',  ( 0.5824936645240084143, 36.57713187198718430, 29.34879219081370039 ) ) ;
#30022 = CARTESIAN_POINT ( 'NONE',  ( -4.000000000000000000, -2.309401076758531346, -5.242734410091827613 ) ) ;
#30023 = CARTESIAN_POINT ( 'NONE',  ( 0.5837799406558258353, -41.89664897202754901, -21.06927512972148975 ) ) ;
#30024 = CARTESIAN_POINT ( 'NONE',  ( 0.5850706913938534814, 44.18063951072247164, -18.49682194437916039 ) ) ;
#30025 = CARTESIAN_POINT ( 'NONE',  ( 2.009741617377216460, 11.13136660361437791, 42.60981993811969915 ) ) ;
#30026 =( NAMED_UNIT ( * ) SI_UNIT ( $, .STERADIAN. ) SOLID_ANGLE_UNIT ( ) );
#30027 = CARTESIAN_POINT ( 'NONE',  ( -5.331200000000000827, 0.000000000000000000, 0.000000000000000000 ) ) ;
#30028 =( BOUNDED_SURFACE ( )  B_SPLINE_SURFACE ( 3, 1, ( 
 ( #39041, #14607 ),
 ( #10201, #24608 ),
 ( #34324, #10508 ),
 ( #13995, #33402 ) ),
 .UNSPECIFIED., .F., .F., .F. ) 
 B_SPLINE_SURFACE_WITH_KNOTS ( ( 4, 4 ),
 ( 2, 2 ),
 ( 0.000000000000000000, 1.000000000000000000 ),
 ( 0.000000000000000000, 1.000000000000000000 ),
 .UNSPECIFIED. ) 
 GEOMETRIC_REPRESENTATION_ITEM ( )  RATIONAL_B_SPLINE_SURFACE ( (
 ( 1.000000000000000000, 1.000000000000000000),
 ( 0.7211978278499968642, 0.9934217856018975334),
 ( 0.7211978278499968642, 0.9934217856018975334),
 ( 1.000000000000000000, 1.000000000000000000) ) ) 
 REPRESENTATION_ITEM ( '' )  SURFACE ( )  );
#30029 = EDGE_CURVE ( 'NONE', #20518, #47447, #18737, .T. ) ;
#30030 = CARTESIAN_POINT ( 'NONE',  ( 0.6026112563231247332, 37.50532343773836885, -31.70002695164217243 ) ) ;
#30031 = FACE_OUTER_BOUND ( 'NONE', #31096, .T. ) ;
#30032 = CARTESIAN_POINT ( 'NONE',  ( 0.5782707292762423457, -41.52883855096556687, 21.79660345823301881 ) ) ;
#30033 = CARTESIAN_POINT ( 'NONE',  ( 0.1129192098497455998, -44.12161472487017733, -0.4846667466135657909 ) ) ;
#30034 = DIRECTION ( 'NONE',  ( -1.000000000000000000, -0.000000000000000000, -0.000000000000000000 ) ) ;
#30035 = DIRECTION ( 'NONE',  ( -1.000000000000000000, -0.000000000000000000, -0.000000000000000000 ) ) ;
#30036 = CARTESIAN_POINT ( 'NONE',  ( 0.8744876279028263033, 27.35388303025786882, 40.76904626731490566 ) ) ;
#30037 = FACE_OUTER_BOUND ( 'NONE', #11945, .T. ) ;
#30038 = CARTESIAN_POINT ( 'NONE',  ( 15.24999999999999289, 2.688986455804112996, 8.896908036367455278E-17 ) ) ;
#30039 = ADVANCED_FACE ( 'NONE', ( #9380 ), #23878, .F. ) ;
#30040 = CLOSED_SHELL ( 'NONE', ( #3448, #40982, #42458, #52372, #42202, #27854, #25392, #14314, #43647, #14178, #47204, #1963, #6053, #34453, #51751, #57869, #40901, #49355, #42531, #55015, #320, #6507, #61576, #9896, #54721, #26299, #20184 ) ) ;
#30041 = ORIENTED_EDGE ( 'NONE', *, *, #28293, .F. ) ;
#30042 = EDGE_CURVE ( 'NONE', #56097, #21039, #4655, .T. ) ;
#30043 = CYLINDRICAL_SURFACE ( 'NONE', #39318, 1.000000000000000666 ) ;
#30044 = CARTESIAN_POINT ( 'NONE',  ( 0.1092355843206037486, 37.19569459163105307, 21.82203846347341525 ) ) ;
#30045 = CARTESIAN_POINT ( 'NONE',  ( 0.6001305935487422083, 12.95698906763746194, 46.33281397023068138 ) ) ;
#30046 = CARTESIAN_POINT ( 'NONE',  ( 0.1073791018717483448, -30.14884492832410601, 30.83464511437086841 ) ) ;
#30047 = CARTESIAN_POINT ( 'NONE',  ( 0.6845945791218023269, 39.91187923413981764, -24.64646864590107000 ) ) ;
#30048 = VERTEX_POINT ( 'NONE', #46388 ) ;
#30049 = CARTESIAN_POINT ( 'NONE',  ( 1.231276596079881047, -0.5545928549373742023, -41.91621640586514985 ) ) ;
#30050 = CARTESIAN_POINT ( 'NONE',  ( 0.6029442701453591180, 28.02372554534090199, -40.32636893792552257 ) ) ;
#30051 = CARTESIAN_POINT ( 'NONE',  ( 0.6021448801613057400, -14.22267499166645166, 47.00273028993500191 ) ) ;
#30052 = ORIENTED_EDGE ( 'NONE', *, *, #46158, .F. ) ;
#30053 = CARTESIAN_POINT ( 'NONE',  ( 0.8560838555295223751, -35.39593983670150124, -30.78149244527203621 ) ) ;
#30054 = CARTESIAN_POINT ( 'NONE',  ( 0.5786265663353153954, 6.967625775955708534, 47.39171391660394761 ) ) ;
#30055 = ADVANCED_FACE ( 'NONE', ( #47957 ), #37075, .F. ) ;
#30056 = ORIENTED_EDGE ( 'NONE', *, *, #19810, .T. ) ;
#30057 = CARTESIAN_POINT ( 'NONE',  ( 4.960386119450141074, -25.57375555595671202, 35.50238712307264421 ) ) ;
#30058 = ORIENTED_EDGE ( 'NONE', *, *, #41056, .T. ) ;
#30059 = CARTESIAN_POINT ( 'NONE',  ( -6.057079549204054558, 9.975405573751219279, 16.47187040802930724 ) ) ;
#30061 = VERTEX_POINT ( 'NONE', #18806 ) ;
#30060 = ADVANCED_FACE ( 'NONE', ( #23184 ), #52223, .F. ) ;
#30062 = CARTESIAN_POINT ( 'NONE',  ( 2.526464513654345545, 1.212545078562781153, 42.96196573359004134 ) ) ;
#30063 = CARTESIAN_POINT ( 'NONE',  ( 4.975801465491694664, 31.15993731089074359, 36.39623109580477234 ) ) ;
#30064 = VERTEX_POINT ( 'NONE', #37003 ) ;
#30065 = DIRECTION ( 'NONE',  ( 1.000000000000000000, 1.558861125776144859E-16, -3.851859888774471706E-32 ) ) ;
#30066 = VERTEX_POINT ( 'NONE', #56992 ) ;
#30067 = CARTESIAN_POINT ( 'NONE',  ( 5.896278296736517710, 16.58497454171972052, 11.37829508603518391 ) ) ;
#30068 = ADVANCED_FACE ( 'NONE', ( #14115 ), #9054, .F. ) ;
#30069 = CARTESIAN_POINT ( 'NONE',  ( 0.1313383488274145194, 33.82021892231549032, -26.75504982351774075 ) ) ;
#30070 = ORIENTED_EDGE ( 'NONE', *, *, #49649, .F. ) ;
#30071 = DIRECTION ( 'NONE',  ( -1.718001593797181987E-16, 1.000000000000000000, 0.000000000000000000 ) ) ;
#30072 = CARTESIAN_POINT ( 'NONE',  ( 0.5819845079324654780, 33.54497088780129133, -34.18710788661915245 ) ) ;
#30073 = CARTESIAN_POINT ( 'NONE',  ( 0.5998501479064699549, 24.50586714782546593, 41.39809967730496254 ) ) ;
#30074 = CARTESIAN_POINT ( 'NONE',  ( -6.016489644550736315, -13.32104266208108534, 13.32727118274432954 ) ) ;
#30075 = ORIENTED_EDGE ( 'NONE', *, *, #34419, .T. ) ;
#30076 = CARTESIAN_POINT ( 'NONE',  ( 0.6000166863083090663, 27.66667954482629099, -40.57558779207448652 ) ) ;
#30077 = EDGE_CURVE ( 'NONE', #45338, #24773, #27885, .T. ) ;
#30078 = CARTESIAN_POINT ( 'NONE',  ( -6.057079549204054558, 15.43788712751036840, 11.51098919024721035 ) ) ;
#30079 = VERTEX_POINT ( 'NONE', #58214 ) ;
#30080 = DIRECTION ( 'NONE',  ( -1.000000000000000000, -0.000000000000000000, -0.000000000000000000 ) ) ;
#30081 = EDGE_LOOP ( 'NONE', ( #36569, #22652, #12349, #58624 ) ) ;
#30082 = CARTESIAN_POINT ( 'NONE',  ( 0.9747592971366227932, 33.84353661172440297, -26.37717450293392929 ) ) ;
#30083 = CARTESIAN_POINT ( 'NONE',  ( 0.1157506346131639274, 25.32019492611800615, 36.13624757367900742 ) ) ;
#30084 = ORIENTED_EDGE ( 'NONE', *, *, #26976, .T. ) ;
#30085 = LINE ( 'NONE', #54489, #17581 ) ;
#30086 = CARTESIAN_POINT ( 'NONE',  ( 4.975801465491695552, -45.55012473237743365, -14.85979367497158599 ) ) ;
#30087 = CARTESIAN_POINT ( 'NONE',  ( 4.553261556744875094, 0.000000000000000000, 0.000000000000000000 ) ) ;
#30088 = CARTESIAN_POINT ( 'NONE',  ( -19.25527904682359548, -12.38827900997423548, -1.669286156354737427 ) ) ;
#30089 = ORIENTED_EDGE ( 'NONE', *, *, #7977, .T. ) ;
#30090 = CARTESIAN_POINT ( 'NONE',  ( 0.6031356755773454870, 18.40989784469860524, -44.44549206087163640 ) ) ;
#30091 = CARTESIAN_POINT ( 'NONE',  ( 4.967162193818130511, 7.970725651239789045, 42.34252806656596846 ) ) ;
#30092 = CARTESIAN_POINT ( 'NONE',  ( 0.7762777257811902532, -5.369627942761314721, -47.60264404062384358 ) ) ;
#30093 = SHAPE_REPRESENTATION_RELATIONSHIP ( 'NONE' , 'NONE' ,  #16880, #30252 ) ;
#30094 = FILL_AREA_STYLE_COLOUR ( '', #14830 ) ;
#30095 =( BOUNDED_SURFACE ( )  B_SPLINE_SURFACE ( 3, 1, ( 
 ( #33132, #4270 ),
 ( #42234, #37217 ),
 ( #61292, #22790 ),
 ( #17477, #32825 ) ),
 .UNSPECIFIED., .F., .F., .F. ) 
 B_SPLINE_SURFACE_WITH_KNOTS ( ( 4, 4 ),
 ( 2, 2 ),
 ( 0.000000000000000000, 1.000000000000000000 ),
 ( 0.000000000000000000, 1.000000000000000000 ),
 .UNSPECIFIED. ) 
 GEOMETRIC_REPRESENTATION_ITEM ( )  RATIONAL_B_SPLINE_SURFACE ( (
 ( 1.000000000000000000, 1.000000000000000000),
 ( 0.9729067724841187204, 0.9999501103223794596),
 ( 0.9729067724841187204, 0.9999501103223794596),
 ( 1.000000000000000000, 1.000000000000000000) ) ) 
 REPRESENTATION_ITEM ( '' )  SURFACE ( )  );
#30096 = CARTESIAN_POINT ( 'NONE',  ( 0.7413678028165011646, -7.957411786230919937, -43.37240700531383197 ) ) ;
#30097 = DIRECTION ( 'NONE',  ( 0.000000000000000000, 0.000000000000000000, 1.000000000000000000 ) ) ;
#30098 = ADVANCED_FACE ( 'NONE', ( #9695 ), #27223, .F. ) ;
#30099 = CARTESIAN_POINT ( 'NONE',  ( 3.678748215320120085, 18.63777698665937876, 45.29068428821796743 ) ) ;
#30100 = CARTESIAN_POINT ( 'NONE',  ( 3.407937589446178528, 3.987184287467786969, 13.10584870154468184 ) ) ;
#30101 = EDGE_CURVE ( 'NONE', #4396, #18712, #48561, .T. ) ;
#30102 = CARTESIAN_POINT ( 'NONE',  ( 4.975801465491695552, 35.64402118370958306, -32.01766832630274706 ) ) ;
#30103 = CARTESIAN_POINT ( 'NONE',  ( 2.648799415243708655, 6.085982952328954809, 48.65673925360762553 ) ) ;
#30104 = CARTESIAN_POINT ( 'NONE',  ( 4.975801465491695552, -42.71626295676279028, 21.70134120755125906 ) ) ;
#30105 = CARTESIAN_POINT ( 'NONE',  ( 1.084202172485504434E-14, 4.618802153517020059, -5.242734410091827613 ) ) ;
#30106 = EDGE_CURVE ( 'NONE', #48896, #41987, #15033, .T. ) ;
#30107 = B_SPLINE_CURVE_WITH_KNOTS ( 'NONE', 3,
 ( #1893, #35444, #35133, #44853 ),
 .UNSPECIFIED., .F., .F.,
 ( 4, 4 ),
 ( 9.813077866773596333E-18, 0.005004948556313810505 ),
 .UNSPECIFIED. ) ;
#30108 = B_SPLINE_CURVE_WITH_KNOTS ( 'NONE', 3,
 ( #46776, #3505, #22642, #41771, #7274, #17953 ),
 .UNSPECIFIED., .F., .F.,
 ( 4, 2, 4 ),
 ( 8.609910155989501895E-17, 0.0002293366620881447408, 0.0004586733241762033959 ),
 .UNSPECIFIED. ) ;
#30109 = EDGE_CURVE ( 'NONE', #35637, #27976, #57281, .T. ) ;
#30110 = CARTESIAN_POINT ( 'NONE',  ( -2.739355103387247858, -3.994689410813018426, -14.38367211327327588 ) ) ;
#30111 = CARTESIAN_POINT ( 'NONE',  ( 0.5997462898726536595, -45.71211507932792273, 17.94308126043545215 ) ) ;
#30112 = VERTEX_POINT ( 'NONE', #34445 ) ;
#30113 = DIRECTION ( 'NONE',  ( -1.000000000000000000, -0.000000000000000000, -0.000000000000000000 ) ) ;
#30114 = DIRECTION ( 'NONE',  ( -0.07439287786467653485, -0.6957517427943121779, 0.7144194931002993965 ) ) ;
#30115 = FACE_OUTER_BOUND ( 'NONE', #13863, .T. ) ;
#30116 = EDGE_LOOP ( 'NONE', ( #39510, #6600, #32923, #36812 ) ) ;
#30117 = FACE_OUTER_BOUND ( 'NONE', #1565, .T. ) ;
#30118 = CARTESIAN_POINT ( 'NONE',  ( 0.1156495703730067576, 4.372604530253175525, 43.90698444271800582 ) ) ;
#30120 = ORIENTED_EDGE ( 'NONE', *, *, #25129, .F. ) ;
#30119 = CIRCLE ( 'NONE', #17133, 47.91270532121795611 ) ;
#30121 = ORIENTED_EDGE ( 'NONE', *, *, #26734, .F. ) ;
#30122 = EDGE_CURVE ( 'NONE', #40320, #2416, #44247, .T. ) ;
#30123 = ORIENTED_EDGE ( 'NONE', *, *, #32212, .F. ) ;
#30124 = CARTESIAN_POINT ( 'NONE',  ( 0.6008123274975392114, 10.50252768641605705, 47.97136086619308770 ) ) ;
#30126 = ORIENTED_EDGE ( 'NONE', *, *, #23844, .T. ) ;
#30125 = ADVANCED_FACE ( 'NONE', ( #6196 ), #11224, .T. ) ;
#30127 = VERTEX_POINT ( 'NONE', #48524 ) ;
#30128 = EDGE_LOOP ( 'NONE', ( #29631, #39276, #51458, #15987 ) ) ;
#30129 = CARTESIAN_POINT ( 'NONE',  ( 0.1119899015040010243, -12.01552140189033757, -42.45690230849656643 ) ) ;
#30130 = CARTESIAN_POINT ( 'NONE',  ( 0.9775691876210974574, -17.29743328507051103, -38.17240509502285306 ) ) ;
#30131 = ORIENTED_EDGE ( 'NONE', *, *, #32508, .T. ) ;
#30132 = CARTESIAN_POINT ( 'NONE',  ( 0.5998501479064699549, 24.50586714782546593, 41.39809967730496254 ) ) ;
#30133 = EDGE_CURVE ( 'NONE', #46497, #61502, #47147, .T. ) ;
#30134 = B_SPLINE_CURVE_WITH_KNOTS ( 'NONE', 3,
 ( #14179, #37999, #51740, #8837 ),
 .UNSPECIFIED., .F., .F.,
 ( 4, 4 ),
 ( 0.000000000000000000, 0.004447772540403795508 ),
 .UNSPECIFIED. ) ;
#30135 = CARTESIAN_POINT ( 'NONE',  ( -2.569797478183783568, -11.33042594333554298, 9.259773107242873280 ) ) ;
#30136 = ORIENTED_EDGE ( 'NONE', *, *, #30779, .F. ) ;
#30137 = CARTESIAN_POINT ( 'NONE',  ( 5.896278296736517710, -9.661066686813860827, -17.64060004895862832 ) ) ;
#30138 = CARTESIAN_POINT ( 'NONE',  ( 1.231276596079881047, 14.27346765619277846, 39.41503383336979027 ) ) ;
#30139 = CARTESIAN_POINT ( 'NONE',  ( 2.618530812446111078, 12.26263843375577522, -45.38011114840042382 ) ) ;
#30140 = DIRECTION ( 'NONE',  ( -1.000000000000000000, -0.000000000000000000, -0.000000000000000000 ) ) ;
#30141 = EDGE_CURVE ( 'NONE', #25296, #8944, #35243, .T. ) ;
#30142 = ORIENTED_EDGE ( 'NONE', *, *, #26409, .T. ) ;
#30143 = CARTESIAN_POINT ( 'NONE',  ( 0.8753041380234465318, -45.84117188851855218, 17.59901382919725421 ) ) ;
#30144 = B_SPLINE_CURVE_WITH_KNOTS ( 'NONE', 3,
 ( #21776, #8583, #17697, #45915, #55574, #27709 ),
 .UNSPECIFIED., .F., .F.,
 ( 4, 2, 4 ),
 ( 1.515177093957746649E-16, 0.0002445252820015210329, 0.0004890505640028906028 ),
 .UNSPECIFIED. ) ;
#30145 = EDGE_CURVE ( 'NONE', #28177, #29973, #38536, .T. ) ;
#30146 = CARTESIAN_POINT ( 'NONE',  ( 5.895881250540457863, 5.954605924855886023, 19.21120375947254644 ) ) ;
#30147 = B_SPLINE_CURVE_WITH_KNOTS ( 'NONE', 3,
 ( #23678, #9571, #47808, #52792, #28997, #24295, #43429, #469, #58706, #59962, #40581, #21137, #49326, #35567, #59644, #45278 ),
 .UNSPECIFIED., .F., .F.,
 ( 4, 3, 3, 3, 3, 4 ),
 ( 1.868480190406682863E-17, 0.0002618515315864420852, 0.0003927756766342001596, 0.0005236998216950582152, 0.0007855159896329938019, 0.001047349442285931773 ),
 .UNSPECIFIED. ) ;
#30148 = CARTESIAN_POINT ( 'NONE',  ( -6.017396004339687465, -2.460690056887917532, 18.68180398134249387 ) ) ;
#30149 = ORIENTED_EDGE ( 'NONE', *, *, #30691, .T. ) ;
#30150 = CARTESIAN_POINT ( 'NONE',  ( 1.834102595619085507, -42.91893299130839523, -9.907721016725536956 ) ) ;
#30151 = CARTESIAN_POINT ( 'NONE',  ( 5.910764540655178756, -1.997730036635652295, 20.01275376278553964 ) ) ;
#30152 = CARTESIAN_POINT ( 'NONE',  ( 0.8751705887134553219, 38.69254731947794568, 28.56654290188667034 ) ) ;
#30153 = CARTESIAN_POINT ( 'NONE',  ( 1.657374760986086271, -5.806532005084459769, 43.67121057774989623 ) ) ;
#30154 = B_SPLINE_CURVE_WITH_KNOTS ( 'NONE', 3,
 ( #50792, #3173, #30758, #10595 ),
 .UNSPECIFIED., .F., .F.,
 ( 4, 4 ),
 ( 8.064132208641563324E-17, 0.005004741218457511680 ),
 .UNSPECIFIED. ) ;
#30155 = EDGE_LOOP ( 'NONE', ( #56149, #17509, #1845, #44075 ) ) ;
#30156 = ORIENTED_EDGE ( 'NONE', *, *, #8391, .T. ) ;
#30157 = CARTESIAN_POINT ( 'NONE',  ( 0.9730545539215883499, 39.44597740938085195, -16.88610103448514721 ) ) ;
#30158 = CARTESIAN_POINT ( 'NONE',  ( 0.1104177457020372594, 34.21590786699005093, 26.24862037251744340 ) ) ;
#30159 = CARTESIAN_POINT ( 'NONE',  ( 0.9762797500689124330, 15.53330887509137703, -38.92352888134260525 ) ) ;
#30160 = CARTESIAN_POINT ( 'NONE',  ( 4.962356264823608143, -19.84272732133934269, -37.11471096901227185 ) ) ;
#30161 = AXIS2_PLACEMENT_3D ( 'NONE', #16522, #40978, #55328 ) ;
#30162 = CARTESIAN_POINT ( 'NONE',  ( 0.1097557419366048670, 34.07666148910645632, -26.42915440612296152 ) ) ;
#30163 = CARTESIAN_POINT ( 'NONE',  ( 0.1129192098497447394, -31.35755906439637641, 31.04279751098549056 ) ) ;
#30164 = CARTESIAN_POINT ( 'NONE',  ( 0.9790724872846788829, 9.754597114931216950, -40.75761333918888596 ) ) ;
#30165 = CARTESIAN_POINT ( 'NONE',  ( 4.975801465491695552, 27.09127437476327671, 39.51822597168504814 ) ) ;
#30166 = CARTESIAN_POINT ( 'NONE',  ( 3.894904216938897878, -14.62320875324691549, -41.45221463607420276 ) ) ;
#30167 = CARTESIAN_POINT ( 'NONE',  ( 0.1102847568649952675, 30.42833243501150520, -30.55869130182077598 ) ) ;
#30168 =( BOUNDED_SURFACE ( )  B_SPLINE_SURFACE ( 3, 1, ( 
 ( #9566, #28068 ),
 ( #34019, #42495 ),
 ( #61556, #28367 ),
 ( #56862, #33094 ) ),
 .UNSPECIFIED., .F., .F., .F. ) 
 B_SPLINE_SURFACE_WITH_KNOTS ( ( 4, 4 ),
 ( 2, 2 ),
 ( 0.000000000000000000, 1.000000000000000000 ),
 ( 0.000000000000000000, 1.000000000000000000 ),
 .UNSPECIFIED. ) 
 GEOMETRIC_REPRESENTATION_ITEM ( )  RATIONAL_B_SPLINE_SURFACE ( (
 ( 1.000000000000000000, 1.000000000000000000),
 ( 0.7223157951917476005, 0.9931996967497186413),
 ( 0.7223157951917476005, 0.9931996967497186413),
 ( 1.000000000000000000, 1.000000000000000000) ) ) 
 REPRESENTATION_ITEM ( '' )  SURFACE ( )  );
#30169 = CARTESIAN_POINT ( 'NONE',  ( 0.1155031312995260795, -6.875818018218064154, -43.58514378904990849 ) ) ;
#30170 = CARTESIAN_POINT ( 'NONE',  ( 4.975801465491694664, -15.94009207553080643, 45.18341283946430309 ) ) ;
#30171 = EDGE_CURVE ( 'NONE', #20290, #16119, #52323, .T. ) ;
#30172 = CARTESIAN_POINT ( 'NONE',  ( 0.8760168074887076939, 44.09317760313751933, -19.22870327415258274 ) ) ;
#30173 = B_SPLINE_CURVE_WITH_KNOTS ( 'NONE', 3,
 ( #56392, #4067, #55777, #22904 ),
 .UNSPECIFIED., .F., .F.,
 ( 4, 4 ),
 ( 0.000000000000000000, 0.005014147105413690846 ),
 .UNSPECIFIED. ) ;
#30174 = CARTESIAN_POINT ( 'NONE',  ( 0.9722240750034576440, 29.92651530838630336, -30.74950257330989700 ) ) ;
#30175 = CARTESIAN_POINT ( 'NONE',  ( 0.5819845079324659221, -41.25022834067366517, 24.34013310064380065 ) ) ;
#30176 = CARTESIAN_POINT ( 'NONE',  ( -2.569797478183783568, 8.547745408040794857, -11.87678401312186161 ) ) ;
#30177 = ITEM_DEFINED_TRANSFORMATION ( 'NONE', 'NONE', #856,  #14677 ) ;
#30179 = EDGE_CURVE ( 'NONE', #45900, #53021, #1508, .T. ) ;
#30178 = CARTESIAN_POINT ( 'NONE',  ( 4.975801465491694664, -46.87746200127448049, -9.906103548668065528 ) ) ;
#30180 = B_SPLINE_CURVE_WITH_KNOTS ( 'NONE', 3,
 ( #27681, #59950, #54930, #31449, #3850, #22059 ),
 .UNSPECIFIED., .F., .F.,
 ( 4, 2, 4 ),
 ( 1.283058336952897540E-16, 0.0002450741128632341853, 0.0004901482257263400011 ),
 .UNSPECIFIED. ) ;
#30181 = CARTESIAN_POINT ( 'NONE',  ( 0.6029442701453591180, -30.54986712454941866, 38.44802782758372217 ) ) ;
#30182 = EDGE_CURVE ( 'NONE', #58552, #13682, #25036, .T. ) ;
#30183 = CARTESIAN_POINT ( 'NONE',  ( 0.8751705887134423323, -47.55935879196466232, -7.160166390004136794 ) ) ;
#30184 = CARTESIAN_POINT ( 'NONE',  ( 0.6021448801613057400, 49.02259304973922127, -2.885569147777831578 ) ) ;
#30185 = EDGE_CURVE ( 'NONE', #9792, #25496, #4215, .T. ) ;
#30187 = ORIENTED_EDGE ( 'NONE', *, *, #36032, .F. ) ;
#30186 = LINE ( 'NONE', #25184, #4310 ) ;
#30188 = ORIENTED_EDGE ( 'NONE', *, *, #26595, .T. ) ;
#30189 = CARTESIAN_POINT ( 'NONE',  ( 0.2230388203127599833, -33.74101226470682491, 26.84831060237785749 ) ) ;
#30190 = CARTESIAN_POINT ( 'NONE',  ( 3.050102900204245682, 43.74992430961583523, -4.622701816140248887 ) ) ;
#30191 = EDGE_CURVE ( 'NONE', #28349, #60557, #19399, .T. ) ;
#30192 = CARTESIAN_POINT ( 'NONE',  ( 0.1157991065609915576, 41.85057238631154064, 13.98112858376594758 ) ) ;
#30193 = ORIENTED_EDGE ( 'NONE', *, *, #54284, .F. ) ;
#30194 = ORIENTED_EDGE ( 'NONE', *, *, #38755, .T. ) ;
#30195 = CARTESIAN_POINT ( 'NONE',  ( 3.238018933889920792, -10.88486934301737996, -7.805582089318734873 ) ) ;
#30196 = CARTESIAN_POINT ( 'NONE',  ( -6.016104459813374383, 11.47525878590937864, -14.94608397322072157 ) ) ;
#30197 = DIRECTION ( 'NONE',  ( -0.000000000000000000, -0.000000000000000000, 1.000000000000000000 ) ) ;
#30198 = EDGE_LOOP ( 'NONE', ( #7549, #16518, #39631, #10464 ) ) ;
#30199 = ORIENTED_EDGE ( 'NONE', *, *, #54444, .F. ) ;
#30200 = EDGE_CURVE ( 'NONE', #10972, #9573, #48231, .T. ) ;
#30201 = FACE_OUTER_BOUND ( 'NONE', #12986, .T. ) ;
#30202 = CARTESIAN_POINT ( 'NONE',  ( 0.6846871229502932144, 29.84551600520687131, -37.47592888575217529 ) ) ;
#30203 = CARTESIAN_POINT ( 'NONE',  ( 0.5835226383429301666, -38.76587123842037386, -26.39033348921869049 ) ) ;
#30204 = B_SPLINE_CURVE_WITH_KNOTS ( 'NONE', 3,
 ( #19757, #14749, #10351, #43896, #57933, #1540, #33864, #25059, #52939, #10041, #44506, #53544, #1235, #20678, #5308, #39812, #24438, #20368, #58867 ),
 .UNSPECIFIED., .F., .F.,
 ( 4, 3, 3, 3, 3, 3, 4 ),
 ( 1.355252715606880543E-20, 0.0002612768053151701369, 0.0003919133833142879981, 0.0005225499612322599945, 0.0006531865391693327059, 0.0008112755173415169300, 0.0009693688056799694289 ),
 .UNSPECIFIED. ) ;
#30205 = DIRECTION ( 'NONE',  ( 0.07500201931887537365, -0.9863955245047961728, -0.1462824881351111328 ) ) ;
#30206 = MANIFOLD_SOLID_BREP ( 'Move Face1', #16058 ) ;
#30207 = CARTESIAN_POINT ( 'NONE',  ( 0.9790724872846777727, -41.06080244794662093, -8.387235081488672250 ) ) ;
#30208 = CIRCLE ( 'NONE', #52209, 42.08604991992415023 ) ;
#30209 = CARTESIAN_POINT ( 'NONE',  ( 0.5980894510889457338, -48.10766805928368939, 0.7015180096003246213 ) ) ;
#30210 = LINE ( 'NONE', #44963, #15965 ) ;
#30211 = VERTEX_POINT ( 'NONE', #3064 ) ;
#30212 = ORIENTED_EDGE ( 'NONE', *, *, #54598, .T. ) ;
#30213 = CARTESIAN_POINT ( 'NONE',  ( 1.231276596079887264, 33.41651732065550817, 25.31033664684050777 ) ) ;
#30214 = DIRECTION ( 'NONE',  ( -1.000000000000000000, -0.000000000000000000, -0.000000000000000000 ) ) ;
#30215 = ORIENTED_EDGE ( 'NONE', *, *, #60760, .T. ) ;
#30216 = DIRECTION ( 'NONE',  ( 0.09835009131224564660, 0.5996571005210301619, 0.7941905447268835516 ) ) ;
#30217 = CARTESIAN_POINT ( 'NONE',  ( 0.5988103564986356764, 44.67429521517308189, 17.84821699813498341 ) ) ;
#30218 = CARTESIAN_POINT ( 'NONE',  ( 0.1154773475650540809, -40.96660263512894318, -16.39149470248417728 ) ) ;
#30219 = ORIENTED_EDGE ( 'NONE', *, *, #59584, .T. ) ;
#30220 = CARTESIAN_POINT ( 'NONE',  ( 0.5809828226811617480, -38.32755012159166341, 28.72298383114474518 ) ) ;
#30221 = CARTESIAN_POINT ( 'NONE',  ( 3.999999999999990674, -2.309401076758548221, -5.242734410091827613 ) ) ;
#30222 = B_SPLINE_CURVE_WITH_KNOTS ( 'NONE', 3,
 ( #40759, #16939, #55117, #31018, #31953, #12546 ),
 .UNSPECIFIED., .F., .F.,
 ( 4, 2, 4 ),
 ( 2.224174099750402646E-17, 0.0002293319059085101167, 0.0004586638118169979531 ),
 .UNSPECIFIED. ) ;
#30223 = CARTESIAN_POINT ( 'NONE',  ( 0.5832367798473397924, 44.14510605973678281, 18.58036934788090022 ) ) ;
#30224 = EDGE_CURVE ( 'NONE', #5867, #54484, #58980, .T. ) ;
#30225 = FACE_OUTER_BOUND ( 'NONE', #27444, .T. ) ;
#30226 = ORIENTED_EDGE ( 'NONE', *, *, #1450, .F. ) ;
#30227 = CARTESIAN_POINT ( 'NONE',  ( 0.5850706913938534814, 23.79070617305439583, -41.56998471741203360 ) ) ;
#30228 = DIRECTION ( 'NONE',  ( -1.000000000000000000, -1.836970198721033632E-16, 2.218671295934095703E-31 ) ) ;
#30229 = ORIENTED_EDGE ( 'NONE', *, *, #51178, .F. ) ;
#30230 = CARTESIAN_POINT ( 'NONE',  ( 0.5988103564986357874, 41.96244062389618534, 23.52668867203664860 ) ) ;
#30231 = CARTESIAN_POINT ( 'NONE',  ( 0.3676999524040323597, 41.59822836379060362, 14.68121181363330408 ) ) ;
#30232 = EDGE_LOOP ( 'NONE', ( #16311, #9507, #38062, #25293 ) ) ;
#30233 = CARTESIAN_POINT ( 'NONE',  ( 4.553261556744875094, 7.233533384971297941, -43.32684572631779218 ) ) ;
#30234 = CARTESIAN_POINT ( 'NONE',  ( -2.569797478183783568, -12.44213550320658612, 7.701637110048465296 ) ) ;
#30235 = CARTESIAN_POINT ( 'NONE',  ( 0.9968887458511664912, -39.89008038581154381, 15.81144734640172622 ) ) ;
#30236 = CARTESIAN_POINT ( 'NONE',  ( 3.376099380956842921, 13.33943071323250606, 1.329651036526637409 ) ) ;
#30237 = CARTESIAN_POINT ( 'NONE',  ( 4.958415959904820092, -43.67231206503777940, 12.48731807541533101 ) ) ;
#30238 = CARTESIAN_POINT ( 'NONE',  ( 0.2285344041767087830, -41.17386732079742728, -15.84972618516879450 ) ) ;
#30239 = CARTESIAN_POINT ( 'NONE',  ( 2.643462169533600914, 7.637863311827604029, -47.42536612906420856 ) ) ;
#30240 = FACE_OUTER_BOUND ( 'NONE', #34699, .T. ) ;
#30241 = CARTESIAN_POINT ( 'NONE',  ( 0.5827357941260210561, -23.63272379758821629, 41.65958460246764616 ) ) ;
#30242 = CARTESIAN_POINT ( 'NONE',  ( 0.5809828226811553087, -33.48000389720640868, 34.25055090842140970 ) ) ;
#30243 = DIRECTION ( 'NONE',  ( 0.1024043820194936449, 0.5087173657443462282, 0.8548216096551014553 ) ) ;
#30244 = VERTEX_POINT ( 'NONE', #55373 ) ;
#30245 = B_SPLINE_CURVE_WITH_KNOTS ( 'NONE', 3,
 ( #12212, #50692, #26908, #21285 ),
 .UNSPECIFIED., .F., .F.,
 ( 4, 4 ),
 ( 6.254634441385501517E-18, 0.004566006591234648103 ),
 .UNSPECIFIED. ) ;
#30246 = CARTESIAN_POINT ( 'NONE',  ( -17.04155827523767641, -12.35689285834061302, 1.886809682956876122 ) ) ;
#30247 = CARTESIAN_POINT ( 'NONE',  ( 0.6039202388192952409, 37.50551550546116175, -31.70015803617710404 ) ) ;
#30248 = CARTESIAN_POINT ( 'NONE',  ( 5.960721111146673579, 5.306302591836305815, 19.82781442290499996 ) ) ;
#30249 = CARTESIAN_POINT ( 'NONE',  ( -6.078075953587585900, -1.843738688193441666, -19.16757162232072531 ) ) ;
#30250 = DIRECTION ( 'NONE',  ( -0.000000000000000000, -0.000000000000000000, 1.000000000000000000 ) ) ;
#30251 = VECTOR ( 'NONE', #39165, 1000.000000000000000 ) ;
#30252 = ADVANCED_BREP_SHAPE_REPRESENTATION ( '', ( #9707, #14677 ), #24677 ) ;
#30253 = DIRECTION ( 'NONE',  ( -0.07836865515943411409, -0.6006129930017440888, 0.7956898808744451435 ) ) ;
#30254 = DIRECTION ( 'NONE',  ( -1.000000000000000000, 4.883898427651973489E-15, -4.807811143603731296E-15 ) ) ;
#30256 = EDGE_CURVE ( 'NONE', #44981, #5400, #30966, .T. ) ;
#30255 = CARTESIAN_POINT ( 'NONE',  ( 4.549368137175248350, -28.46244473166650479, -32.13400537129916046 ) ) ;
#30257 = VECTOR ( 'NONE', #16294, 1000.000000000000000 ) ;
#30258 = CARTESIAN_POINT ( 'NONE',  ( 1.227938101723748288, 29.74462687941226235, 30.94118573761323177 ) ) ;
#30259 = EDGE_CURVE ( 'NONE', #17098, #21985, #61240, .T. ) ;
#30260 = CARTESIAN_POINT ( 'NONE',  ( 0.6023143664670691511, 0.2618215695307587465, -48.10676742339276046 ) ) ;
#30261 = ADVANCED_FACE ( 'NONE', ( #60084 ), #28260, .F. ) ;
#30263 = EDGE_LOOP ( 'NONE', ( #7502, #55022, #32398, #32968 ) ) ;
#30262 = CARTESIAN_POINT ( 'NONE',  ( 4.549368137175248350, -38.40568845698262379, -19.17571786012310753 ) ) ;
#30264 = VERTEX_POINT ( 'NONE', #50375 ) ;
#30265 = CARTESIAN_POINT ( 'NONE',  ( 2.301430502907645614, 1.287492012859394963, -48.01619648598872203 ) ) ;
#30266 = B_SPLINE_CURVE_WITH_KNOTS ( 'NONE', 3,
 ( #44996, #38756, #20550, #39368, #29625, #6105 ),
 .UNSPECIFIED., .F., .F.,
 ( 4, 2, 4 ),
 ( 0.000000000000000000, 0.0002291966416970801085, 0.0004583932833941602170 ),
 .UNSPECIFIED. ) ;
#30267 = ADVANCED_FACE ( 'NONE', ( #25962 ), #25644, .F. ) ;
#30268 = CARTESIAN_POINT ( 'NONE',  ( 0.1368894036331258779, -42.83744898368259868, -10.57422765471428860 ) ) ;
#30269 = CARTESIAN_POINT ( 'NONE',  ( -6.016761891674564211, -16.31696541414278911, 9.424569481870193499 ) ) ;
#30270 = CARTESIAN_POINT ( 'NONE',  ( 0.5998501479064699549, 0.5236536531308225717, 48.10473956285920138 ) ) ;
#30271 = CARTESIAN_POINT ( 'NONE',  ( 0.6254311100348659558, 41.31309618784381854, 24.64676532715809643 ) ) ;
#30272 =( BOUNDED_SURFACE ( )  B_SPLINE_SURFACE ( 3, 1, ( 
 ( #7196, #55434 ),
 ( #49825, #2507 ),
 ( #12557, #26024 ),
 ( #49205, #6252 ) ),
 .UNSPECIFIED., .F., .F., .F. ) 
 B_SPLINE_SURFACE_WITH_KNOTS ( ( 4, 4 ),
 ( 2, 2 ),
 ( 0.000000000000000000, 1.000000000000000000 ),
 ( 0.000000000000000000, 1.000000000000000000 ),
 .UNSPECIFIED. ) 
 GEOMETRIC_REPRESENTATION_ITEM ( )  RATIONAL_B_SPLINE_SURFACE ( (
 ( 1.000000000000000000, 1.000000000000000000),
 ( 0.9732289882329797637, 0.9999525324661233672),
 ( 0.9732289882329797637, 0.9999525324661233672),
 ( 1.000000000000000000, 1.000000000000000000) ) ) 
 REPRESENTATION_ITEM ( '' )  SURFACE ( )  );
#30273 = ORIENTED_EDGE ( 'NONE', *, *, #18335, .T. ) ;
#30274 = ORIENTED_EDGE ( 'NONE', *, *, #6733, .F. ) ;
#30275 = CARTESIAN_POINT ( 'NONE',  ( -5.272380000000000067, 0.000000000000000000, 0.000000000000000000 ) ) ;
#30276 = EDGE_CURVE ( 'NONE', #243, #13900, #40706, .T. ) ;
#30277 = CARTESIAN_POINT ( 'NONE',  ( -6.078726893082806448, -18.90026279491059924, 3.684305572565647946 ) ) ;
#30278 = CARTESIAN_POINT ( 'NONE',  ( 4.549368137175248350, -3.018832571116246477, -42.82045902618772004 ) ) ;
#30279 = ORIENTED_EDGE ( 'NONE', *, *, #23218, .T. ) ;
#30280 = EDGE_CURVE ( 'NONE', #20220, #40686, #40271, .T. ) ;
#30281 = CARTESIAN_POINT ( 'NONE',  ( 0.1073791018717578927, -0.4849339620936172768, 43.12183934961190346 ) ) ;
#30282 = CARTESIAN_POINT ( 'NONE',  ( 4.975610109902397937, 0.000000000000000000, 0.000000000000000000 ) ) ;
#30283 = VERTEX_POINT ( 'NONE', #11565 ) ;
#30284 =( BOUNDED_SURFACE ( )  B_SPLINE_SURFACE ( 3, 1, ( 
 ( #40215, #21070 ),
 ( #54246, #21381 ),
 ( #20158, #30766 ),
 ( #54552, #45216 ) ),
 .UNSPECIFIED., .F., .F., .F. ) 
 B_SPLINE_SURFACE_WITH_KNOTS ( ( 4, 4 ),
 ( 2, 2 ),
 ( 0.000000000000000000, 1.000000000000000000 ),
 ( 0.000000000000000000, 1.000000000000000000 ),
 .UNSPECIFIED. ) 
 GEOMETRIC_REPRESENTATION_ITEM ( )  RATIONAL_B_SPLINE_SURFACE ( (
 ( 1.000000000000000000, 1.000000000000000000),
 ( 0.9754377213608244057, 0.9999580625633939235),
 ( 0.9754377213608244057, 0.9999580625633939235),
 ( 1.000000000000000000, 1.000000000000000000) ) ) 
 REPRESENTATION_ITEM ( '' )  SURFACE ( )  );
#30285 = CARTESIAN_POINT ( 'NONE',  ( 4.553261556744873317, -20.11719049292697648, 39.04917684785332455 ) ) ;
#30286 = ORIENTED_EDGE ( 'NONE', *, *, #39008, .F. ) ;
#30287 = CARTESIAN_POINT ( 'NONE',  ( 0.5834584762367746036, -34.90241844189876730, 31.32183225674696558 ) ) ;
#30288 = CARTESIAN_POINT ( 'NONE',  ( 0.1073791018717483448, 41.77800844988500018, 10.69234304550068337 ) ) ;
#30289 = ORIENTED_EDGE ( 'NONE', *, *, #11452, .F. ) ;
#30290 = CARTESIAN_POINT ( 'NONE',  ( 2.618530812446115519, 41.14519205294185866, 22.73323470438666405 ) ) ;
#30291 = DIRECTION ( 'NONE',  ( -1.000000000000000000, -0.000000000000000000, -0.000000000000000000 ) ) ;
#30292 = CARTESIAN_POINT ( 'NONE',  ( 0.5839879882012688483, 41.47910964649828003, -23.94800997596641423 ) ) ;
#30293 = CARTESIAN_POINT ( 'NONE',  ( 0.2885697896453111588, 43.10898998017122352, 0.8047882042608043296 ) ) ;
#30294 = B_SPLINE_CURVE_WITH_KNOTS ( 'NONE', 3,
 ( #35010, #25898, #54686, #11818, #59391, #15584 ),
 .UNSPECIFIED., .F., .F.,
 ( 4, 2, 4 ),
 ( 1.519728548185745998E-16, 0.0002445252820015179429, 0.0004890505640028839892 ),
 .UNSPECIFIED. ) ;
#30295 = ORIENTED_EDGE ( 'NONE', *, *, #59760, .F. ) ;
#30296 = CARTESIAN_POINT ( 'NONE',  ( 0.8554163680231816613, -38.15570339590838245, 27.30105806512422717 ) ) ;
#30297 = CARTESIAN_POINT ( 'NONE',  ( 0.1157991065609916131, 39.78975866839436293, -19.07137831014408746 ) ) ;
#30298 = VERTEX_POINT ( 'NONE', #30642 ) ;
#30299 = CARTESIAN_POINT ( 'NONE',  ( 3.680882792899937250, 47.77138407787916918, 4.423598386734563626 ) ) ;
#30300 = B_SPLINE_CURVE_WITH_KNOTS ( 'NONE', 3,
 ( #57853, #49699, #34694, #40036, #1764, #10891 ),
 .UNSPECIFIED., .F., .F.,
 ( 4, 2, 4 ),
 ( 5.854691731421724714E-18, 0.0002291472222819923663, 0.0004582944445639788780 ),
 .UNSPECIFIED. ) ;
#30301 = ADVANCED_FACE ( 'NONE', ( #49762 ), #41465, .F. ) ;
#30302 = VERTEX_POINT ( 'NONE', #46318 ) ;
#30303 = CARTESIAN_POINT ( 'NONE',  ( 0.5836750258453363704, -18.49664649301221786, 44.18029554260628089 ) ) ;
#30304 = ORIENTED_EDGE ( 'NONE', *, *, #21395, .F. ) ;
#30305 = CARTESIAN_POINT ( 'NONE',  ( 0.5807400328401637335, -0.5448834511086642074, -47.89582301953904420 ) ) ;
#30306 = CARTESIAN_POINT ( 'NONE',  ( 0.9783242366443551941, 36.19415619989782584, -21.12622889168628504 ) ) ;
#30307 = DIRECTION ( 'NONE',  ( -1.000000000000000000, -0.000000000000000000, -0.000000000000000000 ) ) ;
#30308 = VERTEX_POINT ( 'NONE', #41935 ) ;
#30309 = CARTESIAN_POINT ( 'NONE',  ( 0.1129192098497447394, 43.40062318508790895, 7.958498283669150020 ) ) ;
#30310 = CARTESIAN_POINT ( 'NONE',  ( 0.5809828226811617480, -6.791453954330657794, 47.41188724015877654 ) ) ;
#30311 = CARTESIAN_POINT ( 'NONE',  ( 0.9730545539215892381, -11.59290486963536360, 41.31259007387227911 ) ) ;
#30312 = B_SPLINE_CURVE_WITH_KNOTS ( 'NONE', 3,
 ( #12624, #4100, #27015, #55811 ),
 .UNSPECIFIED., .F., .F.,
 ( 4, 4 ),
 ( 0.000000000000000000, 0.005004741218457425811 ),
 .UNSPECIFIED. ) ;
#30313 = VERTEX_POINT ( 'NONE', #27811 ) ;
#30314 = AXIS2_PLACEMENT_3D ( 'NONE', #39307, #48377, #58365 ) ;
#30315 = ORIENTED_EDGE ( 'NONE', *, *, #19937, .T. ) ;
#30316 = CARTESIAN_POINT ( 'NONE',  ( 0.5839879327111916485, 18.41291455875303029, 44.21534283185609837 ) ) ;
#30317 = CARTESIAN_POINT ( 'NONE',  ( -6.057079549204054558, -18.90348671888462917, 3.672794708214838000 ) ) ;
#30318 = CARTESIAN_POINT ( 'NONE',  ( 4.956653778116994147, 32.11725092155092653, -35.79382859084083179 ) ) ;
#30319 = CARTESIAN_POINT ( 'NONE',  ( 1.827119703190780653, -41.88501940447986982, -9.946884032290961741 ) ) ;
#30320 = CARTESIAN_POINT ( 'NONE',  ( 1.227938101723748288, 34.55893248994541267, -25.45152231597022308 ) ) ;
#30321 = CARTESIAN_POINT ( 'NONE',  ( 3.270143674763207553, 3.806843787665915801, 13.14781761974170671 ) ) ;
#30322 = ORIENTED_EDGE ( 'NONE', *, *, #27745, .F. ) ;
#30323 = CARTESIAN_POINT ( 'NONE',  ( 4.553261556744873317, -29.69864478935373242, -32.36556910513746743 ) ) ;
#30324 = FACE_OUTER_BOUND ( 'NONE', #23888, .T. ) ;
#30325 = EDGE_LOOP ( 'NONE', ( #14807, #24989, #55784, #38582 ) ) ;
#30326 = LINE ( 'NONE', #26245, #44381 ) ;
#30327 = CARTESIAN_POINT ( 'NONE',  ( -4.000000000000000000, -1.933795701539610334, -5.351162342337702604 ) ) ;
#30328 = CARTESIAN_POINT ( 'NONE',  ( 0.5786265663353196143, 24.57327059187455731, -41.11783955080211683 ) ) ;
#30329 = CARTESIAN_POINT ( 'NONE',  ( 1.479689385636123067, 10.94758276098252558, 42.68177921501317229 ) ) ;
#30330 =( NAMED_UNIT ( * ) PLANE_ANGLE_UNIT ( ) SI_UNIT ( $, .RADIAN. ) );
#30331 =( NAMED_UNIT ( * ) PLANE_ANGLE_UNIT ( ) SI_UNIT ( $, .RADIAN. ) );
#30332 = CARTESIAN_POINT ( 'NONE',  ( 0.3622758884714730732, -43.10531414739105571, 0.8252992914326598983 ) ) ;
#30333 = CARTESIAN_POINT ( 'NONE',  ( 0.8760168074887076939, -46.22580377597795120, 13.30888447662000473 ) ) ;
#30334 = EDGE_CURVE ( 'NONE', #53833, #15433, #29803, .T. ) ;
#30335 = CARTESIAN_POINT ( 'NONE',  ( 0.5807400328401637335, 47.89582301953903709, 0.5448834511091745769 ) ) ;
#30336 = CARTESIAN_POINT ( 'NONE',  ( 0.2285344041767098933, -2.173305968327541304, -44.06560916932259175 ) ) ;
#30337 = CARTESIAN_POINT ( 'NONE',  ( 4.549368137175248350, 0.000000000000000000, 0.000000000000000000 ) ) ;
#30338 = EDGE_CURVE ( 'NONE', #32393, #48631, #50770, .T. ) ;
#30339 = CARTESIAN_POINT ( 'NONE',  ( 0.1119898979215348950, -17.34614202713813569, 40.57182107111018610 ) ) ;
#30340 = CARTESIAN_POINT ( 'NONE',  ( 4.956445790443988031, 0.000000000000000000, 0.000000000000000000 ) ) ;
#30341 = VECTOR ( 'NONE', #57500, 1000.000000000000114 ) ;
#30342 = CARTESIAN_POINT ( 'NONE',  ( 2.281351352603293137, -45.98107981851856607, -13.68106635380611991 ) ) ;
#30343 = CARTESIAN_POINT ( 'NONE',  ( 0.3676999524040323597, 40.09552319080426486, -18.39292264373764851 ) ) ;
#30344 = ORIENTED_EDGE ( 'NONE', *, *, #14205, .F. ) ;
#30345 = CARTESIAN_POINT ( 'NONE',  ( 0.3622758884714600280, -39.50828911766986096, -17.25816669464980890 ) ) ;
#30346 = EDGE_CURVE ( 'NONE', #22109, #39562, #21605, .T. ) ;
#30347 = CARTESIAN_POINT ( 'NONE',  ( 0.1073791018717578927, 37.10214135362858912, 21.98088480513677823 ) ) ;
#30348 = CARTESIAN_POINT ( 'NONE',  ( 0.1157991065609915993, -38.40619918333140959, -21.72340281419956654 ) ) ;
#30349 = CARTESIAN_POINT ( 'NONE',  ( 4.975610109902397937, -22.11219452748553138, -43.62912170003438916 ) ) ;
#30350 = DIRECTION ( 'NONE',  ( -1.000000000000000000, -0.000000000000000000, -0.000000000000000000 ) ) ;
#30351 = ORIENTED_EDGE ( 'NONE', *, *, #61535, .F. ) ;
#30352 = EDGE_CURVE ( 'NONE', #3325, #2691, #20216, .T. ) ;
#30353 = CARTESIAN_POINT ( 'NONE',  ( 4.303969348037258058, -48.06163817123227489, 2.158280495710045876 ) ) ;
#30354 = CARTESIAN_POINT ( 'NONE',  ( 0.9756950546413942771, 16.33093981194375033, -39.67916378221920581 ) ) ;
#30355 = CARTESIAN_POINT ( 'NONE',  ( 4.834790513006553603, 24.88720127704591789, -40.16486715427035392 ) ) ;
#30356 = ORIENTED_EDGE ( 'NONE', *, *, #55689, .F. ) ;
#30357 = CARTESIAN_POINT ( 'NONE',  ( 4.553261556744875094, -43.85016385001095784, 2.588956575693979190 ) ) ;
#30358 = DIRECTION ( 'NONE',  ( -1.000000000000000000, -3.135800716341471541E-16, -1.298891185607920445E-16 ) ) ;
#30359 = ORIENTED_EDGE ( 'NONE', *, *, #24821, .F. ) ;
#30360 = FACE_OUTER_BOUND ( 'NONE', #45877, .T. ) ;
#30361 = ORIENTED_EDGE ( 'NONE', *, *, #13814, .T. ) ;
#30362 = LINE ( 'NONE', #49475, #54439 ) ;
#30363 = ORIENTED_EDGE ( 'NONE', *, *, #34146, .F. ) ;
#30364 = CARTESIAN_POINT ( 'NONE',  ( 0.9730545539215883499, 21.89037132892435622, 36.90443313492338717 ) ) ;
#30365 = CARTESIAN_POINT ( 'NONE',  ( 5.958863334805807099, -17.77634700750921937, -10.26176968287938784 ) ) ;
#30366 = EDGE_LOOP ( 'NONE', ( #16216, #29029, #53112, #5392 ) ) ;
#30367 = VERTEX_POINT ( 'NONE', #17803 ) ;
#30368 = CARTESIAN_POINT ( 'NONE',  ( 0.9785694773339237429, 20.33543408136244324, -36.64431096960669265 ) ) ;
#30369 = DIRECTION ( 'NONE',  ( 1.000000000000000000, 0.000000000000000000, 0.000000000000000000 ) ) ;
#30370 = EDGE_CURVE ( 'NONE', #60419, #19501, #24599, .T. ) ;
#30371 = ORIENTED_EDGE ( 'NONE', *, *, #29520, .F. ) ;
#30372 = EDGE_LOOP ( 'NONE', ( #42960, #23216, #4440, #49002 ) ) ;
#30373 = DIRECTION ( 'NONE',  ( -0.1024043820194934645, 0.8548216096550962373, 0.5087173657443551100 ) ) ;
#30374 = CARTESIAN_POINT ( 'NONE',  ( 0.5819845901640485764, 34.18710267837700911, -33.54497622115095368 ) ) ;
#30375 = CARTESIAN_POINT ( 'NONE',  ( 0.6030672727741701600, 23.97812608463474859, 41.70584815505896614 ) ) ;
#30376 = ORIENTED_EDGE ( 'NONE', *, *, #49706, .F. ) ;
#30377 = CARTESIAN_POINT ( 'NONE',  ( 0.6001305935487422083, -46.33281397023054637, -12.95698906763792557 ) ) ;
#30378 = CARTESIAN_POINT ( 'NONE',  ( -2.600000000000000533, -11.64055411052240352, 0.000000000000000000 ) ) ;
#30379 = ORIENTED_EDGE ( 'NONE', *, *, #56080, .F. ) ;
#30380 = AXIS2_PLACEMENT_3D ( 'NONE', #1729, #40004, #54343 ) ;
#30381 = CARTESIAN_POINT ( 'NONE',  ( 4.958415959904820980, -45.08182420577212923, 5.552754280759789829 ) ) ;
#30382 = VERTEX_POINT ( 'NONE', #50987 ) ;
#30383 = CARTESIAN_POINT ( 'NONE',  ( 4.967162193818130511, -38.44485641567084855, 19.45289607368810181 ) ) ;
#30384 =( BOUNDED_SURFACE ( )  B_SPLINE_SURFACE ( 3, 1, ( 
 ( #54059, #15882 ),
 ( #16185, #35298 ),
 ( #6738, #59379 ),
 ( #20572, #24970 ) ),
 .UNSPECIFIED., .F., .F., .F. ) 
 B_SPLINE_SURFACE_WITH_KNOTS ( ( 4, 4 ),
 ( 2, 2 ),
 ( 0.000000000000000000, 1.000000000000000000 ),
 ( 0.000000000000000000, 1.000000000000000000 ),
 .UNSPECIFIED. ) 
 GEOMETRIC_REPRESENTATION_ITEM ( )  RATIONAL_B_SPLINE_SURFACE ( (
 ( 1.000000000000000000, 1.000000000000000000),
 ( 0.7269869731126817891, 0.9931720237060910339),
 ( 0.7269869731126817891, 0.9931720237060910339),
 ( 1.000000000000000000, 1.000000000000000000) ) ) 
 REPRESENTATION_ITEM ( '' )  SURFACE ( )  );
#30385 = CARTESIAN_POINT ( 'NONE',  ( 4.975801465491695552, -2.564218696447830403, 47.84403947906839250 ) ) ;
#30386 = EDGE_LOOP ( 'NONE', ( #22516, #248, #60174, #43483 ) ) ;
#30387 = CARTESIAN_POINT ( 'NONE',  ( -2.600000000000000533, -11.64055411052240352, -1.199999999999999956 ) ) ;
#30388 = LINE ( 'NONE', #11300, #55757 ) ;
#30389 = CARTESIAN_POINT ( 'NONE',  ( 53.15006792977867178, 12.50001440111202022, 0.1723589083839783265 ) ) ;
#30390 = CARTESIAN_POINT ( 'NONE',  ( 0.7242486021783806072, 49.04682582606951513, -2.328162099418285003 ) ) ;
#30391 = B_SPLINE_CURVE_WITH_KNOTS ( 'NONE', 3,
 ( #7339, #27092, #3261, #21463 ),
 .UNSPECIFIED., .F., .F.,
 ( 4, 4 ),
 ( 0.000000000000000000, 0.004447772540403832804 ),
 .UNSPECIFIED. ) ;
#30392 = ORIENTED_EDGE ( 'NONE', *, *, #60745, .F. ) ;
#30393 = CARTESIAN_POINT ( 'NONE',  ( 0.8751705887134553219, -38.69254731947813752, -28.56654290188640033 ) ) ;
#30394 = EDGE_LOOP ( 'NONE', ( #47585, #27532, #28586, #49232 ) ) ;
#30395 = CARTESIAN_POINT ( 'NONE',  ( 0.6254311100348639574, 44.17670535157486000, 19.04346769887709101 ) ) ;
#30397 = B_SPLINE_CURVE_WITH_KNOTS ( 'NONE', 3,
 ( #46029, #22197, #41321, #39396, #1142, #4589 ),
 .UNSPECIFIED., .F., .F.,
 ( 4, 2, 4 ),
 ( 1.738108305489988542E-18, 0.0002291459268755701535, 0.0004582918537511385722 ),
 .UNSPECIFIED. ) ;
#30396 = CARTESIAN_POINT ( 'NONE',  ( -4.923482091946715045, -0.9563062221994793610, 5.749747411347113621E-14 ) ) ;
#30398 = AXIS2_PLACEMENT_3D ( 'NONE', #60968, #3944, #37830 ) ;
#30399 = CARTESIAN_POINT ( 'NONE',  ( 5.838029081930957709, -43.47829931555697414, 18.45812955799579669 ) ) ;
#30400 = CARTESIAN_POINT ( 'NONE',  ( 4.335381028904201628, 0.5556724879614545198, -48.98416147848676871 ) ) ;
#30401 = EDGE_CURVE ( 'NONE', #15298, #6759, #54417, .T. ) ;
#30402 = CARTESIAN_POINT ( 'NONE',  ( 4.960156602257182357, -3.546989772329588675, -46.28683144126599558 ) ) ;
#30403 = CARTESIAN_POINT ( 'NONE',  ( 0.9749527285493316819, 37.30179927241204751, -21.20640438431149732 ) ) ;
#30404 = EDGE_CURVE ( 'NONE', #58558, #18771, #13415, .T. ) ;
#30405 = CARTESIAN_POINT ( 'NONE',  ( 0.6254311100348624031, -42.00127298835437983, 23.45480814408353254 ) ) ;
#30406 = CARTESIAN_POINT ( 'NONE',  ( 4.549368137175248350, 32.13400537129925283, -28.46244473166639111 ) ) ;
#30407 = CARTESIAN_POINT ( 'NONE',  ( 0.3622758884714730732, 41.42293301073625855, -11.95365414648454205 ) ) ;
#30408 = CARTESIAN_POINT ( 'NONE',  ( -6.015611763856276717, -11.47596948473801248, -14.94556629257436953 ) ) ;
#30409 = ADVANCED_FACE ( 'NONE', ( #3978 ), #45485, .F. ) ;
#30410 = B_SPLINE_CURVE_WITH_KNOTS ( 'NONE', 3,
 ( #56087, #9398, #23205, #32928 ),
 .UNSPECIFIED., .F., .F.,
 ( 4, 4 ),
 ( 0.000000000000000000, 0.005004741218457409331 ),
 .UNSPECIFIED. ) ;
#30411 = DIRECTION ( 'NONE',  ( 0.000000000000000000, 0.000000000000000000, 1.000000000000000000 ) ) ;
#30412 = CARTESIAN_POINT ( 'NONE',  ( 0.1154773475650541087, 37.07776829763225379, 23.92034130427944660 ) ) ;
#30413 = VERTEX_POINT ( 'NONE', #56613 ) ;
#30414 = DIRECTION ( 'NONE',  ( -1.000000000000000000, 0.000000000000000000, 0.000000000000000000 ) ) ;
#30415 = DIRECTION ( 'NONE',  ( 0.000000000000000000, 0.000000000000000000, -1.000000000000000000 ) ) ;
#30416 = CARTESIAN_POINT ( 'NONE',  ( 4.975610109902397937, 14.46773809681615575, -46.72401910687593585 ) ) ;
#30417 = ORIENTED_EDGE ( 'NONE', *, *, #39772, .F. ) ;
#30418 = EDGE_CURVE ( 'NONE', #5544, #29351, #22193, .T. ) ;
#30419 = CARTESIAN_POINT ( 'NONE',  ( 4.303969348037246512, -10.35452842635810455, -46.98258166031700966 ) ) ;
#30420 = DIRECTION ( 'NONE',  ( 1.000000000000000000, 0.000000000000000000, -0.000000000000000000 ) ) ;
#30421 = AXIS2_PLACEMENT_3D ( 'NONE', #35914, #26489, #16480 ) ;
#30422 = CARTESIAN_POINT ( 'NONE',  ( -2.708315649062910779, -2.171184472130790244, 14.47261168455365876 ) ) ;
#30423 = PRODUCT_DEFINITION_CONTEXT ( 'detailed design', #50454, 'design' ) ;
#30424 = ORIENTED_EDGE ( 'NONE', *, *, #25117, .F. ) ;
#30425 = CARTESIAN_POINT ( 'NONE',  ( 0.5800708057587371513, -33.42085258735453834, -34.30831467131393708 ) ) ;
#30426 = CARTESIAN_POINT ( 'NONE',  ( 0.8744876279028306332, 37.95405449045402690, 31.14225101233274273 ) ) ;
#30427 = AXIS2_PLACEMENT_3D ( 'NONE', #22843, #57474, #14616 ) ;
#30428 = EDGE_LOOP ( 'NONE', ( #7379, #8795, #37904, #8004 ) ) ;
#30429 = CARTESIAN_POINT ( 'NONE',  ( 5.960221823109900008, 12.49086489703206304, 16.28736530777594993 ) ) ;
#30430 = ORIENTED_EDGE ( 'NONE', *, *, #50647, .T. ) ;
#30431 = VERTEX_POINT ( 'NONE', #33678 ) ;
#30432 = CARTESIAN_POINT ( 'NONE',  ( 0.1073791018717578927, 10.69234304549997105, 41.77800844988518492 ) ) ;
#30433 = ORIENTED_EDGE ( 'NONE', *, *, #9688, .T. ) ;
#30434 = DIRECTION ( 'NONE',  ( -0.07500201931887527651, 0.5805833823197910082, -0.8107389427381679337 ) ) ;
#30435 = AXIS2_PLACEMENT_3D ( 'NONE', #52651, #29167, #29784 ) ;
#30436 = CARTESIAN_POINT ( 'NONE',  ( 0.9762797500689124330, -18.09842611962761083, -37.79909730639192844 ) ) ;
#30437 = ORIENTED_EDGE ( 'NONE', *, *, #7129, .F. ) ;
#30438 = DIRECTION ( 'NONE',  ( -1.000000000000000000, -0.000000000000000000, -0.000000000000000000 ) ) ;
#30439 = CARTESIAN_POINT ( 'NONE',  ( 1.227938101723748288, 41.66816631169206886, -10.28900963485336995 ) ) ;
#30440 = ORIENTED_EDGE ( 'NONE', *, *, #60193, .T. ) ;
#30441 = CARTESIAN_POINT ( 'NONE',  ( 5.895881250540457863, -9.661888320803921459, -17.64016994489037415 ) ) ;
#30442 = CARTESIAN_POINT ( 'NONE',  ( 0.8760168074887090262, 44.77533136581856610, 17.58183840866416503 ) ) ;
#30443 = CARTESIAN_POINT ( 'NONE',  ( 0.7762777257811870335, 24.71864134625287335, -41.03453903600409092 ) ) ;
#30444 = ORIENTED_EDGE ( 'NONE', *, *, #42528, .T. ) ;
#30445 = ADVANCED_FACE ( 'NONE', ( #41316 ), #52759, .F. ) ;
#30446 = EDGE_LOOP ( 'NONE', ( #13391, #8308, #44267, #18709 ) ) ;
#30447 = FACE_OUTER_BOUND ( 'NONE', #15580, .T. ) ;
#30448 = ADVANCED_FACE ( 'NONE', ( #1976 ), #7384, .F. ) ;
#30449 =( BOUNDED_SURFACE ( )  B_SPLINE_SURFACE ( 3, 1, ( 
 ( #261, #25028 ),
 ( #39769, #58824 ),
 ( #53506, #15945 ),
 ( #52588, #29712 ) ),
 .UNSPECIFIED., .F., .F., .F. ) 
 B_SPLINE_SURFACE_WITH_KNOTS ( ( 4, 4 ),
 ( 2, 2 ),
 ( 0.000000000000000000, 1.000000000000000000 ),
 ( 0.000000000000000000, 1.000000000000000000 ),
 .UNSPECIFIED. ) 
 GEOMETRIC_REPRESENTATION_ITEM ( )  RATIONAL_B_SPLINE_SURFACE ( (
 ( 1.000000000000000000, 1.000000000000000000),
 ( 0.9953485035131437453, 0.8621029689291515030),
 ( 0.9953485035131437453, 0.8621029689291515030),
 ( 1.000000000000000000, 1.000000000000000000) ) ) 
 REPRESENTATION_ITEM ( '' )  SURFACE ( )  );
#30450 = CARTESIAN_POINT ( 'NONE',  ( 0.8557997880470599172, -47.37054680076701629, -7.156447707086194043 ) ) ;
#30451 = CARTESIAN_POINT ( 'NONE',  ( 4.975801465491694664, 31.15993731089074359, 36.39623109580477234 ) ) ;
#30452 = ORIENTED_EDGE ( 'NONE', *, *, #2337, .T. ) ;
#30453 = CARTESIAN_POINT ( 'NONE',  ( 3.727782113643637096, -43.01752167612853839, -9.070314479100884952 ) ) ;
#30454 = CARTESIAN_POINT ( 'NONE',  ( 0.7242486021783813843, 48.03329165852890981, 10.18893295790429931 ) ) ;
#30455 = EDGE_CURVE ( 'NONE', #33009, #53253, #58994, .T. ) ;
#30456 = CARTESIAN_POINT ( 'NONE',  ( 1.657374760986086049, 8.592625930871594875, -43.20945760900450949 ) ) ;
#30457 = CARTESIAN_POINT ( 'NONE',  ( 0.5806925824938499181, -35.14454992382352572, 31.04968555388990836 ) ) ;
#30458 = ORIENTED_EDGE ( 'NONE', *, *, #46455, .T. ) ;
#30459 = ORIENTED_EDGE ( 'NONE', *, *, #29958, .F. ) ;
#30460 = CARTESIAN_POINT ( 'NONE',  ( 0.1073791018717578927, 16.05399293000759542, 40.02496097243063389 ) ) ;
#30461 = CARTESIAN_POINT ( 'NONE',  ( 0.1102144999581333162, 34.13606714958013555, 26.35238362727852035 ) ) ;
#30462 = CARTESIAN_POINT ( 'NONE',  ( 0.9785694773339264074, 15.26978228898493839, -39.02779976582937849 ) ) ;
#30463 = DIRECTION ( 'NONE',  ( 0.09835009131224549395, 0.2500873580884707681, -0.9632152266566397225 ) ) ;
#30464 = LINE ( 'NONE', #21086, #18610 ) ;
#30465 = DIRECTION ( 'NONE',  ( 0.000000000000000000, 0.000000000000000000, 1.000000000000000000 ) ) ;
#30466 = CARTESIAN_POINT ( 'NONE',  ( 2.879087469061463178, -14.16979277963087647, -41.65715604029755070 ) ) ;
#30467 = CARTESIAN_POINT ( 'NONE',  ( 3.270143674763207553, 11.02405647745170114, 8.113405361969549645 ) ) ;
#30468 = EDGE_CURVE ( 'NONE', #44808, #59478, #27593, .T. ) ;
#30469 = CARTESIAN_POINT ( 'NONE',  ( 0.1064266379913938187, -6.185137063632724974, -42.67882137217588934 ) ) ;
#30470 = CARTESIAN_POINT ( 'NONE',  ( 4.335381028904201628, 34.47659336712107603, -34.80116890942784380 ) ) ;
#30471 = AXIS2_PLACEMENT_3D ( 'NONE', #10557, #29653, #5821 ) ;
#30472 = DIRECTION ( 'NONE',  ( 0.9848077530122080203, 0.1736481776669314692, -5.551115123125783935E-17 ) ) ;
#30473 = CARTESIAN_POINT ( 'NONE',  ( 0.5804410086790514622, 32.99440095573996246, 33.33000686209444297 ) ) ;
#30474 = CARTESIAN_POINT ( 'NONE',  ( 0.5988103564986355654, 5.677495323490723500, -47.77151399983770830 ) ) ;
#30475 = VECTOR ( 'NONE', #19149, 1000.000000000000000 ) ;
#30476 = CARTESIAN_POINT ( 'NONE',  ( 5.959547316686252039, 20.34955788964373014, 2.682663672454983050 ) ) ;
#30477 = CARTESIAN_POINT ( 'NONE',  ( 4.956445790443988031, 0.000000000000000000, 0.000000000000000000 ) ) ;
#30478 = CARTESIAN_POINT ( 'NONE',  ( 4.958415959904823644, -38.82150677285534357, 23.58165739950832318 ) ) ;
#30479 = CARTESIAN_POINT ( 'NONE',  ( 0.9784957157296353403, -22.35374192235875412, 35.44916471598384788 ) ) ;
#30480 = EDGE_CURVE ( 'NONE', #59613, #6804, #47797, .T. ) ;
#30481 = CARTESIAN_POINT ( 'NONE',  ( -6.077587904424778920, -4.278847002849283321, 18.77465018902185179 ) ) ;
#30482 = CARTESIAN_POINT ( 'NONE',  ( 0.5848930533535030563, 46.45334699384589072, 6.431145734385690815 ) ) ;
#30483 = CARTESIAN_POINT ( 'NONE',  ( 0.5997462898726536595, 48.09935696025624452, 9.899671214447447909 ) ) ;
#30485 = ORIENTED_EDGE ( 'NONE', *, *, #44117, .F. ) ;
#30484 = CARTESIAN_POINT ( 'NONE',  ( 0.5848930533535030563, -41.77346544155627583, -21.31315714272907869 ) ) ;
#30486 = VERTEX_POINT ( 'NONE', #5736 ) ;
#30487 = CARTESIAN_POINT ( 'NONE',  ( 0.6028777368367060907, 17.04167399223566548, -46.05563132618456734 ) ) ;
#30488 = CARTESIAN_POINT ( 'NONE',  ( 0.6252788684277217346, 49.04477175441831349, 2.460628929903515782 ) ) ;
#30489 = CARTESIAN_POINT ( 'NONE',  ( -2.569797478183783568, 10.65947181927825582, 10.02484965418644869 ) ) ;
#30490 = ORIENTED_EDGE ( 'NONE', *, *, #7328, .F. ) ;
#30491 = EDGE_CURVE ( 'NONE', #37326, #18589, #55990, .T. ) ;
#30492 = VERTEX_POINT ( 'NONE', #40247 ) ;
#30493 = CARTESIAN_POINT ( 'NONE',  ( -2.569797478183783568, 12.89088113963426352, 6.924386868080891766 ) ) ;
#30494 = CARTESIAN_POINT ( 'NONE',  ( 0.8760168074887076939, 33.37827814204125332, -34.63873394077453582 ) ) ;
#30495 = DIRECTION ( 'NONE',  ( 0.000000000000000000, 0.000000000000000000, 1.000000000000000000 ) ) ;
#30496 = ORIENTED_EDGE ( 'NONE', *, *, #45068, .F. ) ;
#30497 = CIRCLE ( 'NONE', #25497, 48.91267123290010943 ) ;
#30498 = EDGE_LOOP ( 'NONE', ( #6362, #38834, #52892, #51001 ) ) ;
#30499 = DIRECTION ( 'NONE',  ( 0.000000000000000000, 0.000000000000000000, 1.000000000000000000 ) ) ;
#30500 = CARTESIAN_POINT ( 'NONE',  ( 0.9730545539215883499, 39.83279466599061891, -15.95224156741785393 ) ) ;
#30501 = CARTESIAN_POINT ( 'NONE',  ( -6.078726893082806448, -18.27395335922926378, 6.070969436048390122 ) ) ;
#30502 = ORIENTED_EDGE ( 'NONE', *, *, #14362, .T. ) ;
#30503 = CARTESIAN_POINT ( 'NONE',  ( 0.8557997880470690211, 5.347802024197924275, -47.60865952216993691 ) ) ;
#30504 = B_SPLINE_CURVE_WITH_KNOTS ( 'NONE', 3,
 ( #19572, #39303, #1054, #53970, #48989, #24570 ),
 .UNSPECIFIED., .F., .F.,
 ( 4, 2, 4 ),
 ( 1.219794421808126673E-16, 0.0002448718616795938011, 0.0004897437233590656294 ),
 .UNSPECIFIED. ) ;
#30505 = CARTESIAN_POINT ( 'NONE',  ( 0.000000000000000000, 0.6959691356230525150, -1.199999999999999956 ) ) ;
#30506 = AXIS2_PLACEMENT_3D ( 'NONE', #7788, #27521, #3084 ) ;
#30507 = CARTESIAN_POINT ( 'NONE',  ( 0.7245667037590743931, -24.75815201345817584, -41.24129124474288233 ) ) ;
#30508 = ORIENTED_EDGE ( 'NONE', *, *, #9688, .F. ) ;
#30509 = EDGE_LOOP ( 'NONE', ( #21736, #16545, #28158, #14155 ) ) ;
#30510 = CARTESIAN_POINT ( 'NONE',  ( 1.000433927950261648, -30.63672940459725780, 28.59736856849475828 ) ) ;
#30511 = CARTESIAN_POINT ( 'NONE',  ( 4.322998006666165516, -35.39923696759034044, 32.40067585697738650 ) ) ;
#30512 = AXIS2_PLACEMENT_3D ( 'NONE', #6839, #21901, #20972 ) ;
#30513 = VERTEX_POINT ( 'NONE', #25182 ) ;
#30514 = LINE ( 'NONE', #49324, #51494 ) ;
#30515 = CARTESIAN_POINT ( 'NONE',  ( 1.827119703190779765, -42.82501615430328457, -4.394694966566333960 ) ) ;
#30516 = CARTESIAN_POINT ( 'NONE',  ( 0.8744876279028263033, 46.86690837902584406, -14.62336997314537790 ) ) ;
#30517 = CARTESIAN_POINT ( 'NONE',  ( 4.962356264823608143, 41.96072444189411499, 3.245489512196318316 ) ) ;
#30518 = EDGE_CURVE ( 'NONE', #2003, #44145, #30579, .T. ) ;
#30519 = VECTOR ( 'NONE', #27445, 1000.000000000000000 ) ;
#30520 = EDGE_LOOP ( 'NONE', ( #38895, #45132, #25354, #5161 ) ) ;
#30521 = CARTESIAN_POINT ( 'NONE',  ( 0.9756950546413942771, -30.40918718457318803, -30.27237962848467490 ) ) ;
#30522 = AXIS2_PLACEMENT_3D ( 'NONE', #38404, #43414, #46036 ) ;
#30523 = CARTESIAN_POINT ( 'NONE',  ( 0.9754292580325136797, 32.52564057721537694, 26.42745110573104483 ) ) ;
#30524 = ADVANCED_FACE ( 'NONE', ( #20195 ), #21878, .F. ) ;
#30525 = CARTESIAN_POINT ( 'NONE',  ( 4.999999999999998224, -2.650000000000271250, 80.00000000000000000 ) ) ;
#30526 = ORIENTED_EDGE ( 'NONE', *, *, #57454, .T. ) ;
#30527 = CARTESIAN_POINT ( 'NONE',  ( 5.960221823109900008, -19.82478916873578001, 5.317678907195093174 ) ) ;
#30528 = CARTESIAN_POINT ( 'NONE',  ( 0.8751705887134423323, -37.60752970653809513, -29.98056538504947710 ) ) ;
#30530 = VERTEX_POINT ( 'NONE', #48681 ) ;
#30529 = EDGE_CURVE ( 'NONE', #52958, #46743, #2161, .T. ) ;
#30531 = CARTESIAN_POINT ( 'NONE',  ( 0.7242003506640004584, -48.58741756788937494, 7.090453314815819752 ) ) ;
#30532 =( LENGTH_UNIT ( ) NAMED_UNIT ( * ) SI_UNIT ( .MILLI., .METRE. ) );
#30533 =( BOUNDED_SURFACE ( )  B_SPLINE_SURFACE ( 3, 1, ( 
 ( #4538, #10198 ),
 ( #18678, #9260 ),
 ( #23674, #30511 ),
 ( #40278, #34942 ) ),
 .UNSPECIFIED., .F., .F., .F. ) 
 B_SPLINE_SURFACE_WITH_KNOTS ( ( 4, 4 ),
 ( 2, 2 ),
 ( 0.000000000000000000, 1.000000000000000000 ),
 ( 0.000000000000000000, 1.000000000000000000 ),
 .UNSPECIFIED. ) 
 GEOMETRIC_REPRESENTATION_ITEM ( )  RATIONAL_B_SPLINE_SURFACE ( (
 ( 1.000000000000000000, 1.000000000000000000),
 ( 0.7223157951917480446, 0.9931996967497186413),
 ( 0.7223157951917480446, 0.9931996967497186413),
 ( 1.000000000000000000, 1.000000000000000000) ) ) 
 REPRESENTATION_ITEM ( '' )  SURFACE ( )  );
#30534 = EDGE_CURVE ( 'NONE', #19553, #2469, #5154, .T. ) ;
#30535 = ORIENTED_EDGE ( 'NONE', *, *, #32108, .T. ) ;
#30536 = DIRECTION ( 'NONE',  ( -1.000000000000000000, -3.135800716341489291E-16, 1.298891185607901956E-16 ) ) ;
#30537 = EDGE_CURVE ( 'NONE', #29428, #40414, #2203, .T. ) ;
#30538 = DIRECTION ( 'NONE',  ( 0.000000000000000000, 0.000000000000000000, 1.000000000000000000 ) ) ;
#30539 = CARTESIAN_POINT ( 'NONE',  ( 2.500000000000000000, 1.178949249685212974, -2.042000000000001148 ) ) ;
#30540 = CARTESIAN_POINT ( 'NONE',  ( 0.6041374136657475802, 18.57118264377538353, -44.37863742124648780 ) ) ;
#30541 = CARTESIAN_POINT ( 'NONE',  ( 2.009741617377216460, 21.57548988114320920, 38.39273777697718515 ) ) ;
#30542 = EDGE_CURVE ( 'NONE', #42725, #6542, #44621, .T. ) ;
#30543 = CARTESIAN_POINT ( 'NONE',  ( 0.9730545539215883499, -15.95224156741799426, -39.83279466599056917 ) ) ;
#30544 = DIRECTION ( 'NONE',  ( 0.000000000000000000, 0.000000000000000000, 1.000000000000000000 ) ) ;
#30545 = CARTESIAN_POINT ( 'NONE',  ( 0.5549461598389365813, -32.28688909427809506, -30.04620588494645261 ) ) ;
#30546 = CARTESIAN_POINT ( 'NONE',  ( 0.8753041380234524160, -14.82204010568715624, -46.81287702094778780 ) ) ;
#30547 = ADVANCED_FACE ( 'NONE', ( #16104 ), #28625, .F. ) ;
#30548 = DIRECTION ( 'NONE',  ( 0.000000000000000000, 0.000000000000000000, 1.000000000000000000 ) ) ;
#30549 =( BOUNDED_SURFACE ( )  B_SPLINE_SURFACE ( 3, 1, ( 
 ( #41966, #8723 ),
 ( #23446, #61032 ),
 ( #57233, #32240 ),
 ( #18140, #46653 ) ),
 .UNSPECIFIED., .F., .F., .F. ) 
 B_SPLINE_SURFACE_WITH_KNOTS ( ( 4, 4 ),
 ( 2, 2 ),
 ( 0.000000000000000000, 1.000000000000000000 ),
 ( 0.000000000000000000, 1.000000000000000000 ),
 .UNSPECIFIED. ) 
 GEOMETRIC_REPRESENTATION_ITEM ( )  RATIONAL_B_SPLINE_SURFACE ( (
 ( 1.000000000000000000, 1.000000000000000000),
 ( 0.9952954269826590483, 0.8620686068821307169),
 ( 0.9952954269826590483, 0.8620686068821307169),
 ( 1.000000000000000000, 1.000000000000000000) ) ) 
 REPRESENTATION_ITEM ( '' )  SURFACE ( )  );
#30550 = CARTESIAN_POINT ( 'NONE',  ( 0.9790724872846773286, 15.02455757522504420, 39.12285623072784801 ) ) ;
#30551 = ORIENTED_EDGE ( 'NONE', *, *, #37586, .T. ) ;
#30552 = B_SPLINE_CURVE_WITH_KNOTS ( 'NONE', 3,
 ( #50054, #2103, #35667, #45076 ),
 .UNSPECIFIED., .F., .F.,
 ( 4, 4 ),
 ( 0.000000000000000000, 0.005014147105413693448 ),
 .UNSPECIFIED. ) ;
#30554 = CARTESIAN_POINT ( 'NONE',  ( 4.975801465491694664, 35.64402118370912120, 32.01766832630325155 ) ) ;
#30553 =( BOUNDED_SURFACE ( )  B_SPLINE_SURFACE ( 3, 1, ( 
 ( #59593, #49578 ),
 ( #44302, #58339 ),
 ( #29858, #54568 ),
 ( #15464, #6633 ) ),
 .UNSPECIFIED., .F., .F., .F. ) 
 B_SPLINE_SURFACE_WITH_KNOTS ( ( 4, 4 ),
 ( 2, 2 ),
 ( 0.000000000000000000, 1.000000000000000000 ),
 ( 0.000000000000000000, 1.000000000000000000 ),
 .UNSPECIFIED. ) 
 GEOMETRIC_REPRESENTATION_ITEM ( )  RATIONAL_B_SPLINE_SURFACE ( (
 ( 1.000000000000000000, 1.000000000000000000),
 ( 0.9754377213608244057, 0.9999580625633939235),
 ( 0.9754377213608244057, 0.9999580625633939235),
 ( 1.000000000000000000, 1.000000000000000000) ) ) 
 REPRESENTATION_ITEM ( '' )  SURFACE ( )  );
#30555 = CARTESIAN_POINT ( 'NONE',  ( -5.995132425357893702, 4.885449473615586236, -18.19985213254566858 ) ) ;
#30556 = CARTESIAN_POINT ( 'NONE',  ( 2.648799415243696664, 36.42501529472001920, 32.82888551366023933 ) ) ;
#30557 = CARTESIAN_POINT ( 'NONE',  ( 0.1129192098497447394, 43.99990943031675528, -3.310552508128703497 ) ) ;
#30558 = CARTESIAN_POINT ( 'NONE',  ( -6.078726893082806448, 18.62537590944114640, 4.887679766589625885 ) ) ;
#30559 = CARTESIAN_POINT ( 'NONE',  ( 4.975610109902397937, -36.86873347511098586, -32.14258700041121131 ) ) ;
#30560 = DIRECTION ( 'NONE',  ( -1.000000000000000000, 6.799271724612908544E-15, 1.836909530733817830E-16 ) ) ;
#30561 = CARTESIAN_POINT ( 'NONE',  ( 4.956653778116991482, -8.845409907520609849, -47.27023054223761989 ) ) ;
#30562 = CARTESIAN_POINT ( 'NONE',  ( 0.6023143664670691511, 41.79259346737322289, -23.82663958122392955 ) ) ;
#30563 = CARTESIAN_POINT ( 'NONE',  ( 0.5988103564986355654, -29.76496605343820434, -37.79415694022848271 ) ) ;
#30565 = ORIENTED_EDGE ( 'NONE', *, *, #29256, .F. ) ;
#30564 = CARTESIAN_POINT ( 'NONE',  ( 0.7242003506639987931, 48.34642798422387244, 8.581059100850049859 ) ) ;
#30566 = VERTEX_POINT ( 'NONE', #13259 ) ;
#30567 = CARTESIAN_POINT ( 'NONE',  ( -6.077587904424778920, 0.6110050725292486273, -19.24636833782607681 ) ) ;
#30568 = CIRCLE ( 'NONE', #33588, 72.00000000000002842 ) ;
#30569 = CARTESIAN_POINT ( 'NONE',  ( -6.016489644550737204, 0.004404229198039697445, -18.84320342686341121 ) ) ;
#30570 = CARTESIAN_POINT ( 'NONE',  ( 0.5850706913938533704, 37.88789093229805616, 29.30134895053067368 ) ) ;
#30571 = EDGE_CURVE ( 'NONE', #46482, #41414, #47027, .T. ) ;
#30572 = ORIENTED_EDGE ( 'NONE', *, *, #1369, .T. ) ;
#30573 = CARTESIAN_POINT ( 'NONE',  ( 0.1155031312995260795, -23.01756397718155611, 37.64483206348730704 ) ) ;
#30574 = CARTESIAN_POINT ( 'NONE',  ( 0.6064782688330854210, 32.08784176340432737, 34.20094819424595300 ) ) ;
#30575 = CARTESIAN_POINT ( 'NONE',  ( -6.017396004339686577, -14.94857180792001117, 11.47192209077581460 ) ) ;
#30577 = ADVANCED_FACE ( 'NONE', ( #16718 ), #58607, .F. ) ;
#30576 = VERTEX_POINT ( 'NONE', #27038 ) ;
#30578 = ORIENTED_EDGE ( 'NONE', *, *, #54648, .F. ) ;
#30579 = B_SPLINE_CURVE_WITH_KNOTS ( 'NONE', 3,
 ( #24575, #756, #11101, #20800 ),
 .UNSPECIFIED., .F., .F.,
 ( 4, 4 ),
 ( 5.553824967135426632E-18, 0.004566006591234646368 ),
 .UNSPECIFIED. ) ;
#30580 = CARTESIAN_POINT ( 'NONE',  ( 9.999999999999989342, 85.00000000000001421, 1.040949779275250495E-14 ) ) ;
#30581 = B_SPLINE_CURVE_WITH_KNOTS ( 'NONE', 3,
 ( #21569, #16888, #55065, #55371 ),
 .UNSPECIFIED., .F., .F.,
 ( 4, 4 ),
 ( 6.254634441385502288E-18, 0.004050076154993000749 ),
 .UNSPECIFIED. ) ;
#30582 = DIRECTION ( 'NONE',  ( 0.000000000000000000, 0.000000000000000000, 1.000000000000000000 ) ) ;
#30583 = CARTESIAN_POINT ( 'NONE',  ( 0.6026777506516368677, 37.50538381255011444, 31.70004062632291664 ) ) ;
#30584 = EDGE_LOOP ( 'NONE', ( #35363, #60102, #41669, #22003 ) ) ;
#30585 = EDGE_LOOP ( 'NONE', ( #19388, #61334 ) ) ;
#30586 = CARTESIAN_POINT ( 'NONE',  ( 0.8551540677456834771, 47.90804413217340851, -0.9122407826477434423 ) ) ;
#30587 = ORIENTED_EDGE ( 'NONE', *, *, #19699, .T. ) ;
#30588 = CARTESIAN_POINT ( 'NONE',  ( -6.078726893082806448, -11.01388439747492498, -15.79520154185373038 ) ) ;
#30589 = DIRECTION ( 'NONE',  ( 1.000000000000000000, 0.000000000000000000, 0.000000000000000000 ) ) ;
#30590 = VERTEX_POINT ( 'NONE', #35838 ) ;
#30591 = CARTESIAN_POINT ( 'NONE',  ( 1.091591847532194626, 4.971042726581281990, -41.61787747070175669 ) ) ;
#30592 = CARTESIAN_POINT ( 'NONE',  ( 0.7056759521544974101, -46.84549373964249952, 2.290970407077026483 ) ) ;
#30593 = ORIENTED_EDGE ( 'NONE', *, *, #18369, .F. ) ;
#30594 = FACE_OUTER_BOUND ( 'NONE', #2466, .T. ) ;
#30595 = CARTESIAN_POINT ( 'NONE',  ( 0.7242486021783826056, 11.72324082283336644, -47.68204155637450015 ) ) ;
#30596 = LINE ( 'NONE', #25915, #35748 ) ;
#30597 = CARTESIAN_POINT ( 'NONE',  ( 2.624215991343620935, 43.79392271049097474, -19.66774719432931562 ) ) ;
#30598 = EDGE_CURVE ( 'NONE', #5485, #29821, #55201, .T. ) ;
#30599 = VERTEX_POINT ( 'NONE', #6973 ) ;
#30600 = CARTESIAN_POINT ( 'NONE',  ( 0.6041374136657476912, 44.37863742124666544, -18.57118264377493588 ) ) ;
#30601 = DIRECTION ( 'NONE',  ( 0.000000000000000000, 0.000000000000000000, 1.000000000000000000 ) ) ;
#30602 = EDGE_CURVE ( 'NONE', #61648, #25122, #26229, .T. ) ;
#30603 = ORIENTED_EDGE ( 'NONE', *, *, #34879, .F. ) ;
#30604 = CARTESIAN_POINT ( 'NONE',  ( 5.895596859100789899, -7.225383168024946734, -18.77024297359278293 ) ) ;
#30605 = ORIENTED_EDGE ( 'NONE', *, *, #56286, .T. ) ;
#30606 = CARTESIAN_POINT ( 'NONE',  ( 0.9762797500689124330, 4.697980241568662230, 41.64437257103935508 ) ) ;
#30607 = ORIENTED_EDGE ( 'NONE', *, *, #17420, .F. ) ;
#30608 = CARTESIAN_POINT ( 'NONE',  ( 0.9757954354143116849, 5.207268878499845415E-15, 42.90846090505964128 ) ) ;
#30609 = CARTESIAN_POINT ( 'NONE',  ( 2.624215991343608501, -40.85210347989513480, -25.21574086439748896 ) ) ;
#30610 = EDGE_CURVE ( 'NONE', #59587, #22620, #43298, .T. ) ;
#30611 = CARTESIAN_POINT ( 'NONE',  ( 1.227938101723756947, -30.94118573761292623, -29.74462687941258210 ) ) ;
#30612 = ORIENTED_EDGE ( 'NONE', *, *, #20152, .F. ) ;
#30613 = CARTESIAN_POINT ( 'NONE',  ( 0.3622758884714730732, 15.73321244754854753, -40.13994584881767480 ) ) ;
#30614 = EDGE_CURVE ( 'NONE', #57082, #48917, #41469, .T. ) ;
#30615 = CARTESIAN_POINT ( 'NONE',  ( 5.960721111146673579, -14.51823969584109619, 14.50930005614991813 ) ) ;
#30616 = CARTESIAN_POINT ( 'NONE',  ( 4.975610109902397937, 0.9924324126411095959, -48.90260202733707473 ) ) ;
#30617 = ORIENTED_EDGE ( 'NONE', *, *, #33523, .F. ) ;
#30618 = ORIENTED_EDGE ( 'NONE', *, *, #48931, .F. ) ;
#30619 = CARTESIAN_POINT ( 'NONE',  ( 4.549368137175248350, 42.14271863032833920, -8.166781970325278195 ) ) ;
#30620 = CARTESIAN_POINT ( 'NONE',  ( 0.9762797500689124330, -18.09842611962814019, 37.79909730639167265 ) ) ;
#30621 = CARTESIAN_POINT ( 'NONE',  ( 0.9780303403264796192, 38.45566908893830771, -16.65836511537540332 ) ) ;
#30622 = CARTESIAN_POINT ( 'NONE',  ( 0.1081432562775997697, 30.19275717928080738, 30.79166192943855407 ) ) ;
#30623 = CARTESIAN_POINT ( 'NONE',  ( 0.5848930533535030563, -30.41648929863225703, 35.69468113226040629 ) ) ;
#30624 = DIRECTION ( 'NONE',  ( 0.09835009131224567436, -0.8656670924898649533, 0.4908642831975215115 ) ) ;
#30625 = VERTEX_POINT ( 'NONE', #17035 ) ;
#30626 = AXIS2_PLACEMENT_3D ( 'NONE', #57278, #47606, #47923 ) ;
#30627 = CARTESIAN_POINT ( 'NONE',  ( 1.000110580585051201, -40.93372354294542959, -8.991538226667278977 ) ) ;
#30628 = CARTESIAN_POINT ( 'NONE',  ( 0.8554163680231816613, -14.77070554666818758, -44.53124443315552128 ) ) ;
#30629 = VERTEX_POINT ( 'NONE', #22037 ) ;
#30630 = CARTESIAN_POINT ( 'NONE',  ( 0.9762797500689124330, -31.41867615533404390, 27.73430319715907544 ) ) ;
#30631 = CARTESIAN_POINT ( 'NONE',  ( 0.5997462898726536595, 44.01516392039482639, 21.77652348757905898 ) ) ;
#30632 = CARTESIAN_POINT ( 'NONE',  ( 0.3676999524040323597, -38.02468164711575582, -22.36233818182566324 ) ) ;
#30633 = B_SPLINE_CURVE_WITH_KNOTS ( 'NONE', 3,
 ( #47992, #38602, #48592, #14788, #57349, #29793 ),
 .UNSPECIFIED., .F., .F.,
 ( 4, 2, 4 ),
 ( 4.445228907190568179E-18, 0.0002447193893791691660, 0.0004894387787583338867 ),
 .UNSPECIFIED. ) ;
#30634 = FACE_OUTER_BOUND ( 'NONE', #21067, .T. ) ;
#30635 = CARTESIAN_POINT ( 'NONE',  ( 5.838029081930957709, -40.65053383315965618, -24.05408816047831877 ) ) ;
#30636 = CARTESIAN_POINT ( 'NONE',  ( 0.5782707292762442330, 32.08118243869992625, 34.21306895095013800 ) ) ;
#30637 =( BOUNDED_SURFACE ( )  B_SPLINE_SURFACE ( 3, 1, ( 
 ( #21249, #44770 ),
 ( #49436, #21558 ),
 ( #6491, #25632 ),
 ( #40381, #1812 ) ),
 .UNSPECIFIED., .F., .F., .F. ) 
 B_SPLINE_SURFACE_WITH_KNOTS ( ( 4, 4 ),
 ( 2, 2 ),
 ( 0.000000000000000000, 1.000000000000000000 ),
 ( 0.000000000000000000, 1.000000000000000000 ),
 .UNSPECIFIED. ) 
 GEOMETRIC_REPRESENTATION_ITEM ( )  RATIONAL_B_SPLINE_SURFACE ( (
 ( 1.000000000000000000, 1.000000000000000000),
 ( 0.9953040768229013402, 0.8617119497784988535),
 ( 0.9953040768229013402, 0.8617119497784988535),
 ( 1.000000000000000000, 1.000000000000000000) ) ) 
 REPRESENTATION_ITEM ( '' )  SURFACE ( )  );
#30638 = B_SPLINE_CURVE_WITH_KNOTS ( 'NONE', 3,
 ( #61386, #48245, #61689, #47626 ),
 .UNSPECIFIED., .F., .F.,
 ( 4, 4 ),
 ( 7.589415207398531038E-19, 0.004446298630425094510 ),
 .UNSPECIFIED. ) ;
#30639 = CARTESIAN_POINT ( 'NONE',  ( 0.5997462898726536595, 37.05192695178169515, -32.22896739432000146 ) ) ;
#30640 = CARTESIAN_POINT ( 'NONE',  ( 0.8744876279028263033, 3.827863332834932297, 48.94586308039354350 ) ) ;
#30641 = PLANE ( 'NONE',  #38876 ) ;
#30642 = CARTESIAN_POINT ( 'NONE',  ( 2.500000000000002220, 0.000000000000000000, -5.600000000000000533 ) ) ;
#30643 = CARTESIAN_POINT ( 'NONE',  ( 1.112077966505212068, -21.94633083862179035, 38.22811645700467409 ) ) ;
#30644 = DIRECTION ( 'NONE',  ( 0.000000000000000000, 0.000000000000000000, -1.000000000000000000 ) ) ;
#30645 = DIRECTION ( 'NONE',  ( 0.000000000000000000, 0.000000000000000000, 1.000000000000000000 ) ) ;
#30646 = B_SPLINE_CURVE_WITH_KNOTS ( 'NONE', 3,
 ( #1305, #1009, #25435, #30752 ),
 .UNSPECIFIED., .F., .F.,
 ( 4, 4 ),
 ( 0.000000000000000000, 0.005004741218457424076 ),
 .UNSPECIFIED. ) ;
#30647 = B_SPLINE_CURVE_WITH_KNOTS ( 'NONE', 3,
 ( #54150, #29745, #25983, #2145 ),
 .UNSPECIFIED., .F., .F.,
 ( 4, 4 ),
 ( 0.000000000000000000, 0.005013413432710150247 ),
 .UNSPECIFIED. ) ;
#30648 =( BOUNDED_SURFACE ( )  B_SPLINE_SURFACE ( 3, 1, ( 
 ( #34034, #53105 ),
 ( #10210, #24932 ),
 ( #1097, #13451 ),
 ( #10516, #29610 ) ),
 .UNSPECIFIED., .F., .F., .F. ) 
 B_SPLINE_SURFACE_WITH_KNOTS ( ( 4, 4 ),
 ( 2, 2 ),
 ( 0.000000000000000000, 1.000000000000000000 ),
 ( 0.000000000000000000, 1.000000000000000000 ),
 .UNSPECIFIED. ) 
 GEOMETRIC_REPRESENTATION_ITEM ( )  RATIONAL_B_SPLINE_SURFACE ( (
 ( 1.000000000000000000, 1.000000000000000000),
 ( 0.7269869731126817891, 0.9931720237060910339),
 ( 0.7269869731126817891, 0.9931720237060910339),
 ( 1.000000000000000000, 1.000000000000000000) ) ) 
 REPRESENTATION_ITEM ( '' )  SURFACE ( )  );
#30649 = EDGE_CURVE ( 'NONE', #53648, #30599, #7374, .T. ) ;
#30650 = ORIENTED_EDGE ( 'NONE', *, *, #55935, .F. ) ;
#30651 = AXIS2_PLACEMENT_3D ( 'NONE', #58125, #16168, #34655 ) ;
#30652 = DIRECTION ( 'NONE',  ( -1.000000000000000000, -0.000000000000000000, -0.000000000000000000 ) ) ;
#30653 = CARTESIAN_POINT ( 'NONE',  ( 0.1084644655670281843, 43.12277244437005663, -0.3976617192053908401 ) ) ;
#30654 = MECHANICAL_DESIGN_GEOMETRIC_PRESENTATION_REPRESENTATION (  '', ( #49663 ), #11673 ) ;
#30655 = FACE_OUTER_BOUND ( 'NONE', #1160, .T. ) ;
#30656 = CARTESIAN_POINT ( 'NONE',  ( 4.962356264823603702, 37.36413190407388640, -19.36897635181878030 ) ) ;
#30657 = CARTESIAN_POINT ( 'NONE',  ( 0.1104177457020373287, -41.65375561851293185, 11.16615714989236707 ) ) ;
#30658 = CONICAL_SURFACE ( 'NONE', #17662, 42.92674063221959813, 1.485477209440487556 ) ;
#30659 = ORIENTED_EDGE ( 'NONE', *, *, #31410, .F. ) ;
#30660 = CARTESIAN_POINT ( 'NONE',  ( 0.3676999524040366896, -32.25712563511761743, -30.09033780274121739 ) ) ;
#30661 = DIRECTION ( 'NONE',  ( 1.850371707708593823E-16, -1.000000000000000000, 0.000000000000000000 ) ) ;
#30662 = CARTESIAN_POINT ( 'NONE',  ( 0.6016117650947689910, -13.63814917008489580, 47.17575586526422882 ) ) ;
#30663 = VERTEX_POINT ( 'NONE', #17641 ) ;
#30664 = CARTESIAN_POINT ( 'NONE',  ( 3.559346040607745287, -43.92278903503267884, 2.053992435721407439 ) ) ;
#30665 = CARTESIAN_POINT ( 'NONE',  ( 0.2279481005628809787, -0.6549591441850819429, -44.11433458177015865 ) ) ;
#30666 = ORIENTED_EDGE ( 'NONE', *, *, #53614, .F. ) ;
#30667 = VECTOR ( 'NONE', #10472, 1000.000000000000000 ) ;
#30668 = CARTESIAN_POINT ( 'NONE',  ( 4.303969348037258058, -2.158280495709878455, -48.06163817123227489 ) ) ;
#30669 = FACE_OUTER_BOUND ( 'NONE', #37719, .T. ) ;
#30670 = B_SPLINE_CURVE_WITH_KNOTS ( 'NONE', 3,
 ( #49497, #15697, #6241, #48885, #34803, #44530 ),
 .UNSPECIFIED., .F., .F.,
 ( 4, 2, 4 ),
 ( 7.896833245746192927E-18, 0.0002445244328975387576, 0.0004890488657950696006 ),
 .UNSPECIFIED. ) ;
#30671 = ORIENTED_EDGE ( 'NONE', *, *, #10418, .T. ) ;
#30672 = CARTESIAN_POINT ( 'NONE',  ( 0.8751705887134553219, -47.79200036674276220, -5.393078191592532988 ) ) ;
#30673 = EDGE_LOOP ( 'NONE', ( #23296, #15475, #47401, #27746 ) ) ;
#30674 = CARTESIAN_POINT ( 'NONE',  ( 0.9754292580325137907, 35.75786466006411501, 21.85640825608229321 ) ) ;
#30675 = CARTESIAN_POINT ( 'NONE',  ( 0.1100247026804066219, -26.11768802553221391, -34.31594964380173707 ) ) ;
#30676 = ORIENTED_EDGE ( 'NONE', *, *, #16729, .T. ) ;
#30677 = CIRCLE ( 'NONE', #43732, 49.35315702047511621 ) ;
#30678 = ORIENTED_EDGE ( 'NONE', *, *, #32454, .F. ) ;
#30679 = CARTESIAN_POINT ( 'NONE',  ( 0.9787284016396600173, 19.97613726806151746, -36.84141607995537981 ) ) ;
#30680 = EDGE_CURVE ( 'NONE', #16352, #34782, #17837, .T. ) ;
#30681 = CARTESIAN_POINT ( 'NONE',  ( 0.5839879882012690704, -37.99844431214147988, -29.15719377327484807 ) ) ;
#30683 = EDGE_CURVE ( 'NONE', #35390, #371, #41054, .T. ) ;
#30682 = EDGE_LOOP ( 'NONE', ( #1242, #54464, #49416, #47409 ) ) ;
#30684 = ORIENTED_EDGE ( 'NONE', *, *, #37010, .F. ) ;
#30685 = CARTESIAN_POINT ( 'NONE',  ( 0.8751705887134553219, 34.63284514348538323, 33.37254303619566542 ) ) ;
#30686 = DIRECTION ( 'NONE',  ( 1.000000000000000000, 1.836909530733573776E-16, 0.000000000000000000 ) ) ;
#30687 = LINE ( 'NONE', #39198, #21452 ) ;
#30688 = CARTESIAN_POINT ( 'NONE',  ( 0.5824936645240084143, 32.86261044185514635, -33.45574709952209957 ) ) ;
#30689 = CARTESIAN_POINT ( 'NONE',  ( 4.960386119450146403, -10.60034705332560101, -42.45078452774922084 ) ) ;
#30690 = EDGE_LOOP ( 'NONE', ( #16276, #47912, #17927, #34954 ) ) ;
#30691 = EDGE_CURVE ( 'NONE', #7624, #22663, #46784, .T. ) ;
#30692 = CARTESIAN_POINT ( 'NONE',  ( -6.016761891674565099, 18.20023637398599092, 4.880293656735028129 ) ) ;
#30693 = FACE_OUTER_BOUND ( 'NONE', #60627, .T. ) ;
#30694 = ORIENTED_EDGE ( 'NONE', *, *, #59250, .T. ) ;
#30695 = CARTESIAN_POINT ( 'NONE',  ( 4.962356264823608143, 0.000000000000000000, 0.000000000000000000 ) ) ;
#30696 = ORIENTED_EDGE ( 'NONE', *, *, #16685, .T. ) ;
#30697 = DIRECTION ( 'NONE',  ( 0.09835009131224567436, -0.8579344853044309493, -0.5042575517176655087 ) ) ;
#30698 = FACE_OUTER_BOUND ( 'NONE', #628, .T. ) ;
#30699 = CARTESIAN_POINT ( 'NONE',  ( 4.303969348037246512, -42.70173985163832953, 22.16169334783822720 ) ) ;
#30700 = VERTEX_POINT ( 'NONE', #19499 ) ;
#30701 = CARTESIAN_POINT ( 'NONE',  ( -4.915099999999998914, 0.000000000000000000, 49.35315702047512332 ) ) ;
#30702 = CARTESIAN_POINT ( 'NONE',  ( 4.975610109902397937, -36.86873347511144772, 32.14258700041067840 ) ) ;
#30703 = CARTESIAN_POINT ( 'NONE',  ( 52.11660573588833500, 12.32154690648379436, -2.106899540995512687 ) ) ;
#30704 = CARTESIAN_POINT ( 'NONE',  ( 0.6017667736363750963, -29.00830848931600769, -38.37782726569680847 ) ) ;
#30705 = VECTOR ( 'NONE', #5606, 1000.000000000000000 ) ;
#30706 = EDGE_CURVE ( 'NONE', #25288, #8559, #49219, .T. ) ;
#30707 = COLOUR_RGB ( '', 0.72549020, 0.75294118, 0.79215686) ;
#30708 = ORIENTED_EDGE ( 'NONE', *, *, #45481, .T. ) ;
#30709 = CARTESIAN_POINT ( 'NONE',  ( -6.015611763856276717, -18.68284711750056815, -2.453375430804263235 ) ) ;
#30710 = EDGE_LOOP ( 'NONE', ( #57481, #43029, #5307, #13915 ) ) ;
#30711 = VECTOR ( 'NONE', #34548, 1000.000000000000114 ) ;
#30712 = EDGE_CURVE ( 'NONE', #6250, #42579, #43260, .T. ) ;
#30713 = CARTESIAN_POINT ( 'NONE',  ( 0.7246131072078545454, 44.12003537001153575, 19.16331062551101994 ) ) ;
#30714 = CARTESIAN_POINT ( 'NONE',  ( 0.9790320750461911636, 41.54611640558821506, -5.500667609982005324 ) ) ;
#30715 = CARTESIAN_POINT ( 'NONE',  ( 0.5980271706414711508, 46.38528005876693072, 16.13861941776375986 ) ) ;
#30716 = ORIENTED_EDGE ( 'NONE', *, *, #9114, .T. ) ;
#30717 = DIRECTION ( 'NONE',  ( -0.000000000000000000, -0.000000000000000000, 1.000000000000000000 ) ) ;
#30718 = LINE ( 'NONE', #46091, #5202 ) ;
#30719 = CARTESIAN_POINT ( 'NONE',  ( 0.8560838555295158248, -24.46533024579895610, -40.02274915652004239 ) ) ;
#30720 = MANIFOLD_SOLID_BREP ( 'Hex', #30040 ) ;
#30721 = CARTESIAN_POINT ( 'NONE',  ( 0.8753041380234465318, 32.34805756193355819, 36.94240787824763572 ) ) ;
#30722 = CARTESIAN_POINT ( 'NONE',  ( 4.303969348037258058, 42.70173985163817321, 22.16169334783852207 ) ) ;
#30723 = B_SPLINE_CURVE_WITH_KNOTS ( 'NONE', 3,
 ( #10225, #9921, #9593, #4879, #43141, #32813 ),
 .UNSPECIFIED., .F., .F.,
 ( 4, 2, 4 ),
 ( 0.000000000000000000, 0.0002291966416970759885, 0.0004583932833941519770 ),
 .UNSPECIFIED. ) ;
#30724 = CARTESIAN_POINT ( 'NONE',  ( 0.1073791018717578927, -0.4849339620936172768, 43.12183934961190346 ) ) ;
#30725 = EDGE_CURVE ( 'NONE', #57516, #27042, #4126, .T. ) ;
#30726 = CIRCLE ( 'NONE', #30866, 47.09074272231896430 ) ;
#30727 = LINE ( 'NONE', #21340, #18293 ) ;
#30728 = CARTESIAN_POINT ( 'NONE',  ( 0.6845945791218023269, -46.85360930762397658, -2.268439014493842443 ) ) ;
#30729 = VERTEX_POINT ( 'NONE', #57666 ) ;
#30730 = CARTESIAN_POINT ( 'NONE',  ( 3.221118495291109163, -3.296306199338291165, -43.86223643525207905 ) ) ;
#30731 = CARTESIAN_POINT ( 'NONE',  ( 0.5809828226811617480, 46.11980934799338883, 12.92184523170220345 ) ) ;
#30732 = FACE_OUTER_BOUND ( 'NONE', #40179, .T. ) ;
#30733 = ORIENTED_EDGE ( 'NONE', *, *, #54100, .T. ) ;
#30734 = CARTESIAN_POINT ( 'NONE',  ( 4.553261556744873317, 35.06776520399894537, -26.45357082552063233 ) ) ;
#30735 = CARTESIAN_POINT ( 'NONE',  ( 3.678834586032785570, 26.48313750915808740, 41.19776446968182171 ) ) ;
#30736 = CARTESIAN_POINT ( 'NONE',  ( 3.270143674763207553, 4.983712007628406937, -12.74832469035447424 ) ) ;
#30737 = ORIENTED_EDGE ( 'NONE', *, *, #173, .F. ) ;
#30738 = DIRECTION ( 'NONE',  ( 0.000000000000000000, 0.000000000000000000, 1.000000000000000000 ) ) ;
#30739 = CARTESIAN_POINT ( 'NONE',  ( 0.8554163680231738898, 43.54276151446884313, -17.47092993535008176 ) ) ;
#30740 = CIRCLE ( 'NONE', #43803, 47.91270532121795611 ) ;
#30741 = ORIENTED_EDGE ( 'NONE', *, *, #48278, .F. ) ;
#30742 = CARTESIAN_POINT ( 'NONE',  ( 0.6016118706126978299, 10.58757829817042229, 47.95262496010037978 ) ) ;
#30743 = AXIS2_PLACEMENT_3D ( 'NONE', #24663, #34088, #56930 ) ;
#30744 = CIRCLE ( 'NONE', #9735, 42.08604991992415023 ) ;
#30745 = VERTEX_POINT ( 'NONE', #57361 ) ;
#30746 = ORIENTED_EDGE ( 'NONE', *, *, #23636, .T. ) ;
#30747 = CARTESIAN_POINT ( 'NONE',  ( 0.1155031312995260795, 44.02238668353053441, 2.995179997516315140 ) ) ;
#30748 = ORIENTED_EDGE ( 'NONE', *, *, #36538, .F. ) ;
#30749 = CARTESIAN_POINT ( 'NONE',  ( 4.549368137175248350, -35.57418903283131328, 24.02461520945210793 ) ) ;
#30750 = CARTESIAN_POINT ( 'NONE',  ( 0.7242486021783861583, 41.59294671404158805, -26.09670948638677501 ) ) ;
#30751 = EDGE_LOOP ( 'NONE', ( #44035, #2219 ) ) ;
#30752 = CARTESIAN_POINT ( 'NONE',  ( 4.956653778116982600, -47.05699031914957686, 9.917440902360995736 ) ) ;
#30753 =( BOUNDED_SURFACE ( )  B_SPLINE_SURFACE ( 3, 1, ( 
 ( #11023, #346 ),
 ( #24172, #58590 ),
 ( #10708, #29800 ),
 ( #38306, #57356 ) ),
 .UNSPECIFIED., .F., .F., .F. ) 
 B_SPLINE_SURFACE_WITH_KNOTS ( ( 4, 4 ),
 ( 2, 2 ),
 ( 0.000000000000000000, 1.000000000000000000 ),
 ( 0.000000000000000000, 1.000000000000000000 ),
 .UNSPECIFIED. ) 
 GEOMETRIC_REPRESENTATION_ITEM ( )  RATIONAL_B_SPLINE_SURFACE ( (
 ( 1.000000000000000000, 1.000000000000000000),
 ( 0.7282232189291694135, 0.9929344683865672927),
 ( 0.7282232189291694135, 0.9929344683865672927),
 ( 1.000000000000000000, 1.000000000000000000) ) ) 
 REPRESENTATION_ITEM ( '' )  SURFACE ( )  );
#30754 = LINE ( 'NONE', #5686, #57964 ) ;
#30755 = ADVANCED_FACE ( 'NONE', ( #47690 ), #9415, .F. ) ;
#30756 = ORIENTED_EDGE ( 'NONE', *, *, #56207, .T. ) ;
#30757 = CARTESIAN_POINT ( 'NONE',  ( 1.830465331921977246, 30.51707817982678606, -31.76608246612618558 ) ) ;
#30758 = CARTESIAN_POINT ( 'NONE',  ( 4.963659409799330291, 42.53037318521015209, -13.93274247731977233 ) ) ;
#30759 = CARTESIAN_POINT ( 'NONE',  ( 0.1073791018717578927, 43.12183934961191056, 0.4849339620934667305 ) ) ;
#30760 = CARTESIAN_POINT ( 'NONE',  ( 0.5807400328401574052, -37.66660715020846339, -29.58941477093054573 ) ) ;
#30761 = VERTEX_POINT ( 'NONE', #53590 ) ;
#30762 = ADVANCED_FACE ( 'NONE', ( #25726 ), #11441, .F. ) ;
#30763 = ORIENTED_EDGE ( 'NONE', *, *, #25764, .F. ) ;
#30764 = AXIS2_PLACEMENT_3D ( 'NONE', #50354, #41297, #16867 ) ;
#30765 = CARTESIAN_POINT ( 'NONE',  ( 0.1097557419366048670, 41.71221507312532850, 10.94578341459284765 ) ) ;
#30766 = CARTESIAN_POINT ( 'NONE',  ( 0.6039202388192952409, 17.12343321804727481, -46.02555537607413783 ) ) ;
#30767 = B_SPLINE_CURVE_WITH_KNOTS ( 'NONE', 3,
 ( #24340, #29043, #53139, #52524, #513, #57206 ),
 .UNSPECIFIED., .F., .F.,
 ( 4, 2, 4 ),
 ( 2.224174099750402646E-17, 0.0002293319059085110925, 0.0004586638118169999046 ),
 .UNSPECIFIED. ) ;
#30768 = CARTESIAN_POINT ( 'NONE',  ( 4.060580049360325461, 12.98590958963613318, -41.98611492492495501 ) ) ;
#30769 = EDGE_LOOP ( 'NONE', ( #47831, #12446, #27965, #7603 ) ) ;
#30770 = CARTESIAN_POINT ( 'NONE',  ( 0.7413678028165009426, -42.88130420167055235, -10.28007012301159584 ) ) ;
#30771 = FACE_OUTER_BOUND ( 'NONE', #11186, .T. ) ;
#30772 = CARTESIAN_POINT ( 'NONE',  ( 0.6253024248130495399, 46.38379508687873454, 16.12413658947630779 ) ) ;
#30773 = CARTESIAN_POINT ( 'NONE',  ( 3.660087539127319545, 42.51124390328632785, 22.37124151181794574 ) ) ;
#30774 = ORIENTED_EDGE ( 'NONE', *, *, #11978, .F. ) ;
#30775 = VERTEX_POINT ( 'NONE', #1282 ) ;
#30776 = CARTESIAN_POINT ( 'NONE',  ( 0.2224561200757568247, 15.79689521915808648, 40.12166550582818303 ) ) ;
#30777 = CARTESIAN_POINT ( 'NONE',  ( 0.7954190325252786797, 28.58653703871157248, -38.68220061605139648 ) ) ;
#30778 = CARTESIAN_POINT ( 'NONE',  ( -6.015611763856276717, 7.205255340944613174, 17.41126425312540249 ) ) ;
#30779 = EDGE_CURVE ( 'NONE', #3481, #18802, #5966, .T. ) ;
#30780 = CARTESIAN_POINT ( 'NONE',  ( 1.154321485836934391, -33.53917069757672209, 26.77578840293023887 ) ) ;
#30781 = CARTESIAN_POINT ( 'NONE',  ( 2.281448460670572498, -30.23587867650730487, -37.24544744441608657 ) ) ;
#30782 = CARTESIAN_POINT ( 'NONE',  ( 3.390910168358336918, -43.32159816751995862, 7.572071628396552789 ) ) ;
#30783 = CARTESIAN_POINT ( 'NONE',  ( 5.958863334805807099, 16.28335246510367540, -12.49619391867165064 ) ) ;
#30784 = DIRECTION ( 'NONE',  ( 0.07836865515943410021, -0.9179910502197358158, -0.3887811538706165138 ) ) ;
#30785 = CARTESIAN_POINT ( 'NONE',  ( 0.6009453534118439633, 12.87216801774545338, -46.35353704332099767 ) ) ;
#30786 = VECTOR ( 'NONE', #53275, 1000.000000000000000 ) ;
#30787 = B_SPLINE_CURVE_WITH_KNOTS ( 'NONE', 3,
 ( #28307, #53330, #24847, #20156, #4470, #23610 ),
 .UNSPECIFIED., .F., .F.,
 ( 4, 2, 4 ),
 ( 1.196425325848827598E-16, 0.0002448718616795920663, 0.0004897437233590645452 ),
 .UNSPECIFIED. ) ;
#30788 = CARTESIAN_POINT ( 'NONE',  ( 0.8744876279028306332, -42.33402326122651971, 24.86323641237049387 ) ) ;
#30789 = CARTESIAN_POINT ( 'NONE',  ( 5.895596859100789899, -13.97974974393952508, -14.46010996878344201 ) ) ;
#30790 = CARTESIAN_POINT ( 'NONE',  ( 0.8751705887134553219, 5.393078191592700854, -47.79200036674274088 ) ) ;
#30791 = CARTESIAN_POINT ( 'NONE',  ( 3.238018933889920792, 4.556392162264638834, 12.59550645394246615 ) ) ;
#30792 = CARTESIAN_POINT ( 'NONE',  ( 1.830465331921977468, -23.88195676858206440, 37.01389194318758058 ) ) ;
#30793 = LINE ( 'NONE', #49914, #61643 ) ;
#30794 = DIRECTION ( 'NONE',  ( 0.09722883295013597105, 0.9783250423059166589, -0.1828296082156304347 ) ) ;
#30795 = CARTESIAN_POINT ( 'NONE',  ( -6.078726893082806448, -4.281536037414130469, 18.77398440472997265 ) ) ;
#30796 = CARTESIAN_POINT ( 'NONE',  ( 0.5987334308729317378, 23.24905889540555037, 43.25556804675779432 ) ) ;
#30797 = CARTESIAN_POINT ( 'NONE',  ( 0.6024113833632039894, 48.15977990201467662, 9.600909794929371799 ) ) ;
#30799 = ORIENTED_EDGE ( 'NONE', *, *, #19734, .F. ) ;
#30798 = CARTESIAN_POINT ( 'NONE',  ( -6.015611763856276717, -18.68284711750060367, 2.453375430804002111 ) ) ;
#30800 = ORIENTED_EDGE ( 'NONE', *, *, #49749, .F. ) ;
#30801 = AXIS2_PLACEMENT_3D ( 'NONE', #49358, #31175, #45001 ) ;
#30802 = CARTESIAN_POINT ( 'NONE',  ( -6.016104459813374383, -18.19977249352307425, -4.882138007282940784 ) ) ;
#30803 = CARTESIAN_POINT ( 'NONE',  ( 4.060580049360325461, 1.911233126685682349, -43.90688877949186519 ) ) ;
#30804 = CARTESIAN_POINT ( 'NONE',  ( 4.975801465491695552, 43.22084481528192157, 20.67815041659156705 ) ) ;
#30805 = EDGE_CURVE ( 'NONE', #56952, #56336, #36275, .T. ) ;
#30806 = ORIENTED_EDGE ( 'NONE', *, *, #51597, .T. ) ;
#30807 = ORIENTED_EDGE ( 'NONE', *, *, #56910, .F. ) ;
#30808 = CARTESIAN_POINT ( 'NONE',  ( 0.000000000000000000, 0.000000000000000000, -5.600000000000000533 ) ) ;
#30809 = CARTESIAN_POINT ( 'NONE',  ( -6.016489644550737204, -13.32727118274447342, 13.32104266208094678 ) ) ;
#30810 = CARTESIAN_POINT ( 'NONE',  ( 0.6031357023905875581, 6.236038527293414013, 47.70157053127531555 ) ) ;
#30811 = CIRCLE ( 'NONE', #41851, 43.92652462719577500 ) ;
#30812 = ADVANCED_FACE ( 'NONE', ( #6579 ), #38295, .F. ) ;
#30813 = EDGE_LOOP ( 'NONE', ( #34944, #19973, #47113, #26138 ) ) ;
#30814 = ORIENTED_EDGE ( 'NONE', *, *, #25454, .F. ) ;
#30815 = DIRECTION ( 'NONE',  ( 1.000000000000000000, 1.836909530733573776E-16, -1.925929944387235579E-32 ) ) ;
#30816 = EDGE_CURVE ( 'NONE', #43576, #44327, #46253, .T. ) ;
#30817 = CIRCLE ( 'NONE', #1787, 48.09070567114147110 ) ;
#30818 = B_SPLINE_CURVE_WITH_KNOTS ( 'NONE', 3,
 ( #61800, #38661, #57716, #38059 ),
 .UNSPECIFIED., .F., .F.,
 ( 4, 4 ),
 ( 0.000000000000000000, 0.004041751736740986471 ),
 .UNSPECIFIED. ) ;
#30819 = CARTESIAN_POINT ( 'NONE',  ( 4.975801465491694664, -39.51822597168476392, -27.09127437476367106 ) ) ;
#30820 = CARTESIAN_POINT ( 'NONE',  ( 0.7948878604505666967, -0.7064023212773177240, 49.09378415908586391 ) ) ;
#30821 = ORIENTED_EDGE ( 'NONE', *, *, #55723, .F. ) ;
#30822 = CARTESIAN_POINT ( 'NONE',  ( 1.600000000000000089, -11.64055411052240352, -1.199999999999999956 ) ) ;
#30823 = CARTESIAN_POINT ( 'NONE',  ( 0.6039202388192952409, 41.25132197622592400, -26.64380130654654621 ) ) ;
#30824 =( BOUNDED_SURFACE ( )  B_SPLINE_SURFACE ( 3, 1, ( 
 ( #27540, #7485 ),
 ( #3104, #46358 ),
 ( #60413, #45438 ),
 ( #41063, #50715 ) ),
 .UNSPECIFIED., .F., .F., .F. ) 
 B_SPLINE_SURFACE_WITH_KNOTS ( ( 4, 4 ),
 ( 2, 2 ),
 ( 0.000000000000000000, 1.000000000000000000 ),
 ( 0.000000000000000000, 1.000000000000000000 ),
 .UNSPECIFIED. ) 
 GEOMETRIC_REPRESENTATION_ITEM ( )  RATIONAL_B_SPLINE_SURFACE ( (
 ( 1.000000000000000000, 1.000000000000000000),
 ( 0.7282232189291693025, 0.9929344683865674037),
 ( 0.7282232189291693025, 0.9929344683865674037),
 ( 1.000000000000000000, 1.000000000000000000) ) ) 
 REPRESENTATION_ITEM ( '' )  SURFACE ( )  );
#30825 = CARTESIAN_POINT ( 'NONE',  ( -1.139999999999998570, 0.000000000000000000, 0.000000000000000000 ) ) ;
#30826 = ORIENTED_EDGE ( 'NONE', *, *, #57273, .F. ) ;
#30827 = EDGE_CURVE ( 'NONE', #868, #22443, #57402, .T. ) ;
#30828 = VECTOR ( 'NONE', #42348, 1000.000000000000114 ) ;
#30829 = ORIENTED_EDGE ( 'NONE', *, *, #50010, .T. ) ;
#30830 = DIRECTION ( 'NONE',  ( 0.000000000000000000, 0.000000000000000000, -1.000000000000000000 ) ) ;
#30831 = CARTESIAN_POINT ( 'NONE',  ( 0.2279481005628812007, -40.60382094950545451, -17.25784492262615544 ) ) ;
#30832 = VECTOR ( 'NONE', #8597, 1000.000000000000000 ) ;
#30833 = ORIENTED_EDGE ( 'NONE', *, *, #38727, .T. ) ;
#30834 = CARTESIAN_POINT ( 'NONE',  ( 4.322998006666179727, 45.75942687572297984, -14.45630056002892161 ) ) ;
#30835 = CARTESIAN_POINT ( 'NONE',  ( 5.960721111146673579, 14.51823969584099672, -14.50930005615001583 ) ) ;
#30836 = CARTESIAN_POINT ( 'NONE',  ( 0.9730545539215883499, 41.31259007387230753, 11.59290486963521971 ) ) ;
#30837 = CARTESIAN_POINT ( 'NONE',  ( 4.060580049360325461, -43.82307209454128127, -3.317536217714249336 ) ) ;
#30838 = EDGE_CURVE ( 'NONE', #16591, #51919, #16273, .T. ) ;
#30839 = VERTEX_POINT ( 'NONE', #15412 ) ;
#30840 = CARTESIAN_POINT ( 'NONE',  ( 2.282803330402972453, 12.16313988363625143, -45.37130079277079631 ) ) ;
#30841 = CARTESIAN_POINT ( 'NONE',  ( 0.6016117650947689910, -35.03314589365777465, 34.41263929195476834 ) ) ;
#30842 = ADVANCED_FACE ( 'NONE', ( #24488 ), #60243, .T. ) ;
#30843 = CARTESIAN_POINT ( 'NONE',  ( 4.956445790444001354, -28.36659270909979114, 37.58822246682706947 ) ) ;
#30844 = EDGE_LOOP ( 'NONE', ( #8015, #4375, #13401, #19956 ) ) ;
#30845 = LINE ( 'NONE', #20536, #11498 ) ;
#30846 = CARTESIAN_POINT ( 'NONE',  ( 0.8560838555295223751, 5.603718208093996012, 46.57221463840868125 ) ) ;
#30847 = DIRECTION ( 'NONE',  ( 0.000000000000000000, 0.000000000000000000, -1.000000000000000000 ) ) ;
#30848 = FACE_OUTER_BOUND ( 'NONE', #14510, .T. ) ;
#30849 = VECTOR ( 'NONE', #41615, 1000.000000000000000 ) ;
#30850 = VERTEX_POINT ( 'NONE', #24803 ) ;
#30851 = CARTESIAN_POINT ( 'NONE',  ( 5.860006189529246790, -26.78264244998070609, -40.11385274514709209 ) ) ;
#30852 = CARTESIAN_POINT ( 'NONE',  ( 0.1097557419366048670, -42.72583172879057400, 5.849988371690356459 ) ) ;
#30853 = CARTESIAN_POINT ( 'NONE',  ( 0.1313383488274134925, -22.11173226734867470, -37.02311703718843461 ) ) ;
#30854 = EDGE_CURVE ( 'NONE', #55598, #24289, #44285, .T. ) ;
#30855 = CARTESIAN_POINT ( 'NONE',  ( 1.227938101723748288, -15.63977281655813023, -39.96870412324352628 ) ) ;
#30857 = CARTESIAN_POINT ( 'NONE',  ( 4.553261556744873317, -36.69060082144796553, 24.15241969627054530 ) ) ;
#30856 = PRESENTATION_LAYER_ASSIGNMENT (  '', '', ( #49872 ) ) ;
#30858 = CARTESIAN_POINT ( 'NONE',  ( 0.9730545539215883499, 42.90536227157002003, -0.5054011016614180507 ) ) ;
#30859 = CARTESIAN_POINT ( 'NONE',  ( 2.500000000000000000, 2.629050547790028946E-15, 2.042000000000000259 ) ) ;
#30860 = CARTESIAN_POINT ( 'NONE',  ( 0.1081432562775997835, -41.54352569227153680, -11.56998286599521286 ) ) ;
#30861 = CARTESIAN_POINT ( 'NONE',  ( 0.5809828226811617480, -34.25055090842177208, 33.48000389720603920 ) ) ;
#30862 = CARTESIAN_POINT ( 'NONE',  ( 0.5838002273316447166, 37.91535410490867264, 29.26514720557031168 ) ) ;
#30863 = CARTESIAN_POINT ( 'NONE',  ( 0.9780106845699476636, 14.76917789809602155, 39.21992644906198677 ) ) ;
#30864 = ORIENTED_EDGE ( 'NONE', *, *, #59252, .F. ) ;
#30865 = B_SPLINE_CURVE_WITH_KNOTS ( 'NONE', 3,
 ( #37766, #38681, #48363, #417, #5423, #56823 ),
 .UNSPECIFIED., .F., .F.,
 ( 4, 2, 4 ),
 ( 6.857096618313869002E-18, 0.0002291472222819941282, 0.0004582944445639813716 ),
 .UNSPECIFIED. ) ;
#30866 = AXIS2_PLACEMENT_3D ( 'NONE', #60076, #27487, #51285 ) ;
#30867 = CARTESIAN_POINT ( 'NONE',  ( -17.42749720829281301, -12.33370093165928516, -2.032379639964776441 ) ) ;
#30868 = FACE_OUTER_BOUND ( 'NONE', #60112, .T. ) ;
#30869 = CARTESIAN_POINT ( 'NONE',  ( 2.500000000000000000, 0.000000000000000000, 0.000000000000000000 ) ) ;
#30870 = DIRECTION ( 'NONE',  ( 0.000000000000000000, -0.7071067811865487940, 0.7071067811865461294 ) ) ;
#30871 = CARTESIAN_POINT ( 'NONE',  ( 0.5998501479064699549, -28.86886762351154090, 38.48283596221978797 ) ) ;
#30872 = CARTESIAN_POINT ( 'NONE',  ( 0.9762797500689124330, -30.73989051779348003, 28.48480149377514437 ) ) ;
#30873 = CARTESIAN_POINT ( 'NONE',  ( 3.999999999999990674, -2.309401076758548221, -0.3572655899081733644 ) ) ;
#30874 = CARTESIAN_POINT ( 'NONE',  ( 0.9790850452238877288, -6.920706823809607222, 41.33329344876927536 ) ) ;
#30875 = VECTOR ( 'NONE', #1590, 999.9999999999998863 ) ;
#30876 = CARTESIAN_POINT ( 'NONE',  ( 0.9775691876210963471, 29.40491633870845334, -29.86108846146687767 ) ) ;
#30877 = EDGE_CURVE ( 'NONE', #8147, #15568, #44251, .T. ) ;
#30879 = ORIENTED_EDGE ( 'NONE', *, *, #46935, .F. ) ;
#30878 = CARTESIAN_POINT ( 'NONE',  ( 0.6252788684277199582, -45.25543936479831331, 19.06277889167080275 ) ) ;
#30880 = ORIENTED_EDGE ( 'NONE', *, *, #56895, .T. ) ;
#30881 = CARTESIAN_POINT ( 'NONE',  ( 0.8551540677456834771, -41.03346287276445992, 24.74404575822760677 ) ) ;
#30882 = AXIS2_PLACEMENT_3D ( 'NONE', #26450, #36493, #60260 ) ;
#30883 = CARTESIAN_POINT ( 'NONE',  ( 0.8751705887134423323, -7.160166390004656378, 47.55935879196458416 ) ) ;
#30884 = DIRECTION ( 'NONE',  ( 0.000000000000000000, 0.000000000000000000, -1.000000000000000000 ) ) ;
#30885 = EDGE_CURVE ( 'NONE', #31776, #31779, #13281, .T. ) ;
#30886 = VERTEX_POINT ( 'NONE', #44556 ) ;
#30887 = FACE_OUTER_BOUND ( 'NONE', #26063, .T. ) ;
#30888 = CARTESIAN_POINT ( 'NONE',  ( 5.960721111146673579, -18.96073515164543011, -7.860635756377828187 ) ) ;
#30889 = CARTESIAN_POINT ( 'NONE',  ( 0.1095718737110177449, 41.72082389913616396, -10.91304379105019073 ) ) ;
#30890 = ADVANCED_FACE ( 'NONE', ( #58919 ), #247, .F. ) ;
#30891 = B_SPLINE_CURVE_WITH_KNOTS ( 'NONE', 3,
 ( #40997, #25936, #31877, #45074, #11862, #7106 ),
 .UNSPECIFIED., .F., .F.,
 ( 4, 2, 4 ),
 ( 1.252987389397349539E-17, 0.0002293755540694274696, 0.0004587511081388424166 ),
 .UNSPECIFIED. ) ;
#30892 = ORIENTED_EDGE ( 'NONE', *, *, #41949, .F. ) ;
#30893 = ORIENTED_EDGE ( 'NONE', *, *, #51253, .F. ) ;
#30894 = CARTESIAN_POINT ( 'NONE',  ( 0.8744876279028306332, 46.86690837902563089, 14.62336997314605469 ) ) ;
#30895 = EDGE_CURVE ( 'NONE', #23672, #25014, #3144, .T. ) ;
#30896 = EDGE_CURVE ( 'NONE', #8175, #22775, #6902, .T. ) ;
#30897 = AXIS2_PLACEMENT_3D ( 'NONE', #5196, #14954, #53126 ) ;
#30898 = CARTESIAN_POINT ( 'NONE',  ( 0.1087620492084204749, -39.70193592734194254, -16.83695155255820097 ) ) ;
#30899 = FACE_OUTER_BOUND ( 'NONE', #20832, .T. ) ;
#30900 = ORIENTED_EDGE ( 'NONE', *, *, #19339, .T. ) ;
#30901 = VERTEX_POINT ( 'NONE', #26652 ) ;
#30902 = CARTESIAN_POINT ( 'NONE',  ( 0.1103936448916694457, -6.269440624735986453E-17, 43.12443171339902648 ) ) ;
#30903 = CARTESIAN_POINT ( 'NONE',  ( 5.895596859100789899, 10.82540956478682581, -16.95106754653256331 ) ) ;
#30904 = ORIENTED_EDGE ( 'NONE', *, *, #29634, .T. ) ;
#30905 = AXIS2_PLACEMENT_3D ( 'NONE', #51910, #29039, #37853 ) ;
#30906 = CARTESIAN_POINT ( 'NONE',  ( 4.975610109902397937, -28.45381238669816426, 39.78479568629648355 ) ) ;
#30907 = LINE ( 'NONE', #45042, #61936 ) ;
#30908 = ORIENTED_EDGE ( 'NONE', *, *, #47782, .T. ) ;
#30909 = EDGE_CURVE ( 'NONE', #8473, #23453, #55237, .T. ) ;
#30910 =( BOUNDED_SURFACE ( )  B_SPLINE_SURFACE ( 3, 1, ( 
 ( #58916, #26647 ),
 ( #6898, #26039 ),
 ( #31355, #16967 ),
 ( #54199, #36080 ) ),
 .UNSPECIFIED., .F., .F., .F. ) 
 B_SPLINE_SURFACE_WITH_KNOTS ( ( 4, 4 ),
 ( 2, 2 ),
 ( 0.000000000000000000, 1.000000000000000000 ),
 ( 0.000000000000000000, 1.000000000000000000 ),
 .UNSPECIFIED. ) 
 GEOMETRIC_REPRESENTATION_ITEM ( )  RATIONAL_B_SPLINE_SURFACE ( (
 ( 1.000000000000000000, 1.000000000000000000),
 ( 0.9729067724841187204, 0.9999501103223794596),
 ( 0.9729067724841187204, 0.9999501103223794596),
 ( 1.000000000000000000, 1.000000000000000000) ) ) 
 REPRESENTATION_ITEM ( '' )  SURFACE ( )  );
#30911 = CARTESIAN_POINT ( 'NONE',  ( 0.8744876279028306332, -20.68330519280286239, -44.52584571550401193 ) ) ;
#30912 = CARTESIAN_POINT ( 'NONE',  ( -6.078726893082806448, 15.42998809551244577, -11.51996131248123234 ) ) ;
#30913 = B_SPLINE_CURVE_WITH_KNOTS ( 'NONE', 3,
 ( #19602, #28676, #57776, #33706, #9564, #43420, #29290, #10193, #48101, #19922, #34316, #43110, #14911, #18996, #28364, #23671 ),
 .UNSPECIFIED., .F., .F.,
 ( 4, 3, 3, 3, 3, 4 ),
 ( 9.813676791237319219E-18, 0.0002724568934985577154, 0.0004086836638483823695, 0.0005449104342063580556, 0.0008173270854453611439, 0.001089761613562687491 ),
 .UNSPECIFIED. ) ;
#30914 = ORIENTED_EDGE ( 'NONE', *, *, #47344, .T. ) ;
#30915 = FACE_BOUND ( 'NONE', #55013, .T. ) ;
#30916 = EDGE_CURVE ( 'NONE', #35841, #24101, #51063, .T. ) ;
#30917 = CARTESIAN_POINT ( 'NONE',  ( 5.965394784446460541, 12.50653125159007395, -16.27505370423068598 ) ) ;
#30918 = CARTESIAN_POINT ( 'NONE',  ( 0.8744876279028306332, 48.35212675551500183, 8.510105087371359289 ) ) ;
#30919 = CARTESIAN_POINT ( 'NONE',  ( 4.975610109902397937, -41.30423662854469313, 26.19941685746003301 ) ) ;
#30920 = ORIENTED_EDGE ( 'NONE', *, *, #40202, .T. ) ;
#30921 = DIRECTION ( 'NONE',  ( -1.000000000000000000, 0.000000000000000000, 0.000000000000000000 ) ) ;
#30922 = DIRECTION ( 'NONE',  ( 0.000000000000000000, 0.000000000000000000, 1.000000000000000000 ) ) ;
#30923 = EDGE_LOOP ( 'NONE', ( #38034, #4298, #20498, #36712 ) ) ;
#30924 = EDGE_CURVE ( 'NONE', #55224, #6250, #28246, .T. ) ;
#30925 = CARTESIAN_POINT ( 'NONE',  ( 0.1310142868023686513, -30.94009702668495265, 30.03916697317163198 ) ) ;
#30926 = CIRCLE ( 'NONE', #17084, 47.09074272231896430 ) ;
#30927 = ORIENTED_EDGE ( 'NONE', *, *, #7132, .F. ) ;
#30928 = CARTESIAN_POINT ( 'NONE',  ( 3.680974057930773036, 40.59247216052818885, 25.57193971028174673 ) ) ;
#30929 = ORIENTED_EDGE ( 'NONE', *, *, #14823, .F. ) ;
#30930 = CARTESIAN_POINT ( 'NONE',  ( 1.227938101723756947, 26.79402671879326547, 33.52879263017872091 ) ) ;
#30931 = CARTESIAN_POINT ( 'NONE',  ( -6.015611763856276717, 7.216738110653516891, -17.40650793417836439 ) ) ;
#30932 =( BOUNDED_SURFACE ( )  B_SPLINE_SURFACE ( 3, 1, ( 
 ( #33521, #10016 ),
 ( #4346, #57280 ),
 ( #14414, #52598 ),
 ( #56989, #4652 ) ),
 .UNSPECIFIED., .F., .F., .F. ) 
 B_SPLINE_SURFACE_WITH_KNOTS ( ( 4, 4 ),
 ( 2, 2 ),
 ( 0.000000000000000000, 1.000000000000000000 ),
 ( 0.000000000000000000, 1.000000000000000000 ),
 .UNSPECIFIED. ) 
 GEOMETRIC_REPRESENTATION_ITEM ( )  RATIONAL_B_SPLINE_SURFACE ( (
 ( 1.000000000000000000, 1.000000000000000000),
 ( 0.9952954269826590483, 0.8620686068821339365),
 ( 0.9952954269826590483, 0.8620686068821339365),
 ( 1.000000000000000000, 1.000000000000000000) ) ) 
 REPRESENTATION_ITEM ( '' )  SURFACE ( )  );
#30933 = VECTOR ( 'NONE', #31334, 1000.000000000000000 ) ;
#30934 = CARTESIAN_POINT ( 'NONE',  ( 0.2224561200757586565, -20.89867881469742628, -37.71651051365620333 ) ) ;
#30935 = ORIENTED_EDGE ( 'NONE', *, *, #54648, .T. ) ;
#30936 = CARTESIAN_POINT ( 'NONE',  ( 1.227938101723748288, -11.92353943227977986, 41.23019537246705823 ) ) ;
#30937 =( BOUNDED_SURFACE ( )  B_SPLINE_SURFACE ( 3, 1, ( 
 ( #34504, #38291 ),
 ( #10074, #57646 ),
 ( #49202, #5339 ),
 ( #38912, #48586 ) ),
 .UNSPECIFIED., .F., .F., .F. ) 
 B_SPLINE_SURFACE_WITH_KNOTS ( ( 4, 4 ),
 ( 2, 2 ),
 ( 0.000000000000000000, 1.000000000000000000 ),
 ( 0.000000000000000000, 1.000000000000000000 ),
 .UNSPECIFIED. ) 
 GEOMETRIC_REPRESENTATION_ITEM ( )  RATIONAL_B_SPLINE_SURFACE ( (
 ( 1.000000000000000000, 1.000000000000000000),
 ( 0.7282232189291694135, 0.9929344683865672927),
 ( 0.7282232189291694135, 0.9929344683865672927),
 ( 1.000000000000000000, 1.000000000000000000) ) ) 
 REPRESENTATION_ITEM ( '' )  SURFACE ( )  );
#30938 = CARTESIAN_POINT ( 'NONE',  ( 14.84250595937556483, 5.000000000000015099, -10.00000000000000711 ) ) ;
#30940 = VERTEX_POINT ( 'NONE', #12271 ) ;
#30939 = EDGE_CURVE ( 'NONE', #26668, #1954, #47674, .T. ) ;
#30941 = B_SPLINE_CURVE_WITH_KNOTS ( 'NONE', 3,
 ( #31799, #51191, #2963, #17387, #12702, #59979 ),
 .UNSPECIFIED., .F., .F.,
 ( 4, 2, 4 ),
 ( 6.942281208919283290E-18, 0.0002291472222819949955, 0.0004582944445639830521 ),
 .UNSPECIFIED. ) ;
#30942 = VERTEX_POINT ( 'NONE', #21965 ) ;
#30943 = CARTESIAN_POINT ( 'NONE',  ( 0.8751705887134553219, -37.60752970653848593, 29.98056538504896906 ) ) ;
#30944 = CARTESIAN_POINT ( 'NONE',  ( 0.9968887458511642707, -42.90440775986213851, -0.6574002966412972881 ) ) ;
#30946 = EDGE_CURVE ( 'NONE', #8563, #46275, #30727, .T. ) ;
#30945 = CARTESIAN_POINT ( 'NONE',  ( 0.5806925824938502512, 27.37593026015236219, -38.07598724570169679 ) ) ;
#30947 = CARTESIAN_POINT ( 'NONE',  ( 1.199999999999992628, 8.434754829127421589E-16, 6.887500000000022382 ) ) ;
#30948 = CARTESIAN_POINT ( 'NONE',  ( 0.5800708119828326126, -44.48635609075545005, -17.74761857127114340 ) ) ;
#30949 = CARTESIAN_POINT ( 'NONE',  ( 0.5850706913938533704, 46.31100969101504461, -12.22095376871988215 ) ) ;
#30950 = EDGE_LOOP ( 'NONE', ( #26217, #27231, #40508, #59953 ) ) ;
#30951 = CARTESIAN_POINT ( 'NONE',  ( 3.782542959838396168, -40.24477878435767053, 12.14889435276654162 ) ) ;
#30952 = CARTESIAN_POINT ( 'NONE',  ( 0.3622758884714600280, 42.62881903538200845, 6.444611261694737081 ) ) ;
#30953 = VECTOR ( 'NONE', #18088, 1000.000000000000000 ) ;
#30954 = ORIENTED_EDGE ( 'NONE', *, *, #15858, .F. ) ;
#30955 = DIRECTION ( 'NONE',  ( -0.07836865515943411409, 0.9179910502197414779, -0.3887811538706032466 ) ) ;
#30956 = CARTESIAN_POINT ( 'NONE',  ( 0.9730545539215883499, 42.90536227157002003, 0.5054011016614263774 ) ) ;
#30957 = CARTESIAN_POINT ( 'NONE',  ( 5.895881250540457863, -2.017740640757076154, -20.01140685496494953 ) ) ;
#30958 = CARTESIAN_POINT ( 'NONE',  ( 0.3676999524040323597, -11.75791688508830646, -42.51707861373114383 ) ) ;
#30959 = CARTESIAN_POINT ( 'NONE',  ( 3.660176727303405819, -47.83637937224827397, 4.399934609596405366 ) ) ;
#30960 = DIRECTION ( 'NONE',  ( 0.09835009131224566048, -0.3879606369183696279, 0.9164135549743717135 ) ) ;
#30961 = SHAPE_REPRESENTATION_RELATIONSHIP ( 'NONE' , 'NONE' ,  #13, #21278 ) ;
#30962 = CARTESIAN_POINT ( 'NONE',  ( 0.1156867017252034419, -12.43470245650705586, -42.33581205189435792 ) ) ;
#30963 = CARTESIAN_POINT ( 'NONE',  ( 0.8554163680231738898, -18.91615390926476792, -42.93465493506180053 ) ) ;
#30964 = CARTESIAN_POINT ( 'NONE',  ( 0.2885700199627519447, -40.13549263616314988, -15.75356883787140028 ) ) ;
#30965 = CARTESIAN_POINT ( 'NONE',  ( 4.335381028904201628, 45.77817886910082734, 17.43889867775355285 ) ) ;
#30966 = LINE ( 'NONE', #11889, #41246 ) ;
#30967 = DIRECTION ( 'NONE',  ( 0.000000000000000000, 0.000000000000000000, 1.000000000000000000 ) ) ;
#30968 = ADVANCED_FACE ( 'NONE', ( #54513 ), #53277, .F. ) ;
#30969 = B_SPLINE_CURVE_WITH_KNOTS ( 'NONE', 3,
 ( #39178, #58231, #25361, #20362 ),
 .UNSPECIFIED., .F., .F.,
 ( 4, 4 ),
 ( 0.000000000000000000, 0.004447772540403827600 ),
 .UNSPECIFIED. ) ;
#30970 = DIRECTION ( 'NONE',  ( 0.1736481776669314137, -0.9848077530122077983, 5.551115123125779621E-17 ) ) ;
#30971 = EDGE_CURVE ( 'NONE', #8614, #49719, #41703, .T. ) ;
#30972 = VECTOR ( 'NONE', #28498, 1000.000000000000000 ) ;
#30973 = ORIENTED_EDGE ( 'NONE', *, *, #3459, .T. ) ;
#30974 = CARTESIAN_POINT ( 'NONE',  ( 3.407937589446174087, 3.099921468255003809, 13.34359005742690485 ) ) ;
#30975 = ADVANCED_FACE ( 'NONE', ( #60155 ), #60623, .F. ) ;
#30976 = ADVANCED_FACE ( 'NONE', ( #2528 ), #39458, .F. ) ;
#30977 = AXIS2_PLACEMENT_3D ( 'NONE', #8714, #18130, #8100 ) ;
#30978 = CARTESIAN_POINT ( 'NONE',  ( 0.1092565886968783900, 43.12345370280014833, -0.3103822814775415995 ) ) ;
#30979 = CARTESIAN_POINT ( 'NONE',  ( 0.9757402383260939116, -39.60970160107522986, -16.49876987395769490 ) ) ;
#30980 = CARTESIAN_POINT ( 'NONE',  ( 0.9722240750034578660, -25.65687433776921722, 34.39263040572782870 ) ) ;
#30981 = DIRECTION ( 'NONE',  ( -1.000000000000000000, 0.000000000000000000, 0.000000000000000000 ) ) ;
#30982 = ADVANCED_FACE ( 'NONE', ( #17571 ), #50289, .T. ) ;
#30983 = ORIENTED_EDGE ( 'NONE', *, *, #11710, .T. ) ;
#30984 = CARTESIAN_POINT ( 'NONE',  ( 2.301430502907646947, 30.25184447737433402, -37.31003439265377608 ) ) ;
#30985 = DIRECTION ( 'NONE',  ( 0.000000000000000000, 0.000000000000000000, -1.000000000000000000 ) ) ;
#30986 = DIRECTION ( 'NONE',  ( 1.000000000000000000, 0.000000000000000000, 0.000000000000000000 ) ) ;
#30987 = ORIENTED_EDGE ( 'NONE', *, *, #33689, .T. ) ;
#30988 = ADVANCED_FACE ( 'NONE', ( #46707 ), #36981, .F. ) ;
#30989 = CARTESIAN_POINT ( 'NONE',  ( 0.9722240741986377666, 41.29187377038500983, 11.66659279943990946 ) ) ;
#30990 = ORIENTED_EDGE ( 'NONE', *, *, #48161, .F. ) ;
#30991 = DIRECTION ( 'NONE',  ( -0.07836865515943411409, -0.9608836331491561467, 0.2656332009267280969 ) ) ;
#30992 = CIRCLE ( 'NONE', #25984, 42.92674063221959813 ) ;
#30993 = CARTESIAN_POINT ( 'NONE',  ( 0.6001305935487422083, 33.64689939321895196, 34.38748867424724409 ) ) ;
#30994 = ORIENTED_EDGE ( 'NONE', *, *, #27440, .F. ) ;
#30995 = CARTESIAN_POINT ( 'NONE',  ( 5.901764892641307547, -27.98073834948241156, -40.18793038783513794 ) ) ;
#30996 = ORIENTED_EDGE ( 'NONE', *, *, #17610, .F. ) ;
#30997 = CARTESIAN_POINT ( 'NONE',  ( 4.549368137175248350, 0.000000000000000000, 0.000000000000000000 ) ) ;
#30998 = CARTESIAN_POINT ( 'NONE',  ( 0.1140933569871963454, 20.07213292652290448, 39.29452162660719239 ) ) ;
#30999 = ORIENTED_EDGE ( 'NONE', *, *, #12198, .F. ) ;
#31000 = ORIENTED_EDGE ( 'NONE', *, *, #12325, .F. ) ;
#31001 = CARTESIAN_POINT ( 'NONE',  ( 5.896782393890504181, -9.671431223050909409, -17.63489452692610371 ) ) ;
#31002 = VERTEX_POINT ( 'NONE', #13812 ) ;
#31003 = CARTESIAN_POINT ( 'NONE',  ( 0.5839879327111930918, -38.05372318152033273, -29.08515285004925488 ) ) ;
#31004 = ORIENTED_EDGE ( 'NONE', *, *, #6384, .T. ) ;
#31005 = ORIENTED_EDGE ( 'NONE', *, *, #53036, .T. ) ;
#31006 = CARTESIAN_POINT ( 'NONE',  ( 0.8753041380234471980, 11.79227530596935658, -47.66634631457717575 ) ) ;
#31007 = CARTESIAN_POINT ( 'NONE',  ( 0.6000166863083090663, 41.44150143800075625, -26.35195325346177242 ) ) ;
#31008 = DIRECTION ( 'NONE',  ( 0.02222222222222222307, 0.9997530559290660479, -0.000000000000000000 ) ) ;
#31009 = CARTESIAN_POINT ( 'NONE',  ( 0.1104177457020373010, -16.49849172082188886, 39.84367193872649437 ) ) ;
#31010 = CARTESIAN_POINT ( 'NONE',  ( 3.270143674763207553, -13.53222904135352778, -2.058141141425741338 ) ) ;
#31011 = ORIENTED_EDGE ( 'NONE', *, *, #28155, .T. ) ;
#31012 = CARTESIAN_POINT ( 'NONE',  ( 0.1129192098497455998, -0.9297496242496093855, -44.11448008785053787 ) ) ;
#31013 = FACE_OUTER_BOUND ( 'NONE', #26438, .T. ) ;
#31014 = CARTESIAN_POINT ( 'NONE',  ( -6.077587904424778920, 19.09718056542704900, 2.468545289316316893 ) ) ;
#31015 = ORIENTED_EDGE ( 'NONE', *, *, #61142, .T. ) ;
#31016 =( BOUNDED_SURFACE ( )  B_SPLINE_SURFACE ( 3, 1, ( 
 ( #27178, #31262 ),
 ( #59761, #13096 ),
 ( #7428, #2737 ),
 ( #26559, #3656 ) ),
 .UNSPECIFIED., .F., .F., .F. ) 
 B_SPLINE_SURFACE_WITH_KNOTS ( ( 4, 4 ),
 ( 2, 2 ),
 ( 0.000000000000000000, 1.000000000000000000 ),
 ( 0.000000000000000000, 1.000000000000000000 ),
 .UNSPECIFIED. ) 
 GEOMETRIC_REPRESENTATION_ITEM ( )  RATIONAL_B_SPLINE_SURFACE ( (
 ( 1.000000000000000000, 1.000000000000000000),
 ( 0.7269869731126817891, 0.9931720237060910339),
 ( 0.7269869731126817891, 0.9931720237060910339),
 ( 1.000000000000000000, 1.000000000000000000) ) ) 
 REPRESENTATION_ITEM ( '' )  SURFACE ( )  );
#31017 = EDGE_LOOP ( 'NONE', ( #2412, #58073, #5315, #61086 ) ) ;
#31018 = CARTESIAN_POINT ( 'NONE',  ( 0.2224561200757660395, -33.74134531362616229, -26.84793396060971205 ) ) ;
#31020 = ADVANCED_FACE ( 'NONE', ( #8777 ), #29275, .T. ) ;
#31019 = CARTESIAN_POINT ( 'NONE',  ( 1.231276596079887931, 36.49189576017872128, 20.63051901543724043 ) ) ;
#31021 = CARTESIAN_POINT ( 'NONE',  ( 0.9775691876210972353, 40.51774410171000795, -10.70729293044395369 ) ) ;
#31022 = ORIENTED_EDGE ( 'NONE', *, *, #6540, .T. ) ;
#31023 = CARTESIAN_POINT ( 'NONE',  ( 0.5980271706414711508, 40.77460832818520231, 27.37664257217734587 ) ) ;
#31024 = CARTESIAN_POINT ( 'NONE',  ( -6.078726893082806448, -14.66462719274117887, 12.47969352855413838 ) ) ;
#31025 = CARTESIAN_POINT ( 'NONE',  ( -18.90388840650297553, -12.35675306864543188, -1.887713692035127400 ) ) ;
#31026 =( BOUNDED_SURFACE ( )  B_SPLINE_SURFACE ( 3, 1, ( 
 ( #24679, #52869 ),
 ( #48186, #58168 ),
 ( #15292, #14679 ),
 ( #863, #56945 ) ),
 .UNSPECIFIED., .F., .F., .F. ) 
 B_SPLINE_SURFACE_WITH_KNOTS ( ( 4, 4 ),
 ( 2, 2 ),
 ( 0.000000000000000000, 1.000000000000000000 ),
 ( 0.000000000000000000, 1.000000000000000000 ),
 .UNSPECIFIED. ) 
 GEOMETRIC_REPRESENTATION_ITEM ( )  RATIONAL_B_SPLINE_SURFACE ( (
 ( 1.000000000000000000, 1.000000000000000000),
 ( 0.7282232189291694135, 0.9929344683865672927),
 ( 0.7282232189291694135, 0.9929344683865672927),
 ( 1.000000000000000000, 1.000000000000000000) ) ) 
 REPRESENTATION_ITEM ( '' )  SURFACE ( )  );
#31027 = ORIENTED_EDGE ( 'NONE', *, *, #31173, .T. ) ;
#31028 = CARTESIAN_POINT ( 'NONE',  ( 0.8560838555295223751, 42.82099363437819051, -19.15033519931896322 ) ) ;
#31029 = VERTEX_POINT ( 'NONE', #47932 ) ;
#31030 = CARTESIAN_POINT ( 'NONE',  ( -6.078457390727109555, 18.62736532255359734, -4.880140589945706431 ) ) ;
#31031 = CARTESIAN_POINT ( 'NONE',  ( 0.9757892942422837779, -34.01031843153910472, 26.16173342773525690 ) ) ;
#31032 =( NAMED_UNIT ( * ) PLANE_ANGLE_UNIT ( ) SI_UNIT ( $, .RADIAN. ) );
#31033 = CARTESIAN_POINT ( 'NONE',  ( 4.549368137175248350, -42.82045902618770583, -3.018832571116409014 ) ) ;
#31034 = CIRCLE ( 'NONE', #6987, 43.92652462719577500 ) ;
#31035 = ORIENTED_EDGE ( 'NONE', *, *, #40714, .T. ) ;
#31036 = CARTESIAN_POINT ( 'NONE',  ( 0.9740398440564311811, 21.09418882170589171, -37.36539512267997765 ) ) ;
#31037 = CARTESIAN_POINT ( 'NONE',  ( 0.8560838555295158248, 28.55542365806940452, -37.21505896528851309 ) ) ;
#31038 = CARTESIAN_POINT ( 'NONE',  ( 0.3622758884714600280, -39.50828911766986096, -17.25816669464980890 ) ) ;
#31039 = VECTOR ( 'NONE', #2567, 1000.000000000000114 ) ;
#31040 = CARTESIAN_POINT ( 'NONE',  ( 0.1097557419366048670, 21.36873056345894284, -37.45792859959205856 ) ) ;
#31041 = CARTESIAN_POINT ( 'NONE',  ( 4.975801465491694664, 15.94009207553051510, -45.18341283946441678 ) ) ;
#31042 = CARTESIAN_POINT ( 'NONE',  ( 5.895596859100789899, 19.70914391261472076, -4.009716878325650491 ) ) ;
#31043 = CARTESIAN_POINT ( 'NONE',  ( 4.962356264823603702, 0.9708976703223142213, -42.07484944210863631 ) ) ;
#31044 = FACE_OUTER_BOUND ( 'NONE', #59753, .T. ) ;
#31045 = CARTESIAN_POINT ( 'NONE',  ( 4.834790513006555379, -31.42367164492902631, 35.28657253511686775 ) ) ;
#31046 = B_SPLINE_CURVE_WITH_KNOTS ( 'NONE', 3,
 ( #55157, #16340, #2844, #16041 ),
 .UNSPECIFIED., .F., .F.,
 ( 4, 4 ),
 ( 2.302551629917872730E-17, 0.004564976165746188579 ),
 .UNSPECIFIED. ) ;
#31047 = EDGE_CURVE ( 'NONE', #17533, #19313, #45473, .T. ) ;
#31048 = ADVANCED_FACE ( 'NONE', ( #3748 ), #34685, .F. ) ;
#31049 = CARTESIAN_POINT ( 'NONE',  ( 5.838029081930955932, 46.28366904854783570, 9.427992233631421470 ) ) ;
#31050 = CARTESIAN_POINT ( 'NONE',  ( 0.8560838555295223751, 33.26091945577352504, 33.07694168205818386 ) ) ;
#31051 = ORIENTED_EDGE ( 'NONE', *, *, #27497, .T. ) ;
#31052 = EDGE_CURVE ( 'NONE', #51504, #40436, #28250, .T. ) ;
#31053 = CARTESIAN_POINT ( 'NONE',  ( 1.827326673878743923, -41.24690799101799854, -12.32830836993806578 ) ) ;
#31054 = CARTESIAN_POINT ( 'NONE',  ( 0.5838002273316426072, 46.22850660674022549, 12.52789267095200820 ) ) ;
#31055 = DIRECTION ( 'NONE',  ( 0.000000000000000000, 0.000000000000000000, 1.000000000000000000 ) ) ;
#31056 = ADVANCED_FACE ( 'NONE', ( #61377 ), #47863, .F. ) ;
#31057 = ORIENTED_EDGE ( 'NONE', *, *, #17266, .T. ) ;
#31058 = CARTESIAN_POINT ( 'NONE',  ( 0.5988103564986356764, 47.77151399983768698, 5.677495323490888701 ) ) ;
#31059 = CARTESIAN_POINT ( 'NONE',  ( 4.833616638992205949, 14.43699082351650809, 43.93936707042104928 ) ) ;
#31060 = CARTESIAN_POINT ( 'NONE',  ( 0.6029303876144825880, -12.32464004947847336, -46.50193792184020936 ) ) ;
#31061 = ORIENTED_EDGE ( 'NONE', *, *, #23071, .T. ) ;
#31062 = FACE_OUTER_BOUND ( 'NONE', #54604, .T. ) ;
#31063 = B_SPLINE_CURVE_WITH_KNOTS ( 'NONE', 3,
 ( #58054, #38379, #5119, #24876 ),
 .UNSPECIFIED., .F., .F.,
 ( 4, 4 ),
 ( 0.000000000000000000, 0.005014147105413698652 ),
 .UNSPECIFIED. ) ;
#31064 = CARTESIAN_POINT ( 'NONE',  ( -6.016104459813371719, 13.32794178584997624, 13.32039631884689257 ) ) ;
#31065 = VERTEX_POINT ( 'NONE', #4352 ) ;
#31066 = B_SPLINE_CURVE_WITH_KNOTS ( 'NONE', 3,
 ( #25543, #44679, #54331, #24942, #20854, #25237, #11456, #49653, #50575, #60274, #31168, #41521, #7030, #26783, #41214, #17388 ),
 .UNSPECIFIED., .F., .F.,
 ( 4, 3, 3, 3, 3, 4 ),
 ( 1.868480190406682863E-17, 0.0002618515315864419226, 0.0003927756766341999428, 0.0005236998216950559384, 0.0007855159896329862125, 0.001047349442285928738 ),
 .UNSPECIFIED. ) ;
#31067 = ADVANCED_FACE ( 'NONE', ( #17885 ), #3006, .F. ) ;
#31068 = DIRECTION ( 'NONE',  ( -1.000000000000000000, -0.000000000000000000, -0.000000000000000000 ) ) ;
#31069 = VERTEX_POINT ( 'NONE', #42321 ) ;
#31070 = ORIENTED_EDGE ( 'NONE', *, *, #3806, .T. ) ;
#31071 = CARTESIAN_POINT ( 'NONE',  ( 0.9747592971366223491, -5.279515277919681004, 42.58247319705104417 ) ) ;
#31073 = VERTEX_POINT ( 'NONE', #28489 ) ;
#31072 = EDGE_CURVE ( 'NONE', #14733, #46644, #14118, .T. ) ;
#31074 = CARTESIAN_POINT ( 'NONE',  ( 5.901764892641307547, 19.86141101510697027, -44.76065035194043418 ) ) ;
#31075 = ORIENTED_EDGE ( 'NONE', *, *, #36113, .F. ) ;
#31076 = CARTESIAN_POINT ( 'NONE',  ( 0.9754292589017183879, -22.05710651247192899, 35.63441481479315343 ) ) ;
#31077 = AXIS2_PLACEMENT_3D ( 'NONE', #14713, #23794, #57272 ) ;
#31078 = CARTESIAN_POINT ( 'NONE',  ( -6.078075953587585900, -14.65899360350491243, -12.48635578459696482 ) ) ;
#31079 = ORIENTED_EDGE ( 'NONE', *, *, #49, .T. ) ;
#31080 = CARTESIAN_POINT ( 'NONE',  ( 0.1140933569871964287, 43.38147022400296748, -8.062133172296839234 ) ) ;
#31081 = CARTESIAN_POINT ( 'NONE',  ( 0.5786265663353196143, 46.07681357296485203, 13.09387673186351719 ) ) ;
#31082 = CARTESIAN_POINT ( 'NONE',  ( 0.5797568599927127586, -14.49376273346966926, 44.59995684411468631 ) ) ;
#31083 = DIRECTION ( 'NONE',  ( -1.000000000000000000, -0.000000000000000000, -0.000000000000000000 ) ) ;
#31084 = ORIENTED_EDGE ( 'NONE', *, *, #3762, .F. ) ;
#31085 = B_SPLINE_CURVE_WITH_KNOTS ( 'NONE', 3,
 ( #8139, #60743, #17864, #50317, #31219, #16508 ),
 .UNSPECIFIED., .F., .F.,
 ( 4, 2, 4 ),
 ( 1.544890704737618961E-16, 0.0002445252820015170756, 0.0004890505640028796524 ),
 .UNSPECIFIED. ) ;
#31086 = VERTEX_POINT ( 'NONE', #27577 ) ;
#31087 = CARTESIAN_POINT ( 'NONE',  ( 0.1101816497532063233, 41.68997876247031797, 11.03018586750508945 ) ) ;
#31088 = CARTESIAN_POINT ( 'NONE',  ( 5.896278296736517710, 5.953715084307535044, 19.21146158701290929 ) ) ;
#31089 = EDGE_CURVE ( 'NONE', #23013, #50690, #225, .T. ) ;
#31090 = CARTESIAN_POINT ( 'NONE',  ( 0.7954196712028474003, -47.79303691884135219, 5.415566793624525310 ) ) ;
#31091 = ORIENTED_EDGE ( 'NONE', *, *, #9922, .F. ) ;
#31092 = CARTESIAN_POINT ( 'NONE',  ( 0.5834872094924171693, -46.20467604622292157, -12.61552836343339656 ) ) ;
#31093 = CARTESIAN_POINT ( 'NONE',  ( 3.783198216974392292, -38.10565824507913391, 20.00646744835652413 ) ) ;
#31094 = CARTESIAN_POINT ( 'NONE',  ( 1.092182651088186018, 41.42847769239433831, -6.359435551451717572 ) ) ;
#31095 = CARTESIAN_POINT ( 'NONE',  ( 4.963659409799329403, -42.22332985082321954, 14.83726297270265881 ) ) ;
#31096 = EDGE_LOOP ( 'NONE', ( #36030, #13830, #30041, #1690 ) ) ;
#31097 = ORIENTED_EDGE ( 'NONE', *, *, #42951, .T. ) ;
#31098 = CARTESIAN_POINT ( 'NONE',  ( 5.860006189529246790, 47.30296539008823942, 9.426589201135659124 ) ) ;
#31099 = CARTESIAN_POINT ( 'NONE',  ( 3.221118495291109163, 42.30175278488824375, 12.05500439601543050 ) ) ;
#31100 = CARTESIAN_POINT ( 'NONE',  ( 0.9752132459055881109, -16.20487516111980497, 39.73079175141342745 ) ) ;
#31101 = CARTESIAN_POINT ( 'NONE',  ( 0.1368894036331270159, -18.44144849573008216, -40.08458934930814621 ) ) ;
#31102 = DIRECTION ( 'NONE',  ( 0.000000000000000000, 0.000000000000000000, -1.000000000000000000 ) ) ;
#31103 = CARTESIAN_POINT ( 'NONE',  ( 0.1129192098497447394, 25.64022107388777272, 35.91003830501040994 ) ) ;
#31104 = CARTESIAN_POINT ( 'NONE',  ( 0.8760168074887090262, 46.68716261866160266, 11.58706983520342426 ) ) ;
#31105 = CARTESIAN_POINT ( 'NONE',  ( 4.291220156522060236, 35.59851124210567264, -30.85668476442946329 ) ) ;
#31106 = B_SPLINE_CURVE_WITH_KNOTS ( 'NONE', 3,
 ( #47521, #4884, #19030, #18403, #18092, #42527 ),
 .UNSPECIFIED., .F., .F.,
 ( 4, 2, 4 ),
 ( 1.159750240187440271E-16, 0.0002448718616795938553, 0.0004897437233590718093 ),
 .UNSPECIFIED. ) ;
#31107 = CARTESIAN_POINT ( 'NONE',  ( 0.9722240741986366563, 5.023189681690755748, 42.61332881199389533 ) ) ;
#31108 = CARTESIAN_POINT ( 'NONE',  ( 0.7057020205115015488, -41.89806668505397624, 23.21851350879803277 ) ) ;
#31109 = CARTESIAN_POINT ( 'NONE',  ( 0.5998501479064699549, -17.92509395669137362, 44.64337787626217846 ) ) ;
#31110 = CARTESIAN_POINT ( 'NONE',  ( 1.154321485836933503, 29.75729673892742255, -30.92445806269047637 ) ) ;
#31111 = DIRECTION ( 'NONE',  ( -1.000000000000000000, -5.380183451256670742E-17, 1.298891185607911324E-16 ) ) ;
#31112 = CARTESIAN_POINT ( 'NONE',  ( 0.9789889208857696090, -22.46918319153057553, 35.37613185111973735 ) ) ;
#31113 = AXIS2_PLACEMENT_3D ( 'NONE', #17262, #22574, #32595 ) ;
#31114 = EDGE_CURVE ( 'NONE', #59626, #44755, #58858, .T. ) ;
#31115 = DIRECTION ( 'NONE',  ( 0.000000000000000000, 0.000000000000000000, 1.000000000000000000 ) ) ;
#31116 = CARTESIAN_POINT ( 'NONE',  ( 0.9754292580325131246, -27.49953659056433608, 31.62440440875080583 ) ) ;
#31118 = ORIENTED_EDGE ( 'NONE', *, *, #5361, .T. ) ;
#31117 = CARTESIAN_POINT ( 'NONE',  ( 0.6064782688330886407, 23.15856706935003473, -40.78008359129716354 ) ) ;
#31119 = ORIENTED_EDGE ( 'NONE', *, *, #40120, .F. ) ;
#31120 = CARTESIAN_POINT ( 'NONE',  ( 1.231276596079887264, -11.60895935156443848, 40.28037777618019533 ) ) ;
#31121 = CARTESIAN_POINT ( 'NONE',  ( 2.281351352603290028, -13.68106635380595293, 45.98107981851860160 ) ) ;
#31122 = EDGE_CURVE ( 'NONE', #8559, #20443, #51424, .T. ) ;
#31123 = ORIENTED_EDGE ( 'NONE', *, *, #47380, .T. ) ;
#31124 = ORIENTED_EDGE ( 'NONE', *, *, #29555, .F. ) ;
#31125 = CARTESIAN_POINT ( 'NONE',  ( 3.727782113643637540, -30.05637732902805936, 32.08413872556130997 ) ) ;
#31126 = CARTESIAN_POINT ( 'NONE',  ( 0.5807400328401637335, -12.92266817605982965, -46.12278621143511259 ) ) ;
#31127 = UNCERTAINTY_MEASURE_WITH_UNIT (LENGTH_MEASURE( 1.000000000000000082E-05 ), #1204, 'distance_accuracy_value', 'NONE');
#31128 = VERTEX_POINT ( 'NONE', #15346 ) ;
#31129 = ORIENTED_EDGE ( 'NONE', *, *, #57839, .F. ) ;
#31130 =( BOUNDED_SURFACE ( )  B_SPLINE_SURFACE ( 3, 1, ( 
 ( #15366, #47637 ),
 ( #24127, #53542 ),
 ( #10660, #61698 ),
 ( #33862, #52937 ) ),
 .UNSPECIFIED., .F., .F., .F. ) 
 B_SPLINE_SURFACE_WITH_KNOTS ( ( 4, 4 ),
 ( 2, 2 ),
 ( 0.000000000000000000, 1.000000000000000000 ),
 ( 0.000000000000000000, 1.000000000000000000 ),
 .UNSPECIFIED. ) 
 GEOMETRIC_REPRESENTATION_ITEM ( )  RATIONAL_B_SPLINE_SURFACE ( (
 ( 1.000000000000000000, 1.000000000000000000),
 ( 0.7223157951917476005, 0.9931996967497186413),
 ( 0.7223157951917476005, 0.9931996967497186413),
 ( 1.000000000000000000, 1.000000000000000000) ) ) 
 REPRESENTATION_ITEM ( '' )  SURFACE ( )  );
#31131 = B_SPLINE_CURVE_WITH_KNOTS ( 'NONE', 3,
 ( #33699, #52775, #9878, #48094, #24278, #43413 ),
 .UNSPECIFIED., .F., .F.,
 ( 4, 2, 4 ),
 ( 1.870559545977334001E-17, 0.0002293319059085097643, 0.0004586638118170008262 ),
 .UNSPECIFIED. ) ;
#31132 = CARTESIAN_POINT ( 'NONE',  ( 0.5836750258453351492, 47.89563095930319747, 0.1816059738418068226 ) ) ;
#31133 = DIRECTION ( 'NONE',  ( 0.9848077530122080203, 0.1736481776669315247, -2.220446049250313081E-16 ) ) ;
#31134 = FACE_OUTER_BOUND ( 'NONE', #15266, .T. ) ;
#31135 = ORIENTED_EDGE ( 'NONE', *, *, #55572, .F. ) ;
#31136 = EDGE_CURVE ( 'NONE', #11576, #472, #34148, .T. ) ;
#31137 = DIRECTION ( 'NONE',  ( -1.000000000000000000, -0.000000000000000000, -0.000000000000000000 ) ) ;
#31138 = CARTESIAN_POINT ( 'NONE',  ( -6.078726893082806448, 16.77980020642716141, -9.446287434813061878 ) ) ;
#31139 = CARTESIAN_POINT ( 'NONE',  ( 0.1154773475650540393, 15.07002877585266809, -41.47092792235417136 ) ) ;
#31140 = ORIENTED_EDGE ( 'NONE', *, *, #27382, .F. ) ;
#31141 = ORIENTED_EDGE ( 'NONE', *, *, #2613, .T. ) ;
#31142 = CARTESIAN_POINT ( 'NONE',  ( 0.6845945791218023269, -20.52768236698738846, -42.17843972166372879 ) ) ;
#31143 = CARTESIAN_POINT ( 'NONE',  ( 8.000000000000000000, 0.000000000000000000, 0.000000000000000000 ) ) ;
#31144 = ORIENTED_EDGE ( 'NONE', *, *, #1194, .F. ) ;
#31145 = CARTESIAN_POINT ( 'NONE',  ( 5.895596859100789899, 14.91436009500259097, -13.49407448360508255 ) ) ;
#31146 = CARTESIAN_POINT ( 'NONE',  ( 4.956445790444011124, -11.44166143951963122, -45.67960632101645757 ) ) ;
#31147 = FACE_OUTER_BOUND ( 'NONE', #17827, .T. ) ;
#31148 = CARTESIAN_POINT ( 'NONE',  ( 3.559346040607745287, -43.82484226701208030, -3.579592408850357010 ) ) ;
#31149 = ORIENTED_EDGE ( 'NONE', *, *, #13474, .T. ) ;
#31150 = CARTESIAN_POINT ( 'NONE',  ( 4.335381028904201628, -48.81116855472419758, 4.150502618556926038 ) ) ;
#31151 = VECTOR ( 'NONE', #61637, 1000.000000000000114 ) ;
#31152 = CARTESIAN_POINT ( 'NONE',  ( 0.6028618097248863439, 18.57111736963386051, 44.37846879336940731 ) ) ;
#31153 = AXIS2_PLACEMENT_3D ( 'NONE', #36857, #37470, #13348 ) ;
#31154 = CARTESIAN_POINT ( 'NONE',  ( 5.895596859100789899, 14.91436009500259097, -13.49407448360508255 ) ) ;
#31155 = LINE ( 'NONE', #54017, #19452 ) ;
#31156 = EDGE_CURVE ( 'NONE', #58292, #23810, #2247, .T. ) ;
#31157 = VERTEX_POINT ( 'NONE', #34452 ) ;
#31158 = CARTESIAN_POINT ( 'NONE',  ( 0.1102144999581332607, 42.77179372778542898, -5.503895401229541129 ) ) ;
#31159 = CARTESIAN_POINT ( 'NONE',  ( 0.2230388203127594560, -4.873876086128563934, 42.84312106681672816 ) ) ;
#31160 = CARTESIAN_POINT ( 'NONE',  ( 0.5997462898726536595, -43.04230894295751852, 23.64130434225888777 ) ) ;
#31161 = CARTESIAN_POINT ( 'NONE',  ( 1.154321713695930507, 36.74718012229653397, 22.16897764010616001 ) ) ;
#31162 = ORIENTED_EDGE ( 'NONE', *, *, #16783, .T. ) ;
#31163 = DIRECTION ( 'NONE',  ( -1.000000000000000000, -0.000000000000000000, -0.000000000000000000 ) ) ;
#31164 = CARTESIAN_POINT ( 'NONE',  ( 1.157644175074336035, 20.86452795889626799, -36.35483115806782450 ) ) ;
#31165 = CARTESIAN_POINT ( 'NONE',  ( -6.016761891674565099, -0.003433883959915969616, 18.84319130225482297 ) ) ;
#31166 = B_SPLINE_CURVE_WITH_KNOTS ( 'NONE', 3,
 ( #60621, #26827, #12747, #44497, #56241, #41256 ),
 .UNSPECIFIED., .F., .F.,
 ( 4, 2, 4 ),
 ( 0.000000000000000000, 0.0002447195606305743124, 0.0004894391212611486248 ),
 .UNSPECIFIED. ) ;
#31167 = EDGE_CURVE ( 'NONE', #14312, #2143, #53525, .T. ) ;
#31168 = CARTESIAN_POINT ( 'NONE',  ( 0.6031356219577718170, -41.61861914321228539, 24.12932366310793952 ) ) ;
#31169 = DIRECTION ( 'NONE',  ( 1.000000000000000000, 1.836909530733573776E-16, 0.000000000000000000 ) ) ;
#31170 = DIRECTION ( 'NONE',  ( -1.000000000000000000, -0.000000000000000000, -0.000000000000000000 ) ) ;
#31171 = CARTESIAN_POINT ( 'NONE',  ( 4.694002226626921015, -26.36364849202877991, 37.19197238161595465 ) ) ;
#31172 = CYLINDRICAL_SURFACE ( 'NONE', #16957, 2.649999999999992806 ) ;
#31173 = EDGE_CURVE ( 'NONE', #47431, #32248, #10327, .T. ) ;
#31174 = CARTESIAN_POINT ( 'NONE',  ( 0.6001305935487422083, -6.798494447611897584, -47.62765676940940551 ) ) ;
#31175 = DIRECTION ( 'NONE',  ( -1.000000000000000000, -0.000000000000000000, -0.000000000000000000 ) ) ;
#31176 = B_SPLINE_CURVE_WITH_KNOTS ( 'NONE', 3,
 ( #32492, #52192, #42221, #9286, #28393, #47514 ),
 .UNSPECIFIED., .F., .F.,
 ( 4, 2, 4 ),
 ( 0.000000000000000000, 0.0002293801035737127873, 0.0004587602071474255745 ),
 .UNSPECIFIED. ) ;
#31177 = ORIENTED_EDGE ( 'NONE', *, *, #677, .T. ) ;
#31178 = CARTESIAN_POINT ( 'NONE',  ( 4.553261556744873317, 7.233533384970671776, 43.32684572631789166 ) ) ;
#31179 = CARTESIAN_POINT ( 'NONE',  ( 2.643462169533613793, -11.09243630552565563, 46.73820883660187775 ) ) ;
#31180 = DIRECTION ( 'NONE',  ( 0.000000000000000000, 0.000000000000000000, 1.000000000000000000 ) ) ;
#31181 = CARTESIAN_POINT ( 'NONE',  ( -6.078726893082806448, -1.845620846545350080, -19.16736092839902383 ) ) ;
#31182 = B_SPLINE_CURVE_WITH_KNOTS ( 'NONE', 3,
 ( #1280, #38611, #20413, #39540, #57662, #33909 ),
 .UNSPECIFIED., .F., .F.,
 ( 4, 2, 4 ),
 ( 7.040638946443416885E-18, 0.0002445244328975364808, 0.0004890488657950659143 ),
 .UNSPECIFIED. ) ;
#31183 = FACE_OUTER_BOUND ( 'NONE', #45801, .T. ) ;
#31184 = CARTESIAN_POINT ( 'NONE',  ( 5.896782393890504181, 5.965008392937153126, -19.20793486427423247 ) ) ;
#31185 = DIRECTION ( 'NONE',  ( 0.09835009131224567436, 0.7941905447268818863, -0.5996571005210326044 ) ) ;
#31186 =( BOUNDED_SURFACE ( )  B_SPLINE_SURFACE ( 3, 1, ( 
 ( #55959, #51559 ),
 ( #13077, #32173 ),
 ( #38744, #34338 ),
 ( #57799, #28695 ) ),
 .UNSPECIFIED., .F., .F., .F. ) 
 B_SPLINE_SURFACE_WITH_KNOTS ( ( 4, 4 ),
 ( 2, 2 ),
 ( 0.000000000000000000, 1.000000000000000000 ),
 ( 0.000000000000000000, 1.000000000000000000 ),
 .UNSPECIFIED. ) 
 GEOMETRIC_REPRESENTATION_ITEM ( )  RATIONAL_B_SPLINE_SURFACE ( (
 ( 1.000000000000000000, 1.000000000000000000),
 ( 0.7223157951917480446, 0.9931996967497186413),
 ( 0.7223157951917480446, 0.9931996967497186413),
 ( 1.000000000000000000, 1.000000000000000000) ) ) 
 REPRESENTATION_ITEM ( '' )  SURFACE ( )  );
#31187 = CARTESIAN_POINT ( 'NONE',  ( 0.6028618097248863439, 41.57478760529404838, -24.20479143424847379 ) ) ;
#31188 = EDGE_CURVE ( 'NONE', #58971, #37747, #26041, .T. ) ;
#31189 = CARTESIAN_POINT ( 'NONE',  ( 0.5998501479064708430, 0.5236536531314925913, -48.10473956285919428 ) ) ;
#31191 = ORIENTED_EDGE ( 'NONE', *, *, #17564, .F. ) ;
#31190 = CARTESIAN_POINT ( 'NONE',  ( 0.8744876279028306332, -45.16590161815026505, 19.24555484778404590 ) ) ;
#31192 = VERTEX_POINT ( 'NONE', #48843 ) ;
#31193 = CARTESIAN_POINT ( 'NONE',  ( -6.072942160501519915, 0.6026766405724340858, -19.24684242040570581 ) ) ;
#31194 = CARTESIAN_POINT ( 'NONE',  ( 0.5824936645240075261, -8.159118969952315226, 46.18080723281560296 ) ) ;
#31195 = DIRECTION ( 'NONE',  ( -0.1024043820194934368, -0.9573600124648721232, -0.2701391291102888115 ) ) ;
#31196 = EDGE_CURVE ( 'NONE', #1986, #38401, #40935, .T. ) ;
#31197 = ORIENTED_EDGE ( 'NONE', *, *, #37925, .T. ) ;
#31198 = DIRECTION ( 'NONE',  ( 0.1011922191286468015, 0.5796805626819869772, 0.8085360721925242133 ) ) ;
#31199 = FACE_OUTER_BOUND ( 'NONE', #60021, .T. ) ;
#31201 = CARTESIAN_POINT ( 'NONE',  ( 0.1102144999581332607, 41.68747259405349581, -11.03964818279730586 ) ) ;
#31200 = B_SPLINE_CURVE_WITH_KNOTS ( 'NONE', 3,
 ( #53416, #15234, #29935, #25850 ),
 .UNSPECIFIED., .F., .F.,
 ( 4, 4 ),
 ( 8.673617379884035472E-19, 0.004048833967417085622 ),
 .UNSPECIFIED. ) ;
#31202 = VECTOR ( 'NONE', #590, 1000.000000000000000 ) ;
#31203 = B_SPLINE_CURVE_WITH_KNOTS ( 'NONE', 3,
 ( #32546, #22215, #18440, #17826, #37252, #50697 ),
 .UNSPECIFIED., .F., .F.,
 ( 4, 2, 4 ),
 ( 0.002336974151641539946, 0.003500975885716448889, 0.004664977619791357832 ),
 .UNSPECIFIED. ) ;
#31204 = EDGE_CURVE ( 'NONE', #48474, #49527, #56647, .T. ) ;
#31205 =( BOUNDED_SURFACE ( )  B_SPLINE_SURFACE ( 3, 1, ( 
 ( #30795, #45860 ),
 ( #21102, #16403 ),
 ( #35837, #25797 ),
 ( #30481, #1657 ) ),
 .UNSPECIFIED., .F., .F., .F. ) 
 B_SPLINE_SURFACE_WITH_KNOTS ( ( 4, 4 ),
 ( 2, 2 ),
 ( 0.000000000000000000, 1.000000000000000000 ),
 ( 0.000000000000000000, 1.000000000000000000 ),
 .UNSPECIFIED. ) 
 GEOMETRIC_REPRESENTATION_ITEM ( )  RATIONAL_B_SPLINE_SURFACE ( (
 ( 1.000000000000000000, 1.000000000000000000),
 ( 0.9953485035131437453, 0.8621029689291523912),
 ( 0.9953485035131437453, 0.8621029689291523912),
 ( 1.000000000000000000, 1.000000000000000000) ) ) 
 REPRESENTATION_ITEM ( '' )  SURFACE ( )  );
#31206 = AXIS2_PLACEMENT_3D ( 'NONE', #46329, #28424, #8704 ) ;
#31207 = ORIENTED_EDGE ( 'NONE', *, *, #30534, .T. ) ;
#31208 = EDGE_LOOP ( 'NONE', ( #42127, #23165, #47504, #19234 ) ) ;
#31209 = CARTESIAN_POINT ( 'NONE',  ( -6.016761891674564211, 7.214149619366359900, 17.40752468084784965 ) ) ;
#31210 = CARTESIAN_POINT ( 'NONE',  ( -6.078726893082806448, -18.90156862012333860, 3.677600436084480062 ) ) ;
#31211 = DIRECTION ( 'NONE',  ( -1.000000000000000000, 0.000000000000000000, 0.000000000000000000 ) ) ;
#31212 = ORIENTED_EDGE ( 'NONE', *, *, #55652, .T. ) ;
#31213 = EDGE_CURVE ( 'NONE', #9908, #26144, #8836, .T. ) ;
#31214 = B_SPLINE_CURVE_WITH_KNOTS ( 'NONE', 3,
 ( #41813, #60878, #17998, #56182 ),
 .UNSPECIFIED., .F., .F.,
 ( 4, 4 ),
 ( 3.469446951953614189E-18, 0.004042984057420972825 ),
 .UNSPECIFIED. ) ;
#31215 = ORIENTED_EDGE ( 'NONE', *, *, #57759, .F. ) ;
#31216 = DIRECTION ( 'NONE',  ( -1.000000000000000000, -0.000000000000000000, -0.000000000000000000 ) ) ;
#31217 = CARTESIAN_POINT ( 'NONE',  ( 0.6254311100348644015, 0.6881768005102522068, -48.10157347124182792 ) ) ;
#31218 = ORIENTED_EDGE ( 'NONE', *, *, #60368, .T. ) ;
#31219 = CARTESIAN_POINT ( 'NONE',  ( 0.5800708057587384836, 34.30831467131400814, -33.42085258735440334 ) ) ;
#31220 = CARTESIAN_POINT ( 'NONE',  ( -4.062725214796418349, -12.40828859588279798, 0.000000000000000000 ) ) ;
#31221 = ORIENTED_EDGE ( 'NONE', *, *, #2168, .F. ) ;
#31222 = CARTESIAN_POINT ( 'NONE',  ( 1.227938101723756947, 15.63977281655895979, -39.96870412324319943 ) ) ;
#31223 = CARTESIAN_POINT ( 'NONE',  ( 0.5850706913938533704, 0.1816364388707057964, -47.89601588673689037 ) ) ;
#31224 = B_SPLINE_CURVE_WITH_KNOTS ( 'NONE', 3,
 ( #55053, #31264, #45690, #36291 ),
 .UNSPECIFIED., .F., .F.,
 ( 4, 4 ),
 ( 1.951563910473907981E-18, 0.004444878191957666973 ),
 .UNSPECIFIED. ) ;
#31225 = VERTEX_POINT ( 'NONE', #30345 ) ;
#31226 = CARTESIAN_POINT ( 'NONE',  ( 0.6027935024548038978, -47.67281620606627968, -6.452291758824557633 ) ) ;
#31227 = CARTESIAN_POINT ( 'NONE',  ( 0.8560838555295158248, 46.89922841446242074, 0.9138972643637033322 ) ) ;
#31228 = CARTESIAN_POINT ( 'NONE',  ( -2.000000000000022649, -3.464101615137742396, -5.600000000000000533 ) ) ;
#31229 = EDGE_LOOP ( 'NONE', ( #27460, #33200, #59509, #40493 ) ) ;
#31230 = CARTESIAN_POINT ( 'NONE',  ( 4.956653778116975495, -26.26162724282400518, 40.28700667097671584 ) ) ;
#31231 = CARTESIAN_POINT ( 'NONE',  ( 0.1064266418746774578, -42.82540703015436634, 5.071708474752518292 ) ) ;
#31232 = VERTEX_POINT ( 'NONE', #43246 ) ;
#31233 = CARTESIAN_POINT ( 'NONE',  ( 5.895881250540457863, -7.224475463583877044, -18.77057899704682953 ) ) ;
#31234 = VERTEX_POINT ( 'NONE', #49458 ) ;
#31235 = CARTESIAN_POINT ( 'NONE',  ( 0.5832366564991534608, -18.07697797533119655, 44.35361744978930432 ) ) ;
#31236 = ORIENTED_EDGE ( 'NONE', *, *, #21019, .T. ) ;
#31237 = CARTESIAN_POINT ( 'NONE',  ( 4.956445790444006683, -23.10347171912805564, -41.03373788315033721 ) ) ;
#31238 = CARTESIAN_POINT ( 'NONE',  ( 0.6254311100348637353, -17.77188277739589140, -44.70341307176148860 ) ) ;
#31239 = CARTESIAN_POINT ( 'NONE',  ( 4.956653778116966613, 48.02038484091100656, 2.599733001514495712 ) ) ;
#31240 = VERTEX_POINT ( 'NONE', #24111 ) ;
#31241 = CARTESIAN_POINT ( 'NONE',  ( 0.8744876279028306332, -8.712669995481570950, -48.31603700562917680 ) ) ;
#31242 = ADVANCED_FACE ( 'NONE', ( #38542 ), #30043, .F. ) ;
#31243 = FACE_OUTER_BOUND ( 'NONE', #42897, .T. ) ;
#31244 = MANIFOLD_SOLID_BREP ( 'Body', #61019 ) ;
#31245 = CARTESIAN_POINT ( 'NONE',  ( 16.60577576646022635, -4.999999999999987566, 6.123233995736738672E-16 ) ) ;
#31246 = ORIENTED_EDGE ( 'NONE', *, *, #32906, .F. ) ;
#31247 = B_SPLINE_CURVE_WITH_KNOTS ( 'NONE', 3,
 ( #56599, #37849, #18410, #37529, #9299, #56905, #51280, #32507, #55982, #3350, #23407, #50974, #42535, #36598, #46932, #47223, #13405, #51583, #41607 ),
 .UNSPECIFIED., .F., .F.,
 ( 4, 3, 3, 3, 3, 3, 4 ),
 ( 6.071532165918824830E-18, 0.0002724573126191775444, 0.0004086839781548516214, 0.0005449106435901876662, 0.0006811373090491506990, 0.0008459866663933703502, 0.001010840725717213799 ),
 .UNSPECIFIED. ) ;
#31248 = VECTOR ( 'NONE', #57585, 1000.000000000000000 ) ;
#31249 = EDGE_CURVE ( 'NONE', #54442, #44595, #15041, .T. ) ;
#31250 = EDGE_LOOP ( 'NONE', ( #15773, #59734, #13380, #26988 ) ) ;
#31251 = AXIS2_PLACEMENT_3D ( 'NONE', #43046, #52405, #707 ) ;
#31252 = CARTESIAN_POINT ( 'NONE',  ( 0.9762797500689124330, 3.691134646837550104, 41.74566217230983511 ) ) ;
#31253 = CARTESIAN_POINT ( 'NONE',  ( 0.5800708057587384836, -6.873290064481704320, 47.40012370174861900 ) ) ;
#31254 = CARTESIAN_POINT ( 'NONE',  ( 0.9775691876210990117, 38.72908157502681803, -16.01224373237266718 ) ) ;
#31255 = CARTESIAN_POINT ( 'NONE',  ( 0.1095718737110177865, -5.374020908746645731, -42.78833451865665438 ) ) ;
#31256 = CARTESIAN_POINT ( 'NONE',  ( 2.624215991343620935, 34.92983774302966538, 32.93378783738860704 ) ) ;
#31257 = CARTESIAN_POINT ( 'NONE',  ( 0.1064266379913938326, 41.79703901861803672, 10.61815631313376329 ) ) ;
#31258 = ORIENTED_EDGE ( 'NONE', *, *, #35694, .T. ) ;
#31259 = EDGE_CURVE ( 'NONE', #47550, #26385, #27308, .T. ) ;
#31260 = CARTESIAN_POINT ( 'NONE',  ( 5.838029081930955932, -16.95764376597146850, -44.08518318051234530 ) ) ;
#31261 = VERTEX_POINT ( 'NONE', #55381 ) ;
#31262 = CARTESIAN_POINT ( 'NONE',  ( 5.860006189529246790, -47.30296539008818257, -9.426589201135987750 ) ) ;
#31263 = CARTESIAN_POINT ( 'NONE',  ( 0.5837157313716021534, 36.74748076922353590, 29.13519728262657438 ) ) ;
#31264 = CARTESIAN_POINT ( 'NONE',  ( 2.281448460670566281, 44.80776276180771589, 17.13756432392853668 ) ) ;
#31265 = CARTESIAN_POINT ( 'NONE',  ( -6.016761891674565099, -14.94721834528406923, -11.47373234755518823 ) ) ;
#31266 = CARTESIAN_POINT ( 'NONE',  ( -6.016761891674564211, 18.68153697670645030, -2.462934516563616949 ) ) ;
#31267 = CARTESIAN_POINT ( 'NONE',  ( 0.7245667037590759474, -47.57651946688182676, 7.091191019330059575 ) ) ;
#31268 = CARTESIAN_POINT ( 'NONE',  ( 5.910764540655177868, -2.028561139977089756, 20.00965212517543890 ) ) ;
#31269 = SURFACE_SIDE_STYLE ('',( #8075 ) ) ;
#31270 = CARTESIAN_POINT ( 'NONE',  ( 0.1140933569871964287, -12.19049900475206449, -42.40685892752544106 ) ) ;
#31271 = CARTESIAN_POINT ( 'NONE',  ( 0.6001305935487422083, 48.10757715638247589, 0.5236757026890891398 ) ) ;
#31272 = CARTESIAN_POINT ( 'NONE',  ( 0.5807400328401574052, 5.711437504335963311, 47.55718917606844798 ) ) ;
#31273 = ADVANCED_FACE ( 'NONE', ( #55074 ), #5007, .F. ) ;
#31274 = DIRECTION ( 'NONE',  ( 0.000000000000000000, 0.7071067811865500152, -0.7071067811865449082 ) ) ;
#31275 = CARTESIAN_POINT ( 'NONE',  ( -6.010958268070873523, -17.40352239307062021, 7.224487401384238616 ) ) ;
#31276 = LINE ( 'NONE', #41022, #10505 ) ;
#31277 = EDGE_CURVE ( 'NONE', #25998, #35346, #14842, .T. ) ;
#31278 = DIRECTION ( 'NONE',  ( 0.07500201931887535978, -0.9899952385360587526, 0.1195162113439968143 ) ) ;
#31279 = PRODUCT_DEFINITION_SHAPE ( 'NONE', 'NONE',  #61980 ) ;
#31280 = DIRECTION ( 'NONE',  ( 0.09722883295013591554, -0.8634569929835322899, 0.4949632060173673187 ) ) ;
#31281 = CARTESIAN_POINT ( 'NONE',  ( 5.959547316686252039, 10.25972575517530139, -17.77749189599207114 ) ) ;
#31282 = EDGE_CURVE ( 'NONE', #29154, #2006, #44699, .T. ) ;
#31283 = EDGE_LOOP ( 'NONE', ( #35148, #43916, #50789, #11814 ) ) ;
#31284 = CARTESIAN_POINT ( 'NONE',  ( 0.1104177457020373010, 11.15670205480004640, -41.65628910360727843 ) ) ;
#31285 =( BOUNDED_SURFACE ( )  B_SPLINE_SURFACE ( 3, 1, ( 
 ( #42481, #60937 ),
 ( #46248, #13349 ),
 ( #55925, #56847 ),
 ( #56234, #37471 ) ),
 .UNSPECIFIED., .F., .F., .F. ) 
 B_SPLINE_SURFACE_WITH_KNOTS ( ( 4, 4 ),
 ( 2, 2 ),
 ( 0.000000000000000000, 1.000000000000000000 ),
 ( 0.000000000000000000, 1.000000000000000000 ),
 .UNSPECIFIED. ) 
 GEOMETRIC_REPRESENTATION_ITEM ( )  RATIONAL_B_SPLINE_SURFACE ( (
 ( 1.000000000000000000, 1.000000000000000000),
 ( 0.7223157951917480446, 0.9931996967497186413),
 ( 0.7223157951917480446, 0.9931996967497186413),
 ( 1.000000000000000000, 1.000000000000000000) ) ) 
 REPRESENTATION_ITEM ( '' )  SURFACE ( )  );
#31286 = FACE_OUTER_BOUND ( 'NONE', #31468, .T. ) ;
#31287 = CARTESIAN_POINT ( 'NONE',  ( 0.6008122571543326185, -47.61009277872437906, -12.03468387896310787 ) ) ;
#31288 = CARTESIAN_POINT ( 'NONE',  ( -99.49999999999975842, 2.999999999999994671, 1.500000000000001554 ) ) ;
#31289 = ORIENTED_EDGE ( 'NONE', *, *, #56671, .F. ) ;
#31290 = CARTESIAN_POINT ( 'NONE',  ( 0.3676999524040323597, -40.57213187173838520, -17.31625533148287843 ) ) ;
#31291 = CARTESIAN_POINT ( 'NONE',  ( 0.8554163680231816613, -2.480940174720135172, -46.85136507041474374 ) ) ;
#31292 = EDGE_CURVE ( 'NONE', #34772, #40345, #32702, .T. ) ;
#31293 = AXIS2_PLACEMENT_3D ( 'NONE', #1906, #39542, #29187 ) ;
#31294 = CARTESIAN_POINT ( 'NONE',  ( 4.962356264823608143, 0.000000000000000000, 0.000000000000000000 ) ) ;
#31295 = EDGE_LOOP ( 'NONE', ( #25010, #11606, #16137, #11497 ) ) ;
#31296 = CARTESIAN_POINT ( 'NONE',  ( 0.3676999524040323597, -0.5887207181719652516, -44.10900124961835900 ) ) ;
#31297 = ORIENTED_EDGE ( 'NONE', *, *, #47552, .F. ) ;
#31298 =( BOUNDED_SURFACE ( )  B_SPLINE_SURFACE ( 3, 1, ( 
 ( #46239, #31824 ),
 ( #3282, #22414 ),
 ( #21483, #41542 ),
 ( #36849, #40623 ) ),
 .UNSPECIFIED., .F., .F., .F. ) 
 B_SPLINE_SURFACE_WITH_KNOTS ( ( 4, 4 ),
 ( 2, 2 ),
 ( 0.000000000000000000, 1.000000000000000000 ),
 ( 0.000000000000000000, 1.000000000000000000 ),
 .UNSPECIFIED. ) 
 GEOMETRIC_REPRESENTATION_ITEM ( )  RATIONAL_B_SPLINE_SURFACE ( (
 ( 1.000000000000000000, 1.000000000000000000),
 ( 0.7269869731126821222, 0.9931720237060910339),
 ( 0.7269869731126821222, 0.9931720237060910339),
 ( 1.000000000000000000, 1.000000000000000000) ) ) 
 REPRESENTATION_ITEM ( '' )  SURFACE ( )  );
#31299 = CARTESIAN_POINT ( 'NONE',  ( -6.017396004339686577, -13.32495836419615287, -13.32329839588568987 ) ) ;
#31300 = ORIENTED_EDGE ( 'NONE', *, *, #49268, .T. ) ;
#31301 = CARTESIAN_POINT ( 'NONE',  ( 0.6000166863083106206, -34.91285637184702040, 34.53861522509602366 ) ) ;
#31302 = VERTEX_POINT ( 'NONE', #40713 ) ;
#31303 = CARTESIAN_POINT ( 'NONE',  ( 1.511324885427794085, -0.4710387770532362128, -46.93530688883296165 ) ) ;
#31304 = CARTESIAN_POINT ( 'NONE',  ( 1.231276596079881935, 41.65019306089989470, -4.747440258479600494 ) ) ;
#31305 =( BOUNDED_SURFACE ( )  B_SPLINE_SURFACE ( 3, 1, ( 
 ( #17681, #23008 ),
 ( #36809, #28608 ),
 ( #56800, #52102 ),
 ( #47732, #13929 ) ),
 .UNSPECIFIED., .F., .F., .F. ) 
 B_SPLINE_SURFACE_WITH_KNOTS ( ( 4, 4 ),
 ( 2, 2 ),
 ( 0.000000000000000000, 1.000000000000000000 ),
 ( 0.000000000000000000, 1.000000000000000000 ),
 .UNSPECIFIED. ) 
 GEOMETRIC_REPRESENTATION_ITEM ( )  RATIONAL_B_SPLINE_SURFACE ( (
 ( 1.000000000000000000, 1.000000000000000000),
 ( 0.7211978278499970862, 0.9934217856018976445),
 ( 0.7211978278499970862, 0.9934217856018976445),
 ( 1.000000000000000000, 1.000000000000000000) ) ) 
 REPRESENTATION_ITEM ( '' )  SURFACE ( )  );
#31306 = VERTEX_POINT ( 'NONE', #2762 ) ;
#31307 = CARTESIAN_POINT ( 'NONE',  ( 5.901463166500146684, -9.678444301826155893, -17.63081354439112403 ) ) ;
#31308 = ORIENTED_EDGE ( 'NONE', *, *, #54942, .F. ) ;
#31309 = CARTESIAN_POINT ( 'NONE',  ( 0.5836750258453355933, -37.88760409476676472, -29.30109045202428319 ) ) ;
#31310 = VERTEX_POINT ( 'NONE', #17501 ) ;
#31311 = ORIENTED_EDGE ( 'NONE', *, *, #3967, .T. ) ;
#31312 = CARTESIAN_POINT ( 'NONE',  ( -6.017396004339687465, 13.32329839588554954, 13.32495836419629320 ) ) ;
#31313 = CARTESIAN_POINT ( 'NONE',  ( 0.1129192098497455998, -40.71518461128082578, -17.00663193740825463 ) ) ;
#31314 = CARTESIAN_POINT ( 'NONE',  ( 0.8557997880470599172, 44.60232077416710439, -17.48760788519168941 ) ) ;
#31315 = DIRECTION ( 'NONE',  ( -1.000000000000000000, -0.000000000000000000, -0.000000000000000000 ) ) ;
#31316 = CARTESIAN_POINT ( 'NONE',  ( 4.967162193818130511, 36.06913038482799294, 23.56777426397191277 ) ) ;
#31317 = ORIENTED_EDGE ( 'NONE', *, *, #54318, .F. ) ;
#31318 = CARTESIAN_POINT ( 'NONE',  ( 2.706805983486679779, 5.870773205767990888, 43.61548045460686041 ) ) ;
#31319 = ADVANCED_FACE ( 'NONE', ( #6509 ), #25651, .F. ) ;
#31320 = CARTESIAN_POINT ( 'NONE',  ( 5.910764540655177868, 17.94353875551725253, 9.084638429701733742 ) ) ;
#31321 = CARTESIAN_POINT ( 'NONE',  ( 0.5809828226811617480, -44.45562576850614533, 17.82437196699665094 ) ) ;
#31322 = ORIENTED_EDGE ( 'NONE', *, *, #25246, .T. ) ;
#31323 = EDGE_CURVE ( 'NONE', #48040, #37577, #48325, .T. ) ;
#31324 = B_SPLINE_CURVE_WITH_KNOTS ( 'NONE', 3,
 ( #10503, #58701, #786, #59329, #53395, #16432 ),
 .UNSPECIFIED., .F., .F.,
 ( 4, 2, 4 ),
 ( 1.737169676453554432E-17, 0.0002293755540694307222, 0.0004587511081388440429 ),
 .UNSPECIFIED. ) ;
#31325 = ORIENTED_EDGE ( 'NONE', *, *, #61732, .T. ) ;
#31326 = CARTESIAN_POINT ( 'NONE',  ( 0.8753041380234465318, 44.61941359694289133, -20.49990873486825294 ) ) ;
#31327 = CARTESIAN_POINT ( 'NONE',  ( 0.5824936645240095245, -44.41937930270042756, 15.03851460095492598 ) ) ;
#31328 = EDGE_LOOP ( 'NONE', ( #44524, #30322, #35975, #20863 ) ) ;
#31329 = CARTESIAN_POINT ( 'NONE',  ( 0.1103310638050662013, -42.74468893497613919, -5.710544932888772962 ) ) ;
#31330 = CARTESIAN_POINT ( 'NONE',  ( 1.000433927950263868, 9.073595347253974097, -40.91562715060270250 ) ) ;
#31331 = ADVANCED_FACE ( 'NONE', ( #6827 ), #52288, .T. ) ;
#31332 = ADVANCED_FACE ( 'NONE', ( #52225 ), #8289, .T. ) ;
#31333 = ORIENTED_EDGE ( 'NONE', *, *, #19260, .T. ) ;
#31334 = DIRECTION ( 'NONE',  ( 1.000000000000000000, 1.836909530733573776E-16, -1.925929944387235853E-32 ) ) ;
#31335 = VERTEX_POINT ( 'NONE', #18739 ) ;
#31336 = EDGE_CURVE ( 'NONE', #28511, #37598, #50655, .T. ) ;
#31337 = CARTESIAN_POINT ( 'NONE',  ( 4.956653778116991482, 9.917440902361805755, -47.05699031914939212 ) ) ;
#31338 = CARTESIAN_POINT ( 'NONE',  ( 3.660087539127316880, -32.61167949558411294, 35.27260502801121334 ) ) ;
#31339 = CARTESIAN_POINT ( 'NONE',  ( 5.974727161628369032, 14.50236057684825042, 14.52429704002368993 ) ) ;
#31340 = CONICAL_SURFACE ( 'NONE', #12353, 43.92652462719577500, 1.486293639869522343 ) ;
#31341 = SURFACE_STYLE_USAGE ( .BOTH. , #16630 ) ;
#31342 = DIRECTION ( 'NONE',  ( 1.000000000000000000, -0.000000000000000000, -0.000000000000000000 ) ) ;
#31343 = EDGE_CURVE ( 'NONE', #29821, #35268, #51299, .T. ) ;
#31344 = ORIENTED_EDGE ( 'NONE', *, *, #60835, .T. ) ;
#31345 = CARTESIAN_POINT ( 'NONE',  ( 1.092182651088186685, 10.47430941773377455, 40.58386411695983043 ) ) ;
#31346 = CARTESIAN_POINT ( 'NONE',  ( -6.057079549204054558, 0.6257114429644480280, 19.24681054850080031 ) ) ;
#31347 = EDGE_CURVE ( 'NONE', #36264, #32791, #35712, .T. ) ;
#31348 = CARTESIAN_POINT ( 'NONE',  ( 0.6254087463353915632, 46.28445368454755027, -13.11428234126315573 ) ) ;
#31349 = CARTESIAN_POINT ( 'NONE',  ( 0.1092565886968785011, 21.29292791075586777, -37.50119754628587998 ) ) ;
#31350 = B_SPLINE_CURVE_WITH_KNOTS ( 'NONE', 3,
 ( #35822, #39288, #58652, #44920 ),
 .UNSPECIFIED., .F., .F.,
 ( 4, 4 ),
 ( 0.000000000000000000, 0.005004948556313813107 ),
 .UNSPECIFIED. ) ;
#31351 = CARTESIAN_POINT ( 'NONE',  ( 0.5807400328401574052, 11.87003418057308402, -46.40483864045133089 ) ) ;
#31352 = CARTESIAN_POINT ( 'NONE',  ( -4.214292481396491930, -11.25702090725073035, -1.199999999999999956 ) ) ;
#31353 = B_SPLINE_CURVE_WITH_KNOTS ( 'NONE', 3,
 ( #39733, #58782, #9974, #11206, #30293, #6456 ),
 .UNSPECIFIED., .F., .F.,
 ( 4, 2, 4 ),
 ( 1.807478856737577690E-17, 0.0002293319059085095204, 0.0004586638118170009346 ),
 .UNSPECIFIED. ) ;
#31354 = CARTESIAN_POINT ( 'NONE',  ( 0.1119898979215350060, 43.19989880356775558, -8.984990351321133772 ) ) ;
#31355 = CARTESIAN_POINT ( 'NONE',  ( 5.894904586330512508, 5.957793302349664089, -19.21026056637754920 ) ) ;
#31356 = CIRCLE ( 'NONE', #60346, 47.91270532121795611 ) ;
#31357 = CARTESIAN_POINT ( 'NONE',  ( 4.956653778116991482, 8.845409907521601056, -47.27023054223744225 ) ) ;
#31358 = CARTESIAN_POINT ( 'NONE',  ( -6.078726893082806448, -4.288195875146425529, -18.77246434022707788 ) ) ;
#31359 = CARTESIAN_POINT ( 'NONE',  ( -6.078726893082806448, -11.01388439747515235, 15.79520154185357050 ) ) ;
#31360 = ORIENTED_EDGE ( 'NONE', *, *, #53238, .T. ) ;
#31361 = CARTESIAN_POINT ( 'NONE',  ( 0.7764139734771251522, -46.13398389262297883, 8.467349118943408470 ) ) ;
#31362 = DIRECTION ( 'NONE',  ( -1.000000000000000000, -0.000000000000000000, -0.000000000000000000 ) ) ;
#31363 = CARTESIAN_POINT ( 'NONE',  ( 4.956653778116966613, 0.000000000000000000, 0.000000000000000000 ) ) ;
#31364 = EDGE_LOOP ( 'NONE', ( #43851, #59823, #40556, #52844 ) ) ;
#31365 = CARTESIAN_POINT ( 'NONE',  ( 4.962356264823608143, -42.08379584346670299, -0.4355746408611892995 ) ) ;
#31366 = CARTESIAN_POINT ( 'NONE',  ( 0.9788927965476035276, -41.82430862360842383, -2.657784940308306698 ) ) ;
#31367 = EDGE_CURVE ( 'NONE', #57370, #12019, #8383, .T. ) ;
#31368 = CARTESIAN_POINT ( 'NONE',  ( 0.6025881611877910160, -12.24025891548890854, -46.52425620537265161 ) ) ;
#31369 = EDGE_LOOP ( 'NONE', ( #12152, #17520, #14996, #4068 ) ) ;
#31370 = CARTESIAN_POINT ( 'NONE',  ( 2.624215991343608501, -28.09277600149193077, -38.92973006074542042 ) ) ;
#31371 = EDGE_CURVE ( 'NONE', #32449, #55625, #59635, .T. ) ;
#31372 = B_SPLINE_CURVE_WITH_KNOTS ( 'NONE', 3,
 ( #25403, #52979, #1580, #11316 ),
 .UNSPECIFIED., .F., .F.,
 ( 4, 4 ),
 ( 3.127317220692750759E-18, 0.004050076154993002484 ),
 .UNSPECIFIED. ) ;
#31373 = CARTESIAN_POINT ( 'NONE',  ( 0.9756008150404610335, -41.48296819691540804, -10.96816689273740586 ) ) ;
#31374 = DIRECTION ( 'NONE',  ( 0.000000000000000000, 0.000000000000000000, 1.000000000000000000 ) ) ;
#31375 = ORIENTED_EDGE ( 'NONE', *, *, #19531, .T. ) ;
#31376 = CARTESIAN_POINT ( 'NONE',  ( 5.959547316686252039, 20.34955788964376566, -2.682663672454702830 ) ) ;
#31377 = ORIENTED_EDGE ( 'NONE', *, *, #33681, .T. ) ;
#31378 = ORIENTED_EDGE ( 'NONE', *, *, #21279, .T. ) ;
#31379 = CARTESIAN_POINT ( 'NONE',  ( 0.9730545539215883499, -6.101350888304943432, 42.47233286818615028 ) ) ;
#31380 = ORIENTED_EDGE ( 'NONE', *, *, #34105, .T. ) ;
#31381 = DIRECTION ( 'NONE',  ( 0.000000000000000000, 0.000000000000000000, 1.000000000000000000 ) ) ;
#31382 = VECTOR ( 'NONE', #7505, 1000.000000000000114 ) ;
#31383 = ORIENTED_EDGE ( 'NONE', *, *, #29706, .T. ) ;
#31384 = FACE_OUTER_BOUND ( 'NONE', #50259, .T. ) ;
#31385 =( BOUNDED_SURFACE ( )  B_SPLINE_SURFACE ( 3, 1, ( 
 ( #25694, #49494 ),
 ( #21930, #16936 ),
 ( #2174, #20999 ),
 ( #49810, #58883 ) ),
 .UNSPECIFIED., .F., .F., .F. ) 
 B_SPLINE_SURFACE_WITH_KNOTS ( ( 4, 4 ),
 ( 2, 2 ),
 ( 0.000000000000000000, 1.000000000000000000 ),
 ( 0.000000000000000000, 1.000000000000000000 ),
 .UNSPECIFIED. ) 
 GEOMETRIC_REPRESENTATION_ITEM ( )  RATIONAL_B_SPLINE_SURFACE ( (
 ( 1.000000000000000000, 1.000000000000000000),
 ( 0.7211978278499968642, 0.9934217856018975334),
 ( 0.7211978278499968642, 0.9934217856018975334),
 ( 1.000000000000000000, 1.000000000000000000) ) ) 
 REPRESENTATION_ITEM ( '' )  SURFACE ( )  );
#31386 = LINE ( 'NONE', #37039, #43026 ) ;
#31387 = VERTEX_POINT ( 'NONE', #8699 ) ;
#31388 = CARTESIAN_POINT ( 'NONE',  ( 2.618530812446111078, 45.68928551531458027, -11.05513357215843229 ) ) ;
#31389 = CARTESIAN_POINT ( 'NONE',  ( 4.956445790444018229, -5.251077430595369577, -46.79705371022334504 ) ) ;
#31390 = CARTESIAN_POINT ( 'NONE',  ( 0.5817217712918333339, -44.14976367950093561, -15.81244196993600326 ) ) ;
#31391 = CARTESIAN_POINT ( 'NONE',  ( -2.601141883200662974, 14.73012113219607144, 2.412251831840835692 ) ) ;
#31392 = ORIENTED_EDGE ( 'NONE', *, *, #61422, .F. ) ;
#31393 = DIRECTION ( 'NONE',  ( -1.000000000000000000, -0.000000000000000000, -0.000000000000000000 ) ) ;
#31394 = VECTOR ( 'NONE', #25521, 1000.000000000000000 ) ;
#31395 = EDGE_LOOP ( 'NONE', ( #20309, #21200, #59075, #46417 ) ) ;
#31396 = CARTESIAN_POINT ( 'NONE',  ( 0.9756354156337442296, -42.90827993934340157, -0.1303083999671457160 ) ) ;
#31397 = EDGE_CURVE ( 'NONE', #54532, #9438, #33487, .T. ) ;
#31398 = CARTESIAN_POINT ( 'NONE',  ( 0.9757787079277437936, 26.08967489699762154, 34.06559579809977123 ) ) ;
#31399 = CARTESIAN_POINT ( 'NONE',  ( 0.5988103622719985752, -47.77151394450001476, 5.677495780220241706 ) ) ;
#31400 = VERTEX_POINT ( 'NONE', #22812 ) ;
#31401 = CARTESIAN_POINT ( 'NONE',  ( 0.5839254288179553942, -46.24038938821425404, -12.48406597209087820 ) ) ;
#31402 = CARTESIAN_POINT ( 'NONE',  ( -6.079354080745853928, 0.6160181061932726854, -19.24612888195971649 ) ) ;
#31403 = EDGE_CURVE ( 'NONE', #36286, #9581, #42484, .T. ) ;
#31404 = FACE_OUTER_BOUND ( 'NONE', #14132, .T. ) ;
#31405 = CARTESIAN_POINT ( 'NONE',  ( 0.5797568599927133137, -35.19933661194119878, 30.98761060085561070 ) ) ;
#31406 = ADVANCED_FACE ( 'NONE', ( #32847 ), #11082, .F. ) ;
#31407 = VERTEX_POINT ( 'NONE', #22505 ) ;
#31408 = ORIENTED_EDGE ( 'NONE', *, *, #39071, .F. ) ;
#31409 = LINE ( 'NONE', #49573, #1897 ) ;
#31410 = EDGE_CURVE ( 'NONE', #18068, #31400, #55866, .T. ) ;
#31411 = CARTESIAN_POINT ( 'NONE',  ( 0.6067375320500726366, 13.08014790719091103, -46.07640252006464010 ) ) ;
#31412 = DIRECTION ( 'NONE',  ( 0.000000000000000000, 0.000000000000000000, 1.000000000000000000 ) ) ;
#31413 = CARTESIAN_POINT ( 'NONE',  ( 5.895596859100789899, -19.39920506799832722, 5.310275505304355548 ) ) ;
#31414 = CARTESIAN_POINT ( 'NONE',  ( -6.016104459813374383, -14.95258000663140407, 11.46679299034574839 ) ) ;
#31415 = CARTESIAN_POINT ( 'NONE',  ( 0.3676999524040366896, 25.91024933382758277, 35.70167450949220722 ) ) ;
#31416 = CARTESIAN_POINT ( 'NONE',  ( 3.783198216974387851, -42.41041696600773747, -7.325057189010854231 ) ) ;
#31417 = CARTESIAN_POINT ( 'NONE',  ( 5.880360259849739535, -3.184717612777607787, -47.86623372148049071 ) ) ;
#31418 = CARTESIAN_POINT ( 'NONE',  ( 0.5997462898726536595, -42.52950339524503676, 24.55184251941493301 ) ) ;
#31419 = CARTESIAN_POINT ( 'NONE',  ( 5.901764892641307547, -37.25947723020409086, -31.77613607680425289 ) ) ;
#31420 = CARTESIAN_POINT ( 'NONE',  ( 0.7044674535452954967, -20.64605418817902205, 44.55943412196435816 ) ) ;
#31421 = CARTESIAN_POINT ( 'NONE',  ( 1.227938101723756947, 29.74462687941269223, -30.94118573761281965 ) ) ;
#31422 = VECTOR ( 'NONE', #52668, 1000.000000000000114 ) ;
#31423 = CARTESIAN_POINT ( 'NONE',  ( 0.6009453534118440743, -33.70725662590634641, -34.32439302680955961 ) ) ;
#31424 = CARTESIAN_POINT ( 'NONE',  ( 0.9730545539215883499, 42.60426903087353878, 5.099196237955034405 ) ) ;
#31425 = CARTESIAN_POINT ( 'NONE',  ( 0.9791128995231607179, -22.54602046135226345, 35.32724721234943388 ) ) ;
#31426 = LINE ( 'NONE', #45247, #35495 ) ;
#31427 = CARTESIAN_POINT ( 'NONE',  ( 0.6021447746440204973, 17.20494439911720974, 45.99490218830531063 ) ) ;
#31428 = CARTESIAN_POINT ( 'NONE',  ( 0.5997462898726536595, -47.63132954987539591, 11.95023328037892441 ) ) ;
#31430 = ORIENTED_EDGE ( 'NONE', *, *, #10680, .T. ) ;
#31429 = CARTESIAN_POINT ( 'NONE',  ( -6.017396004339686577, -18.68180398134251874, 2.460690056887720800 ) ) ;
#31431 = EDGE_LOOP ( 'NONE', ( #37156, #39415, #4304, #19657, #51303 ) ) ;
#31432 = DIRECTION ( 'NONE',  ( 0.000000000000000000, -0.000000000000000000, 1.000000000000000000 ) ) ;
#31433 = CARTESIAN_POINT ( 'NONE',  ( 5.895881250540457863, 3.340873024792621937, -19.83346286054237950 ) ) ;
#31434 = LINE ( 'NONE', #59933, #48803 ) ;
#31435 = ORIENTED_EDGE ( 'NONE', *, *, #9114, .F. ) ;
#31436 = VERTEX_POINT ( 'NONE', #53751 ) ;
#31437 = CARTESIAN_POINT ( 'NONE',  ( 4.975801465491695552, 0.000000000000000000, 0.000000000000000000 ) ) ;
#31438 = VECTOR ( 'NONE', #4251, 1000.000000000000227 ) ;
#31439 = CARTESIAN_POINT ( 'NONE',  ( 5.901764892641307547, 48.56171591663477471, 6.304856435458333408 ) ) ;
#31440 = B_SPLINE_CURVE_WITH_KNOTS ( 'NONE', 3,
 ( #48546, #38875, #57927, #9718 ),
 .UNSPECIFIED., .F., .F.,
 ( 4, 4 ),
 ( 8.673617379884035472E-19, 0.004444878191957692126 ),
 .UNSPECIFIED. ) ;
#31441 = ORIENTED_EDGE ( 'NONE', *, *, #6161, .T. ) ;
#31442 = EDGE_LOOP ( 'NONE', ( #25428, #22835, #4018, #42279 ) ) ;
#31443 = EDGE_CURVE ( 'NONE', #13518, #48016, #38711, .T. ) ;
#31444 = LINE ( 'NONE', #37098, #39591 ) ;
#31445 = FACE_OUTER_BOUND ( 'NONE', #2147, .T. ) ;
#31446 = CARTESIAN_POINT ( 'NONE',  ( 5.838029081930955932, 25.43272996496320815, -39.80252887295205255 ) ) ;
#31447 = ORIENTED_EDGE ( 'NONE', *, *, #29412, .T. ) ;
#31448 = CARTESIAN_POINT ( 'NONE',  ( 2.624215991343620935, 47.76052319582216654, 4.864192649745549879 ) ) ;
#31449 = CARTESIAN_POINT ( 'NONE',  ( 0.6254311100348637353, -19.04346769887721535, 44.17670535157478184 ) ) ;
#31450 = CIRCLE ( 'NONE', #4456, 2.649999999999985700 ) ;
#31451 = CARTESIAN_POINT ( 'NONE',  ( 0.1100053167205930771, 21.71746606919056077, 37.25683392728340948 ) ) ;
#31452 = ORIENTED_EDGE ( 'NONE', *, *, #55338, .T. ) ;
#31453 = VERTEX_POINT ( 'NONE', #10568 ) ;
#31454 = CARTESIAN_POINT ( 'NONE',  ( 1.154321713695927398, -0.8253077511129642829, 42.90848032340448270 ) ) ;
#31455 = B_SPLINE_CURVE_WITH_KNOTS ( 'NONE', 3,
 ( #33463, #5226, #48462, #5529 ),
 .UNSPECIFIED., .F., .F.,
 ( 4, 4 ),
 ( 6.254634441385500747E-18, 0.004050076154993005953 ),
 .UNSPECIFIED. ) ;
#31456 = ORIENTED_EDGE ( 'NONE', *, *, #4112, .T. ) ;
#31457 = CARTESIAN_POINT ( 'NONE',  ( 0.8551540677456715978, -33.23105123575924580, 34.52115452272916940 ) ) ;
#31458 = CARTESIAN_POINT ( 'NONE',  ( -6.078457390727109555, 9.985927120572020144, 16.46437883979022487 ) ) ;
#31459 = DIRECTION ( 'NONE',  ( 1.000000000000000000, 0.000000000000000000, 0.000000000000000000 ) ) ;
#31460 = CARTESIAN_POINT ( 'NONE',  ( 0.5980894510889457338, -29.84264441023752212, -37.73932204245508615 ) ) ;
#31461 = CARTESIAN_POINT ( 'NONE',  ( 2.281448460670565392, 47.71650330356587233, 4.956513608981339303 ) ) ;
#31462 = VERTEX_POINT ( 'NONE', #4913 ) ;
#31463 = CARTESIAN_POINT ( 'NONE',  ( 0.5835226383429308328, -13.72009239797509217, 44.84419181050082415 ) ) ;
#31464 = CARTESIAN_POINT ( 'NONE',  ( 0.6031356755773454870, 18.40994522247695286, 44.44547243635328471 ) ) ;
#31465 = ADVANCED_FACE ( 'NONE', ( #20582 ), #33461, .F. ) ;
#31466 = CARTESIAN_POINT ( 'NONE',  ( 0.8751705887134423323, 37.60752970653787486, 29.98056538504974000 ) ) ;
#31467 = AXIS2_PLACEMENT_3D ( 'NONE', #59578, #12010, #35186 ) ;
#31468 = EDGE_LOOP ( 'NONE', ( #17939, #20432, #24357, #16289 ) ) ;
#31469 = FACE_OUTER_BOUND ( 'NONE', #52335, .T. ) ;
#31470 = EDGE_CURVE ( 'NONE', #3325, #46104, #48460, .T. ) ;
#31471 = FACE_OUTER_BOUND ( 'NONE', #25668, .T. ) ;
#31472 = CARTESIAN_POINT ( 'NONE',  ( 0.5800708057587400379, 33.42085258735475861, 34.30831467131368129 ) ) ;
#31473 = CARTESIAN_POINT ( 'NONE',  ( -6.016489644550737204, -4.881234076340502881, 18.19999694163062642 ) ) ;
#31474 = ORIENTED_EDGE ( 'NONE', *, *, #202, .F. ) ;
#31475 = CARTESIAN_POINT ( 'NONE',  ( -6.057079549204054558, 15.42772006041544053, -11.52461213391554473 ) ) ;
#31476 = ADVANCED_FACE ( 'NONE', ( #10885 ), #22242, .F. ) ;
#31477 = CARTESIAN_POINT ( 'NONE',  ( 3.238018933889920792, -6.973938193058539348, 11.43554451904465807 ) ) ;
#31478 = FACE_OUTER_BOUND ( 'NONE', #26663, .T. ) ;
#31479 = B_SPLINE_CURVE_WITH_KNOTS ( 'NONE', 3,
 ( #19742, #24423, #57294, #38866, #58224, #923 ),
 .UNSPECIFIED., .F., .F.,
 ( 4, 2, 4 ),
 ( 4.445228907190568179E-18, 0.0002447193893791738822, 0.0004894387787583433192 ),
 .UNSPECIFIED. ) ;
#31480 = CARTESIAN_POINT ( 'NONE',  ( 0.5786265663353153954, 46.07681357296503677, -13.09387673186287060 ) ) ;
#31481 = CARTESIAN_POINT ( 'NONE',  ( 0.5997462898726536595, -43.04230894295751852, 23.64130434225888777 ) ) ;
#31482 = CARTESIAN_POINT ( 'NONE',  ( 0.9730545539215883499, -5.099196237954599198, -42.60426903087358852 ) ) ;
#31483 = CARTESIAN_POINT ( 'NONE',  ( 0.8753041380234530822, 48.93739466471257060, -4.033575498629232037 ) ) ;
#31484 = B_SPLINE_CURVE_WITH_KNOTS ( 'NONE', 3,
 ( #43696, #44314, #15174, #53650, #34279, #29560, #11089, #48670, #5725, #39296, #10781, #29868, #30169, #48983, #6032, #1341, #20478, #6334, #1650 ),
 .UNSPECIFIED., .F., .F.,
 ( 4, 3, 3, 3, 3, 3, 4 ),
 ( 1.734776414728241573E-18, 0.0002612768053151722511, 0.0003919133833142921723, 0.0005225499612322614040, 0.0006531865391693354164, 0.0008112755173415183395, 0.0009693688056799726815 ),
 .UNSPECIFIED. ) ;
#31485 = CARTESIAN_POINT ( 'NONE',  ( 0.6021448801613057400, 41.29830282053138291, -26.57049722475356290 ) ) ;
#31487 = ORIENTED_EDGE ( 'NONE', *, *, #29878, .T. ) ;
#31486 = EDGE_CURVE ( 'NONE', #1744, #3087, #7254, .T. ) ;
#31488 = CARTESIAN_POINT ( 'NONE',  ( 0.5806925824938499181, -46.75147433417400578, -3.677228565731735621 ) ) ;
#31489 = CARTESIAN_POINT ( 'NONE',  ( 3.660176727303410704, -40.62966184289471983, -25.63023984566688185 ) ) ;
#31491 = EDGE_CURVE ( 'NONE', #22425, #13149, #53153, .T. ) ;
#31490 = CARTESIAN_POINT ( 'NONE',  ( 4.962356264823596597, 41.32726869310139506, 7.955655864260913646 ) ) ;
#31492 = CARTESIAN_POINT ( 'NONE',  ( 4.967162193818129623, -38.44485641567058565, -19.45289607368863116 ) ) ;
#31493 = CARTESIAN_POINT ( 'NONE',  ( 5.880360259849752858, 3.090325311464201530, 47.87242051977166568 ) ) ;
#31494 = CARTESIAN_POINT ( 'NONE',  ( 0.9789233960466696693, -31.16971095351161125, 28.01402944788343063 ) ) ;
#31495 = SHAPE_DEFINITION_REPRESENTATION ( #46321, #53251 ) ;
#31496 = CARTESIAN_POINT ( 'NONE',  ( 1.830465331921977468, -13.71215074184886795, 41.86111534480661334 ) ) ;
#31497 = CIRCLE ( 'NONE', #37518, 48.91267123290010943 ) ;
#31498 =( BOUNDED_SURFACE ( )  B_SPLINE_SURFACE ( 3, 1, ( 
 ( #41823, #18006 ),
 ( #56192, #12693 ),
 ( #27082, #23014 ),
 ( #21764, #31790 ) ),
 .UNSPECIFIED., .F., .F., .F. ) 
 B_SPLINE_SURFACE_WITH_KNOTS ( ( 4, 4 ),
 ( 2, 2 ),
 ( 0.000000000000000000, 1.000000000000000000 ),
 ( 0.000000000000000000, 1.000000000000000000 ),
 .UNSPECIFIED. ) 
 GEOMETRIC_REPRESENTATION_ITEM ( )  RATIONAL_B_SPLINE_SURFACE ( (
 ( 1.000000000000000000, 1.000000000000000000),
 ( 0.9953390228620291325, 0.8624445117760984880),
 ( 0.9953390228620291325, 0.8624445117760984880),
 ( 1.000000000000000000, 1.000000000000000000) ) ) 
 REPRESENTATION_ITEM ( '' )  SURFACE ( )  );
#31499 = CARTESIAN_POINT ( 'NONE',  ( 0.5549461598389364703, 36.47739348819886374, -24.79147958016848818 ) ) ;
#31500 = FACE_OUTER_BOUND ( 'NONE', #35422, .T. ) ;
#31502 = ORIENTED_EDGE ( 'NONE', *, *, #55043, .F. ) ;
#31501 = CARTESIAN_POINT ( 'NONE',  ( 4.553261556744875094, 0.000000000000000000, 0.000000000000000000 ) ) ;
#31503 = ORIENTED_EDGE ( 'NONE', *, *, #24821, .T. ) ;
#31504 = CARTESIAN_POINT ( 'NONE',  ( 2.648799415243696664, -2.956030660112017650, 48.94669903094667518 ) ) ;
#31505 = CARTESIAN_POINT ( 'NONE',  ( -2.601141883200665639, -11.02917173973140308, 10.05747474294113175 ) ) ;
#31506 = CARTESIAN_POINT ( 'NONE',  ( 5.981074661064941900, 17.77058762078863552, 10.26976685693829339 ) ) ;
#31507 = CARTESIAN_POINT ( 'NONE',  ( 0.8744876279028263033, 37.95405449045444612, -31.14225101233220627 ) ) ;
#31508 = VERTEX_POINT ( 'NONE', #29352 ) ;
#31509 = CARTESIAN_POINT ( 'NONE',  ( 4.975801465491694664, 36.39623109580467997, -31.15993731089085017 ) ) ;
#31510 = CARTESIAN_POINT ( 'NONE',  ( 0.8753041380234530822, -8.714053517583518982, -48.32394436680091587 ) ) ;
#31511 = DIRECTION ( 'NONE',  ( 0.000000000000000000, 0.000000000000000000, 1.000000000000000000 ) ) ;
#31512 = ORIENTED_EDGE ( 'NONE', *, *, #47864, .T. ) ;
#31513 = VERTEX_POINT ( 'NONE', #10259 ) ;
#31514 = EDGE_CURVE ( 'NONE', #13235, #52485, #57286, .T. ) ;
#31515 = PRESENTATION_LAYER_ASSIGNMENT (  '', '', ( #48506 ) ) ;
#31516 = LINE ( 'NONE', #54684, #56314 ) ;
#31518 = CARTESIAN_POINT ( 'NONE',  ( 0.1081432562775999084, -39.67792926340389670, -16.89351827868208744 ) ) ;
#31517 = CIRCLE ( 'NONE', #28473, 9.499999999999996447 ) ;
#31519 = DIRECTION ( 'NONE',  ( 0.000000000000000000, 0.000000000000000000, -1.000000000000000000 ) ) ;
#31520 = VERTEX_POINT ( 'NONE', #43174 ) ;
#31521 = AXIS2_PLACEMENT_3D ( 'NONE', #23676, #33401, #52478 ) ;
#31522 = B_SPLINE_CURVE_WITH_KNOTS ( 'NONE', 3,
 ( #38039, #37104, #61175, #28902 ),
 .UNSPECIFIED., .F., .F.,
 ( 4, 4 ),
 ( 0.000000000000000000, 0.005013413432710153717 ),
 .UNSPECIFIED. ) ;
#31523 = CARTESIAN_POINT ( 'NONE',  ( 0.1157506346131639274, -42.70450186874222709, -11.10253033976606929 ) ) ;
#31524 = CARTESIAN_POINT ( 'NONE',  ( 3.376099380956838925, 10.22925587767796074, 8.664335394077147257 ) ) ;
#31525 = ORIENTED_EDGE ( 'NONE', *, *, #15588, .T. ) ;
#31526 = CARTESIAN_POINT ( 'NONE',  ( 4.553261556744875094, 0.000000000000000000, 0.000000000000000000 ) ) ;
#31527 = CARTESIAN_POINT ( 'NONE',  ( 0.1158516988532803382, 33.63005810211861046, 28.56503721126445328 ) ) ;
#31528 = ORIENTED_EDGE ( 'NONE', *, *, #13115, .F. ) ;
#31529 = CARTESIAN_POINT ( 'NONE',  ( 0.8753041380234465318, -31.30612550145435335, 37.82941757363136048 ) ) ;
#31530 = CARTESIAN_POINT ( 'NONE',  ( 4.956445790444004018, -47.08764048036452721, -0.5405220916603282744 ) ) ;
#31531 = ORIENTED_EDGE ( 'NONE', *, *, #32909, .T. ) ;
#31532 = FACE_OUTER_BOUND ( 'NONE', #52620, .T. ) ;
#31533 = CARTESIAN_POINT ( 'NONE',  ( 0.5980271706414734822, 44.54819170408481455, 20.67626317151556847 ) ) ;
#31534 = CARTESIAN_POINT ( 'NONE',  ( 0.5806925824938494740, 45.08220210717442455, -12.91578164539189721 ) ) ;
#31535 = CARTESIAN_POINT ( 'NONE',  ( -6.015611763856276717, 7.205255340944613174, 17.41126425312540249 ) ) ;
#31536 = ORIENTED_EDGE ( 'NONE', *, *, #269, .T. ) ;
#31537 = ORIENTED_EDGE ( 'NONE', *, *, #16275, .F. ) ;
#31538 = CARTESIAN_POINT ( 'NONE',  ( 5.974727161628367256, -7.840226266082667372, 18.96851388233644897 ) ) ;
#31539 = CARTESIAN_POINT ( 'NONE',  ( 0.1145239942831223490, 39.89514688507366458, -18.85000625260029139 ) ) ;
#31540 = EDGE_LOOP ( 'NONE', ( #45660, #49571, #34390, #41516 ) ) ;
#31541 = CARTESIAN_POINT ( 'NONE',  ( 5.896278296736517710, 8.471169747519471827, 18.24188210473619165 ) ) ;
#31542 = ORIENTED_EDGE ( 'NONE', *, *, #56374, .F. ) ;
#31543 = CARTESIAN_POINT ( 'NONE',  ( 3.376099380956842921, 0.8831717405837441470, -13.37641175011824046 ) ) ;
#31544 = EDGE_CURVE ( 'NONE', #96, #15197, #21327, .T. ) ;
#31545 = ORIENTED_EDGE ( 'NONE', *, *, #53614, .T. ) ;
#31546 = CARTESIAN_POINT ( 'NONE',  ( 0.6253024248130477636, 10.25657594887568358, 48.02339926767562872 ) ) ;
#31547 = DIRECTION ( 'NONE',  ( -0.000000000000000000, -0.000000000000000000, -1.000000000000000000 ) ) ;
#31548 = CARTESIAN_POINT ( 'NONE',  ( 0.1310142868023671248, -21.00772081177052897, -37.66054729763584419 ) ) ;
#31549 = ORIENTED_EDGE ( 'NONE', *, *, #59487, .F. ) ;
#31550 = FACE_OUTER_BOUND ( 'NONE', #25279, .T. ) ;
#31551 = EDGE_CURVE ( 'NONE', #26377, #9042, #60293, .T. ) ;
#31552 = CARTESIAN_POINT ( 'NONE',  ( 4.962356264823602814, 41.15374796524927348, -8.809348799717806600 ) ) ;
#31553 = CARTESIAN_POINT ( 'NONE',  ( 4.956445790444026223, 7.299064093731650438, -46.52162629890785439 ) ) ;
#31554 = ORIENTED_EDGE ( 'NONE', *, *, #59686, .F. ) ;
#31555 = ADVANCED_FACE ( 'NONE', ( #34381 ), #51306, .F. ) ;
#31556 =( BOUNDED_SURFACE ( )  B_SPLINE_SURFACE ( 3, 1, ( 
 ( #26309, #45442 ),
 ( #50423, #7490 ),
 ( #26615, #9666 ),
 ( #3714, #32569 ) ),
 .UNSPECIFIED., .F., .F., .F. ) 
 B_SPLINE_SURFACE_WITH_KNOTS ( ( 4, 4 ),
 ( 2, 2 ),
 ( 0.000000000000000000, 1.000000000000000000 ),
 ( 0.000000000000000000, 1.000000000000000000 ),
 .UNSPECIFIED. ) 
 GEOMETRIC_REPRESENTATION_ITEM ( )  RATIONAL_B_SPLINE_SURFACE ( (
 ( 1.000000000000000000, 1.000000000000000000),
 ( 0.7269869731126817891, 0.9931720237060910339),
 ( 0.7269869731126817891, 0.9931720237060910339),
 ( 1.000000000000000000, 1.000000000000000000) ) ) 
 REPRESENTATION_ITEM ( '' )  SURFACE ( )  );
#31557 = ORIENTED_EDGE ( 'NONE', *, *, #47041, .T. ) ;
#31558 = CARTESIAN_POINT ( 'NONE',  ( 0.5998501479064708430, 33.64490850298796687, 34.38546660123309096 ) ) ;
#31559 = CARTESIAN_POINT ( 'NONE',  ( 0.5997462898726536595, -2.096122762665173944, 49.06279547180476897 ) ) ;
#31560 = CARTESIAN_POINT ( 'NONE',  ( 0.6016118706126977189, 32.75634973515021642, 36.58650853542129511 ) ) ;
#31561 = B_SPLINE_CURVE_WITH_KNOTS ( 'NONE', 3,
 ( #54054, #30563, #15876, #2048, #7360, #50295 ),
 .UNSPECIFIED., .F., .F.,
 ( 4, 2, 4 ),
 ( 3.496446946337351263E-18, 0.0002450742804987350977, 0.0004901485609974667260 ),
 .UNSPECIFIED. ) ;
#31562 = CARTESIAN_POINT ( 'NONE',  ( 0.3622758884714600280, -36.91764744403305087, -22.26738722580154217 ) ) ;
#31564 = CIRCLE ( 'NONE', #50547, 75.00000000000001421 ) ;
#31563 = CARTESIAN_POINT ( 'NONE',  ( 0.8751705887134423323, -37.60752970653809513, -29.98056538504947710 ) ) ;
#31565 = VERTEX_POINT ( 'NONE', #1147 ) ;
#31566 = CARTESIAN_POINT ( 'NONE',  ( 4.549368137175248350, 13.59764261105693350, 40.71620287708348940 ) ) ;
#31567 = CARTESIAN_POINT ( 'NONE',  ( 4.553261556744873317, -43.82122302957819215, 3.039733214543990591 ) ) ;
#31568 = ORIENTED_EDGE ( 'NONE', *, *, #42189, .T. ) ;
#31569 = CONICAL_SURFACE ( 'NONE', #45574, 42.08604991992415023, 1.569615340895231137 ) ;
#31570 = CARTESIAN_POINT ( 'NONE',  ( 0.9740398440564311811, -30.04629765303410949, 30.63262235044618365 ) ) ;
#31571 = CARTESIAN_POINT ( 'NONE',  ( 1.154321713695929175, 42.90848032340444718, 0.8253077511128138477 ) ) ;
#31573 = EDGE_CURVE ( 'NONE', #39908, #9401, #47562, .T. ) ;
#31572 = DIRECTION ( 'NONE',  ( -1.000000000000000000, -3.135800716341489291E-16, 1.298891185607901956E-16 ) ) ;
#31574 = VECTOR ( 'NONE', #21243, 1000.000000000000114 ) ;
#31575 = CARTESIAN_POINT ( 'NONE',  ( 0.2279481005628793411, -38.06357991528984996, -22.30845963093949891 ) ) ;
#31576 = CARTESIAN_POINT ( 'NONE',  ( 0.6001305935487315502, -47.76436356026972163, 5.760103278697207507 ) ) ;
#31577 = CARTESIAN_POINT ( 'NONE',  ( 4.956445790444004018, -45.55738122058073003, 11.91902120403828036 ) ) ;
#31578 = CARTESIAN_POINT ( 'NONE',  ( -2.708315649062910779, -5.842990691604685871, 13.41752550814500822 ) ) ;
#31579 = FACE_OUTER_BOUND ( 'NONE', #13662, .T. ) ;
#31580 =( BOUNDED_SURFACE ( )  B_SPLINE_SURFACE ( 3, 1, ( 
 ( #29975, #33462 ),
 ( #19666, #9957 ),
 ( #29053, #15583 ),
 ( #53456, #24355 ) ),
 .UNSPECIFIED., .F., .F., .F. ) 
 B_SPLINE_SURFACE_WITH_KNOTS ( ( 4, 4 ),
 ( 2, 2 ),
 ( 0.000000000000000000, 1.000000000000000000 ),
 ( 0.000000000000000000, 1.000000000000000000 ),
 .UNSPECIFIED. ) 
 GEOMETRIC_REPRESENTATION_ITEM ( )  RATIONAL_B_SPLINE_SURFACE ( (
 ( 1.000000000000000000, 1.000000000000000000),
 ( 0.7223157951917476005, 0.9931996967497186413),
 ( 0.7223157951917476005, 0.9931996967497186413),
 ( 1.000000000000000000, 1.000000000000000000) ) ) 
 REPRESENTATION_ITEM ( '' )  SURFACE ( )  );
#31581 = CARTESIAN_POINT ( 'NONE',  ( 0.9749527285493307938, -39.75066842359295549, 16.15611883305632190 ) ) ;
#31582 = CARTESIAN_POINT ( 'NONE',  ( 4.975610109902397937, -46.59897809419034331, -14.86555238512655919 ) ) ;
#31583 = CARTESIAN_POINT ( 'NONE',  ( 0.6021448801613057400, 22.94537434242217699, -43.41717327179489416 ) ) ;
#31584 = CARTESIAN_POINT ( 'NONE',  ( 0.8760168074886960365, 44.77533136581880768, -17.58183840866353975 ) ) ;
#31585 = B_SPLINE_CURVE_WITH_KNOTS ( 'NONE', 3,
 ( #42047, #12916, #26995, #32012 ),
 .UNSPECIFIED., .F., .F.,
 ( 4, 4 ),
 ( 0.000000000000000000, 0.005014147105413698652 ),
 .UNSPECIFIED. ) ;
#31586 = DIRECTION ( 'NONE',  ( -1.000000000000000000, -0.000000000000000000, -0.000000000000000000 ) ) ;
#31587 = CARTESIAN_POINT ( 'NONE',  ( -6.015611763856276717, -14.94556629257433578, 11.47596948473805689 ) ) ;
#31588 = CARTESIAN_POINT ( 'NONE',  ( 1.834102595619085951, 16.42859871478874112, 40.86929029388846857 ) ) ;
#31589 = CARTESIAN_POINT ( 'NONE',  ( 0.8557997880470599172, 37.44587306708097429, 29.88293891557482951 ) ) ;
#31590 = CARTESIAN_POINT ( 'NONE',  ( 0.8557997880470599172, -47.37054680076701629, -7.156447707086194043 ) ) ;
#31591 = ORIENTED_EDGE ( 'NONE', *, *, #14435, .T. ) ;
#31592 = CARTESIAN_POINT ( 'NONE',  ( 0.1102847568649952675, 11.07236323260753252, -41.67876919128912050 ) ) ;
#31593 = CARTESIAN_POINT ( 'NONE',  ( 3.727782113643637096, -33.03100872435383195, -29.01258758810796934 ) ) ;
#31594 = CARTESIAN_POINT ( 'NONE',  ( 0.1139756605157202368, -38.63988289368274565, -21.30527328286372679 ) ) ;
#31595 = B_SPLINE_CURVE_WITH_KNOTS ( 'NONE', 3,
 ( #59141, #1506, #25640, #16250, #35374, #30030, #11560, #25334, #44174, #20039, #39774, #10316, #58828, #586, #49140, #30639 ),
 .UNSPECIFIED., .F., .F.,
 ( 4, 3, 3, 3, 3, 4 ),
 ( 1.962735358247463844E-17, 0.0002612764279487714823, 0.0003919131003184828229, 0.0005225497727000612443, 0.0007837925190632434027, 0.001045051706266712831 ),
 .UNSPECIFIED. ) ;
#31596 = CARTESIAN_POINT ( 'NONE',  ( 0.5809828226811565299, 28.72298383114543796, -38.32755012159114472 ) ) ;
#31597 = ORIENTED_EDGE ( 'NONE', *, *, #48672, .T. ) ;
#31598 = EDGE_CURVE ( 'NONE', #23179, #48312, #20284, .T. ) ;
#31599 = CARTESIAN_POINT ( 'NONE',  ( 2.706805983486679779, -40.14236207468513840, 18.03792893834089028 ) ) ;
#31600 = CARTESIAN_POINT ( 'NONE',  ( -6.078457390727109555, 13.82950465835784648, 13.39922803529989004 ) ) ;
#31601 = ADVANCED_FACE ( 'NONE', ( #2999 ), #31340, .F. ) ;
#31602 = CARTESIAN_POINT ( 'NONE',  ( 4.960156602257182357, -30.22163187094412251, 35.23783291257160499 ) ) ;
#31603 = ORIENTED_EDGE ( 'NONE', *, *, #1079, .T. ) ;
#31604 = EDGE_CURVE ( 'NONE', #35775, #5057, #24313, .T. ) ;
#31605 = CARTESIAN_POINT ( 'NONE',  ( 0.2940133293163009198, -0.6094640175106790236, -44.11200633829074746 ) ) ;
#31606 = ORIENTED_EDGE ( 'NONE', *, *, #56242, .T. ) ;
#31607 = CARTESIAN_POINT ( 'NONE',  ( -6.001507490154111224, -18.84387066167321478, -0.01557731607573140456 ) ) ;
#31608 = CARTESIAN_POINT ( 'NONE',  ( 5.959828726073459926, 14.51699876360180141, 14.51059719297121831 ) ) ;
#31609 = CONICAL_SURFACE ( 'NONE', #7576, 43.08621763946400307, 1.568696531533066763 ) ;
#31610 = ORIENTED_EDGE ( 'NONE', *, *, #25639, .T. ) ;
#31611 = CARTESIAN_POINT ( 'NONE',  ( 0.5807400328401637335, 28.72484455891696697, -38.33001520688919328 ) ) ;
#31612 = ORIENTED_EDGE ( 'NONE', *, *, #22135, .T. ) ;
#31613 = DIRECTION ( 'NONE',  ( 0.000000000000000000, 0.000000000000000000, 1.000000000000000000 ) ) ;
#31614 = CARTESIAN_POINT ( 'NONE',  ( 0.9754292580325137907, 41.60825679387271236, -5.008036888756832283 ) ) ;
#31615 = CIRCLE ( 'NONE', #22630, 5.453125000000000000 ) ;
#31616 = VERTEX_POINT ( 'NONE', #35626 ) ;
#31617 = CARTESIAN_POINT ( 'NONE',  ( 3.407937589446178528, 10.58239600294650451, -8.699069120706665714 ) ) ;
#31618 = ORIENTED_EDGE ( 'NONE', *, *, #46789, .T. ) ;
#31619 = CARTESIAN_POINT ( 'NONE',  ( 2.643462169533613793, -1.382267876918128469, -48.01657676222237114 ) ) ;
#31620 = ORIENTED_EDGE ( 'NONE', *, *, #32544, .F. ) ;
#31621 = EDGE_CURVE ( 'NONE', #58203, #48545, #10323, .T. ) ;
#31622 = ORIENTED_EDGE ( 'NONE', *, *, #11931, .T. ) ;
#31623 = CARTESIAN_POINT ( 'NONE',  ( 1.129531546211701931, 0.000000000000000000, 0.000000000000000000 ) ) ;
#31625 = VECTOR ( 'NONE', #7757, 1000.000000000000000 ) ;
#31624 = LINE ( 'NONE', #60120, #6400 ) ;
#31626 = CARTESIAN_POINT ( 'NONE',  ( 0.8560838555295158248, -44.60403252362548443, 14.52078223488980768 ) ) ;
#31627 = CARTESIAN_POINT ( 'NONE',  ( 5.958863334805807099, -19.82657410201439063, -5.311251202228782553 ) ) ;
#31628 = CARTESIAN_POINT ( 'NONE',  ( 0.5786265663353196143, 33.35675271369539274, 34.37803667029822918 ) ) ;
#31629 = ORIENTED_EDGE ( 'NONE', *, *, #46094, .T. ) ;
#31630 = FACE_OUTER_BOUND ( 'NONE', #19086, .T. ) ;
#31631 = ADVANCED_FACE ( 'NONE', ( #54067, #45031 ), #55305, .F. ) ;
#31632 = DIRECTION ( 'NONE',  ( -1.000000000000000000, -0.000000000000000000, -0.000000000000000000 ) ) ;
#31633 = CARTESIAN_POINT ( 'NONE',  ( 0.5848930533535030563, -46.77916419324618857, 3.314042813373282659 ) ) ;
#31634 = VERTEX_POINT ( 'NONE', #59082 ) ;
#31635 = EDGE_CURVE ( 'NONE', #58429, #22109, #56529, .T. ) ;
#31636 = ORIENTED_EDGE ( 'NONE', *, *, #45193, .F. ) ;
#31637 = B_SPLINE_CURVE_WITH_KNOTS ( 'NONE', 3,
 ( #9263, #28372, #4541, #47807, #42810, #52479 ),
 .UNSPECIFIED., .F., .F.,
 ( 4, 2, 4 ),
 ( 1.511777545972668437E-16, 0.0002445252820015209787, 0.0004890505640028907112 ),
 .UNSPECIFIED. ) ;
#31638 = CARTESIAN_POINT ( 'NONE',  ( 0.1100053167205930632, -21.71746606919081657, -37.25683392728325316 ) ) ;
#31639 = CARTESIAN_POINT ( 'NONE',  ( -6.072942160501519027, -8.893884846139481937, -17.07931423191899967 ) ) ;
#31640 = CARTESIAN_POINT ( 'NONE',  ( 0.9754292589017213855, 40.26172081468631347, -11.63276854130313431 ) ) ;
#31641 = EDGE_LOOP ( 'NONE', ( #37032, #45109, #33306, #56672 ) ) ;
#31642 = CARTESIAN_POINT ( 'NONE',  ( 0.1100247026804066219, -42.73303500775683972, -5.797046384219709303 ) ) ;
#31643 = LINE ( 'NONE', #22249, #14737 ) ;
#31644 = ORIENTED_EDGE ( 'NONE', *, *, #21729, .T. ) ;
#31645 = CARTESIAN_POINT ( 'NONE',  ( 2.500000000000000000, 0.000000000000000000, 0.000000000000000000 ) ) ;
#31646 = VERTEX_POINT ( 'NONE', #15891 ) ;
#31647 = CARTESIAN_POINT ( 'NONE',  ( -6.010958268070873523, -11.45964880703816746, -14.95835081545485679 ) ) ;
#31649 = EDGE_CURVE ( 'NONE', #7712, #31065, #38587, .T. ) ;
#31648 = CARTESIAN_POINT ( 'NONE',  ( 0.9745511491811738036, -34.24777528633303803, 25.84997388131846918 ) ) ;
#31650 = CARTESIAN_POINT ( 'NONE',  ( 3.678748215320119641, -18.11950377857164796, 45.50050985558087291 ) ) ;
#31651 = CARTESIAN_POINT ( 'NONE',  ( 3.678834586032788234, 36.06700467432391832, 33.13281671471128220 ) ) ;
#31652 = ORIENTED_EDGE ( 'NONE', *, *, #44980, .T. ) ;
#31653 = CARTESIAN_POINT ( 'NONE',  ( 0.9762797500689124330, 10.20671408565980975, 40.64662068068264489 ) ) ;
#31654 = CARTESIAN_POINT ( 'NONE',  ( 0.1313383488274146305, 4.995828979989462404, -42.83318330237621296 ) ) ;
#31655 = AXIS2_PLACEMENT_3D ( 'NONE', #12461, #49731, #55034 ) ;
#31656 = FACE_OUTER_BOUND ( 'NONE', #55399, .T. ) ;
#31657 = DIRECTION ( 'NONE',  ( 0.1011922191286468015, 0.9481578383257814879, 0.3012587731655313461 ) ) ;
#31658 = CIRCLE ( 'NONE', #8609, 2.649999999999992806 ) ;
#31659 = VECTOR ( 'NONE', #17381, 1000.000000000000227 ) ;
#31660 = CARTESIAN_POINT ( 'NONE',  ( 0.9772918015221174759, 29.43140870804984743, 29.83503037052932427 ) ) ;
#31661 = CARTESIAN_POINT ( 'NONE',  ( 0.7764146366350225259, 31.96094562988600174, -34.32984748163959665 ) ) ;
#31662 = CARTESIAN_POINT ( 'NONE',  ( 0.5807400328401637335, -44.45848844984455184, 17.82553128098392392 ) ) ;
#31663 = CARTESIAN_POINT ( 'NONE',  ( 5.959828726073459926, 19.82738831247205979, 5.308046411395318742 ) ) ;
#31664 = CARTESIAN_POINT ( 'NONE',  ( 0.1129192098497447394, -40.71518461128108157, 17.00663193740767909 ) ) ;
#31665 = CARTESIAN_POINT ( 'NONE',  ( -6.078457390727109555, -4.289140445936316048, -18.77226105914099108 ) ) ;
#31666 = CARTESIAN_POINT ( 'NONE',  ( 0.5819845079324661441, -29.51613512130358075, -37.72030202710103453 ) ) ;
#31667 = CIRCLE ( 'NONE', #28666, 11.40403086437694569 ) ;
#31668 = ORIENTED_EDGE ( 'NONE', *, *, #32904, .T. ) ;
#31669 = CARTESIAN_POINT ( 'NONE',  ( 4.956445790443995136, 19.33052208089553758, 42.94029536716820417 ) ) ;
#31670 = CARTESIAN_POINT ( 'NONE',  ( 5.895881250540457863, -4.666996818433856831, 19.56391633352149739 ) ) ;
#31671 = CARTESIAN_POINT ( 'NONE',  ( 0.1365634738349414956, -18.44080531820494429, 40.08490138243215029 ) ) ;
#31672 = EDGE_LOOP ( 'NONE', ( #18585, #12845, #26187, #1234 ) ) ;
#31673 = ADVANCED_FACE ( 'NONE', ( #7695 ), #41107, .F. ) ;
#31674 =( BOUNDED_SURFACE ( )  B_SPLINE_SURFACE ( 3, 1, ( 
 ( #58412, #15230 ),
 ( #14932, #24001 ),
 ( #57478, #1101 ),
 ( #20239, #165 ) ),
 .UNSPECIFIED., .F., .F., .F. ) 
 B_SPLINE_SURFACE_WITH_KNOTS ( ( 4, 4 ),
 ( 2, 2 ),
 ( 0.000000000000000000, 1.000000000000000000 ),
 ( 0.000000000000000000, 1.000000000000000000 ),
 .UNSPECIFIED. ) 
 GEOMETRIC_REPRESENTATION_ITEM ( )  RATIONAL_B_SPLINE_SURFACE ( (
 ( 1.000000000000000000, 1.000000000000000000),
 ( 0.7223157951917480446, 0.9931996967497186413),
 ( 0.7223157951917480446, 0.9931996967497186413),
 ( 1.000000000000000000, 1.000000000000000000) ) ) 
 REPRESENTATION_ITEM ( '' )  SURFACE ( )  );
#31675 = CARTESIAN_POINT ( 'NONE',  ( 4.967162193818131399, -14.26841313271251543, -40.65506779172179108 ) ) ;
#31676 = CARTESIAN_POINT ( 'NONE',  ( 2.624215991343608501, -25.21574086439734685, 40.85210347989523427 ) ) ;
#31677 = B_SPLINE_CURVE_WITH_KNOTS ( 'NONE', 3,
 ( #56650, #36968, #32249, #61949, #56031, #38198, #4014, #51329, #52566, #52255, #47271, #41974, #4317, #9351, #37899, #18454 ),
 .UNSPECIFIED., .F., .F.,
 ( 4, 3, 3, 3, 3, 4 ),
 ( 1.868480190406682863E-17, 0.0002612764279487713196, 0.0003919131003184810340, 0.0005225497727000705684, 0.0007837925190632463301, 0.001045051706266716951 ),
 .UNSPECIFIED. ) ;
#31678 = EDGE_CURVE ( 'NONE', #19565, #9646, #31516, .T. ) ;
#31679 = DIRECTION ( 'NONE',  ( 0.000000000000000000, 0.000000000000000000, -1.000000000000000000 ) ) ;
#31680 = VERTEX_POINT ( 'NONE', #7066 ) ;
#31681 = CARTESIAN_POINT ( 'NONE',  ( 5.965394784446458765, 12.50653125158985723, 16.27505370423085296 ) ) ;
#31682 =( BOUNDED_SURFACE ( )  B_SPLINE_SURFACE ( 3, 1, ( 
 ( #27386, #12383 ),
 ( #17689, #56193 ),
 ( #13305, #7645 ),
 ( #26773, #45907 ) ),
 .UNSPECIFIED., .F., .F., .F. ) 
 B_SPLINE_SURFACE_WITH_KNOTS ( ( 4, 4 ),
 ( 2, 2 ),
 ( 0.000000000000000000, 1.000000000000000000 ),
 ( 0.000000000000000000, 1.000000000000000000 ),
 .UNSPECIFIED. ) 
 GEOMETRIC_REPRESENTATION_ITEM ( )  RATIONAL_B_SPLINE_SURFACE ( (
 ( 1.000000000000000000, 1.000000000000000000),
 ( 0.9952954269826590483, 0.8620686068821307169),
 ( 0.9952954269826590483, 0.8620686068821307169),
 ( 1.000000000000000000, 1.000000000000000000) ) ) 
 REPRESENTATION_ITEM ( '' )  SURFACE ( )  );
#31683 = CARTESIAN_POINT ( 'NONE',  ( 0.6001305935487315502, 34.38748867424666855, 33.64689939321954171 ) ) ;
#31684 = EDGE_CURVE ( 'NONE', #14, #27845, #22150, .T. ) ;
#31685 = CARTESIAN_POINT ( 'NONE',  ( 1.112077966505211624, -11.53183610920814672, 42.54464808972942791 ) ) ;
#31686 = ORIENTED_EDGE ( 'NONE', *, *, #57322, .T. ) ;
#31687 = EDGE_CURVE ( 'NONE', #45383, #3021, #37936, .T. ) ;
#31688 = CARTESIAN_POINT ( 'NONE',  ( 0.6030672727741701600, 29.21669544497198245, 38.21927534816993699 ) ) ;
#31689 = EDGE_LOOP ( 'NONE', ( #48137, #52473, #23710, #23635 ) ) ;
#31690 = EDGE_LOOP ( 'NONE', ( #3776, #59614, #34572, #6598 ) ) ;
#31691 = CARTESIAN_POINT ( 'NONE',  ( 0.1139756605157204866, 44.05734318149369244, 2.430171081038008385 ) ) ;
#31692 = VERTEX_POINT ( 'NONE', #30580 ) ;
#31693 = VERTEX_POINT ( 'NONE', #30894 ) ;
#31694 = CARTESIAN_POINT ( 'NONE',  ( 4.298430060108861639, 0.6201974722425471764, 48.94032081561889669 ) ) ;
#31695 = EDGE_CURVE ( 'NONE', #13688, #1749, #61320, .T. ) ;
#31696 = CARTESIAN_POINT ( 'NONE',  ( 0.8560838555295158248, -6.899551485031924614, -46.39794201672231111 ) ) ;
#31697 = AXIS2_PLACEMENT_3D ( 'NONE', #20464, #39595, #48656 ) ;
#31698 = EDGE_CURVE ( 'NONE', #331, #14833, #28289, .T. ) ;
#31699 = ORIENTED_EDGE ( 'NONE', *, *, #59314, .T. ) ;
#31700 = CARTESIAN_POINT ( 'NONE',  ( 5.838029081930957709, 46.28366904854798491, -9.427992233630753560 ) ) ;
#31701 = CARTESIAN_POINT ( 'NONE',  ( 5.838029081930957709, -46.81536740852270384, -6.275861100912842439 ) ) ;
#31702 = B_SPLINE_CURVE_WITH_KNOTS ( 'NONE', 3,
 ( #857, #43494, #34698, #57856, #14984, #19070 ),
 .UNSPECIFIED., .F., .F.,
 ( 4, 2, 4 ),
 ( 1.528339392293451082E-16, 0.0002445252820015200571, 0.0004890505640028873502 ),
 .UNSPECIFIED. ) ;
#31703 = CARTESIAN_POINT ( 'NONE',  ( 3.221118495291108719, -37.36356056591105101, 23.21046663682675870 ) ) ;
#31704 = AXIS2_PLACEMENT_3D ( 'NONE', #30282, #29979, #59709 ) ;
#31705 = CARTESIAN_POINT ( 'NONE',  ( 0.5837800005270550319, -30.27734249767566155, 35.81225753733249206 ) ) ;
#31706 = ORIENTED_EDGE ( 'NONE', *, *, #47859, .T. ) ;
#31707 = CARTESIAN_POINT ( 'NONE',  ( 3.376099380956842921, -8.298464850405602888, 10.52824129466312186 ) ) ;
#31708 = EDGE_LOOP ( 'NONE', ( #36117, #56824, #56346, #5703 ) ) ;
#31709 = CARTESIAN_POINT ( 'NONE',  ( 0.8560838555295158248, -30.97734773434503808, 35.22466126774251194 ) ) ;
#31710 = VERTEX_POINT ( 'NONE', #50009 ) ;
#31711 = CARTESIAN_POINT ( 'NONE',  ( 3.238931869106855377, -7.419701784410841938, -42.34694073502587486 ) ) ;
#31712 = CARTESIAN_POINT ( 'NONE',  ( 0.1064266418746777076, -41.79703894102878081, 10.61815661559926660 ) ) ;
#31713 = ORIENTED_EDGE ( 'NONE', *, *, #25953, .F. ) ;
#31714 = FACE_OUTER_BOUND ( 'NONE', #55794, .T. ) ;
#31715 = CARTESIAN_POINT ( 'NONE',  ( -6.016489644550736315, -4.881234076340246197, -18.19999694163069037 ) ) ;
#31716 = CARTESIAN_POINT ( 'NONE',  ( 5.860006189529234355, -31.81514841426733042, -36.25227510158496358 ) ) ;
#31717 = CARTESIAN_POINT ( 'NONE',  ( 0.6031357023905874470, -41.64046004335399687, -24.09149424676601470 ) ) ;
#31718 = VECTOR ( 'NONE', #12583, 1000.000000000000000 ) ;
#31719 = ORIENTED_EDGE ( 'NONE', *, *, #22325, .F. ) ;
#31720 = B_SPLINE_CURVE_WITH_KNOTS ( 'NONE', 3,
 ( #58656, #43691, #733, #19872 ),
 .UNSPECIFIED., .F., .F.,
 ( 4, 4 ),
 ( 2.303004670188525934E-17, 0.004564976165746189446 ),
 .UNSPECIFIED. ) ;
#31721 = ORIENTED_EDGE ( 'NONE', *, *, #1765, .T. ) ;
#31722 = CARTESIAN_POINT ( 'NONE',  ( 0.5797568665920713737, 21.98355169411229681, -41.42401191958792595 ) ) ;
#31723 = CARTESIAN_POINT ( 'NONE',  ( 0.9756354156337464500, -16.54067710771387922, 39.59221474545856978 ) ) ;
#31725 = ADVANCED_FACE ( 'NONE', ( #26194 ), #22427, .T. ) ;
#31724 = CARTESIAN_POINT ( 'NONE',  ( -6.078075953587585900, -18.27673012847649048, 6.062698248962721692 ) ) ;
#31726 = CONICAL_SURFACE ( 'NONE', #51693, 42.92674063221959813, 1.485477209440487556 ) ;
#31727 = B_SPLINE_CURVE_WITH_KNOTS ( 'NONE', 3,
 ( #25780, #39912, #27323, #31100, #2261, #12318, #41452, #16700, #26395, #60822, #3195, #31723, #46151, #40525, #50814, #17017, #51417, #7581, #36134 ),
 .UNSPECIFIED., .F., .F.,
 ( 4, 3, 3, 3, 3, 3, 4 ),
 ( 3.469446951953614189E-18, 0.0002724573126191747797, 0.0004086839781548505372, 0.0005449106435901899430, 0.0006811373090491522168, 0.0008459866663933644955, 0.001010840725717214884 ),
 .UNSPECIFIED. ) ;
#31728 = EDGE_CURVE ( 'NONE', #33861, #39282, #7943, .T. ) ;
#31729 = CARTESIAN_POINT ( 'NONE',  ( 0.5830081025819935370, 4.422179700680720416, -46.68700419899666798 ) ) ;
#31730 = DIRECTION ( 'NONE',  ( 1.000000000000000000, 0.000000000000000000, 0.000000000000000000 ) ) ;
#31731 = DIRECTION ( 'NONE',  ( 0.8831157194574072999, 0.000000000000000000, -0.4691552259617553511 ) ) ;
#31732 = B_SPLINE_CURVE_WITH_KNOTS ( 'NONE', 3,
 ( #24995, #20599, #20295, #44133 ),
 .UNSPECIFIED., .F., .F.,
 ( 4, 4 ),
 ( 5.051591013050331407E-17, 0.005004948556313863414 ),
 .UNSPECIFIED. ) ;
#31733 = DIRECTION ( 'NONE',  ( 0.000000000000000000, 0.000000000000000000, 1.000000000000000000 ) ) ;
#31734 = CARTESIAN_POINT ( 'NONE',  ( 0.8744876279028306332, 37.95405449045402690, 31.14225101233274273 ) ) ;
#31735 = CARTESIAN_POINT ( 'NONE',  ( 4.335381028904216727, -11.88755795484514444, 47.52307664213822136 ) ) ;
#31736 = CARTESIAN_POINT ( 'NONE',  ( 0.5987334363312689645, 16.39078270287454941, 46.29152350980928077 ) ) ;
#31737 = CARTESIAN_POINT ( 'NONE',  ( 4.975610109902397937, 8.374023221151757568, 48.19050883970187016 ) ) ;
#31738 = CARTESIAN_POINT ( 'NONE',  ( 0.9972139404380304661, 42.62325912566431185, 4.947665363828915197 ) ) ;
#31739 = CARTESIAN_POINT ( 'NONE',  ( 0.9790320750461896093, -22.62273297271198658, 35.27816726231058908 ) ) ;
#31740 = CARTESIAN_POINT ( 'NONE',  ( 0.5997462898726536595, -39.04071682475809268, 29.78882441375220580 ) ) ;
#31741 = VECTOR ( 'NONE', #49171, 1000.000000000000000 ) ;
#31742 = CARTESIAN_POINT ( 'NONE',  ( 4.975801465491695552, 0.000000000000000000, 0.000000000000000000 ) ) ;
#31743 = CARTESIAN_POINT ( 'NONE',  ( 0.6027935024548037868, 46.51312430684505728, -12.28245664247797819 ) ) ;
#31745 = EDGE_LOOP ( 'NONE', ( #1593, #52938, #47716, #2472 ) ) ;
#31744 = CARTESIAN_POINT ( 'NONE',  ( 4.549368137175248350, 42.84816078363930814, -2.596185425821480930 ) ) ;
#31746 = ORIENTED_EDGE ( 'NONE', *, *, #48242, .T. ) ;
#31747 = AXIS2_PLACEMENT_3D ( 'NONE', #34492, #54175, #43917 ) ;
#31748 = CARTESIAN_POINT ( 'NONE',  ( 6.999999999999995559, 54.69470952477936976, 58.44237546506825964 ) ) ;
#31749 = CARTESIAN_POINT ( 'NONE',  ( 3.894904216938897878, 2.001151192542965696, -43.91036012583801806 ) ) ;
#31750 = AXIS2_PLACEMENT_3D ( 'NONE', #53249, #10667, #29446 ) ;
#31751 = FACE_OUTER_BOUND ( 'NONE', #39648, .T. ) ;
#31752 = EDGE_LOOP ( 'NONE', ( #20166, #50608, #35816, #45142 ) ) ;
#31753 = EDGE_CURVE ( 'NONE', #29096, #50421, #55747, .T. ) ;
#31754 = ORIENTED_EDGE ( 'NONE', *, *, #29520, .T. ) ;
#31755 = DIRECTION ( 'NONE',  ( 0.000000000000000000, -1.000000000000000000, 0.000000000000000000 ) ) ;
#31756 = CARTESIAN_POINT ( 'NONE',  ( 0.9762797500689124330, -39.42083772998312696, -14.22400568939859866 ) ) ;
#31757 = B_SPLINE_CURVE_WITH_KNOTS ( 'NONE', 3,
 ( #61198, #56494, #46206, #31466 ),
 .UNSPECIFIED., .F., .F.,
 ( 4, 4 ),
 ( 0.000000000000000000, 0.004445488388166994251 ),
 .UNSPECIFIED. ) ;
#31758 = EDGE_CURVE ( 'NONE', #48507, #41039, #47347, .T. ) ;
#31759 =( BOUNDED_SURFACE ( )  B_SPLINE_SURFACE ( 3, 1, ( 
 ( #53063, #5435 ),
 ( #24573, #27930 ),
 ( #32954, #23526 ),
 ( #61112, #50263 ) ),
 .UNSPECIFIED., .F., .F., .F. ) 
 B_SPLINE_SURFACE_WITH_KNOTS ( ( 4, 4 ),
 ( 2, 2 ),
 ( 0.000000000000000000, 1.000000000000000000 ),
 ( 0.000000000000000000, 1.000000000000000000 ),
 .UNSPECIFIED. ) 
 GEOMETRIC_REPRESENTATION_ITEM ( )  RATIONAL_B_SPLINE_SURFACE ( (
 ( 1.000000000000000000, 1.000000000000000000),
 ( 0.9732289882329797637, 0.9999525324661233672),
 ( 0.9732289882329797637, 0.9999525324661233672),
 ( 1.000000000000000000, 1.000000000000000000) ) ) 
 REPRESENTATION_ITEM ( '' )  SURFACE ( )  );
#31760 = B_SPLINE_CURVE_WITH_KNOTS ( 'NONE', 3,
 ( #41183, #46811, #56172, #3233 ),
 .UNSPECIFIED., .F., .F.,
 ( 4, 4 ),
 ( 2.909219710836648185E-18, 0.004042984057420972825 ),
 .UNSPECIFIED. ) ;
#31761 = ORIENTED_EDGE ( 'NONE', *, *, #9635, .T. ) ;
#31762 = ORIENTED_EDGE ( 'NONE', *, *, #57273, .T. ) ;
#31763 = CARTESIAN_POINT ( 'NONE',  ( 0.5819845079324652559, 47.89381220525411464, -0.4540594263154777988 ) ) ;
#31764 = EDGE_CURVE ( 'NONE', #61173, #22462, #23362, .T. ) ;
#31765 = EDGE_CURVE ( 'NONE', #5485, #17533, #8622, .T. ) ;
#31766 = FACE_OUTER_BOUND ( 'NONE', #52689, .T. ) ;
#31767 = CARTESIAN_POINT ( 'NONE',  ( 0.7242486021783850481, 48.94187082523895782, 3.962920955507279075 ) ) ;
#31768 = EDGE_CURVE ( 'NONE', #48721, #52874, #9247, .T. ) ;
#31769 = MANIFOLD_SOLID_BREP ( 'M5 Clearance Hole2', #11054 ) ;
#31770 = ORIENTED_EDGE ( 'NONE', *, *, #60144, .T. ) ;
#31771 = CARTESIAN_POINT ( 'NONE',  ( 5.974727161628369032, -20.34732802718245281, -2.694421823322846965 ) ) ;
#31772 = DIRECTION ( 'NONE',  ( 0.000000000000000000, 0.000000000000000000, 1.000000000000000000 ) ) ;
#31773 = EDGE_CURVE ( 'NONE', #24092, #26757, #20713, .T. ) ;
#31774 = CARTESIAN_POINT ( 'NONE',  ( 0.1103872315293168010, 0.02583155086974350811, -43.12442619660166088 ) ) ;
#31775 = ORIENTED_EDGE ( 'NONE', *, *, #20383, .F. ) ;
#31776 = VERTEX_POINT ( 'NONE', #51228 ) ;
#31777 = CARTESIAN_POINT ( 'NONE',  ( 0.5786265663353196143, -41.11783955080221631, -24.57327059187441520 ) ) ;
#31778 = B_SPLINE_CURVE_WITH_KNOTS ( 'NONE', 3,
 ( #11706, #30785, #36139, #49905, #12326, #21398, #35826, #59913, #41149, #59598, #16707, #50513, #45532, #12029, #21707, #40848 ),
 .UNSPECIFIED., .F., .F.,
 ( 4, 3, 3, 3, 3, 4 ),
 ( 2.030557555191247372E-17, 0.0002618515315864389952, 0.0003927756766341964734, 0.0005236998216950555047, 0.0007855159896329897903, 0.001047349442285926569 ),
 .UNSPECIFIED. ) ;
#31779 = VERTEX_POINT ( 'NONE', #34307 ) ;
#31780 = CARTESIAN_POINT ( 'NONE',  ( 5.896278296736517710, 14.91306641426042923, -13.49545959714752819 ) ) ;
#31781 = CARTESIAN_POINT ( 'NONE',  ( 1.793429038971303680, -0.3977116370890650399, 41.94332992053986686 ) ) ;
#31782 = CARTESIAN_POINT ( 'NONE',  ( 0.6030672727741701600, 34.07876014368860496, -33.95535904584750853 ) ) ;
#31783 = CARTESIAN_POINT ( 'NONE',  ( 0.5835226383429291674, -38.55970297496715204, 26.69066842602997980 ) ) ;
#31784 = CARTESIAN_POINT ( 'NONE',  ( -6.001507490154111224, 2.444174634178140071, 18.68469198366097572 ) ) ;
#31785 = EDGE_LOOP ( 'NONE', ( #47909, #28146 ) ) ;
#31786 = CARTESIAN_POINT ( 'NONE',  ( 0.9754402186311939005, -30.47320128434239805, -30.20795797590429999 ) ) ;
#31787 = CARTESIAN_POINT ( 'NONE',  ( 4.956445790444035104, 39.12691469764034480, -26.20348443209818967 ) ) ;
#31788 = CARTESIAN_POINT ( 'NONE',  ( 0.1098349054025746507, 39.92296693299707044, -16.30574661324329711 ) ) ;
#31789 = VERTEX_POINT ( 'NONE', #61846 ) ;
#31790 = CARTESIAN_POINT ( 'NONE',  ( 0.5807400328401637335, -18.83234461715150942, -44.04145271122585115 ) ) ;
#31791 = LINE ( 'NONE', #56498, #60651 ) ;
#31792 = CARTESIAN_POINT ( 'NONE',  ( -2.601141883200665639, -1.938888835821155343, -14.79986951130707418 ) ) ;
#31793 = FACE_OUTER_BOUND ( 'NONE', #19586, .T. ) ;
#31794 = AXIS2_PLACEMENT_3D ( 'NONE', #57530, #210, #57220 ) ;
#31795 = ORIENTED_EDGE ( 'NONE', *, *, #13247, .F. ) ;
#31796 = CARTESIAN_POINT ( 'NONE',  ( 0.9762797500689124330, -12.89881610234921006, -39.87411852747946028 ) ) ;
#31797 = AXIS2_PLACEMENT_3D ( 'NONE', #51337, #13157, #41664 ) ;
#31798 = CARTESIAN_POINT ( 'NONE',  ( 5.895881250540457863, -15.78174954617524861, 12.46852288244675222 ) ) ;
#31799 = CARTESIAN_POINT ( 'NONE',  ( 1.231276596079887931, 40.64579686208652731, 10.25650859035686757 ) ) ;
#31800 = PRODUCT ( 'BR-540', 'BR-540', '', ( #7357 ) ) ;
#31801 = DIRECTION ( 'NONE',  ( 0.000000000000000000, 0.000000000000000000, 1.000000000000000000 ) ) ;
#31802 = CARTESIAN_POINT ( 'NONE',  ( 5.895596859100789899, -9.662743138698242973, -17.63971593444825103 ) ) ;
#31803 = CARTESIAN_POINT ( 'NONE',  ( 0.5806925824938511393, 40.62497527030930655, 23.42720099863236882 ) ) ;
#31804 = EDGE_CURVE ( 'NONE', #43662, #4858, #4924, .T. ) ;
#31805 = B_SPLINE_CURVE_WITH_KNOTS ( 'NONE', 3,
 ( #61208, #42754, #43373, #4490, #9216, #33658 ),
 .UNSPECIFIED., .F., .F.,
 ( 4, 2, 4 ),
 ( 8.148123767742043513E-18, 0.0002291978881530196295, 0.0004583957763060310733 ),
 .UNSPECIFIED. ) ;
#31806 = CARTESIAN_POINT ( 'NONE',  ( 0.5809828226811553087, -6.791453954330003207, -47.41188724015886180 ) ) ;
#31807 = CARTESIAN_POINT ( 'NONE',  ( 4.967162193818130511, -8.839793687085512275, 42.16965968614191240 ) ) ;
#31808 = CARTESIAN_POINT ( 'NONE',  ( 4.975610109902397937, 45.55079628452135410, -17.82061629079668919 ) ) ;
#31809 = CARTESIAN_POINT ( 'NONE',  ( 4.549368137175248350, -42.84816078363928682, -2.596185425821792236 ) ) ;
#31810 = EDGE_LOOP ( 'NONE', ( #28452, #41811, #3701, #43762 ) ) ;
#31811 = VECTOR ( 'NONE', #32502, 1000.000000000000000 ) ;
#31812 = CARTESIAN_POINT ( 'NONE',  ( -17.83651567053104969, -12.32233744059949387, -2.099999999999997868 ) ) ;
#31813 = LINE ( 'NONE', #12716, #38417 ) ;
#31814 = CARTESIAN_POINT ( 'NONE',  ( 5.901764892641288895, 35.20706988846465890, 34.03606465660275404 ) ) ;
#31815 = CARTESIAN_POINT ( 'NONE',  ( 0.5809828226811617480, -44.45562576850614533, 17.82437196699665094 ) ) ;
#31816 = CARTESIAN_POINT ( 'NONE',  ( 0.8760168074887090262, 0.8912768426699538837, 48.09529047980637984 ) ) ;
#31817 = CIRCLE ( 'NONE', #25812, 48.35291015139245019 ) ;
#31818 = CARTESIAN_POINT ( 'NONE',  ( 1.114299999999999846, 6.898680348956876061E-16, 5.633200000000004870 ) ) ;
#31819 = APPLICATION_PROTOCOL_DEFINITION ( 'draft international standard', 'automotive_design', 1998, #44793 ) ;
#31820 = CARTESIAN_POINT ( 'NONE',  ( 4.975801465491694664, 2.564218696446817880, 47.84403947906844223 ) ) ;
#31821 = DIRECTION ( 'NONE',  ( -1.000000000000000000, -0.000000000000000000, -0.000000000000000000 ) ) ;
#31822 = VECTOR ( 'NONE', #17253, 1000.000000000000227 ) ;
#31823 = LINE ( 'NONE', #3279, #60420 ) ;
#31825 = ORIENTED_EDGE ( 'NONE', *, *, #57631, .F. ) ;
#31824 = CARTESIAN_POINT ( 'NONE',  ( 0.8551540677456739292, 11.51835730326480345, 46.51172240253124812 ) ) ;
#31826 = ORIENTED_EDGE ( 'NONE', *, *, #34196, .T. ) ;
#31827 = CARTESIAN_POINT ( 'NONE',  ( 2.359973842542475886, -19.18972130672883480, -39.62184360681084883 ) ) ;
#31828 = CARTESIAN_POINT ( 'NONE',  ( 4.303969348037258058, -42.70173985163801689, -22.16169334783882050 ) ) ;
#31829 = CARTESIAN_POINT ( 'NONE',  ( 0.8744876279028263033, -8.712669995482247742, 48.31603700562906312 ) ) ;
#31830 = ORIENTED_EDGE ( 'NONE', *, *, #58968, .T. ) ;
#31831 = DIRECTION ( 'NONE',  ( 0.09722883295013591554, 0.9927043560032293712, -0.07130649069592721878 ) ) ;
#31832 = CARTESIAN_POINT ( 'NONE',  ( 0.1101816497532063094, 5.494186916735715798, -42.77304337559937153 ) ) ;
#31833 = ADVANCED_FACE ( 'NONE', ( #43100 ), #54213, .F. ) ;
#31834 = VERTEX_POINT ( 'NONE', #43727 ) ;
#31835 = VERTEX_POINT ( 'NONE', #5454 ) ;
#31836 = EDGE_CURVE ( 'NONE', #59097, #23973, #28907, .T. ) ;
#31837 = CARTESIAN_POINT ( 'NONE',  ( 0.9787464366903548818, 25.00166030498751724, -33.63407461019966149 ) ) ;
#31838 = VECTOR ( 'NONE', #45572, 1000.000000000000114 ) ;
#31839 = EDGE_CURVE ( 'NONE', #11505, #46408, #24591, .T. ) ;
#31840 = AXIS2_PLACEMENT_3D ( 'NONE', #46022, #46316, #50076 ) ;
#31841 = FACE_OUTER_BOUND ( 'NONE', #50529, .T. ) ;
#31842 = CARTESIAN_POINT ( 'NONE',  ( 0.6028618097248863439, 41.74935807801012544, 23.90242650600291086 ) ) ;
#31843 = ORIENTED_EDGE ( 'NONE', *, *, #13660, .T. ) ;
#31844 = EDGE_CURVE ( 'NONE', #47787, #59402, #19287, .T. ) ;
#31845 = CARTESIAN_POINT ( 'NONE',  ( 0.5806925824938494740, 45.08220210717442455, -12.91578164539189721 ) ) ;
#31846 = CARTESIAN_POINT ( 'NONE',  ( 0.5848930533535030563, 43.10374212188066423, -18.47540249840228199 ) ) ;
#31847 = CARTESIAN_POINT ( 'NONE',  ( -2.601141883200662974, -12.77988133643097868, 7.711683376288982927 ) ) ;
#31848 = FACE_OUTER_BOUND ( 'NONE', #12360, .T. ) ;
#31849 = VERTEX_POINT ( 'NONE', #57770 ) ;
#31850 = CARTESIAN_POINT ( 'NONE',  ( -6.078075953587585900, 12.00179475453301237, -15.05828997320744733 ) ) ;
#31851 = EDGE_CURVE ( 'NONE', #27614, #34543, #31131, .T. ) ;
#31852 = AXIS2_PLACEMENT_3D ( 'NONE', #60212, #17324, #27027 ) ;
#31853 = ORIENTED_EDGE ( 'NONE', *, *, #46006, .F. ) ;
#31854 = CARTESIAN_POINT ( 'NONE',  ( 4.694002226626920127, -44.81211596887070669, -8.376098963038668188 ) ) ;
#31855 = CARTESIAN_POINT ( 'NONE',  ( -6.078075953587585900, 16.77554405305491514, -9.453903742430952661 ) ) ;
#31856 = CARTESIAN_POINT ( 'NONE',  ( 4.553261556744875094, 38.38432632180499837, -21.35844232721162683 ) ) ;
#31857 = EDGE_CURVE ( 'NONE', #25296, #44894, #2714, .T. ) ;
#31858 = ORIENTED_EDGE ( 'NONE', *, *, #25432, .F. ) ;
#31859 = ORIENTED_EDGE ( 'NONE', *, *, #11831, .T. ) ;
#31860 = CARTESIAN_POINT ( 'NONE',  ( 2.528100132419517365, -28.01580866738180831, -31.26288923539745213 ) ) ;
#31861 = CARTESIAN_POINT ( 'NONE',  ( 0.5827359174754830340, 41.29633904010511714, 24.26188383263383130 ) ) ;
#31862 = VERTEX_POINT ( 'NONE', #53080 ) ;
#31863 = CARTESIAN_POINT ( 'NONE',  ( 0.5326698147273822848, 0.000000000000000000, 0.000000000000000000 ) ) ;
#31864 =( GEOMETRIC_REPRESENTATION_CONTEXT ( 3 ) GLOBAL_UNCERTAINTY_ASSIGNED_CONTEXT ( ( #12976 ) ) GLOBAL_UNIT_ASSIGNED_CONTEXT ( ( #29104, #264, #23795 ) ) REPRESENTATION_CONTEXT ( 'NONE', 'WORKASPACE' ) );
#31865 = ORIENTED_EDGE ( 'NONE', *, *, #30404, .T. ) ;
#31866 = CARTESIAN_POINT ( 'NONE',  ( 4.000000000000000000, 0.000000000000000000, 0.000000000000000000 ) ) ;
#31867 = CIRCLE ( 'NONE', #4818, 48.91267123290010943 ) ;
#31868 = VERTEX_POINT ( 'NONE', #18873 ) ;
#31869 = CARTESIAN_POINT ( 'NONE',  ( 4.975610109902397937, -16.35148546628954236, 46.09857188876348744 ) ) ;
#31870 = CARTESIAN_POINT ( 'NONE',  ( 0.6029443199889047422, -48.70424120927577150, -6.279691878037166219 ) ) ;
#31871 = CARTESIAN_POINT ( 'NONE',  ( 0.1103878639767399000, -26.21398130517543024, 34.24245495762976077 ) ) ;
#31872 = ORIENTED_EDGE ( 'NONE', *, *, #58101, .T. ) ;
#31873 = CARTESIAN_POINT ( 'NONE',  ( 0.1152809850208375564, -27.33770535629795262, -34.63517212808380208 ) ) ;
#31874 = CARTESIAN_POINT ( 'NONE',  ( 1.231276596079887264, -0.5545928549379750550, 41.91621640586514985 ) ) ;
#31875 = CARTESIAN_POINT ( 'NONE',  ( 0.5848930533535030563, 43.24595201260119381, 18.14003078584358519 ) ) ;
#31876 = ORIENTED_EDGE ( 'NONE', *, *, #3098, .T. ) ;
#31877 = CARTESIAN_POINT ( 'NONE',  ( 0.1365634738349354727, 29.18960898986780350, 33.08820555185599943 ) ) ;
#31878 = CARTESIAN_POINT ( 'NONE',  ( 4.975610109902397937, -17.43163075979710541, 45.70106843599904778 ) ) ;
#31879 = CARTESIAN_POINT ( 'NONE',  ( 2.618530812446115519, 46.37964111407213608, -7.658699584659897752 ) ) ;
#31880 = ADVANCED_FACE ( 'NONE', ( #8510 ), #42078, .T. ) ;
#31881 = CARTESIAN_POINT ( 'NONE',  ( 0.2279481005628775092, 33.09720086222342417, 29.17325456918634430 ) ) ;
#31882 = EDGE_LOOP ( 'NONE', ( #44744, #43492, #45418, #25015 ) ) ;
#31883 = CARTESIAN_POINT ( 'NONE',  ( 0.1092355843206037486, 37.49628696754459867, -21.30139719602332349 ) ) ;
#31884 = CONICAL_SURFACE ( 'NONE', #24906, 43.92652462719577500, 1.486293639869522343 ) ;
#31885 = EDGE_CURVE ( 'NONE', #26419, #39143, #16164, .T. ) ;
#31886 = PLANE ( 'NONE',  #20805 ) ;
#31887 = ORIENTED_EDGE ( 'NONE', *, *, #58243, .T. ) ;
#31888 = CIRCLE ( 'NONE', #59900, 42.08604991992415023 ) ;
#31889 = CARTESIAN_POINT ( 'NONE',  ( 0.8551540677456715978, 19.17641535420913002, -43.91216198251520098 ) ) ;
#31890 = EDGE_CURVE ( 'NONE', #37253, #30061, #20299, .T. ) ;
#31891 = DIRECTION ( 'NONE',  ( 1.000000000000000000, 0.000000000000000000, 0.000000000000000000 ) ) ;
#31892 = CARTESIAN_POINT ( 'NONE',  ( 0.6028777368367060907, 44.20642035250607904, 21.38532742158998801 ) ) ;
#31893 = CARTESIAN_POINT ( 'NONE',  ( 4.549368137175248350, 0.000000000000000000, 0.000000000000000000 ) ) ;
#31894 = CARTESIAN_POINT ( 'NONE',  ( 5.965394784446460541, -12.50653125159019474, 16.27505370423059716 ) ) ;
#31895 = DIRECTION ( 'NONE',  ( 1.000000000000000000, 0.000000000000000000, 0.000000000000000000 ) ) ;
#31896 = LINE ( 'NONE', #31578, #57602 ) ;
#31897 = CARTESIAN_POINT ( 'NONE',  ( 0.5835871038041859915, 10.73853903563474255, 45.64995325607297616 ) ) ;
#31898 = CARTESIAN_POINT ( 'NONE',  ( 0.9745511491811745808, -39.77127619790150703, 16.10518088436892725 ) ) ;
#31899 = DIRECTION ( 'NONE',  ( -1.626303258728256651E-16, 1.000000000000000000, 0.000000000000000000 ) ) ;
#31900 = CARTESIAN_POINT ( 'NONE',  ( 3.782625744892852637, 18.67351185206663544, -37.66348442730344459 ) ) ;
#31901 = CARTESIAN_POINT ( 'NONE',  ( 0.9754292580325137907, 9.147692842514130618, 40.89800951834966014 ) ) ;
#31902 = B_SPLINE_CURVE_WITH_KNOTS ( 'NONE', 3,
 ( #52198, #4264, #18710, #48743, #5801, #39681, #24951, #1723, #39371, #44087, #34353, #499, #19954, #35280, #25549, #44685, #1416, #15549, #58427 ),
 .UNSPECIFIED., .F., .F.,
 ( 4, 3, 3, 3, 3, 3, 4 ),
 ( 7.807008523764759705E-18, 0.0002732106629380613477, 0.0004098138914053775462, 0.0005464171197651491833, 0.0006830203481512603196, 0.0008196235766963692708, 0.001011968216111142245 ),
 .UNSPECIFIED. ) ;
#31903 = FACE_OUTER_BOUND ( 'NONE', #33246, .T. ) ;
#31904 = CARTESIAN_POINT ( 'NONE',  ( 0.6021447746440204973, -1.835079692253900996, -49.07314562580602058 ) ) ;
#31905 = FACE_OUTER_BOUND ( 'NONE', #37732, .T. ) ;
#31906 = CARTESIAN_POINT ( 'NONE',  ( -2.739355103387248747, -12.87605224490611633, 7.553465796405332000 ) ) ;
#31907 = CARTESIAN_POINT ( 'NONE',  ( 0.1073791018717578927, 26.63563652260167203, -33.91564619577780348 ) ) ;
#31908 = VERTEX_POINT ( 'NONE', #22949 ) ;
#31909 = ADVANCED_FACE ( 'NONE', ( #4110 ), #19317, .T. ) ;
#31910 = CARTESIAN_POINT ( 'NONE',  ( 0.1101816497532062955, 11.03018586750494556, -41.68997876247036771 ) ) ;
#31911 = CARTESIAN_POINT ( 'NONE',  ( -6.015611763856276717, -11.46610900684733281, 14.95313250337425970 ) ) ;
#31912 = CARTESIAN_POINT ( 'NONE',  ( 42.00000000000000711, -18.99999999999998934, 2.326828918379968998E-15 ) ) ;
#31913 = DIRECTION ( 'NONE',  ( 1.000000000000000000, 1.836909530733573776E-16, -1.925929944387235579E-32 ) ) ;
#31914 = EDGE_LOOP ( 'NONE', ( #18659, #15117 ) ) ;
#31915 = ADVANCED_FACE ( 'NONE', ( #36752 ), #52049, .F. ) ;
#31916 = CARTESIAN_POINT ( 'NONE',  ( 0.8551540677456715978, -34.52115452272952467, 33.23105123575887632 ) ) ;
#31917 = CARTESIAN_POINT ( 'NONE',  ( 0.8744876279028306332, 33.66006955981207227, 35.74003032466684004 ) ) ;
#31918 = ORIENTED_EDGE ( 'NONE', *, *, #27036, .F. ) ;
#31919 = CARTESIAN_POINT ( 'NONE',  ( -6.078726893082806448, -6.647148524917478873, -18.07233957617019371 ) ) ;
#31920 = ORIENTED_EDGE ( 'NONE', *, *, #34519, .F. ) ;
#31921 = CARTESIAN_POINT ( 'NONE',  ( 4.956653778116966613, 48.02038484091100656, 2.599733001514495712 ) ) ;
#31923 = CARTESIAN_POINT ( 'NONE',  ( 0.8557997880470690211, -44.60232077416674201, -17.48760788519264153 ) ) ;
#31922 = VECTOR ( 'NONE', #41112, 1000.000000000000114 ) ;
#31924 = ORIENTED_EDGE ( 'NONE', *, *, #4919, .T. ) ;
#31925 = CARTESIAN_POINT ( 'NONE',  ( 2.648799415243708655, 3.327403256649515750, -48.92285611917233012 ) ) ;
#31926 = DIRECTION ( 'NONE',  ( -1.000000000000000000, -0.000000000000000000, -0.000000000000000000 ) ) ;
#31927 = ORIENTED_EDGE ( 'NONE', *, *, #8838, .F. ) ;
#31928 = CARTESIAN_POINT ( 'NONE',  ( 3.376099380956842921, -11.30600709870807208, -7.202956831470656240 ) ) ;
#31929 = CARTESIAN_POINT ( 'NONE',  ( 3.376099380956842921, 10.79965495504287887, 7.942029745857468903 ) ) ;
#31930 = EDGE_CURVE ( 'NONE', #61413, #11680, #13965, .T. ) ;
#31931 = ORIENTED_EDGE ( 'NONE', *, *, #60677, .T. ) ;
#31932 = CARTESIAN_POINT ( 'NONE',  ( 0.9762797500689124330, -27.44172181261435739, 31.67454323498272117 ) ) ;
#31934 = VERTEX_POINT ( 'NONE', #57048 ) ;
#31933 =( BOUNDED_SURFACE ( )  B_SPLINE_SURFACE ( 3, 1, ( 
 ( #30317, #59748 ),
 ( #40372, #25017 ),
 ( #49424, #11863 ),
 ( #40074, #20929 ) ),
 .UNSPECIFIED., .F., .F., .F. ) 
 B_SPLINE_SURFACE_WITH_KNOTS ( ( 4, 4 ),
 ( 2, 2 ),
 ( 0.000000000000000000, 1.000000000000000000 ),
 ( 0.000000000000000000, 1.000000000000000000 ),
 .UNSPECIFIED. ) 
 GEOMETRIC_REPRESENTATION_ITEM ( )  RATIONAL_B_SPLINE_SURFACE ( (
 ( 1.000000000000000000, 1.000000000000000000),
 ( 0.7211978278499968642, 0.9934217856018975334),
 ( 0.7211978278499968642, 0.9934217856018975334),
 ( 1.000000000000000000, 1.000000000000000000) ) ) 
 REPRESENTATION_ITEM ( '' )  SURFACE ( )  );
#31935 = FACE_OUTER_BOUND ( 'NONE', #25323, .T. ) ;
#31936 = VECTOR ( 'NONE', #23392, 1000.000000000000114 ) ;
#31937 = VERTEX_POINT ( 'NONE', #14176 ) ;
#31938 = ORIENTED_EDGE ( 'NONE', *, *, #27305, .T. ) ;
#31939 = CARTESIAN_POINT ( 'NONE',  ( 4.335381028904201628, 12.96255624111893923, -47.24117889469074782 ) ) ;
#31940 = DIRECTION ( 'NONE',  ( 0.09835009131224552170, -0.8579344853044379438, 0.5042575517176537403 ) ) ;
#31941 = CARTESIAN_POINT ( 'NONE',  ( 0.8560838555295158248, 39.88643293834648063, 24.68694597426990001 ) ) ;
#31942 = AXIS2_PLACEMENT_3D ( 'NONE', #2499, #59826, #16303 ) ;
#31943 = DIRECTION ( 'NONE',  ( 0.000000000000000000, 0.000000000000000000, 1.000000000000000000 ) ) ;
#31944 = CARTESIAN_POINT ( 'NONE',  ( 5.960221823109900008, -14.51763960716768409, -14.50993159119805931 ) ) ;
#31945 = EDGE_LOOP ( 'NONE', ( #10212, #43967, #48458, #2561 ) ) ;
#31946 = CARTESIAN_POINT ( 'NONE',  ( 4.960156602257182357, -38.31207700265973415, 26.21519897043416236 ) ) ;
#31947 = CARTESIAN_POINT ( 'NONE',  ( 0.9787284016396619046, -17.47079291802099377, 38.09340354634191783 ) ) ;
#31948 = CARTESIAN_POINT ( 'NONE',  ( 0.5804410086790514622, -46.75463715370018036, 3.677466040799790559 ) ) ;
#31949 = B_SPLINE_CURVE_WITH_KNOTS ( 'NONE', 3,
 ( #17941, #23245, #46148, #22628, #13237, #13865, #47071, #60821, #55818, #18544, #37673, #32037, #61735, #19710, #38836, #12631, #50813, #37058, #56122 ),
 .UNSPECIFIED., .F., .F.,
 ( 4, 3, 3, 3, 3, 3, 4 ),
 ( 8.240649770922408386E-18, 0.0002732106629380604804, 0.0004098138914053759199, 0.0005464171197651462560, 0.0006830203481512570670, 0.0008196235766963637414, 0.001011968216111141811 ),
 .UNSPECIFIED. ) ;
#31950 = EDGE_LOOP ( 'NONE', ( #22431, #34715, #23736, #36492 ) ) ;
#31951 = EDGE_LOOP ( 'NONE', ( #44326, #6595, #28083, #27674 ) ) ;
#31952 =( BOUNDED_SURFACE ( )  B_SPLINE_SURFACE ( 3, 1, ( 
 ( #28798, #52596 ),
 ( #58211, #38231 ),
 ( #9687, #15337 ),
 ( #44175, #5278 ) ),
 .UNSPECIFIED., .F., .F., .F. ) 
 B_SPLINE_SURFACE_WITH_KNOTS ( ( 4, 4 ),
 ( 2, 2 ),
 ( 0.000000000000000000, 1.000000000000000000 ),
 ( 0.000000000000000000, 1.000000000000000000 ),
 .UNSPECIFIED. ) 
 GEOMETRIC_REPRESENTATION_ITEM ( )  RATIONAL_B_SPLINE_SURFACE ( (
 ( 1.000000000000000000, 1.000000000000000000),
 ( 0.7211978278499970862, 0.9934217856018976445),
 ( 0.7211978278499970862, 0.9934217856018976445),
 ( 1.000000000000000000, 1.000000000000000000) ) ) 
 REPRESENTATION_ITEM ( '' )  SURFACE ( )  );
#31953 = CARTESIAN_POINT ( 'NONE',  ( 0.2885697896453123246, -33.71073718007520625, -26.88157175352875683 ) ) ;
#31954 = CARTESIAN_POINT ( 'NONE',  ( -6.015611763856276717, 2.453375430804336954, -18.68284711750055749 ) ) ;
#31955 = CARTESIAN_POINT ( 'NONE',  ( 1.157644175074338255, 40.20129498541808744, 11.86836791536983426 ) ) ;
#31957 = VERTEX_POINT ( 'NONE', #51421 ) ;
#31956 = ADVANCED_FACE ( 'NONE', ( #56435 ), #47484, .F. ) ;
#31958 = CARTESIAN_POINT ( 'NONE',  ( 4.834790513006555379, 18.70372717509382454, -43.39078163255459941 ) ) ;
#31959 = CARTESIAN_POINT ( 'NONE',  ( 1.092182651088184686, 8.955214945688501516, -40.94588269556293625 ) ) ;
#31960 = ORIENTED_EDGE ( 'NONE', *, *, #57434, .T. ) ;
#31961 = DIRECTION ( 'NONE',  ( 0.09722883295013594329, 0.7529176304110362095, -0.6508929219613506234 ) ) ;
#31962 = CARTESIAN_POINT ( 'NONE',  ( 0.1073791018717578927, 40.02496097243057704, -16.05399293000775529 ) ) ;
#31963 = FACE_OUTER_BOUND ( 'NONE', #51625, .T. ) ;
#31964 = B_SPLINE_CURVE_WITH_KNOTS ( 'NONE', 3,
 ( #48098, #61852, #52160, #5150, #33088, #3921 ),
 .UNSPECIFIED., .F., .F.,
 ( 4, 2, 4 ),
 ( 0.000000000000000000, 0.0002447195606305749629, 0.0004894391212611499259 ),
 .UNSPECIFIED. ) ;
#31965 = CARTESIAN_POINT ( 'NONE',  ( 1.227938101723756947, -0.8460948827222184443, -42.91134962331487657 ) ) ;
#31966 = CARTESIAN_POINT ( 'NONE',  ( 2.185380717157383579, -43.46326555698310301, 7.054385174511375034 ) ) ;
#31967 = EDGE_CURVE ( 'NONE', #5629, #25496, #9490, .T. ) ;
#31968 = CARTESIAN_POINT ( 'NONE',  ( 0.1313383488274141586, 39.59253935480796827, -17.09007684155463735 ) ) ;
#31969 = AXIS2_PLACEMENT_3D ( 'NONE', #49159, #53835, #30661 ) ;
#31970 = ORIENTED_EDGE ( 'NONE', *, *, #2227, .T. ) ;
#31971 = CARTESIAN_POINT ( 'NONE',  ( 0.2940133293163019190, 21.11549836636102739, -38.73469088966953677 ) ) ;
#31972 = CARTESIAN_POINT ( 'NONE',  ( -48.95476116535499500, 0.000000000000000000, 0.000000000000000000 ) ) ;
#31973 = EDGE_CURVE ( 'NONE', #23427, #41881, #36324, .T. ) ;
#31974 = CARTESIAN_POINT ( 'NONE',  ( 1.227938101723748288, -17.20315230597871903, 39.32113113558960293 ) ) ;
#31975 = CARTESIAN_POINT ( 'NONE',  ( 0.1098349054025746507, 21.74670956129760668, -37.23978094195829414 ) ) ;
#31976 = AXIS2_PLACEMENT_3D ( 'NONE', #24057, #57536, #58465 ) ;
#31977 = CARTESIAN_POINT ( 'NONE',  ( 0.5804410086790514622, -46.06497594411302998, -8.805557513507348943 ) ) ;
#31978 = CARTESIAN_POINT ( 'NONE',  ( 0.8744876279028306332, 33.66006955981207227, 35.74003032466684004 ) ) ;
#31979 = B_SPLINE_CURVE_WITH_KNOTS ( 'NONE', 3,
 ( #56446, #8849, #19194, #52362, #9455, #23876 ),
 .UNSPECIFIED., .F., .F.,
 ( 4, 2, 4 ),
 ( 9.543442895606953578E-18, 0.0002291978881530156180, 0.0004583957763060216950 ),
 .UNSPECIFIED. ) ;
#31980 = FACE_OUTER_BOUND ( 'NONE', #49564, .T. ) ;
#31981 = CARTESIAN_POINT ( 'NONE',  ( 0.5806925824938502512, 37.13995815321093374, 28.63295078613632683 ) ) ;
#31982 = ADVANCED_FACE ( 'NONE', ( #28247 ), #53856, .F. ) ;
#31983 = DIRECTION ( 'NONE',  ( -1.000000000000000000, -5.380183451256670742E-17, 1.298891185607911324E-16 ) ) ;
#31984 = DIRECTION ( 'NONE',  ( -0.07906939808003032866, 0.9145849808368812228, -0.3965883799544098753 ) ) ;
#31985 = ORIENTED_EDGE ( 'NONE', *, *, #48783, .F. ) ;
#31986 = CIRCLE ( 'NONE', #50970, 6.887500000000022382 ) ;
#31987 = CARTESIAN_POINT ( 'NONE',  ( 0.5987334308729320709, 46.41165616633498558, -16.04746330320246273 ) ) ;
#31988 = CARTESIAN_POINT ( 'NONE',  ( 0.5832366564991503521, 46.33368520589916528, 12.13301812590366247 ) ) ;
#31989 = CARTESIAN_POINT ( 'NONE',  ( 0.000000000000000000, 0.000000000000000000, -5.599999999999999645 ) ) ;
#31990 = VERTEX_POINT ( 'NONE', #13549 ) ;
#31991 = EDGE_CURVE ( 'NONE', #6142, #55166, #12513, .T. ) ;
#31992 = CARTESIAN_POINT ( 'NONE',  ( 2.643462169533600914, -11.09243630552500903, -46.73820883660201986 ) ) ;
#31993 = DIRECTION ( 'NONE',  ( 1.000000000000000000, 1.836970198721027962E-16, -2.033782021272921061E-31 ) ) ;
#31994 = B_SPLINE_CURVE_WITH_KNOTS ( 'NONE', 3,
 ( #27239, #3405, #12855, #55110, #61047, #3712 ),
 .UNSPECIFIED., .F., .F.,
 ( 4, 2, 4 ),
 ( 5.898697549827395015E-18, 0.0002291472222819930982, 0.0004582944445639802874 ),
 .UNSPECIFIED. ) ;
#31995 = B_SPLINE_CURVE_WITH_KNOTS ( 'NONE', 3,
 ( #58165, #52549, #5841, #33788 ),
 .UNSPECIFIED., .F., .F.,
 ( 4, 4 ),
 ( 0.000000000000000000, 0.004442905043737213969 ),
 .UNSPECIFIED. ) ;
#31996 = ADVANCED_FACE ( 'NONE', ( #45298 ), #58729, .T. ) ;
#31997 = ORIENTED_EDGE ( 'NONE', *, *, #1896, .T. ) ;
#31999 = CARTESIAN_POINT ( 'NONE',  ( -6.079354080745853928, 19.25598488485689330, -0.001167186744193668890 ) ) ;
#31998 = B_SPLINE_CURVE_WITH_KNOTS ( 'NONE', 3,
 ( #47020, #27276, #17892, #32920, #3751, #51686 ),
 .UNSPECIFIED., .F., .F.,
 ( 4, 2, 4 ),
 ( 1.867239236438689166E-17, 0.0002293755540694309119, 0.0004587511081388431214 ),
 .UNSPECIFIED. ) ;
#32000 = CARTESIAN_POINT ( 'NONE',  ( 4.291220156522059348, 44.16776250362676848, -16.38895215469610989 ) ) ;
#32001 = CARTESIAN_POINT ( 'NONE',  ( -6.077587904424778920, -19.21610359950805247, 1.239912838430311970 ) ) ;
#32002 = ORIENTED_EDGE ( 'NONE', *, *, #3684, .T. ) ;
#32003 = ORIENTED_EDGE ( 'NONE', *, *, #12676, .T. ) ;
#32004 = EDGE_LOOP ( 'NONE', ( #16831, #61338, #24872, #10002 ) ) ;
#32005 = CARTESIAN_POINT ( 'NONE',  ( 0.1158516988532803799, 44.03663622717940740, 2.777918038363759390 ) ) ;
#32006 = ORIENTED_EDGE ( 'NONE', *, *, #25181, .F. ) ;
#32007 = CARTESIAN_POINT ( 'NONE',  ( -6.078075953587585900, 19.25604180663921738, -0.005309246513132053445 ) ) ;
#32008 = EDGE_CURVE ( 'NONE', #59505, #40325, #23708, .T. ) ;
#32009 = B_SPLINE_CURVE_WITH_KNOTS ( 'NONE', 3,
 ( #59498, #48566, #11287, #53864, #44215, #39826, #44522, #30375, #53556, #49490, #6544, #34794, #58879, #10990, #15997, #30073 ),
 .UNSPECIFIED., .F., .F.,
 ( 4, 3, 3, 3, 3, 4 ),
 ( 1.868480190406682863E-17, 0.0002618515315864419226, 0.0003927756766341999970, 0.0005236998216950594079, 0.0007855159896329896819, 0.001047349442285925702 ),
 .UNSPECIFIED. ) ;
#32010 = ORIENTED_EDGE ( 'NONE', *, *, #22204, .T. ) ;
#32011 = CARTESIAN_POINT ( 'NONE',  ( 2.301529144917016101, 28.20894756932140979, -38.87759814529788827 ) ) ;
#32012 = CARTESIAN_POINT ( 'NONE',  ( 4.549368137175248350, 42.84816078363930814, -2.596185425821480930 ) ) ;
#32013 = ORIENTED_EDGE ( 'NONE', *, *, #32537, .T. ) ;
#32014 = CARTESIAN_POINT ( 'NONE',  ( 4.000000000000000000, 0.000000000000000000, -5.600000000000000533 ) ) ;
#32015 = CIRCLE ( 'NONE', #26020, 0.7500000000000015543 ) ;
#32016 = CARTESIAN_POINT ( 'NONE',  ( 49.16300155221411217, 12.28471438860442078, -2.313890179308903505 ) ) ;
#32017 = CARTESIAN_POINT ( 'NONE',  ( 2.533389852662419894, -37.55112757475649943, 22.96439308142020153 ) ) ;
#32018 = CARTESIAN_POINT ( 'NONE',  ( 4.999999999999997335, 8.388739760877188892E-13, -80.00000000000001421 ) ) ;
#32019 = ORIENTED_EDGE ( 'NONE', *, *, #4685, .T. ) ;
#32020 = CARTESIAN_POINT ( 'NONE',  ( 2.000000000000027089, 3.464101615137739731, 0.000000000000000000 ) ) ;
#32021 = ORIENTED_EDGE ( 'NONE', *, *, #20307, .T. ) ;
#32022 = CARTESIAN_POINT ( 'NONE',  ( 0.9752132459055870006, -42.90780255730422255, 0.2329632697542413367 ) ) ;
#32023 = ORIENTED_EDGE ( 'NONE', *, *, #22606, .F. ) ;
#32024 = CARTESIAN_POINT ( 'NONE',  ( 0.5797568665920713737, -25.76189042052133615, -39.18609843506905577 ) ) ;
#32025 = CARTESIAN_POINT ( 'NONE',  ( 0.2224561200757598778, -41.44719785461225570, -11.89200283918776435 ) ) ;
#32026 = EDGE_LOOP ( 'NONE', ( #10012, #46442, #60191, #5411 ) ) ;
#32027 = CARTESIAN_POINT ( 'NONE',  ( 5.000000000000007994, -56.56854249492410958, 56.56854249492351983 ) ) ;
#32028 = CARTESIAN_POINT ( 'NONE',  ( 4.335381028904216727, -17.86707742387240216, 45.61276566920378883 ) ) ;
#32029 = CARTESIAN_POINT ( 'NONE',  ( 1.296416391601052265, 8.720348633736866972, -43.20026497351888395 ) ) ;
#32030 = CARTESIAN_POINT ( 'NONE',  ( 0.5835226383429256147, -1.749062421197752570, -46.86345329990871278 ) ) ;
#32031 =( BOUNDED_SURFACE ( )  B_SPLINE_SURFACE ( 3, 1, ( 
 ( #29131, #52618 ),
 ( #47942, #15671 ),
 ( #10969, #4991 ),
 ( #48855, #25053 ) ),
 .UNSPECIFIED., .F., .F., .F. ) 
 B_SPLINE_SURFACE_WITH_KNOTS ( ( 4, 4 ),
 ( 2, 2 ),
 ( 0.000000000000000000, 1.000000000000000000 ),
 ( 0.000000000000000000, 1.000000000000000000 ),
 .UNSPECIFIED. ) 
 GEOMETRIC_REPRESENTATION_ITEM ( )  RATIONAL_B_SPLINE_SURFACE ( (
 ( 1.000000000000000000, 1.000000000000000000),
 ( 0.9953040768229005630, 0.8617119497784937465),
 ( 0.9953040768229005630, 0.8617119497784937465),
 ( 1.000000000000000000, 1.000000000000000000) ) ) 
 REPRESENTATION_ITEM ( '' )  SURFACE ( )  );
#32032 = EDGE_CURVE ( 'NONE', #24292, #4853, #14725, .T. ) ;
#32033 = CONICAL_SURFACE ( 'NONE', #22013, 42.92674063221959813, 1.485477209440487556 ) ;
#32034 = EDGE_LOOP ( 'NONE', ( #48438, #8471, #42058, #28506 ) ) ;
#32035 = ORIENTED_EDGE ( 'NONE', *, *, #28488, .F. ) ;
#32036 = CARTESIAN_POINT ( 'NONE',  ( -4.915099999999999802, 0.000000000000000000, 0.000000000000000000 ) ) ;
#32037 = CARTESIAN_POINT ( 'NONE',  ( 0.9789233960466703355, -41.82366163528425318, 2.667968187515405543 ) ) ;
#32038 = EDGE_CURVE ( 'NONE', #49001, #39397, #8713, .T. ) ;
#32039 = CARTESIAN_POINT ( 'NONE',  ( 0.8744876279028306332, -49.08725279547490317, 0.8897546699139438076 ) ) ;
#32040 = LINE ( 'NONE', #42076, #15787 ) ;
#32041 = B_SPLINE_CURVE_WITH_KNOTS ( 'NONE', 3,
 ( #36292, #44772, #17176, #54425, #35369, #7751, #59445, #11237, #21252, #40383, #40087, #26874, #35990, #2115, #11877, #46014 ),
 .UNSPECIFIED., .F., .F.,
 ( 4, 3, 3, 3, 3, 4 ),
 ( 8.674294979774126656E-18, 0.0002732102107931834944, 0.0004098135523333795282, 0.0005464168938825003348, 0.0008195847345945455036, 0.001092771384553109602 ),
 .UNSPECIFIED. ) ;
#32042 = EDGE_CURVE ( 'NONE', #9806, #31849, #45358, .T. ) ;
#32043 = CARTESIAN_POINT ( 'NONE',  ( 0.8753041380234530822, -26.21158409634513120, -41.52217705074249210 ) ) ;
#32044 = PLANE ( 'NONE',  #39853 ) ;
#32045 = CARTESIAN_POINT ( 'NONE',  ( 0.5806925824938502512, 4.150136846023314341, -46.71186922509998141 ) ) ;
#32046 = CARTESIAN_POINT ( 'NONE',  ( 1.091591847532195958, -13.16112942808253017, 39.79376412370536542 ) ) ;
#32047 = EDGE_CURVE ( 'NONE', #35054, #19605, #57284, .T. ) ;
#32048 = CARTESIAN_POINT ( 'NONE',  ( 4.833616638992205949, -43.64812679991108979, -15.29495699393711838 ) ) ;
#32049 = LINE ( 'NONE', #51125, #39234 ) ;
#32050 = CARTESIAN_POINT ( 'NONE',  ( 0.9772918015221172539, 33.14542697680284533, 25.64600409958848815 ) ) ;
#32051 = CARTESIAN_POINT ( 'NONE',  ( 0.5807400328401637335, -11.87003418057209636, -46.40483864045158668 ) ) ;
#32052 = FACE_OUTER_BOUND ( 'NONE', #8253, .T. ) ;
#32053 = CARTESIAN_POINT ( 'NONE',  ( 4.553261556744875094, 0.000000000000000000, 0.000000000000000000 ) ) ;
#32054 = CARTESIAN_POINT ( 'NONE',  ( 0.5980894510889457338, -38.59343625445427506, -28.72954109785590049 ) ) ;
#32055 = CARTESIAN_POINT ( 'NONE',  ( 4.553261556744873317, -15.38244134641770167, -41.14510984366982171 ) ) ;
#32056 = CARTESIAN_POINT ( 'NONE',  ( 5.960721111146673579, 10.26825948882926021, -17.77250458025982027 ) ) ;
#32057 = EDGE_CURVE ( 'NONE', #29670, #7691, #37390, .T. ) ;
#32058 = CARTESIAN_POINT ( 'NONE',  ( 0.7764139734771232648, -13.04263755106484624, -45.05474532852694125 ) ) ;
#32059 = CIRCLE ( 'NONE', #52063, 8.000000000000000000 ) ;
#32060 = CARTESIAN_POINT ( 'NONE',  ( 0.6024113833632039894, -47.55614101750226297, 12.24562455019367668 ) ) ;
#32062 = ORIENTED_EDGE ( 'NONE', *, *, #50356, .F. ) ;
#32061 = CARTESIAN_POINT ( 'NONE',  ( 0.9762797500689124330, 25.26481495167912783, -33.43671500974812716 ) ) ;
#32063 = EDGE_LOOP ( 'NONE', ( #49535, #3905, #42425, #46984 ) ) ;
#32064 = CARTESIAN_POINT ( 'NONE',  ( 0.6845945791218034371, 43.51705215793874260, -17.51207275559303511 ) ) ;
#32065 = CARTESIAN_POINT ( 'NONE',  ( 4.956653778116966613, 0.000000000000000000, 0.000000000000000000 ) ) ;
#32067 = EDGE_CURVE ( 'NONE', #6622, #56918, #55375, .T. ) ;
#32066 = CARTESIAN_POINT ( 'NONE',  ( 0.1073791018717578927, -0.4849339620936172768, 43.12183934961190346 ) ) ;
#32068 = EDGE_LOOP ( 'NONE', ( #16612, #40067, #53412 ) ) ;
#32069 = ORIENTED_EDGE ( 'NONE', *, *, #15091, .T. ) ;
#32070 = CARTESIAN_POINT ( 'NONE',  ( 1.834102595619085285, -30.72137182784087273, 31.56572599946387570 ) ) ;
#32071 = CARTESIAN_POINT ( 'NONE',  ( 0.5998501479064699549, 6.798102206413494386, 47.62484632993690781 ) ) ;
#32072 = B_SPLINE_CURVE_WITH_KNOTS ( 'NONE', 3,
 ( #25527, #12615, #37046, #12303, #56109, #27615 ),
 .UNSPECIFIED., .F., .F.,
 ( 4, 2, 4 ),
 ( 9.929776742050823831E-18, 0.0002448709889506581324, 0.0004897419779013063986 ),
 .UNSPECIFIED. ) ;
#32073 = EDGE_CURVE ( 'NONE', #46288, #36503, #54179, .T. ) ;
#32074 = ORIENTED_EDGE ( 'NONE', *, *, #9405, .F. ) ;
#32075 = VERTEX_POINT ( 'NONE', #7340 ) ;
#32076 = DIRECTION ( 'NONE',  ( -1.826024711554534160E-16, 1.000000000000000000, 0.000000000000000000 ) ) ;
#32077 = CIRCLE ( 'NONE', #56016, 15.50000000000000000 ) ;
#32078 = CARTESIAN_POINT ( 'NONE',  ( 3.407937589446178528, 11.14158115674373484, 7.970324840161996605 ) ) ;
#32079 = CARTESIAN_POINT ( 'NONE',  ( 0.9758171775293928984, -41.44488232057073418, 11.11125068417978135 ) ) ;
#32080 = ORIENTED_EDGE ( 'NONE', *, *, #47739, .T. ) ;
#32081 = CARTESIAN_POINT ( 'NONE',  ( 5.960721111146673579, -20.34914600876573587, -2.685391721745965299 ) ) ;
#32082 = ADVANCED_FACE ( 'NONE', ( #12705 ), #32671, .F. ) ;
#32083 = CARTESIAN_POINT ( 'NONE',  ( 3.661921753702005677, -41.09997312006429127, 22.87844691765657146 ) ) ;
#32084 = EDGE_CURVE ( 'NONE', #38640, #16773, #57173, .T. ) ;
#32085 = FACE_OUTER_BOUND ( 'NONE', #55916, .T. ) ;
#32086 = EDGE_LOOP ( 'NONE', ( #52526, #1114, #42280, #8636 ) ) ;
#32087 = ORIENTED_EDGE ( 'NONE', *, *, #29580, .F. ) ;
#32088 = CARTESIAN_POINT ( 'NONE',  ( 1.088908134280559104, -29.78762923589991019, 30.89124834763379113 ) ) ;
#32089 = ORIENTED_EDGE ( 'NONE', *, *, #59624, .T. ) ;
#32090 = CARTESIAN_POINT ( 'NONE',  ( 0.5819845079324659221, 44.07435181061364204, -18.74766465427176598 ) ) ;
#32091 = CARTESIAN_POINT ( 'NONE',  ( 0.9722240750034545353, 16.95645446544487456, 39.41582016107707176 ) ) ;
#32092 = CARTESIAN_POINT ( 'NONE',  ( 4.553261556744875094, 0.000000000000000000, 0.000000000000000000 ) ) ;
#32093 = CARTESIAN_POINT ( 'NONE',  ( 0.5824936645240071931, -38.86801570395647332, 26.23957953697626877 ) ) ;
#32094 = DIRECTION ( 'NONE',  ( 0.09835009131224564660, -0.6981896185982674474, -0.7091251765524044792 ) ) ;
#32095 = ORIENTED_EDGE ( 'NONE', *, *, #44068, .T. ) ;
#32096 = DIRECTION ( 'NONE',  ( -0.07439287786467650709, 0.3693942911085772440, -0.9262902123089734596 ) ) ;
#32097 = FACE_OUTER_BOUND ( 'NONE', #1693, .T. ) ;
#32098 = B_SPLINE_CURVE_WITH_KNOTS ( 'NONE', 3,
 ( #7277, #40854, #54901, #41154, #45855, #40538, #16712, #12333, #60216, #59919, #54269, #12035, #26716, #40241, #1653, #17030, #6645, #17328, #25793, #44931, #36144, #55209, #6966, #1970, #49912 ),
 .UNSPECIFIED., .F., .F.,
 ( 4, 3, 3, 3, 3, 3, 3, 3, 4 ),
 ( 7.757919228897728493E-18, 0.0005656085177311412663, 0.001131215744874502441, 0.001696821861372768735, 0.002262427090022499018, 0.002828031679238746793, 0.003393635864401606164, 0.003977030878808133357, 0.004561030005651160735 ),
 .UNSPECIFIED. ) ;
#32099 = CARTESIAN_POINT ( 'NONE',  ( 0.1102847568649952675, 39.80641842112245143, -16.58813073670667748 ) ) ;
#32100 = ORIENTED_EDGE ( 'NONE', *, *, #54625, .F. ) ;
#32101 = CARTESIAN_POINT ( 'NONE',  ( 0.1129192098497455998, 15.69290830752535726, -41.23935519181593889 ) ) ;
#32102 = CARTESIAN_POINT ( 'NONE',  ( -6.010958268070873523, 13.31406649671962761, 13.33459572764762591 ) ) ;
#32103 = CARTESIAN_POINT ( 'NONE',  ( 0.9757787079277443487, 30.31292661677494493, 30.36877398309911769 ) ) ;
#32104 = CARTESIAN_POINT ( 'NONE',  ( 1.227938101723748288, 33.52879263017863565, 26.79402671879338271 ) ) ;
#32105 = ORIENTED_EDGE ( 'NONE', *, *, #52324, .T. ) ;
#32106 = CARTESIAN_POINT ( 'NONE',  ( -6.077587904424778920, 15.42837212129427193, -11.52221137980032495 ) ) ;
#32107 = DIRECTION ( 'NONE',  ( -1.000000000000000000, -0.000000000000000000, -0.000000000000000000 ) ) ;
#32108 = EDGE_CURVE ( 'NONE', #33073, #4875, #5329, .T. ) ;
#32109 = EDGE_CURVE ( 'NONE', #49082, #53370, #10167, .T. ) ;
#32110 = CARTESIAN_POINT ( 'NONE',  ( 1.091591847532201509, -23.20683314692016452, 34.90274897836625456 ) ) ;
#32111 = LINE ( 'NONE', #45596, #61360 ) ;
#32112 = AXIS2_PLACEMENT_3D ( 'NONE', #61817, #38372, #58043 ) ;
#32113 = CARTESIAN_POINT ( 'NONE',  ( 0.9752570700956806338, 42.90785210525868365, 0.2306661201222729995 ) ) ;
#32114 = CARTESIAN_POINT ( 'NONE',  ( 0.9758171775293909000, -5.606549717953911660, -42.54062484958063095 ) ) ;
#32115 = DIRECTION ( 'NONE',  ( 0.000000000000000000, 0.000000000000000000, -1.000000000000000000 ) ) ;
#32116 = ADVANCED_FACE ( 'NONE', ( #36510 ), #26619, .F. ) ;
#32117 = CARTESIAN_POINT ( 'NONE',  ( 4.335381028904201628, 8.818319717467213437, 48.18707383754355078 ) ) ;
#32118 = EDGE_CURVE ( 'NONE', #39207, #33948, #50430, .T. ) ;
#32119 = CARTESIAN_POINT ( 'NONE',  ( 0.8560838555295223751, -8.701885300215751684, -46.09392613244852299 ) ) ;
#32120 = ORIENTED_EDGE ( 'NONE', *, *, #10691, .T. ) ;
#32121 = EDGE_CURVE ( 'NONE', #46997, #18605, #32111, .T. ) ;
#32122 = CARTESIAN_POINT ( 'NONE',  ( 0.5786265663353153954, -41.83999636203303396, -23.32245830379073226 ) ) ;
#32123 = CARTESIAN_POINT ( 'NONE',  ( 4.553261556744873317, 12.71466023209499419, 42.04612920360230532 ) ) ;
#32124 = CARTESIAN_POINT ( 'NONE',  ( 0.1129192098497455998, -35.06977877439224045, -26.77802092202373174 ) ) ;
#32125 = CARTESIAN_POINT ( 'NONE',  ( 0.5980894510889448457, -37.73932204245498667, -29.84264441023765002 ) ) ;
#32126 = FACE_OUTER_BOUND ( 'NONE', #42274, .T. ) ;
#32127 = APPLICATION_PROTOCOL_DEFINITION ( 'draft international standard', 'automotive_design', 1998, #50787 ) ;
#32128 = CARTESIAN_POINT ( 'NONE',  ( -2.708315649062910779, 11.76894112707812212, -8.698422600177005748 ) ) ;
#32129 =( BOUNDED_SURFACE ( )  B_SPLINE_SURFACE ( 3, 1, ( 
 ( #30567, #7364 ),
 ( #31193, #31504 ),
 ( #2367, #40018 ),
 ( #16184, #54359 ) ),
 .UNSPECIFIED., .F., .F., .F. ) 
 B_SPLINE_SURFACE_WITH_KNOTS ( ( 4, 4 ),
 ( 2, 2 ),
 ( 0.000000000000000000, 1.000000000000000000 ),
 ( 0.000000000000000000, 1.000000000000000000 ),
 .UNSPECIFIED. ) 
 GEOMETRIC_REPRESENTATION_ITEM ( )  RATIONAL_B_SPLINE_SURFACE ( (
 ( 1.000000000000000000, 1.000000000000000000),
 ( 0.7211978278499970862, 0.9934217856018976445),
 ( 0.7211978278499970862, 0.9934217856018976445),
 ( 1.000000000000000000, 1.000000000000000000) ) ) 
 REPRESENTATION_ITEM ( '' )  SURFACE ( )  );
#32130 = EDGE_CURVE ( 'NONE', #20167, #23759, #26469, .T. ) ;
#32131 = CYLINDRICAL_SURFACE ( 'NONE', #40514, 2.649999999999992806 ) ;
#32132 = CARTESIAN_POINT ( 'NONE',  ( 0.6029442701453591180, -1.486909339572786815, 49.08497046728426483 ) ) ;
#32134 = ORIENTED_EDGE ( 'NONE', *, *, #44014, .F. ) ;
#32133 = DIRECTION ( 'NONE',  ( 0.000000000000000000, 1.224646799147324364E-16, 1.000000000000000000 ) ) ;
#32135 = EDGE_LOOP ( 'NONE', ( #16046, #7719 ) ) ;
#32136 = B_SPLINE_CURVE_WITH_KNOTS ( 'NONE', 3,
 ( #25781, #45231, #21084, #49899 ),
 .UNSPECIFIED., .F., .F.,
 ( 4, 4 ),
 ( 1.551583845779545699E-17, 0.005004948556313820913 ),
 .UNSPECIFIED. ) ;
#32137 = CARTESIAN_POINT ( 'NONE',  ( 0.6067099128993189705, -37.56352526808326786, 29.71710940500716447 ) ) ;
#32138 = CARTESIAN_POINT ( 'NONE',  ( 0.8760168074886960365, -17.58183840866369607, -44.77533136581875084 ) ) ;
#32139 = CARTESIAN_POINT ( 'NONE',  ( 4.549368137175248350, 0.000000000000000000, 0.000000000000000000 ) ) ;
#32140 = B_SPLINE_CURVE_WITH_KNOTS ( 'NONE', 3,
 ( #52481, #28684, #51243, #8328 ),
 .UNSPECIFIED., .F., .F.,
 ( 4, 4 ),
 ( 2.204559228842524708E-17, 0.004559932413162186803 ),
 .UNSPECIFIED. ) ;
#32141 = ORIENTED_EDGE ( 'NONE', *, *, #58835, .T. ) ;
#32142 = CARTESIAN_POINT ( 'NONE',  ( 0.5988103564986360094, -38.53259703935813718, -28.80261217992908129 ) ) ;
#32143 = DIRECTION ( 'NONE',  ( 0.000000000000000000, 0.000000000000000000, -1.000000000000000000 ) ) ;
#32144 = CARTESIAN_POINT ( 'NONE',  ( 0.6023143664670691511, -44.34466302085811407, -18.65155446683236562 ) ) ;
#32145 = EDGE_LOOP ( 'NONE', ( #1291, #36107, #16531, #51414 ) ) ;
#32146 = ORIENTED_EDGE ( 'NONE', *, *, #5684, .F. ) ;
#32147 = DIRECTION ( 'NONE',  ( -0.07906939808003032866, 0.2232318573464505962, -0.9715531730960047518 ) ) ;
#32148 = CARTESIAN_POINT ( 'NONE',  ( 1.657374760986086493, 37.58311877771095055, 22.98694477725811325 ) ) ;
#32149 = CARTESIAN_POINT ( 'NONE',  ( 4.962356264823608143, 0.000000000000000000, 0.000000000000000000 ) ) ;
#32150 = CARTESIAN_POINT ( 'NONE',  ( 5.960221823109900008, -20.34928172836728777, -2.684531185214347193 ) ) ;
#32151 = EDGE_CURVE ( 'NONE', #40264, #13345, #42253, .T. ) ;
#32152 = B_SPLINE_CURVE_WITH_KNOTS ( 'NONE', 3,
 ( #14772, #10683, #39837, #48577 ),
 .UNSPECIFIED., .F., .F.,
 ( 4, 4 ),
 ( 1.084202172485504434E-19, 0.004444878191957696463 ),
 .UNSPECIFIED. ) ;
#32153 = CARTESIAN_POINT ( 'NONE',  ( 0.1139756605157204034, -42.78034046113214117, -10.80729798444754408 ) ) ;
#32154 = CIRCLE ( 'NONE', #44173, 43.92652462719577500 ) ;
#32155 = EDGE_CURVE ( 'NONE', #42216, #52728, #38675, .T. ) ;
#32156 = B_SPLINE_CURVE_WITH_KNOTS ( 'NONE', 3,
 ( #20717, #44550, #58278, #48293, #19488, #44241, #39857, #53893, #38605, #11019, #5043, #15408, #15722, #43937, #20108, #29795, #25099, #38925, #58911, #58585, #34828, #48908, #39535, #5957, #33903, #39228, #16025, #14790, #54195, #43309 ),
 .UNSPECIFIED., .F., .F.,
 ( 4, 2, 2, 2, 2, 2, 2, 2, 2, 2, 2, 2, 2, 2, 4 ),
 ( 0.000000000000000000, 0.0004121561524868821188, 0.0008243123049737642377, 0.001236468457460646302, 0.001648624609947528042, 0.002472936914921291304, 0.002885093067408174561, 0.003297249219895058252, 0.003709405372381941943, 0.004121561524868825634, 0.004945873829842592148, 0.005358029982329475839, 0.005770186134816359530, 0.006182342287303243221, 0.006594498439790126912 ),
 .UNSPECIFIED. ) ;
#32157 = ORIENTED_EDGE ( 'NONE', *, *, #45187, .T. ) ;
#32158 = CARTESIAN_POINT ( 'NONE',  ( -6.078726893082806448, 12.00325722817150620, -15.05708661006732108 ) ) ;
#32159 = CARTESIAN_POINT ( 'NONE',  ( -6.077587904424778920, -6.644566705895037728, 18.07334376048996916 ) ) ;
#32160 = ORIENTED_EDGE ( 'NONE', *, *, #32549, .F. ) ;
#32161 = DIRECTION ( 'NONE',  ( -1.000000000000000000, -0.000000000000000000, -0.000000000000000000 ) ) ;
#32162 = CARTESIAN_POINT ( 'NONE',  ( 5.910764540655177868, -9.679148173057056326, 17.62995544841702866 ) ) ;
#32163 = CARTESIAN_POINT ( 'NONE',  ( 3.221118495291108719, 38.77389282677542326, -20.76888669908632323 ) ) ;
#32164 = CARTESIAN_POINT ( 'NONE',  ( 1.830465331921976135, 37.57662538868725477, -22.98637162052015626 ) ) ;
#32165 = ORIENTED_EDGE ( 'NONE', *, *, #35754, .F. ) ;
#32166 = ORIENTED_EDGE ( 'NONE', *, *, #32356, .F. ) ;
#32167 = CARTESIAN_POINT ( 'NONE',  ( 0.5804410086790514622, 36.46521478791949278, -29.49250688439851231 ) ) ;
#32168 = ORIENTED_EDGE ( 'NONE', *, *, #20841, .T. ) ;
#32169 = CARTESIAN_POINT ( 'NONE',  ( -6.017396004339687465, -2.458362590802666947, -18.68211039806566376 ) ) ;
#32170 = EDGE_LOOP ( 'NONE', ( #31322, #53194, #23524, #25511 ) ) ;
#32171 = CARTESIAN_POINT ( 'NONE',  ( 1.000433927950263646, -39.80191350348199109, -13.12350407148118059 ) ) ;
#32172 = VERTEX_POINT ( 'NONE', #28024 ) ;
#32173 = CARTESIAN_POINT ( 'NONE',  ( 2.643462169533600914, 46.02269433264213205, 13.76277278785576463 ) ) ;
#32174 = CARTESIAN_POINT ( 'NONE',  ( 0.9791128995231609400, 24.86348713967445789, 33.73639639175184612 ) ) ;
#32175 = CARTESIAN_POINT ( 'NONE',  ( 4.963659409799330291, 44.68724496494571241, 2.450325214228553428 ) ) ;
#32176 = ORIENTED_EDGE ( 'NONE', *, *, #56949, .T. ) ;
#32177 = CARTESIAN_POINT ( 'NONE',  ( 0.1156867017252034419, -27.41316746739866872, -34.57544007933292818 ) ) ;
#32178 = CARTESIAN_POINT ( 'NONE',  ( 0.1154773475650540254, -27.37012761473843270, 34.60953256545158041 ) ) ;
#32179 = MANIFOLD_SOLID_BREP ( 'RollersSimplified', #3994 ) ;
#32180 = CARTESIAN_POINT ( 'NONE',  ( 1.231276596079881047, 29.74482033789362134, -29.53849072116746655 ) ) ;
#32181 = EDGE_CURVE ( 'NONE', #33708, #6988, #40040, .T. ) ;
#32182 = ORIENTED_EDGE ( 'NONE', *, *, #35153, .F. ) ;
#32183 = CARTESIAN_POINT ( 'NONE',  ( -20.00694009185712119, -12.48893006068259837, 0.5428783724460725102 ) ) ;
#32184 = CARTESIAN_POINT ( 'NONE',  ( 0.5997462898726536595, -39.04071682475767346, -29.78882441375276358 ) ) ;
#32185 = CARTESIAN_POINT ( 'NONE',  ( 0.6254311100348635133, -24.64676532715822077, 41.31309618784372617 ) ) ;
#32186 = CARTESIAN_POINT ( 'NONE',  ( 0.8554163680231816613, 46.36773742900852113, -7.158100224664470268 ) ) ;
#32187 = CARTESIAN_POINT ( 'NONE',  ( 4.975801465491695552, -9.906103548667894998, -46.87746200127453022 ) ) ;
#32188 = ORIENTED_EDGE ( 'NONE', *, *, #19278, .T. ) ;
#32189 = EDGE_CURVE ( 'NONE', #32408, #46644, #40818, .T. ) ;
#32190 = CARTESIAN_POINT ( 'NONE',  ( 0.1095718737110177865, 37.47471772507220322, -21.33933464366381116 ) ) ;
#32191 = EDGE_CURVE ( 'NONE', #24422, #22241, #31805, .T. ) ;
#32192 = CARTESIAN_POINT ( 'NONE',  ( 0.7242003506640003474, -48.79688540705116395, -5.465862118380373502 ) ) ;
#32193 = ORIENTED_EDGE ( 'NONE', *, *, #3170, .T. ) ;
#32194 = ADVANCED_FACE ( 'NONE', ( #61814 ), #33048, .F. ) ;
#32195 = CARTESIAN_POINT ( 'NONE',  ( -6.078075953587585900, 16.77554405305477658, 9.453903742431199575 ) ) ;
#32196 = CARTESIAN_POINT ( 'NONE',  ( 0.5809828226811565299, 28.72298383114543796, -38.32755012159114472 ) ) ;
#32197 = CARTESIAN_POINT ( 'NONE',  ( 5.965394784446458765, -2.693446924985486657, -20.34787558161485777 ) ) ;
#32198 = CARTESIAN_POINT ( 'NONE',  ( 4.962356264823609031, 31.50371261889155150, -27.90612278853226513 ) ) ;
#32199 = B_SPLINE_CURVE_WITH_KNOTS ( 'NONE', 3,
 ( #37444, #8590, #18021, #51815 ),
 .UNSPECIFIED., .F., .F.,
 ( 4, 4 ),
 ( 3.252606517456513302E-19, 0.004444878191957676514 ),
 .UNSPECIFIED. ) ;
#32200 = CARTESIAN_POINT ( 'NONE',  ( 5.959828726073459926, -10.26672511661743670, -17.77343634131838002 ) ) ;
#32201 = CARTESIAN_POINT ( 'NONE',  ( 0.1129192098497447394, -40.71518461128108157, 17.00663193740767909 ) ) ;
#32202 = CIRCLE ( 'NONE', #58150, 42.92674063221959813 ) ;
#32203 = DIRECTION ( 'NONE',  ( 1.836909530733573776E-16, -1.000000000000000000, 0.000000000000000000 ) ) ;
#32204 = PRESENTATION_STYLE_ASSIGNMENT (( #45695 ) ) ;
#32205 = CARTESIAN_POINT ( 'NONE',  ( 0.6028618097248862329, 38.27229381545012643, 29.14732267129586418 ) ) ;
#32206 = VECTOR ( 'NONE', #45330, 1000.000000000000000 ) ;
#32207 = FACE_OUTER_BOUND ( 'NONE', #35640, .T. ) ;
#32208 = CARTESIAN_POINT ( 'NONE',  ( 1.157644175074335591, 19.41637191003240659, 37.14844246170341791 ) ) ;
#32209 =( BOUNDED_SURFACE ( )  B_SPLINE_SURFACE ( 3, 1, ( 
 ( #48618, #38032 ),
 ( #23898, #10419 ),
 ( #28895, #15121 ),
 ( #34539, #4751 ) ),
 .UNSPECIFIED., .F., .F., .F. ) 
 B_SPLINE_SURFACE_WITH_KNOTS ( ( 4, 4 ),
 ( 2, 2 ),
 ( 0.000000000000000000, 1.000000000000000000 ),
 ( 0.000000000000000000, 1.000000000000000000 ),
 .UNSPECIFIED. ) 
 GEOMETRIC_REPRESENTATION_ITEM ( )  RATIONAL_B_SPLINE_SURFACE ( (
 ( 1.000000000000000000, 1.000000000000000000),
 ( 0.9953040768229013402, 0.8617119497784988535),
 ( 0.9953040768229013402, 0.8617119497784988535),
 ( 1.000000000000000000, 1.000000000000000000) ) ) 
 REPRESENTATION_ITEM ( '' )  SURFACE ( )  );
#32210 = CARTESIAN_POINT ( 'NONE',  ( 4.962356264823609031, -32.75738977283769771, -26.42326651140497873 ) ) ;
#32212 = EDGE_CURVE ( 'NONE', #28122, #47245, #14617, .T. ) ;
#32211 = CARTESIAN_POINT ( 'NONE',  ( 5.860006189529246790, -21.31760477694550460, -43.26650951066891793 ) ) ;
#32213 = B_SPLINE_CURVE_WITH_KNOTS ( 'NONE', 3,
 ( #40902, #4090, #59967, #55253, #27616, #37340 ),
 .UNSPECIFIED., .F., .F.,
 ( 4, 2, 4 ),
 ( 1.241905198432914574E-16, 0.0002450741128632342395, 0.0004901482257263442294 ),
 .UNSPECIFIED. ) ;
#32214 = DIRECTION ( 'NONE',  ( -0.9848077530122080203, -0.1736481776669315524, 2.220446049250313574E-16 ) ) ;
#32215 = DIRECTION ( 'NONE',  ( 0.09835009131224552170, -0.007732607185423958154, -0.9951218349151971232 ) ) ;
#32216 = CARTESIAN_POINT ( 'NONE',  ( 5.894904586330512508, -17.30455939762460460, -10.25093342655803497 ) ) ;
#32217 = EDGE_CURVE ( 'NONE', #36286, #31306, #410, .T. ) ;
#32218 = CARTESIAN_POINT ( 'NONE',  ( 4.975610109902397937, 30.04451009524531102, -38.59762713269398660 ) ) ;
#32219 = CARTESIAN_POINT ( 'NONE',  ( 7.999999999999983125, 80.00000000000001421, -2.649999999999992806 ) ) ;
#32220 = CARTESIAN_POINT ( 'NONE',  ( 0.6031356219577718170, -38.11305734842083126, 29.35521383643393634 ) ) ;
#32221 = ORIENTED_EDGE ( 'NONE', *, *, #35236, .T. ) ;
#32222 = CARTESIAN_POINT ( 'NONE',  ( 1.154321713695932727, -29.75729669971086722, -30.92445811446677340 ) ) ;
#32223 = CARTESIAN_POINT ( 'NONE',  ( 2.643462169533600914, 47.42536612906418725, 7.637863311827770119 ) ) ;
#32224 = CARTESIAN_POINT ( 'NONE',  ( 3.221118495291109163, 28.14629310243162763, -33.80159174142189471 ) ) ;
#32225 = FACE_OUTER_BOUND ( 'NONE', #40881, .T. ) ;
#32226 = ORIENTED_EDGE ( 'NONE', *, *, #35305, .T. ) ;
#32227 = FACE_OUTER_BOUND ( 'NONE', #38327, .T. ) ;
#32228 = CARTESIAN_POINT ( 'NONE',  ( 4.967162193818130511, 42.96271701169388990, -3.259922920617310371 ) ) ;
#32229 = VERTEX_POINT ( 'NONE', #36063 ) ;
#32230 = ADVANCED_FACE ( 'NONE', ( #16628 ), #6635, .F. ) ;
#32231 = CARTESIAN_POINT ( 'NONE',  ( 0.8560838555295158248, 37.37287335782446718, -28.34856559090329142 ) ) ;
#32232 = ORIENTED_EDGE ( 'NONE', *, *, #3793, .T. ) ;
#32233 = CARTESIAN_POINT ( 'NONE',  ( 1.227938101723756947, 39.32113113558990847, -17.20315230597801914 ) ) ;
#32234 = CARTESIAN_POINT ( 'NONE',  ( 0.1064266379913939853, 22.04679939086782525, 37.06314005629921127 ) ) ;
#32235 = EDGE_LOOP ( 'NONE', ( #3947, #13970 ) ) ;
#32236 = CYLINDRICAL_SURFACE ( 'NONE', #13477, 2.649999999999992806 ) ;
#32237 = CARTESIAN_POINT ( 'NONE',  ( 0.1103310638050662290, 26.18709435931479845, 34.26302445194755109 ) ) ;
#32238 = ORIENTED_EDGE ( 'NONE', *, *, #35595, .T. ) ;
#32239 = CARTESIAN_POINT ( 'NONE',  ( 0.5835226383429293895, -7.979743399672678095, -46.21218637785216288 ) ) ;
#32240 = CARTESIAN_POINT ( 'NONE',  ( 0.5782707292762423457, -30.83005644796779521, -35.34464560754199880 ) ) ;
#32241 = VECTOR ( 'NONE', #34142, 1000.000000000000000 ) ;
#32242 = ORIENTED_EDGE ( 'NONE', *, *, #49831, .F. ) ;
#32243 = CARTESIAN_POINT ( 'NONE',  ( 3.680882792899938138, -42.44216617524801194, -22.36818923730755415 ) ) ;
#32244 = ORIENTED_EDGE ( 'NONE', *, *, #34215, .F. ) ;
#32245 = CARTESIAN_POINT ( 'NONE',  ( 2.282803330402964015, -43.92595983154121342, -16.64352607877350465 ) ) ;
#32246 = VECTOR ( 'NONE', #3075, 1000.000000000000000 ) ;
#32247 = ORIENTED_EDGE ( 'NONE', *, *, #46654, .F. ) ;
#32248 = VERTEX_POINT ( 'NONE', #20708 ) ;
#32249 = CARTESIAN_POINT ( 'NONE',  ( 0.6016118706126978299, -42.61631147553848820, -24.40084119459445589 ) ) ;
#32250 = CARTESIAN_POINT ( 'NONE',  ( -2.708315649062916552, -12.54007339125019982, 7.544341609839765539 ) ) ;
#32251 = DIRECTION ( 'NONE',  ( -1.000000000000000000, -0.000000000000000000, -0.000000000000000000 ) ) ;
#32252 = B_SPLINE_CURVE_WITH_KNOTS ( 'NONE', 3,
 ( #57170, #14304, #24300, #29921, #52487, #9900, #58100, #29608, #39046, #42816, #33410, #10828, #475, #48115, #38421, #29002, #44066, #43435, #34031 ),
 .UNSPECIFIED., .F., .F.,
 ( 4, 3, 3, 3, 3, 3, 4 ),
 ( 5.204170427930421283E-18, 0.0002724573126191775444, 0.0004086839781548478809, 0.0005449106435901823536, 0.0006811373090491453864, 0.0008459866663933667723, 0.001010840725717211197 ),
 .UNSPECIFIED. ) ;
#32253 = CARTESIAN_POINT ( 'NONE',  ( 0.1097557419366048670, -16.29667732266778302, 39.92664986079706324 ) ) ;
#32254 = DIRECTION ( 'NONE',  ( 0.07836865515943411409, 0.9873352307081162405, 0.1379401902675667646 ) ) ;
#32255 = ORIENTED_EDGE ( 'NONE', *, *, #49707, .T. ) ;
#32256 = CARTESIAN_POINT ( 'NONE',  ( 0.9730545539215883499, 11.59290486963506517, 41.31259007387235727 ) ) ;
#32257 = CARTESIAN_POINT ( 'NONE',  ( 5.901463166500145796, 17.94437285245830793, 9.083906278281064672 ) ) ;
#32258 = CARTESIAN_POINT ( 'NONE',  ( 0.5997462898726536595, 46.43852004798865352, -15.96920429754923632 ) ) ;
#32259 = ORIENTED_EDGE ( 'NONE', *, *, #14524, .F. ) ;
#32260 = VERTEX_POINT ( 'NONE', #54188 ) ;
#32261 = CARTESIAN_POINT ( 'NONE',  ( 0.9730545539215883499, 11.59290486963565137, -41.31259007387218674 ) ) ;
#32262 = DIRECTION ( 'NONE',  ( 0.000000000000000000, 0.000000000000000000, 1.000000000000000000 ) ) ;
#32263 = CARTESIAN_POINT ( 'NONE',  ( -2.600000000000000533, -11.64055411052240352, -1.199999999999999956 ) ) ;
#32264 = DIRECTION ( 'NONE',  ( 0.000000000000000000, 0.000000000000000000, 1.000000000000000000 ) ) ;
#32265 = LINE ( 'NONE', #55427, #41764 ) ;
#32266 = ADVANCED_FACE ( 'NONE', ( #12249 ), #11625, .T. ) ;
#32267 = ORIENTED_EDGE ( 'NONE', *, *, #30101, .F. ) ;
#32268 = CARTESIAN_POINT ( 'NONE',  ( 0.5827357941260213892, 47.53228940613941234, 5.891356987507786691 ) ) ;
#32269 = EDGE_CURVE ( 'NONE', #27827, #4313, #49768, .T. ) ;
#32270 = CARTESIAN_POINT ( 'NONE',  ( 4.322998006666179727, 30.86725474310310702, 36.74401119231420410 ) ) ;
#32271 = CARTESIAN_POINT ( 'NONE',  ( 0.9758171775293921213, -34.03798695362329596, 26.12572690811900600 ) ) ;
#32272 = LINE ( 'NONE', #4035, #28942 ) ;
#32273 = B_SPLINE_CURVE_WITH_KNOTS ( 'NONE', 3,
 ( #6993, #12058, #16738, #16424 ),
 .UNSPECIFIED., .F., .F.,
 ( 4, 4 ),
 ( 2.909219710836648185E-18, 0.004050076154993001616 ),
 .UNSPECIFIED. ) ;
#32274 = CARTESIAN_POINT ( 'NONE',  ( 43.00000000000000000, 1.530808498934191521E-15, -12.50000000000000000 ) ) ;
#32275 = ORIENTED_EDGE ( 'NONE', *, *, #58020, .T. ) ;
#32276 = CARTESIAN_POINT ( 'NONE',  ( 0.5998501479064708430, 37.84527566984816360, 29.69975237324626605 ) ) ;
#32277 = CARTESIAN_POINT ( 'NONE',  ( 2.648799415243696664, 46.95584109391764827, -14.13033794544045030 ) ) ;
#32278 = CARTESIAN_POINT ( 'NONE',  ( 0.2885697896453117139, -39.51953439758099051, -17.24062360132701954 ) ) ;
#32279 = B_SPLINE_CURVE_WITH_KNOTS ( 'NONE', 3,
 ( #48504, #5568, #24708, #43847, #890, #37133 ),
 .UNSPECIFIED., .F., .F.,
 ( 4, 2, 4 ),
 ( 0.000000000000000000, 0.0002447195606305758845, 0.0004894391212611517690 ),
 .UNSPECIFIED. ) ;
#32281 = ADVANCED_FACE ( 'NONE', ( #49513 ), #30272, .F. ) ;
#32280 = CARTESIAN_POINT ( 'NONE',  ( 0.1100247026804066219, 21.70899701554524341, -37.26174279786191335 ) ) ;
#32282 = CARTESIAN_POINT ( 'NONE',  ( -6.078075953587585900, 0.6224930363967494662, 19.24597819459363279 ) ) ;
#32283 = CARTESIAN_POINT ( 'NONE',  ( 0.5839879882012665169, 6.251648354650867212, -47.48621496524027208 ) ) ;
#32284 = EDGE_CURVE ( 'NONE', #8036, #54532, #24365, .T. ) ;
#32285 = LINE ( 'NONE', #3139, #28121 ) ;
#32286 = MECHANICAL_DESIGN_GEOMETRIC_PRESENTATION_REPRESENTATION (  '', ( #54242 ), #24272 ) ;
#32287 = CARTESIAN_POINT ( 'NONE',  ( 5.895596859100789899, -7.225383168025214076, 18.77024297359267990 ) ) ;
#32288 = ORIENTED_EDGE ( 'NONE', *, *, #3757, .F. ) ;
#32289 = CARTESIAN_POINT ( 'NONE',  ( 2.281448460670571166, -43.80196084514292210, 19.56578495220155389 ) ) ;
#32290 = CARTESIAN_POINT ( 'NONE',  ( 2.185380717157383579, 23.99818600003833780, -36.91756860594645673 ) ) ;
#32291 = CARTESIAN_POINT ( 'NONE',  ( 0.8557997880470697982, 34.51495345639548873, 33.22501220301912639 ) ) ;
#32292 = CARTESIAN_POINT ( 'NONE',  ( 0.6001305935487315502, -41.40054608060309960, 24.50730504006385502 ) ) ;
#32293 = ORIENTED_EDGE ( 'NONE', *, *, #7479, .F. ) ;
#32294 = CARTESIAN_POINT ( 'NONE',  ( -6.078075953587585900, 5.483964907265516331, -18.45863762965772636 ) ) ;
#32295 = CARTESIAN_POINT ( 'NONE',  ( 0.9762797500689124330, -41.84568905980455611, -2.294143041716810050 ) ) ;
#32296 = B_SPLINE_CURVE_WITH_KNOTS ( 'NONE', 3,
 ( #2282, #21411, #40248, #39306 ),
 .UNSPECIFIED., .F., .F.,
 ( 4, 4 ),
 ( 2.380113941701692686E-17, 0.004559932413162186803 ),
 .UNSPECIFIED. ) ;
#32297 =( BOUNDED_SURFACE ( )  B_SPLINE_SURFACE ( 3, 1, ( 
 ( #16971, #21650 ),
 ( #36083, #7525 ),
 ( #55145, #12272 ),
 ( #31359, #58811 ) ),
 .UNSPECIFIED., .F., .F., .F. ) 
 B_SPLINE_SURFACE_WITH_KNOTS ( ( 4, 4 ),
 ( 2, 2 ),
 ( 0.000000000000000000, 1.000000000000000000 ),
 ( 0.000000000000000000, 1.000000000000000000 ),
 .UNSPECIFIED. ) 
 GEOMETRIC_REPRESENTATION_ITEM ( )  RATIONAL_B_SPLINE_SURFACE ( (
 ( 1.000000000000000000, 1.000000000000000000),
 ( 0.9754377213608244057, 0.9999580625633939235),
 ( 0.9754377213608244057, 0.9999580625633939235),
 ( 1.000000000000000000, 1.000000000000000000) ) ) 
 REPRESENTATION_ITEM ( '' )  SURFACE ( )  );
#32298 =( NAMED_UNIT ( * ) SI_UNIT ( $, .STERADIAN. ) SOLID_ANGLE_UNIT ( ) );
#32299 = B_SPLINE_CURVE_WITH_KNOTS ( 'NONE', 3,
 ( #45137, #30689, #40142, #6865 ),
 .UNSPECIFIED., .F., .F.,
 ( 4, 4 ),
 ( 0.000000000000000000, 0.005004948556313807036 ),
 .UNSPECIFIED. ) ;
#32300 = VERTEX_POINT ( 'NONE', #1889 ) ;
#32301 = CARTESIAN_POINT ( 'NONE',  ( 5.981074661064941900, -19.82752479807530932, 5.303881226583333941 ) ) ;
#32303 = EDGE_CURVE ( 'NONE', #29097, #11449, #23580, .T. ) ;
#32302 = VECTOR ( 'NONE', #39801, 1000.000000000000227 ) ;
#32304 = CARTESIAN_POINT ( 'NONE',  ( 4.967162193818130511, -40.93989340068600313, -13.42934394584206359 ) ) ;
#32305 = ORIENTED_EDGE ( 'NONE', *, *, #31188, .F. ) ;
#32306 = CARTESIAN_POINT ( 'NONE',  ( 0.3622758884714730732, 0.8252992914322084816, 43.10531414739106282 ) ) ;
#32307 = ORIENTED_EDGE ( 'NONE', *, *, #29968, .F. ) ;
#32308 = ORIENTED_EDGE ( 'NONE', *, *, #21884, .F. ) ;
#32309 = CARTESIAN_POINT ( 'NONE',  ( -4.915099999999998914, 0.000000000000000000, 0.000000000000000000 ) ) ;
#32310 = EDGE_LOOP ( 'NONE', ( #16654, #2841, #2495, #15624 ) ) ;
#32311 = CARTESIAN_POINT ( 'NONE',  ( 0.5782707292762442330, -14.58551739541110948, 44.57576736317366084 ) ) ;
#32312 = B_SPLINE_CURVE_WITH_KNOTS ( 'NONE', 3,
 ( #17664, #21434, #50244, #22359, #54928, #17359 ),
 .UNSPECIFIED., .F., .F.,
 ( 4, 2, 4 ),
 ( 2.196881373128401347E-17, 0.0002293755540694319690, 0.0004587511081388419287 ),
 .UNSPECIFIED. ) ;
#32313 = ORIENTED_EDGE ( 'NONE', *, *, #31323, .F. ) ;
#32314 = CARTESIAN_POINT ( 'NONE',  ( 4.958415959904820092, 45.35203410338238683, -2.529220533737273957 ) ) ;
#32315 =( BOUNDED_SURFACE ( )  B_SPLINE_SURFACE ( 3, 1, ( 
 ( #59824, #26940 ),
 ( #26313, #8130 ),
 ( #26621, #56042 ),
 ( #17542, #16617 ) ),
 .UNSPECIFIED., .F., .F., .F. ) 
 B_SPLINE_SURFACE_WITH_KNOTS ( ( 4, 4 ),
 ( 2, 2 ),
 ( 0.000000000000000000, 1.000000000000000000 ),
 ( 0.000000000000000000, 1.000000000000000000 ),
 .UNSPECIFIED. ) 
 GEOMETRIC_REPRESENTATION_ITEM ( )  RATIONAL_B_SPLINE_SURFACE ( (
 ( 1.000000000000000000, 1.000000000000000000),
 ( 0.9751682680413298332, 0.9999560080971552356),
 ( 0.9751682680413298332, 0.9999560080971552356),
 ( 1.000000000000000000, 1.000000000000000000) ) ) 
 REPRESENTATION_ITEM ( '' )  SURFACE ( )  );
#32316 = CARTESIAN_POINT ( 'NONE',  ( -6.079354080745853928, -1.847856142170532623, 19.16711723045499483 ) ) ;
#32317 = CARTESIAN_POINT ( 'NONE',  ( -6.077587904424778920, -14.65844225831500225, -12.48703695652317158 ) ) ;
#32318 = ORIENTED_EDGE ( 'NONE', *, *, #18176, .T. ) ;
#32319 = CARTESIAN_POINT ( 'NONE',  ( 0.1129192098497447394, 15.69290830752478882, 41.23935519181615206 ) ) ;
#32320 = CARTESIAN_POINT ( 'NONE',  ( 0.09136607875274982415, 0.000000000000000000, 43.12527911185304674 ) ) ;
#32321 = CARTESIAN_POINT ( 'NONE',  ( 2.879087469061463178, -37.45964864250908022, 23.08411575874515975 ) ) ;
#32322 = CARTESIAN_POINT ( 'NONE',  ( 0.5806925824938499181, 46.89268439822727430, -0.5463627657667492477 ) ) ;
#32323 = EDGE_LOOP ( 'NONE', ( #32755, #39742, #15809, #5832 ) ) ;
#32324 = CARTESIAN_POINT ( 'NONE',  ( 4.975610109902397937, 0.000000000000000000, 0.000000000000000000 ) ) ;
#32325 = CARTESIAN_POINT ( 'NONE',  ( 4.960156602257184133, 20.99019478193049792, 41.40608197274642066 ) ) ;
#32327 = ORIENTED_EDGE ( 'NONE', *, *, #21888, .T. ) ;
#32326 = B_SPLINE_CURVE_WITH_KNOTS ( 'NONE', 3,
 ( #54126, #7133, #11247, #48001 ),
 .UNSPECIFIED., .F., .F.,
 ( 4, 4 ),
 ( 0.000000000000000000, 0.005014147105413698652 ),
 .UNSPECIFIED. ) ;
#32328 = VECTOR ( 'NONE', #56002, 1000.000000000000114 ) ;
#32329 = DIRECTION ( 'NONE',  ( 0.000000000000000000, 0.000000000000000000, 1.000000000000000000 ) ) ;
#32330 = VERTEX_POINT ( 'NONE', #1572 ) ;
#32331 = CARTESIAN_POINT ( 'NONE',  ( 0.1157991065609915715, -12.63256843914561145, 42.27718746756933399 ) ) ;
#32332 = DIRECTION ( 'NONE',  ( 1.000000000000000000, 1.836909530733573776E-16, 0.000000000000000000 ) ) ;
#32333 = ORIENTED_EDGE ( 'NONE', *, *, #36817, .T. ) ;
#32334 = CARTESIAN_POINT ( 'NONE',  ( 45.00000000000001421, 7.805869035311033600E-47, 13.00000000000000178 ) ) ;
#32335 = CARTESIAN_POINT ( 'NONE',  ( 5.901764892641307547, -16.95277890151849221, 45.94120976809283263 ) ) ;
#32336 = CARTESIAN_POINT ( 'NONE',  ( 0.8557997880470697982, 24.73961900479251952, 41.02602466100786671 ) ) ;
#32337 = DIRECTION ( 'NONE',  ( -1.000000000000000000, -0.000000000000000000, 1.925929944387235853E-32 ) ) ;
#32338 = EDGE_CURVE ( 'NONE', #10841, #10038, #56406, .T. ) ;
#32339 = ORIENTED_EDGE ( 'NONE', *, *, #61435, .F. ) ;
#32340 = CARTESIAN_POINT ( 'NONE',  ( 4.553261556744875094, -43.82122302957815663, -3.039733214544628748 ) ) ;
#32341 = EDGE_CURVE ( 'NONE', #9094, #39332, #318, .T. ) ;
#32342 = DIRECTION ( 'NONE',  ( 0.000000000000000000, 0.000000000000000000, 1.000000000000000000 ) ) ;
#32343 = CARTESIAN_POINT ( 'NONE',  ( -6.017396004339686577, 18.68180398134253650, -2.460690056887598232 ) ) ;
#32344 = VECTOR ( 'NONE', #50908, 1000.000000000000000 ) ;
#32345 = B_SPLINE_CURVE_WITH_KNOTS ( 'NONE', 3,
 ( #45589, #21151, #44670, #36195 ),
 .UNSPECIFIED., .F., .F.,
 ( 4, 4 ),
 ( 2.250920953359534068E-17, 0.004564976165746189446 ),
 .UNSPECIFIED. ) ;
#32346 = EDGE_CURVE ( 'NONE', #61018, #46714, #16018, .T. ) ;
#32347 = B_SPLINE_CURVE_WITH_KNOTS ( 'NONE', 3,
 ( #19413, #32902, #9069, #38530 ),
 .UNSPECIFIED., .F., .F.,
 ( 4, 4 ),
 ( 1.962615573354718958E-17, 0.005004741218457442291 ),
 .UNSPECIFIED. ) ;
#32348 = CARTESIAN_POINT ( 'NONE',  ( -6.078457390727109555, 9.978433202401264523, 16.46892169702449138 ) ) ;
#32349 = DIRECTION ( 'NONE',  ( 1.000000000000000000, 0.000000000000000000, 0.000000000000000000 ) ) ;
#32350 = CARTESIAN_POINT ( 'NONE',  ( 0.8744876279028263033, 37.95405449045444612, -31.14225101233220627 ) ) ;
#32351 = DIRECTION ( 'NONE',  ( -1.000000000000000000, -1.836909530733573776E-16, 1.361838123766442686E-32 ) ) ;
#32352 = CARTESIAN_POINT ( 'NONE',  ( -5.995132425357893702, 2.468096378288119563, 18.68182899165012500 ) ) ;
#32353 = CARTESIAN_POINT ( 'NONE',  ( 4.962356264823608143, 0.000000000000000000, 0.000000000000000000 ) ) ;
#32354 = CARTESIAN_POINT ( 'NONE',  ( 0.9791128995231609400, 32.89306773298482511, 25.96889542047248511 ) ) ;
#32355 = CARTESIAN_POINT ( 'NONE',  ( -6.077587904424778920, 5.484810954822468609, -18.45840919970596516 ) ) ;
#32356 = EDGE_CURVE ( 'NONE', #55001, #14065, #17248, .T. ) ;
#32357 = CARTESIAN_POINT ( 'NONE',  ( 0.1103310638050661874, -21.63353985999714624, 37.30561229499292608 ) ) ;
#32358 = CARTESIAN_POINT ( 'NONE',  ( 2.528190830796654076, 38.15965687918174609, 17.49556295224946822 ) ) ;
#32359 = CARTESIAN_POINT ( 'NONE',  ( 0.9754642270333697684, 37.07163437210445522, 21.60621846558649040 ) ) ;
#32360 = CARTESIAN_POINT ( 'NONE',  ( 0.1129192098497455998, -31.35755906439593943, -31.04279751098591689 ) ) ;
#32361 = CARTESIAN_POINT ( 'NONE',  ( 3.680882792899937250, 46.78529781139673105, 10.62117075007664369 ) ) ;
#32362 = CARTESIAN_POINT ( 'NONE',  ( 0.5817217712918328898, 45.34790564380423916, -11.94999613928816196 ) ) ;
#32363 = CARTESIAN_POINT ( 'NONE',  ( 0.6009452777970410997, 46.35353542372322977, -12.87217382175445479 ) ) ;
#32365 = ORIENTED_EDGE ( 'NONE', *, *, #33078, .F. ) ;
#32364 = DIRECTION ( 'NONE',  ( 0.000000000000000000, 0.000000000000000000, -1.000000000000000000 ) ) ;
#32366 = ORIENTED_EDGE ( 'NONE', *, *, #51654, .T. ) ;
#32367 = CARTESIAN_POINT ( 'NONE',  ( 4.549368137175248350, -19.17571786012296187, -38.40568845698270195 ) ) ;
#32368 = CARTESIAN_POINT ( 'NONE',  ( 0.5839254288179560604, 23.86932519546729381, 41.52446060675833195 ) ) ;
#32369 = CARTESIAN_POINT ( 'NONE',  ( 0.8557997880470697982, 37.44587306708137930, -29.88293891557432858 ) ) ;
#32370 = ORIENTED_EDGE ( 'NONE', *, *, #4943, .F. ) ;
#32371 = ORIENTED_EDGE ( 'NONE', *, *, #27305, .F. ) ;
#32372 = CARTESIAN_POINT ( 'NONE',  ( 1.112077966505210957, -30.92531005629962948, 31.41107325530738947 ) ) ;
#32373 = CARTESIAN_POINT ( 'NONE',  ( 4.390527457369401532, 27.14076954505956252, 34.54799509567215665 ) ) ;
#32374 = VECTOR ( 'NONE', #26560, 999.9999999999998863 ) ;
#32375 = UNCERTAINTY_MEASURE_WITH_UNIT (LENGTH_MEASURE( 1.000000000000000082E-05 ), #25774, 'distance_accuracy_value', 'NONE');
#32376 = ORIENTED_EDGE ( 'NONE', *, *, #6664, .T. ) ;
#32377 = EDGE_LOOP ( 'NONE', ( #61455, #54943, #16593, #8904 ) ) ;
#32378 = CARTESIAN_POINT ( 'NONE',  ( 0.9757787079277443487, -11.06737752163067334, -41.45659305953932972 ) ) ;
#32379 = CARTESIAN_POINT ( 'NONE',  ( 40.00000000000000000, 7.347638122934295104E-15, -7.703719777548943412E-31 ) ) ;
#32380 = CARTESIAN_POINT ( 'NONE',  ( 0.9741495583595178864, -41.54695848110004874, 10.72301204857641643 ) ) ;
#32381 = B_SPLINE_CURVE_WITH_KNOTS ( 'NONE', 3,
 ( #16633, #12255, #31345, #7513, #55441, #31653 ),
 .UNSPECIFIED., .F., .F.,
 ( 4, 2, 4 ),
 ( 6.732537572691846445E-18, 0.0002291472222819932608, 0.0004582944445639797995 ),
 .UNSPECIFIED. ) ;
#32382 = EDGE_LOOP ( 'NONE', ( #19999, #41948, #58609, #16535, #369, #50387 ) ) ;
#32383 = EDGE_CURVE ( 'NONE', #3369, #42030, #60139, .T. ) ;
#32384 = ORIENTED_EDGE ( 'NONE', *, *, #33394, .T. ) ;
#32385 = CARTESIAN_POINT ( 'NONE',  ( -6.001507490154110336, 11.48377994779700728, 14.94036486426017341 ) ) ;
#32386 = CIRCLE ( 'NONE', #5342, 15.99999999999999645 ) ;
#32387 = B_SPLINE_CURVE_WITH_KNOTS ( 'NONE', 3,
 ( #22173, #56593, #26868, #13711 ),
 .UNSPECIFIED., .F., .F.,
 ( 4, 4 ),
 ( 4.336808689942017736E-19, 0.004444878191957683453 ),
 .UNSPECIFIED. ) ;
#32388 = ADVANCED_FACE ( 'NONE', ( #44543 ), #4630, .F. ) ;
#32389 = FACE_OUTER_BOUND ( 'NONE', #30844, .T. ) ;
#32390 = VERTEX_POINT ( 'NONE', #51351 ) ;
#32391 = B_SPLINE_CURVE_WITH_KNOTS ( 'NONE', 3,
 ( #47728, #23918, #43048, #85 ),
 .UNSPECIFIED., .F., .F.,
 ( 4, 4 ),
 ( 5.485677294651095664E-18, 0.004050076154992997279 ),
 .UNSPECIFIED. ) ;
#32392 = CARTESIAN_POINT ( 'NONE',  ( 0.1095718737110178420, 21.33933464366368682, 37.47471772507226717 ) ) ;
#32393 = VERTEX_POINT ( 'NONE', #55740 ) ;
#32394 = ADVANCED_FACE ( 'NONE', ( #17554 ), #35064, .F. ) ;
#32395 = VERTEX_POINT ( 'NONE', #47287 ) ;
#32396 = B_SPLINE_CURVE_WITH_KNOTS ( 'NONE', 3,
 ( #34036, #47505, #5174, #28081 ),
 .UNSPECIFIED., .F., .F.,
 ( 4, 4 ),
 ( 0.000000000000000000, 0.005013413432710147645 ),
 .UNSPECIFIED. ) ;
#32397 = CARTESIAN_POINT ( 'NONE',  ( 1.227938101723756947, -29.74462687941247552, 30.94118573761302926 ) ) ;
#32398 = ORIENTED_EDGE ( 'NONE', *, *, #22407, .T. ) ;
#32399 = FACE_OUTER_BOUND ( 'NONE', #20901, .T. ) ;
#32400 = CARTESIAN_POINT ( 'NONE',  ( 4.833616638992205949, 15.29495699393727293, -43.64812679991103295 ) ) ;
#32401 = DIRECTION ( 'NONE',  ( 0.000000000000000000, 0.000000000000000000, -1.000000000000000000 ) ) ;
#32402 = CARTESIAN_POINT ( 'NONE',  ( 4.958415959904820980, -22.27126879049791341, 39.58780797523441208 ) ) ;
#32403 = CARTESIAN_POINT ( 'NONE',  ( 4.553261556744873317, -43.07273893850290136, 8.618510669437750238 ) ) ;
#32404 = VERTEX_POINT ( 'NONE', #37920 ) ;
#32405 = FACE_OUTER_BOUND ( 'NONE', #48812, .T. ) ;
#32406 = CARTESIAN_POINT ( 'NONE',  ( 1.231276596079881047, 32.36747132271556637, 26.63876069172986405 ) ) ;
#32407 = CARTESIAN_POINT ( 'NONE',  ( 0.8760168074887076939, 47.56749362999713782, -7.161346975773211554 ) ) ;
#32408 = VERTEX_POINT ( 'NONE', #31962 ) ;
#32409 = CARTESIAN_POINT ( 'NONE',  ( 4.967162193818130511, 0.000000000000000000, 0.000000000000000000 ) ) ;
#32410 = CARTESIAN_POINT ( 'NONE',  ( 0.2285344041767103096, 30.21943416597249765, 32.14478136469291059 ) ) ;
#32411 = CARTESIAN_POINT ( 'NONE',  ( 0.9756354156337445627, 30.24859376089824536, 30.43287766742259493 ) ) ;
#32412 = CARTESIAN_POINT ( 'NONE',  ( -2.060000000000000941, 2.522772406243548923E-16, -0.3080913168122707546 ) ) ;
#32413 = EDGE_CURVE ( 'NONE', #9792, #59574, #39248, .T. ) ;
#32414 = ORIENTED_EDGE ( 'NONE', *, *, #45557, .T. ) ;
#32415 = CARTESIAN_POINT ( 'NONE',  ( 4.553261556744875094, 7.233533384971297941, -43.32684572631779218 ) ) ;
#32416 = CARTESIAN_POINT ( 'NONE',  ( 5.958863334805807099, -10.26176968287932745, -17.77634700750925134 ) ) ;
#32417 = B_SPLINE_CURVE_WITH_KNOTS ( 'NONE', 3,
 ( #10655, #24123, #29742, #14436, #43261, #15976 ),
 .UNSPECIFIED., .F., .F.,
 ( 4, 2, 4 ),
 ( 3.471140604459641645E-18, 0.0002291459268755744903, 0.0004582918537511455111 ),
 .UNSPECIFIED. ) ;
#32418 = AXIS2_PLACEMENT_3D ( 'NONE', #18556, #9450, #57352 ) ;
#32419 = CARTESIAN_POINT ( 'NONE',  ( 5.894904586330512508, 12.98639672351335328, -15.35848013968714199 ) ) ;
#32420 = ADVANCED_FACE ( 'NONE', ( #46682 ), #7827, .F. ) ;
#32421 = FACE_OUTER_BOUND ( 'NONE', #46974, .T. ) ;
#32422 = CARTESIAN_POINT ( 'NONE',  ( 0.1313383488274147970, -34.59671037481856359, -25.74310646082139442 ) ) ;
#32423 = CARTESIAN_POINT ( 'NONE',  ( 0.3622758884714600280, 15.73321244754796666, 40.13994584881788086 ) ) ;
#32424 = CARTESIAN_POINT ( 'NONE',  ( 0.6000166863083106206, 22.25084548767499015, 43.78039923061538019 ) ) ;
#32425 = CARTESIAN_POINT ( 'NONE',  ( 7.000000000000021316, -80.00000000000001421, -1.954818893553044610E-31 ) ) ;
#32426 = CARTESIAN_POINT ( 'NONE',  ( 0.9769922540276041456, 41.90628016062868255, 0.4418576524454907450 ) ) ;
#32427 = CARTESIAN_POINT ( 'NONE',  ( 5.895881250540457863, -4.666996818433588601, -19.56391633352155779 ) ) ;
#32428 = ORIENTED_EDGE ( 'NONE', *, *, #10966, .F. ) ;
#32429 = FACE_OUTER_BOUND ( 'NONE', #4522, .T. ) ;
#32430 = CARTESIAN_POINT ( 'NONE',  ( 4.963659409799332067, 40.34793212403996421, -19.36487359954654508 ) ) ;
#32431 = CARTESIAN_POINT ( 'NONE',  ( 0.1152809850208375564, -35.22899213320485501, -26.56808980277553900 ) ) ;
#32432 = DIRECTION ( 'NONE',  ( -1.000000000000000000, -3.135800716341471541E-16, -1.298891185607920445E-16 ) ) ;
#32433 = EDGE_CURVE ( 'NONE', #27055, #18471, #22349, .T. ) ;
#32434 = CARTESIAN_POINT ( 'NONE',  ( 2.185380717157382691, -24.04382478636127018, -36.88786104818167644 ) ) ;
#32435 = CARTESIAN_POINT ( 'NONE',  ( 0.1100053167205930216, 42.77858932361496613, 5.450899213259652321 ) ) ;
#32436 = CARTESIAN_POINT ( 'NONE',  ( 0.5834584762367766020, -25.38722266164445429, 39.43000018439352061 ) ) ;
#32437 = CARTESIAN_POINT ( 'NONE',  ( 2.618530812446115519, -39.53489722556178521, -25.43066437516854705 ) ) ;
#32438 = CARTESIAN_POINT ( 'NONE',  ( 4.956445790444026223, 2.113652668516905031, -47.04328350079857302 ) ) ;
#32440 = ORIENTED_EDGE ( 'NONE', *, *, #21706, .T. ) ;
#32439 = CARTESIAN_POINT ( 'NONE',  ( 0.5998501479064699549, -46.60114184914309021, -11.94461217097453343 ) ) ;
#32441 = VERTEX_POINT ( 'NONE', #26949 ) ;
#32442 = CARTESIAN_POINT ( 'NONE',  ( 0.1149546198390367507, -7.312467115531964268, 43.51407116907684269 ) ) ;
#32443 = CARTESIAN_POINT ( 'NONE',  ( 0.1103310638050662290, 39.81020119244058009, 16.57910240621655262 ) ) ;
#32444 = CARTESIAN_POINT ( 'NONE',  ( 5.965394784446460541, -5.326334832595787994, 19.82223131420045092 ) ) ;
#32445 = VERTEX_POINT ( 'NONE', #41995 ) ;
#32446 = CARTESIAN_POINT ( 'NONE',  ( 0.5837157313716030416, 22.45749545691984750, 41.16913845812719330 ) ) ;
#32447 = CARTESIAN_POINT ( 'NONE',  ( -6.077587904424778920, -6.656176160390709917, 18.06907137391894125 ) ) ;
#32448 = CARTESIAN_POINT ( 'NONE',  ( 0.1087620492084206830, 5.987629195157810003, -42.70684898916390893 ) ) ;
#32449 = VERTEX_POINT ( 'NONE', #4032 ) ;
#32450 = EDGE_LOOP ( 'NONE', ( #29378, #25387, #2985, #40668 ) ) ;
#32451 = CARTESIAN_POINT ( 'NONE',  ( 0.9752570700956822991, 41.38610171411352212, 11.32817567195924902 ) ) ;
#32452 = CARTESIAN_POINT ( 'NONE',  ( 4.226256110419178924, 38.08231154255455664, 21.92178819264073653 ) ) ;
#32453 = CARTESIAN_POINT ( 'NONE',  ( 0.5817217712918327788, 46.89379117910313255, 0.4553052372231276568 ) ) ;
#32454 = EDGE_CURVE ( 'NONE', #36974, #21596, #25798, .T. ) ;
#32455 = CARTESIAN_POINT ( 'NONE',  ( 0.8551540677456715978, 47.61725548905990735, 5.348818140991062009 ) ) ;
#32456 = EDGE_CURVE ( 'NONE', #38817, #48578, #53409, .T. ) ;
#32457 = CARTESIAN_POINT ( 'NONE',  ( 0.1156495703730067437, -42.71546320847479450, -11.06038679778003875 ) ) ;
#32458 = AXIS2_PLACEMENT_3D ( 'NONE', #21610, #17844, #40750 ) ;
#32459 = CARTESIAN_POINT ( 'NONE',  ( 5.901463166500146684, 5.972693816097455866, 19.20533256467557237 ) ) ;
#32460 = ORIENTED_EDGE ( 'NONE', *, *, #30838, .T. ) ;
#32461 = EDGE_CURVE ( 'NONE', #40550, #35241, #55323, .T. ) ;
#32462 = EDGE_CURVE ( 'NONE', #8721, #7194, #51979, .T. ) ;
#32463 = DIRECTION ( 'NONE',  ( 1.000000000000000000, 0.000000000000000000, 0.000000000000000000 ) ) ;
#32464 = DIRECTION ( 'NONE',  ( 0.07906939808003035641, -0.5848023231963108692, -0.8073129957280876789 ) ) ;
#32465 = ORIENTED_EDGE ( 'NONE', *, *, #60948, .T. ) ;
#32466 = CARTESIAN_POINT ( 'NONE',  ( 0.6023143664670691511, -47.66103278671586452, -6.538774821499023560 ) ) ;
#32467 = ADVANCED_FACE ( 'NONE', ( #42300 ), #50379, .F. ) ;
#32468 = CARTESIAN_POINT ( 'NONE',  ( -6.078726893082806448, 16.77644806189623239, -9.452239506869167585 ) ) ;
#32469 = CARTESIAN_POINT ( 'NONE',  ( 0.7056759521544981872, 46.36311911575824496, 7.085902551898405122 ) ) ;
#32470 = CARTESIAN_POINT ( 'NONE',  ( 0.2279481005628813950, -34.89833595118959408, -26.99277004886345210 ) ) ;
#32471 = CIRCLE ( 'NONE', #5430, 48.09070567114147110 ) ;
#32472 = VERTEX_POINT ( 'NONE', #4335 ) ;
#32473 = ORIENTED_EDGE ( 'NONE', *, *, #53168, .T. ) ;
#32474 = CARTESIAN_POINT ( 'NONE',  ( 0.9756950546413931669, 0.09673755062796540738, 42.90834738653779823 ) ) ;
#32475 = CARTESIAN_POINT ( 'NONE',  ( 0.08486401232817714080, 0.000000000000000000, 0.000000000000000000 ) ) ;
#32476 = LINE ( 'NONE', #32795, #39190 ) ;
#32477 = EDGE_CURVE ( 'NONE', #21542, #3021, #23471, .T. ) ;
#32478 = ORIENTED_EDGE ( 'NONE', *, *, #35446, .T. ) ;
#32479 = CARTESIAN_POINT ( 'NONE',  ( 0.8551540677456739292, 29.88829867897867842, -37.45266983663464799 ) ) ;
#32480 = VERTEX_POINT ( 'NONE', #25026 ) ;
#32481 = CARTESIAN_POINT ( 'NONE',  ( 0.5549461598389365813, 43.45051165307260277, 7.567742896862155177 ) ) ;
#32482 = CARTESIAN_POINT ( 'NONE',  ( 4.967162193818130511, 35.57684288742009215, -24.30453456948074376 ) ) ;
#32483 = EDGE_CURVE ( 'NONE', #44510, #34393, #364, .T. ) ;
#32484 = CARTESIAN_POINT ( 'NONE',  ( 3.661933894777862797, 46.33057283091471845, 8.130755568270412681 ) ) ;
#32485 = ORIENTED_EDGE ( 'NONE', *, *, #57022, .T. ) ;
#32486 = B_SPLINE_CURVE_WITH_KNOTS ( 'NONE', 3,
 ( #6843, #25981, #2142, #59477 ),
 .UNSPECIFIED., .F., .F.,
 ( 4, 4 ),
 ( 6.254634441385501517E-18, 0.004566006591234645501 ),
 .UNSPECIFIED. ) ;
#32487 = CARTESIAN_POINT ( 'NONE',  ( 2.528190830796656741, 33.68156755522954882, -25.05606000901808983 ) ) ;
#32488 = CARTESIAN_POINT ( 'NONE',  ( -6.079354080745853928, -4.283721817891463779, 18.77345686428268934 ) ) ;
#32489 = CARTESIAN_POINT ( 'NONE',  ( 0.5806925824938499181, -42.09901922557445175, 20.66143612114793626 ) ) ;
#32490 = ADVANCED_BREP_SHAPE_REPRESENTATION ( '', ( #52453, #14677 ), #18740 ) ;
#32491 = ORIENTED_EDGE ( 'NONE', *, *, #7190, .F. ) ;
#32492 = CARTESIAN_POINT ( 'NONE',  ( 0.3676999524040366896, 24.55639947021014180, -36.64606156713571750 ) ) ;
#32493 =( BOUNDED_SURFACE ( )  B_SPLINE_SURFACE ( 3, 1, ( 
 ( #53129, #1125 ),
 ( #506, #19647 ),
 ( #10236, #188 ),
 ( #57822, #20264 ) ),
 .UNSPECIFIED., .F., .F., .F. ) 
 B_SPLINE_SURFACE_WITH_KNOTS ( ( 4, 4 ),
 ( 2, 2 ),
 ( 0.000000000000000000, 1.000000000000000000 ),
 ( 0.000000000000000000, 1.000000000000000000 ),
 .UNSPECIFIED. ) 
 GEOMETRIC_REPRESENTATION_ITEM ( )  RATIONAL_B_SPLINE_SURFACE ( (
 ( 1.000000000000000000, 1.000000000000000000),
 ( 0.9952954269826590483, 0.8620686068821339365),
 ( 0.9952954269826590483, 0.8620686068821339365),
 ( 1.000000000000000000, 1.000000000000000000) ) ) 
 REPRESENTATION_ITEM ( '' )  SURFACE ( )  );
#32494 = CARTESIAN_POINT ( 'NONE',  ( 50.15577769773999961, 0.000000000000000000, 10.00000000000000000 ) ) ;
#32495 = CARTESIAN_POINT ( 'NONE',  ( 0.5998501479064708430, -24.50586714782633280, 41.39809967730445095 ) ) ;
#32496 = VECTOR ( 'NONE', #57521, 1000.000000000000114 ) ;
#32497 = CARTESIAN_POINT ( 'NONE',  ( 4.967162193818131399, 42.16965968614193372, 8.839793687085363061 ) ) ;
#32498 = B_SPLINE_CURVE_WITH_KNOTS ( 'NONE', 3,
 ( #18818, #27277, #46400, #60772, #17893, #37017 ),
 .UNSPECIFIED., .F., .F.,
 ( 4, 2, 4 ),
 ( 1.285010118223292934E-16, 0.0002450741128632324506, 0.0004901482257263364232 ),
 .UNSPECIFIED. ) ;
#32499 = CARTESIAN_POINT ( 'NONE',  ( 0.5797568599927134247, 36.41064399614844405, 29.55486952190357997 ) ) ;
#32500 = ORIENTED_EDGE ( 'NONE', *, *, #49508, .T. ) ;
#32501 = CARTESIAN_POINT ( 'NONE',  ( -6.079354080745853928, 5.479977851902325447, -18.45976159084461088 ) ) ;
#32502 = DIRECTION ( 'NONE',  ( 0.000000000000000000, -1.000000000000000000, 1.287488025362403787E-15 ) ) ;
#32503 = EDGE_LOOP ( 'NONE', ( #2681, #17111, #22732 ) ) ;
#32504 = DIRECTION ( 'NONE',  ( -1.000000000000000000, 0.000000000000000000, 0.000000000000000000 ) ) ;
#32505 = LINE ( 'NONE', #50663, #41380 ) ;
#32506 = CARTESIAN_POINT ( 'NONE',  ( 4.975801465491695552, 45.55012473237732706, 14.85979367497190040 ) ) ;
#32507 = CARTESIAN_POINT ( 'NONE',  ( 0.9757892942422833338, 5.549787678908993271, -42.54806590760148310 ) ) ;
#32508 = EDGE_CURVE ( 'NONE', #2406, #29558, #26578, .T. ) ;
#32509 = CARTESIAN_POINT ( 'NONE',  ( 5.959547316686252039, -10.26589671991350983, -17.77392908783930636 ) ) ;
#32510 = DIRECTION ( 'NONE',  ( 0.000000000000000000, 1.000000000000000000, 0.000000000000000000 ) ) ;
#32512 = B_SPLINE_CURVE_WITH_KNOTS ( 'NONE', 3,
 ( #1406, #25851, #54644, #40298, #16455, #29620 ),
 .UNSPECIFIED., .F., .F.,
 ( 4, 2, 4 ),
 ( 2.197015137584159369E-17, 0.0002293755540694313998, 0.0004587511081388407903 ),
 .UNSPECIFIED. ) ;
#32511 = CARTESIAN_POINT ( 'NONE',  ( 0.5836750258453337059, -47.89563095930320458, -0.1816059738421414715 ) ) ;
#32513 = CARTESIAN_POINT ( 'NONE',  ( 4.956445790444004906, -46.59545590650544966, 6.811867512257108181 ) ) ;
#32514 = EDGE_CURVE ( 'NONE', #25197, #48814, #15389, .T. ) ;
#32515 = CARTESIAN_POINT ( 'NONE',  ( 0.6846871229502899947, 41.05093867799220675, -24.69859318104445833 ) ) ;
#32516 = CARTESIAN_POINT ( 'NONE',  ( 0.7246131072078548785, -44.12003537001164233, -19.16331062551070730 ) ) ;
#32517 = VECTOR ( 'NONE', #55654, 1000.000000000000000 ) ;
#32518 = FACE_OUTER_BOUND ( 'NONE', #49792, .T. ) ;
#32519 = ORIENTED_EDGE ( 'NONE', *, *, #44370, .F. ) ;
#32520 = AXIS2_PLACEMENT_3D ( 'NONE', #17272, #31362, #45478 ) ;
#32521 = CARTESIAN_POINT ( 'NONE',  ( 0.8554163680231708922, -41.45413358837855355, -21.97180651536612928 ) ) ;
#32522 = CARTESIAN_POINT ( 'NONE',  ( 0.6028777368367060907, -1.486945628974875477, -49.08491440358785241 ) ) ;
#32523 = CARTESIAN_POINT ( 'NONE',  ( 0.3676999524040366896, 16.00695768809390884, 41.10629986868691077 ) ) ;
#32524 = AXIS2_PLACEMENT_3D ( 'NONE', #5693, #24841, #16362 ) ;
#32525 = CARTESIAN_POINT ( 'NONE',  ( 0.7246131072078569879, -48.09507913767667020, -0.8205838906001429178 ) ) ;
#32526 = CARTESIAN_POINT ( 'NONE',  ( 0.5837799406558231707, 46.48971530503088445, 6.160350674627294687 ) ) ;
#32527 = CARTESIAN_POINT ( 'NONE',  ( 2.185380717157383579, 32.57763254378428996, -29.62292458400025197 ) ) ;
#32528 = VERTEX_POINT ( 'NONE', #10622 ) ;
#32529 = CARTESIAN_POINT ( 'NONE',  ( 4.956653778117001252, 47.27023054223765541, -8.845409907520457082 ) ) ;
#32530 = CARTESIAN_POINT ( 'NONE',  ( -6.001507490154110336, -18.68469198366095085, -2.444174634178336358 ) ) ;
#32531 = CARTESIAN_POINT ( 'NONE',  ( 1.112077966505211624, 28.84925631676179236, -33.32792725475640339 ) ) ;
#32532 = CARTESIAN_POINT ( 'NONE',  ( 0.6845945791218023269, -25.96635969083004980, -39.06602981005851660 ) ) ;
#32533 = VERTEX_POINT ( 'NONE', #19108 ) ;
#32534 = ADVANCED_FACE ( 'NONE', ( #58204 ), #36705, .F. ) ;
#32535 = CARTESIAN_POINT ( 'NONE',  ( -15.25000000000000711, -2.688986455804108555, -9.952330921218299798E-16 ) ) ;
#32536 = B_SPLINE_CURVE_WITH_KNOTS ( 'NONE', 3,
 ( #39715, #58766, #54069, #11190 ),
 .UNSPECIFIED., .F., .F.,
 ( 4, 4 ),
 ( 2.308109569601360422E-17, 0.004559932413162187670 ),
 .UNSPECIFIED. ) ;
#32537 = EDGE_CURVE ( 'NONE', #19087, #52200, #4143, .T. ) ;
#32538 = CARTESIAN_POINT ( 'NONE',  ( 0.5998501479064699549, 23.59887241503354716, -41.92175333043595487 ) ) ;
#32539 = ORIENTED_EDGE ( 'NONE', *, *, #32483, .F. ) ;
#32540 = B_SPLINE_CURVE_WITH_KNOTS ( 'NONE', 3,
 ( #60699, #36624, #55693, #46639, #41952, #56315, #17819, #12824, #3992, #46335, #23132, #36944, #18127, #37247, #13429, #32538 ),
 .UNSPECIFIED., .F., .F.,
 ( 4, 3, 3, 3, 3, 4 ),
 ( 1.868480190406682863E-17, 0.0002618515315864432236, 0.0003927756766342012438, 0.0005236998216950575647, 0.0007855159896329922840, 0.001047349442285927003 ),
 .UNSPECIFIED. ) ;
#32541 = CARTESIAN_POINT ( 'NONE',  ( -6.078457390727109555, -6.646245994447022909, -18.07268450504254176 ) ) ;
#32542 = ORIENTED_EDGE ( 'NONE', *, *, #35946, .F. ) ;
#32543 = EDGE_CURVE ( 'NONE', #22775, #45810, #59351, .T. ) ;
#32544 = EDGE_CURVE ( 'NONE', #10228, #28932, #15328, .T. ) ;
#32545 = CARTESIAN_POINT ( 'NONE',  ( 4.335381028904201628, -28.85261930641560468, -39.58892783119288339 ) ) ;
#32546 = CARTESIAN_POINT ( 'NONE',  ( -2.000000000000009770, 3.464101615137749057, -5.600000000000000533 ) ) ;
#32547 = ORIENTED_EDGE ( 'NONE', *, *, #30468, .T. ) ;
#32548 = FACE_OUTER_BOUND ( 'NONE', #43895, .T. ) ;
#32549 = EDGE_CURVE ( 'NONE', #17351, #21388, #34808, .T. ) ;
#32550 = CARTESIAN_POINT ( 'NONE',  ( 0.5838002273316420521, -29.26514720557047156, 37.91535410490859448 ) ) ;
#32551 = ORIENTED_EDGE ( 'NONE', *, *, #15155, .F. ) ;
#32552 = CARTESIAN_POINT ( 'NONE',  ( 0.9752570700956790795, 21.25416333281098957, 37.27462300504085135 ) ) ;
#32553 = CARTESIAN_POINT ( 'NONE',  ( 0.5987334363312690755, -43.08218153649183790, 23.56880439328305243 ) ) ;
#32554 = ORIENTED_EDGE ( 'NONE', *, *, #37865, .T. ) ;
#32555 = CARTESIAN_POINT ( 'NONE',  ( 0.9762797500689124330, -6.471194619075235188, -41.40589843715211771 ) ) ;
#32556 = ORIENTED_EDGE ( 'NONE', *, *, #49452, .F. ) ;
#32557 = CARTESIAN_POINT ( 'NONE',  ( 0.8560838555295223751, -39.18289055412714106, -25.78902716088815694 ) ) ;
#32558 = VECTOR ( 'NONE', #54079, 1000.000000000000227 ) ;
#32559 = ORIENTED_EDGE ( 'NONE', *, *, #10261, .F. ) ;
#32560 = ORIENTED_EDGE ( 'NONE', *, *, #45215, .T. ) ;
#32561 = CARTESIAN_POINT ( 'NONE',  ( 4.975801465491694664, 46.87746200127440943, 9.906103548668390602 ) ) ;
#32562 = CARTESIAN_POINT ( 'NONE',  ( 0.6846871229502932144, 47.60345020167359564, -5.395516691086709393 ) ) ;
#32563 = CARTESIAN_POINT ( 'NONE',  ( 0.5839879327111914264, 29.22928252017514339, 37.94312859586424480 ) ) ;
#32564 = AXIS2_PLACEMENT_3D ( 'NONE', #44954, #15815, #10808 ) ;
#32565 = CARTESIAN_POINT ( 'NONE',  ( 0.1087620492084205720, -16.83695155255859177, 39.70193592734176491 ) ) ;
#32566 = CARTESIAN_POINT ( 'NONE',  ( 5.960721111146673579, 16.28787783074210438, 12.49016043756476790 ) ) ;
#32567 = ORIENTED_EDGE ( 'NONE', *, *, #30571, .F. ) ;
#32568 = CARTESIAN_POINT ( 'NONE',  ( 0.9757892942422822236, 11.15510465569001575, 41.43309903783659109 ) ) ;
#32569 = CARTESIAN_POINT ( 'NONE',  ( 0.8551540677456834771, -5.348818140991232539, 47.61725548905988603 ) ) ;
#32570 = CARTESIAN_POINT ( 'NONE',  ( 0.9730545539215883499, 21.89037132892487847, -36.90443313492307453 ) ) ;
#32571 = AXIS2_PLACEMENT_3D ( 'NONE', #34499, #53567, #49504 ) ;
#32572 = EDGE_LOOP ( 'NONE', ( #54057, #41425, #24305, #33382 ) ) ;
#32573 = ORIENTED_EDGE ( 'NONE', *, *, #36719, .T. ) ;
#32574 = CARTESIAN_POINT ( 'NONE',  ( 0.1092355843206037486, -21.30139719602345494, -37.49628696754451340 ) ) ;
#32575 = CARTESIAN_POINT ( 'NONE',  ( -2.708315649062910779, 14.54141329178162323, -1.648584381066900306 ) ) ;
#32576 = CARTESIAN_POINT ( 'NONE',  ( 2.624215991343608501, 13.78323291683847351, -45.98641578154015974 ) ) ;
#32577 = CARTESIAN_POINT ( 'NONE',  ( 0.1097557419366048670, -34.07666148910663395, 26.42915440612274125 ) ) ;
#32578 = CARTESIAN_POINT ( 'NONE',  ( 2.533389852662419894, -34.30621192938689745, 27.57778734397685483 ) ) ;
#32579 =( BOUNDED_SURFACE ( )  B_SPLINE_SURFACE ( 3, 1, ( 
 ( #4000, #60705 ),
 ( #31608, #4303 ),
 ( #13434, #3690 ),
 ( #42566, #46046 ) ),
 .UNSPECIFIED., .F., .F., .F. ) 
 B_SPLINE_SURFACE_WITH_KNOTS ( ( 4, 4 ),
 ( 2, 2 ),
 ( 0.000000000000000000, 1.000000000000000000 ),
 ( 0.000000000000000000, 1.000000000000000000 ),
 .UNSPECIFIED. ) 
 GEOMETRIC_REPRESENTATION_ITEM ( )  RATIONAL_B_SPLINE_SURFACE ( (
 ( 1.000000000000000000, 1.000000000000000000),
 ( 0.9953390228620291325, 0.8624445117761032620),
 ( 0.9953390228620291325, 0.8624445117761032620),
 ( 1.000000000000000000, 1.000000000000000000) ) ) 
 REPRESENTATION_ITEM ( '' )  SURFACE ( )  );
#32580 = VERTEX_POINT ( 'NONE', #29710 ) ;
#32581 = LINE ( 'NONE', #8752, #34931 ) ;
#32582 = CARTESIAN_POINT ( 'NONE',  ( 0.9762797500689124330, -17.18051571332144434, 38.22505284509125545 ) ) ;
#32583 = CARTESIAN_POINT ( 'NONE',  ( 3.050102900204245682, 42.79960004823801967, -10.17936564275614053 ) ) ;
#32584 = CARTESIAN_POINT ( 'NONE',  ( 2.706805983486679779, -39.13097409860326081, -20.13809771091093381 ) ) ;
#32585 = CARTESIAN_POINT ( 'NONE',  ( 1.834102595619085285, -41.29959790234792649, -15.31473009759111825 ) ) ;
#32586 = CARTESIAN_POINT ( 'NONE',  ( 0.5988103622719987973, -5.677495780220720434, -47.77151394449995792 ) ) ;
#32587 = EDGE_CURVE ( 'NONE', #26593, #3829, #60329, .T. ) ;
#32588 = ORIENTED_EDGE ( 'NONE', *, *, #22149, .T. ) ;
#32589 = CARTESIAN_POINT ( 'NONE',  ( 4.956653778116991482, -21.75875759808677046, -42.88673967249153662 ) ) ;
#32590 = CARTESIAN_POINT ( 'NONE',  ( 0.2230388203127614266, 4.873876086128248630, -42.84312106681679921 ) ) ;
#32591 = CARTESIAN_POINT ( 'NONE',  ( 0.5782707292762423457, -7.086273146448189841, 46.36292793387347899 ) ) ;
#32592 = CARTESIAN_POINT ( 'NONE',  ( 0.1098349054025746369, -16.30574661324343566, -39.92296693299701360 ) ) ;
#32593 = CARTESIAN_POINT ( 'NONE',  ( 0.9790724872846768845, 29.10550071523391225, 30.15302701383349060 ) ) ;
#32594 = CARTESIAN_POINT ( 'NONE',  ( 0.5806925824938499181, -14.41498975133639426, 44.62544602368059543 ) ) ;
#32595 = DIRECTION ( 'NONE',  ( 0.000000000000000000, 0.000000000000000000, -1.000000000000000000 ) ) ;
#32596 = CARTESIAN_POINT ( 'NONE',  ( 0.5832655196449149093, 22.73672770770176399, -41.01556285264354784 ) ) ;
#32597 = CARTESIAN_POINT ( 'NONE',  ( 2.618530812446111078, 31.65223561859532708, 34.75432015653772311 ) ) ;
#32598 = ORIENTED_EDGE ( 'NONE', *, *, #56084, .T. ) ;
#32599 = CARTESIAN_POINT ( 'NONE',  ( 0.8557997880470690211, -43.90420959842193582, 19.17299735371994629 ) ) ;
#32600 = AXIS2_PLACEMENT_3D ( 'NONE', #47483, #43107, #144 ) ;
#32601 = CARTESIAN_POINT ( 'NONE',  ( 0.5839879327111922036, 46.28746210677714146, 12.30864801674728604 ) ) ;
#32602 = DIRECTION ( 'NONE',  ( -0.1011922191286467321, -0.6783146913069645345, 0.7277700971769569538 ) ) ;
#32603 = CARTESIAN_POINT ( 'NONE',  ( 0.8560838555295223751, 42.82099363437819051, -19.15033519931896322 ) ) ;
#32604 = ORIENTED_EDGE ( 'NONE', *, *, #55780, .F. ) ;
#32605 = CARTESIAN_POINT ( 'NONE',  ( 0.6845945791218023269, -45.78817307429886796, 10.19066863517794985 ) ) ;
#32606 = CIRCLE ( 'NONE', #16597, 42.08604991992415023 ) ;
#32607 = CARTESIAN_POINT ( 'NONE',  ( 1.231276596079887264, 35.62927148397050559, -22.08691432816256395 ) ) ;
#32608 = ADVANCED_FACE ( 'NONE', ( #47598 ), #24360, .F. ) ;
#32609 = ORIENTED_EDGE ( 'NONE', *, *, #49449, .T. ) ;
#32610 = LINE ( 'NONE', #23204, #8041 ) ;
#32611 = CARTESIAN_POINT ( 'NONE',  ( 4.553261556744873317, 31.71129487083125653, 30.39627186743183174 ) ) ;
#32612 = EDGE_CURVE ( 'NONE', #60714, #47165, #22811, .T. ) ;
#32613 = CARTESIAN_POINT ( 'NONE',  ( 2.528190830796658517, 25.86513783113687737, -33.06431280291939601 ) ) ;
#32614 = ORIENTED_EDGE ( 'NONE', *, *, #54814, .T. ) ;
#32615 = AXIS2_PLACEMENT_3D ( 'NONE', #31972, #41385, #22874 ) ;
#32616 = CARTESIAN_POINT ( 'NONE',  ( 6.000000000000000888, -15.14599999999998658, 1.854850041988580043E-15 ) ) ;
#32617 = VERTEX_POINT ( 'NONE', #30630 ) ;
#32618 = EDGE_CURVE ( 'NONE', #56342, #43333, #54423, .T. ) ;
#32619 = VERTEX_POINT ( 'NONE', #20633 ) ;
#32620 = CARTESIAN_POINT ( 'NONE',  ( 0.5804410086790514622, -20.23572001627617922, 42.30881098870867874 ) ) ;
#32621 = CARTESIAN_POINT ( 'NONE',  ( -6.078726893082806448, 5.475592473157615991, -18.46109228449443052 ) ) ;
#32622 = ORIENTED_EDGE ( 'NONE', *, *, #2595, .T. ) ;
#32623 = CARTESIAN_POINT ( 'NONE',  ( 0.8554163680231708922, -14.77070554666881286, 44.53124443315531522 ) ) ;
#32624 = VERTEX_POINT ( 'NONE', #16243 ) ;
#32625 = CARTESIAN_POINT ( 'NONE',  ( 0.5848930533535030563, 45.27791896734265720, 12.21405487028406966 ) ) ;
#32626 = CARTESIAN_POINT ( 'NONE',  ( 0.7954196712028469562, 48.09103417491925114, 0.8690072546827309896 ) ) ;
#32627 = CARTESIAN_POINT ( 'NONE',  ( 2.500000000000000000, 0.000000000000000000, 0.000000000000000000 ) ) ;
#32628 = ORIENTED_EDGE ( 'NONE', *, *, #19420, .F. ) ;
#32629 = CARTESIAN_POINT ( 'NONE',  ( 0.9749527285493303497, -16.15611883305616203, -39.75066842359304076 ) ) ;
#32630 = EDGE_CURVE ( 'NONE', #60778, #23902, #11552, .T. ) ;
#32631 = CARTESIAN_POINT ( 'NONE',  ( 0.5804410086790514622, 22.05813747677496295, -41.38790189066234859 ) ) ;
#32632 = CARTESIAN_POINT ( 'NONE',  ( 0.5830081025819929819, -44.39003745708693316, -15.12470194551506886 ) ) ;
#32633 = CARTESIAN_POINT ( 'NONE',  ( 0.5806925824938502512, 17.36345040154772690, 43.56297685531322372 ) ) ;
#32634 = EDGE_LOOP ( 'NONE', ( #1262, #12938, #9926, #33010 ) ) ;
#32635 = CARTESIAN_POINT ( 'NONE',  ( 0.6846871229502899947, 13.23224427737829245, 46.04462816497493094 ) ) ;
#32636 = EDGE_CURVE ( 'NONE', #49531, #31692, #45399, .T. ) ;
#32637 = DIRECTION ( 'NONE',  ( -1.000000000000000000, -0.000000000000000000, -0.000000000000000000 ) ) ;
#32638 = VERTEX_POINT ( 'NONE', #16873 ) ;
#32639 = CARTESIAN_POINT ( 'NONE',  ( 4.549368137175248350, 32.41327393324141326, -28.14399996863463116 ) ) ;
#32640 = VERTEX_POINT ( 'NONE', #40085 ) ;
#32641 = CARTESIAN_POINT ( 'NONE',  ( 0.8751705887134553219, -7.160166390003972481, -47.55935879196468363 ) ) ;
#32642 = CARTESIAN_POINT ( 'NONE',  ( 0.5824936645240081923, 11.22543641052009811, -45.53271083994098234 ) ) ;
#32643 = ORIENTED_EDGE ( 'NONE', *, *, #8861, .T. ) ;
#32644 = CARTESIAN_POINT ( 'NONE',  ( 0.9787284016396619046, -34.65686640017599274, -23.56348043581808227 ) ) ;
#32645 = CARTESIAN_POINT ( 'NONE',  ( 4.967162193818130511, -28.74031574030035685, 32.10009971360062764 ) ) ;
#32646 = CARTESIAN_POINT ( 'NONE',  ( 0.6026777506516367566, 28.23790448320244550, 40.17669898130948525 ) ) ;
#32647 = DIRECTION ( 'NONE',  ( 0.000000000000000000, -1.047444401652941269E-14, 1.000000000000000000 ) ) ;
#32648 = VECTOR ( 'NONE', #41192, 1000.000000000000000 ) ;
#32649 = ORIENTED_EDGE ( 'NONE', *, *, #33170, .F. ) ;
#32650 = DIRECTION ( 'NONE',  ( -1.000000000000000000, 0.000000000000000000, -0.000000000000000000 ) ) ;
#32651 = CIRCLE ( 'NONE', #40675, 43.08621763946400307 ) ;
#32652 = CARTESIAN_POINT ( 'NONE',  ( 5.960221823109900008, 17.77840967225720448, -10.25807604135603235 ) ) ;
#32653 = CARTESIAN_POINT ( 'NONE',  ( -5.995132425357893702, -17.41298668506975744, 7.203480333239017597 ) ) ;
#32654 = CARTESIAN_POINT ( 'NONE',  ( 0.5837374860065642768, -44.31936661703457503, -18.16107481025645498 ) ) ;
#32655 = B_SPLINE_CURVE_WITH_KNOTS ( 'NONE', 3,
 ( #61125, #47667, #55817, #57044 ),
 .UNSPECIFIED., .F., .F.,
 ( 4, 4 ),
 ( 0.000000000000000000, 0.005004948556313801832 ),
 .UNSPECIFIED. ) ;
#32656 = B_SPLINE_CURVE_WITH_KNOTS ( 'NONE', 3,
 ( #5768, #44058, #1086, #27066, #31454, #7631 ),
 .UNSPECIFIED., .F., .F.,
 ( 4, 2, 4 ),
 ( 0.000000000000000000, 0.0002291966416970791327, 0.0004583932833941582654 ),
 .UNSPECIFIED. ) ;
#32657 = DIRECTION ( 'NONE',  ( 1.000000000000000000, -0.000000000000000000, -0.000000000000000000 ) ) ;
#32658 = FACE_OUTER_BOUND ( 'NONE', #12822, .T. ) ;
#32659 = EDGE_CURVE ( 'NONE', #22415, #5939, #20592, .T. ) ;
#32660 = CARTESIAN_POINT ( 'NONE',  ( 1.000110580585051867, -13.04367042783479391, 39.82813257663394069 ) ) ;
#32661 = CIRCLE ( 'NONE', #25669, 47.09074272231896430 ) ;
#32662 = CARTESIAN_POINT ( 'NONE',  ( 0.2279481005628849200, -41.17370996425396612, 15.85020803814284385 ) ) ;
#32663 = CARTESIAN_POINT ( 'NONE',  ( 3.661921753702002569, -33.59527669226428515, 32.92398074055204660 ) ) ;
#32664 = CARTESIAN_POINT ( 'NONE',  ( 5.960221823109900008, 19.82761049839341894, -5.307149561567879203 ) ) ;
#32665 = EDGE_CURVE ( 'NONE', #47413, #42220, #27248, .T. ) ;
#32666 = CARTESIAN_POINT ( 'NONE',  ( 1.227938101723756947, 33.52879263017899092, -26.79402671879293507 ) ) ;
#32667 = CARTESIAN_POINT ( 'NONE',  ( 2.281351352603289584, -1.314116150903787084, 47.95523304704244083 ) ) ;
#32668 = CARTESIAN_POINT ( 'NONE',  ( 0.6001305935487422083, 29.70149728382386556, 37.84751346122865101 ) ) ;
#32669 = CARTESIAN_POINT ( 'NONE',  ( -6.016761891674565099, 14.94721834528414917, 11.47373234755508342 ) ) ;
#32670 = LINE ( 'NONE', #27647, #19750 ) ;
#32671 =( BOUNDED_SURFACE ( )  B_SPLINE_SURFACE ( 3, 1, ( 
 ( #7653, #41522 ),
 ( #22702, #60584 ),
 ( #36827, #59982 ),
 ( #21782, #27396 ) ),
 .UNSPECIFIED., .F., .F., .F. ) 
 B_SPLINE_SURFACE_WITH_KNOTS ( ( 4, 4 ),
 ( 2, 2 ),
 ( 0.000000000000000000, 1.000000000000000000 ),
 ( 0.000000000000000000, 1.000000000000000000 ),
 .UNSPECIFIED. ) 
 GEOMETRIC_REPRESENTATION_ITEM ( )  RATIONAL_B_SPLINE_SURFACE ( (
 ( 1.000000000000000000, 1.000000000000000000),
 ( 0.7223157951917480446, 0.9931996967497186413),
 ( 0.7223157951917480446, 0.9931996967497186413),
 ( 1.000000000000000000, 1.000000000000000000) ) ) 
 REPRESENTATION_ITEM ( '' )  SURFACE ( )  );
#32672 = DIRECTION ( 'NONE',  ( -1.000000000000000000, -0.000000000000000000, -0.000000000000000000 ) ) ;
#32673 = CARTESIAN_POINT ( 'NONE',  ( 1.154321485836935279, 11.90271791109313071, 41.23280395520811226 ) ) ;
#32675 = VERTEX_POINT ( 'NONE', #45689 ) ;
#32674 = CARTESIAN_POINT ( 'NONE',  ( 0.9758171775293918992, 39.64453667157746253, 16.41489794146139758 ) ) ;
#32676 = DIRECTION ( 'NONE',  ( 0.000000000000000000, 0.000000000000000000, -1.000000000000000000 ) ) ;
#32677 = CARTESIAN_POINT ( 'NONE',  ( 2.643462169533613793, -46.02269433264243048, 13.76277278785480540 ) ) ;
#32678 = FACE_OUTER_BOUND ( 'NONE', #10121, .T. ) ;
#32679 = ORIENTED_EDGE ( 'NONE', *, *, #39411, .T. ) ;
#32680 = ORIENTED_EDGE ( 'NONE', *, *, #40265, .F. ) ;
#32681 = CARTESIAN_POINT ( 'NONE',  ( 0.5809828226811617480, -34.25055090842177208, 33.48000389720603920 ) ) ;
#32682 = CARTESIAN_POINT ( 'NONE',  ( 0.3676999524040366896, 14.45783756353458216, -41.67639039443420756 ) ) ;
#32683 =( BOUNDED_SURFACE ( )  B_SPLINE_SURFACE ( 3, 1, ( 
 ( #39394, #15573 ),
 ( #34679, #10877 ),
 ( #58754, #7683 ),
 ( #55603, #26812 ) ),
 .UNSPECIFIED., .F., .F., .F. ) 
 B_SPLINE_SURFACE_WITH_KNOTS ( ( 4, 4 ),
 ( 2, 2 ),
 ( 0.000000000000000000, 1.000000000000000000 ),
 ( 0.000000000000000000, 1.000000000000000000 ),
 .UNSPECIFIED. ) 
 GEOMETRIC_REPRESENTATION_ITEM ( )  RATIONAL_B_SPLINE_SURFACE ( (
 ( 1.000000000000000000, 1.000000000000000000),
 ( 0.9729067724841187204, 0.9999501103223794596),
 ( 0.9729067724841187204, 0.9999501103223794596),
 ( 1.000000000000000000, 1.000000000000000000) ) ) 
 REPRESENTATION_ITEM ( '' )  SURFACE ( )  );
#32684 = ORIENTED_EDGE ( 'NONE', *, *, #15884, .F. ) ;
#32685 = VERTEX_POINT ( 'NONE', #21870 ) ;
#32686 = CARTESIAN_POINT ( 'NONE',  ( 0.6031356755773454870, -38.16621646312189142, -29.28593560184418365 ) ) ;
#32687 = EDGE_CURVE ( 'NONE', #27345, #1527, #30326, .T. ) ;
#32688 = AXIS2_PLACEMENT_3D ( 'NONE', #36832, #2971, #16789 ) ;
#32689 = CARTESIAN_POINT ( 'NONE',  ( 4.975610109902397937, 14.46773809681547718, 46.72401910687614190 ) ) ;
#32690 = CIRCLE ( 'NONE', #48686, 47.91270532121795611 ) ;
#32691 = CARTESIAN_POINT ( 'NONE',  ( 4.833616638992208614, -8.578242093416086789, 45.44786513329582789 ) ) ;
#32692 = AXIS2_PLACEMENT_3D ( 'NONE', #26200, #2383, #59397 ) ;
#32693 = ORIENTED_EDGE ( 'NONE', *, *, #55429, .T. ) ;
#32694 = EDGE_CURVE ( 'NONE', #8818, #14042, #29450, .T. ) ;
#32695 = VERTEX_POINT ( 'NONE', #25948 ) ;
#32696 = CARTESIAN_POINT ( 'NONE',  ( 4.962356264823593044, 27.50309822711036034, 31.85616401534038644 ) ) ;
#32697 = ORIENTED_EDGE ( 'NONE', *, *, #50202, .T. ) ;
#32698 = DIRECTION ( 'NONE',  ( -1.000000000000000000, -1.836909530733573776E-16, 1.925929944387235853E-32 ) ) ;
#32699 = CARTESIAN_POINT ( 'NONE',  ( 4.975610109902397937, -32.45573888811600227, -36.59336579715246529 ) ) ;
#32700 = CARTESIAN_POINT ( 'NONE',  ( 0.1103310638050661874, -30.43528225250919661, -30.55179781597986732 ) ) ;
#32701 = VERTEX_POINT ( 'NONE', #54113 ) ;
#32702 = B_SPLINE_CURVE_WITH_KNOTS ( 'NONE', 3,
 ( #36618, #40105, #50383, #55682 ),
 .UNSPECIFIED., .F., .F.,
 ( 4, 4 ),
 ( 1.951563910473907981E-18, 0.004446298630425045938 ),
 .UNSPECIFIED. ) ;
#32703 = CYLINDRICAL_SURFACE ( 'NONE', #45003, 10.00000000000000000 ) ;
#32704 = ORIENTED_EDGE ( 'NONE', *, *, #32868, .F. ) ;
#32705 = VERTEX_POINT ( 'NONE', #45084 ) ;
#32706 = CARTESIAN_POINT ( 'NONE',  ( 0.6039202388192952409, 41.06127625758627886, 26.93576256479796882 ) ) ;
#32707 = ORIENTED_EDGE ( 'NONE', *, *, #11110, .F. ) ;
#32708 = CARTESIAN_POINT ( 'NONE',  ( 0.5806925824938499181, -8.338382001838064994, 46.14860504863594315 ) ) ;
#32709 = CARTESIAN_POINT ( 'NONE',  ( 21.00000000000000355, 0.000000000000000000, 2.055000000000000160 ) ) ;
#32710 = LINE ( 'NONE', #51792, #12667 ) ;
#32711 = CARTESIAN_POINT ( 'NONE',  ( 0.5837800005270558090, -38.66299731356561864, 26.54068381509792474 ) ) ;
#32712 = FACE_OUTER_BOUND ( 'NONE', #50804, .T. ) ;
#32713 = ADVANCED_FACE ( 'NONE', ( #20941 ), #30637, .F. ) ;
#32714 = VERTEX_POINT ( 'NONE', #59443 ) ;
#32715 = CARTESIAN_POINT ( 'NONE',  ( 4.962356264823608143, -38.91448554252697534, 16.02805081171152324 ) ) ;
#32716 = CARTESIAN_POINT ( 'NONE',  ( 5.901764892641288895, -48.05798712428990882, 9.403262253136601245 ) ) ;
#32717 = CARTESIAN_POINT ( 'NONE',  ( 5.896278296736517710, -18.51903684540615913, -7.846798960905831066 ) ) ;
#32718 = EDGE_LOOP ( 'NONE', ( #45990, #25609, #52166, #27299 ) ) ;
#32719 = CARTESIAN_POINT ( 'NONE',  ( 0.8753041380234465318, -29.91468680897799359, -38.93905290314259560 ) ) ;
#32720 = CARTESIAN_POINT ( 'NONE',  ( 0.1368894036331277653, 30.13294619814276132, 32.23145791525983839 ) ) ;
#32721 = CARTESIAN_POINT ( 'NONE',  ( 4.956445790443996913, 8.365049606151725214, 46.34181691762049127 ) ) ;
#32722 = CARTESIAN_POINT ( 'NONE',  ( 0.6000166863083090663, -34.91285637184651591, -34.53861522509652815 ) ) ;
#32723 = ORIENTED_EDGE ( 'NONE', *, *, #33216, .F. ) ;
#32724 = VERTEX_POINT ( 'NONE', #16551 ) ;
#32725 = CARTESIAN_POINT ( 'NONE',  ( 5.960721111146673579, 18.96557324978276071, 7.848955554238579602 ) ) ;
#32726 = CARTESIAN_POINT ( 'NONE',  ( 4.963659409799332067, 36.94443854030220109, 25.25989740981512099 ) ) ;
#32727 = DIRECTION ( 'NONE',  ( 0.9848077530122079093, 0.1736481776669315802, -5.551115123125782086E-17 ) ) ;
#32728 = B_SPLINE_CURVE_WITH_KNOTS ( 'NONE', 3,
 ( #37833, #56269, #47207, #22771 ),
 .UNSPECIFIED., .F., .F.,
 ( 4, 4 ),
 ( 0.000000000000000000, 0.004041751736740986471 ),
 .UNSPECIFIED. ) ;
#32729 = CARTESIAN_POINT ( 'NONE',  ( 0.6027444965799114707, 32.91815440601231302, 36.44082362391626617 ) ) ;
#32730 = CARTESIAN_POINT ( 'NONE',  ( 4.553261556744875094, 0.000000000000000000, 0.000000000000000000 ) ) ;
#32731 = CARTESIAN_POINT ( 'NONE',  ( -6.010958268070873523, -4.891065400978513722, 18.19761767765828608 ) ) ;
#32732 = CARTESIAN_POINT ( 'NONE',  ( 0.6029443199889047422, -42.78819218835079852, 24.09788893465896464 ) ) ;
#32733 = CARTESIAN_POINT ( 'NONE',  ( 0.9754642270333693244, 42.90808635884410194, 0.1757168848620660473 ) ) ;
#32734 = CARTESIAN_POINT ( 'NONE',  ( 4.691466044806102964, -14.01607102724513076, -42.32811009116549883 ) ) ;
#32735 = CARTESIAN_POINT ( 'NONE',  ( 4.963659409799328515, -9.199077662859210136, 43.79875484948445319 ) ) ;
#32736 = AXIS2_PLACEMENT_3D ( 'NONE', #28829, #35097, #47951 ) ;
#32737 = CARTESIAN_POINT ( 'NONE',  ( 0.3676999524040366896, -22.15802448780013378, 38.14410221935873579 ) ) ;
#32738 = CARTESIAN_POINT ( 'NONE',  ( 0.5809828226811617480, -6.791453954330657794, 47.41188724015877654 ) ) ;
#32739 = ORIENTED_EDGE ( 'NONE', *, *, #42614, .F. ) ;
#32740 = MECHANICAL_DESIGN_GEOMETRIC_PRESENTATION_REPRESENTATION (  '', ( #43761 ), #39781 ) ;
#32741 = CIRCLE ( 'NONE', #56720, 47.91270532121795611 ) ;
#32742 = CARTESIAN_POINT ( 'NONE',  ( 0.6001305935487315502, 23.60027211631770427, 41.92422178329178450 ) ) ;
#32743 = CARTESIAN_POINT ( 'NONE',  ( 4.956653778116992370, 21.75875759808766929, -42.88673967249108188 ) ) ;
#32744 = CARTESIAN_POINT ( 'NONE',  ( 0.1154773475650540393, -35.46900651670787141, -26.24677516884419504 ) ) ;
#32745 = FACE_OUTER_BOUND ( 'NONE', #35164, .T. ) ;
#32746 = CARTESIAN_POINT ( 'NONE',  ( 3.221118495291109163, -24.39610253492621084, -36.60043170192283668 ) ) ;
#32747 = CARTESIAN_POINT ( 'NONE',  ( 4.962356264823608143, 0.000000000000000000, 0.000000000000000000 ) ) ;
#32748 = EDGE_CURVE ( 'NONE', #12007, #448, #12283, .T. ) ;
#32749 = DIRECTION ( 'NONE',  ( -1.000000000000000000, -0.000000000000000000, -0.000000000000000000 ) ) ;
#32750 = CARTESIAN_POINT ( 'NONE',  ( 5.917102823773431552, 16.57624106732469826, 11.38937882984319039 ) ) ;
#32751 = EDGE_CURVE ( 'NONE', #11571, #41967, #9255, .T. ) ;
#32752 = AXIS2_PLACEMENT_3D ( 'NONE', #14197, #55, #13266 ) ;
#32753 = CARTESIAN_POINT ( 'NONE',  ( 0.2224561200757612656, 6.380320192201981655, -42.64482917976813070 ) ) ;
#32755 = ORIENTED_EDGE ( 'NONE', *, *, #18052, .T. ) ;
#32754 = DIRECTION ( 'NONE',  ( 0.000000000000000000, 1.000000000000000000, -1.224646799147353207E-16 ) ) ;
#32757 = ORIENTED_EDGE ( 'NONE', *, *, #3438, .T. ) ;
#32756 = B_SPLINE_CURVE_WITH_KNOTS ( 'NONE', 3,
 ( #61268, #33111, #51878, #18387, #56264, #56578, #28387, #57178, #14311, #4870, #57479, #13693, #23387, #42513, #8976, #28085 ),
 .UNSPECIFIED., .F., .F.,
 ( 4, 3, 3, 3, 3, 4 ),
 ( 3.469446951953614189E-18, 0.0002732102107931881022, 0.0004098135523333745409, 0.0005464168938824928538, 0.0008195847345945353121, 0.001092771384553107650 ),
 .UNSPECIFIED. ) ;
#32758 = CARTESIAN_POINT ( 'NONE',  ( 1.088908134280556661, -42.90644581410504799, 0.7803765577540302534 ) ) ;
#32759 = CARTESIAN_POINT ( 'NONE',  ( -6.078726893082806448, 3.076629396955338436, -19.00863995194055178 ) ) ;
#32760 = CARTESIAN_POINT ( 'NONE',  ( 0.7057020205114954425, 17.55108080125446435, 44.57024707370717209 ) ) ;
#32761 = ORIENTED_EDGE ( 'NONE', *, *, #23573, .F. ) ;
#32762 = CARTESIAN_POINT ( 'NONE',  ( 0.6026777506516368677, 10.75755792781037812, -47.91472986532454570 ) ) ;
#32763 = CARTESIAN_POINT ( 'NONE',  ( 0.000000000000000000, 0.000000000000000000, 0.000000000000000000 ) ) ;
#32764 = CARTESIAN_POINT ( 'NONE',  ( 0.6028618097248863439, -44.51207924874665167, -18.24855319618731286 ) ) ;
#32765 = CONICAL_SURFACE ( 'NONE', #3698, 43.08621763946400307, 1.568696531533066763 ) ;
#32766 = EDGE_LOOP ( 'NONE', ( #61419, #20072, #51049, #56848 ) ) ;
#32767 = ORIENTED_EDGE ( 'NONE', *, *, #28790, .F. ) ;
#32768 = CARTESIAN_POINT ( 'NONE',  ( 0.9749527285493307938, 41.37154756071291928, 11.38116287125068204 ) ) ;
#32769 = ADVANCED_FACE ( 'NONE', ( #27179 ), #49482, .F. ) ;
#32770 = AXIS2_PLACEMENT_3D ( 'NONE', #52442, #32749, #18966 ) ;
#32771 = DIRECTION ( 'NONE',  ( -1.000000000000000000, -0.000000000000000000, -0.000000000000000000 ) ) ;
#32772 = CARTESIAN_POINT ( 'NONE',  ( 4.956445790443988031, 0.000000000000000000, 0.000000000000000000 ) ) ;
#32773 = CARTESIAN_POINT ( 'NONE',  ( 0.9772918015221172539, 32.63115054127247561, -26.29724073174774546 ) ) ;
#32774 = EDGE_CURVE ( 'NONE', #44156, #23013, #33252, .T. ) ;
#32775 = CARTESIAN_POINT ( 'NONE',  ( 0.5988103564986361205, -17.84821699813511486, 44.67429521517301794 ) ) ;
#32776 = CARTESIAN_POINT ( 'NONE',  ( 0.8560838555295158248, 42.82099363437792050, 19.15033519931955297 ) ) ;
#32777 = EDGE_CURVE ( 'NONE', #27088, #57237, #28675, .T. ) ;
#32778 = CARTESIAN_POINT ( 'NONE',  ( 0.1139756605157203340, 33.85464405449629055, 28.29873311013023951 ) ) ;
#32779 = CONICAL_SURFACE ( 'NONE', #5719, 2.060000000000000941, 0.9599310885968777018 ) ;
#32780 = EDGE_LOOP ( 'NONE', ( #60138, #21419, #46043, #21771 ) ) ;
#32781 = CARTESIAN_POINT ( 'NONE',  ( 4.967162193818130511, 13.42934394584164082, 40.93989340068615945 ) ) ;
#32782 = CARTESIAN_POINT ( 'NONE',  ( 4.967162193818130511, 0.000000000000000000, 0.000000000000000000 ) ) ;
#32783 = VECTOR ( 'NONE', #17075, 1000.000000000000227 ) ;
#32784 = ORIENTED_EDGE ( 'NONE', *, *, #21360, .F. ) ;
#32785 = AXIS2_PLACEMENT_3D ( 'NONE', #14085, #61344, #14388 ) ;
#32786 = CARTESIAN_POINT ( 'NONE',  ( 0.9790320750461911636, -37.36543188631139856, -18.97792487316815979 ) ) ;
#32787 = CARTESIAN_POINT ( 'NONE',  ( -6.078726893082806448, -17.34758611459996303, -8.357948149232475643 ) ) ;
#32788 = CARTESIAN_POINT ( 'NONE',  ( 0.5997462898726536595, -49.10477184366966696, -0.5225058138009923692 ) ) ;
#32789 = CARTESIAN_POINT ( 'NONE',  ( 0.9968887458511642707, 15.81144734640186833, 39.89008038581149407 ) ) ;
#32790 = EDGE_CURVE ( 'NONE', #46275, #61755, #39404, .T. ) ;
#32791 = VERTEX_POINT ( 'NONE', #36595 ) ;
#32792 = VERTEX_POINT ( 'NONE', #32196 ) ;
#32793 = CARTESIAN_POINT ( 'NONE',  ( 0.9762797500689124330, -31.41867615533404390, 27.73430319715907544 ) ) ;
#32794 = CARTESIAN_POINT ( 'NONE',  ( 0.8560838555295223751, 3.785103201470721768, -46.75516899590834186 ) ) ;
#32795 = CARTESIAN_POINT ( 'NONE',  ( -2.739355103387247858, 1.171460933655153136, 14.88204442379933390 ) ) ;
#32796 =( REPRESENTATION_RELATIONSHIP ('NONE','NONE', #44881, #19619 ) REPRESENTATION_RELATIONSHIP_WITH_TRANSFORMATION ( #30177 )SHAPE_REPRESENTATION_RELATIONSHIP( ) );
#32797 =( BOUNDED_SURFACE ( )  B_SPLINE_SURFACE ( 3, 1, ( 
 ( #57775, #14909 ),
 ( #20217, #16428 ),
 ( #54612, #21126 ),
 ( #11744, #40268 ) ),
 .UNSPECIFIED., .F., .F., .F. ) 
 B_SPLINE_SURFACE_WITH_KNOTS ( ( 4, 4 ),
 ( 2, 2 ),
 ( 0.000000000000000000, 1.000000000000000000 ),
 ( 0.000000000000000000, 1.000000000000000000 ),
 .UNSPECIFIED. ) 
 GEOMETRIC_REPRESENTATION_ITEM ( )  RATIONAL_B_SPLINE_SURFACE ( (
 ( 1.000000000000000000, 1.000000000000000000),
 ( 0.7282232189291694135, 0.9929344683865672927),
 ( 0.7282232189291694135, 0.9929344683865672927),
 ( 1.000000000000000000, 1.000000000000000000) ) ) 
 REPRESENTATION_ITEM ( '' )  SURFACE ( )  );
#32798 = EDGE_LOOP ( 'NONE', ( #1098, #15981, #42876, #36736 ) ) ;
#32799 = CARTESIAN_POINT ( 'NONE',  ( 0.6041374136657475802, -18.24862627831505435, -44.51224464244992163 ) ) ;
#32800 = ORIENTED_EDGE ( 'NONE', *, *, #25260, .F. ) ;
#32801 = CARTESIAN_POINT ( 'NONE',  ( 2.359973842542475886, 43.47549606496694707, 6.929439842984741915 ) ) ;
#32802 = CARTESIAN_POINT ( 'NONE',  ( 0.6021447746440204973, -25.23315518945873137, 42.12871963724009561 ) ) ;
#32803 = B_SPLINE_CURVE_WITH_KNOTS ( 'NONE', 3,
 ( #24161, #14783, #52973, #29171 ),
 .UNSPECIFIED., .F., .F.,
 ( 4, 4 ),
 ( 0.000000000000000000, 0.002320612883253031153 ),
 .UNSPECIFIED. ) ;
#32804 = CARTESIAN_POINT ( 'NONE',  ( 0.1156867017252034696, 37.04796616592829395, -23.96645593831968313 ) ) ;
#32805 = ORIENTED_EDGE ( 'NONE', *, *, #23975, .F. ) ;
#32806 = CARTESIAN_POINT ( 'NONE',  ( 0.5809828226811617480, -0.5448590168535863976, 47.89273459658653564 ) ) ;
#32807 = CARTESIAN_POINT ( 'NONE',  ( 0.6000166863083106206, 10.41802958826996495, -47.99258423138293495 ) ) ;
#32808 = CARTESIAN_POINT ( 'NONE',  ( 1.092182651088184464, -41.86503207152927786, -2.019968834440684979 ) ) ;
#32809 = CIRCLE ( 'NONE', #56782, 72.00000000000002842 ) ;
#32810 = VERTEX_POINT ( 'NONE', #8069 ) ;
#32811 = CARTESIAN_POINT ( 'NONE',  ( 0.6017666602106490625, -29.56224131406243671, -37.95277954208626170 ) ) ;
#32812 = CARTESIAN_POINT ( 'NONE',  ( 0.1152339509894530906, 33.45292367112824650, -28.77228854833953164 ) ) ;
#32813 = CARTESIAN_POINT ( 'NONE',  ( 1.227938101723748288, 26.79402671879374864, -33.52879263017835143 ) ) ;
#32814 = CARTESIAN_POINT ( 'NONE',  ( 0.6029303876144825880, 47.71279573267359098, -6.149480157546095782 ) ) ;
#32815 = CARTESIAN_POINT ( 'NONE',  ( 0.1365634738349432442, -38.75391421075912746, 21.09494614755793407 ) ) ;
#32816 = ORIENTED_EDGE ( 'NONE', *, *, #57839, .T. ) ;
#32817 = CARTESIAN_POINT ( 'NONE',  ( -6.010958268070873523, -9.434296419346091866, -16.31164801516952068 ) ) ;
#32818 = ADVANCED_FACE ( 'NONE', ( #8994 ), #28102, .T. ) ;
#32819 = FACE_BOUND ( 'NONE', #3085, .T. ) ;
#32820 = EDGE_LOOP ( 'NONE', ( #46806, #31713, #22165, #12894 ) ) ;
#32821 = EDGE_CURVE ( 'NONE', #29080, #4682, #32505, .T. ) ;
#32822 = LINE ( 'NONE', #28720, #42956 ) ;
#32823 = CARTESIAN_POINT ( 'NONE',  ( 0.9775691876210987896, -27.34475084661038835, 31.75843683380510996 ) ) ;
#32824 = CARTESIAN_POINT ( 'NONE',  ( 0.8551540677456739292, 5.348818140990903025, 47.61725548905992156 ) ) ;
#32825 = CARTESIAN_POINT ( 'NONE',  ( 0.5804410086790514622, 40.62771722849996081, -23.42879520283628025 ) ) ;
#32826 = B_SPLINE_CURVE_WITH_KNOTS ( 'NONE', 3,
 ( #33430, #5797, #10226, #38754, #48431, #23707 ),
 .UNSPECIFIED., .F., .F.,
 ( 4, 2, 4 ),
 ( 1.910689091754275557E-17, 0.0002293755540694318064, 0.0004587511081388444766 ),
 .UNSPECIFIED. ) ;
#32827 = FACE_OUTER_BOUND ( 'NONE', #42252, .T. ) ;
#32828 = FACE_OUTER_BOUND ( 'NONE', #4293, .T. ) ;
#32829 = CARTESIAN_POINT ( 'NONE',  ( 4.549368137175248350, -24.02461520945246320, -35.57418903283107880 ) ) ;
#32830 = ADVANCED_FACE ( 'NONE', ( #8673 ), #17855, .F. ) ;
#32831 = DIRECTION ( 'NONE',  ( 1.149946807736160365E-16, -0.3937045127299804714, 0.9192370513942791366 ) ) ;
#32832 = FACE_OUTER_BOUND ( 'NONE', #29536, .T. ) ;
#32833 = CARTESIAN_POINT ( 'NONE',  ( -6.078726893082806448, 12.00859800336359129, -15.05282748397562820 ) ) ;
#32834 = CARTESIAN_POINT ( 'NONE',  ( 4.553261556744875094, 0.000000000000000000, 0.000000000000000000 ) ) ;
#32835 = EDGE_CURVE ( 'NONE', #51034, #5328, #17484, .T. ) ;
#32836 = EDGE_CURVE ( 'NONE', #9438, #31616, #251, .T. ) ;
#32837 = CARTESIAN_POINT ( 'NONE',  ( 0.5837800005270555870, 32.60177022003745861, 33.70993677184314663 ) ) ;
#32838 = CARTESIAN_POINT ( 'NONE',  ( 4.975610109902397937, 45.55079628452135410, -17.82061629079668919 ) ) ;
#32839 = ORIENTED_EDGE ( 'NONE', *, *, #37410, .F. ) ;
#32840 = VECTOR ( 'NONE', #24981, 1000.000000000000114 ) ;
#32841 = DIRECTION ( 'NONE',  ( -1.000000000000000000, -5.380183451256491399E-17, -1.298891185607892835E-16 ) ) ;
#32842 = LINE ( 'NONE', #24037, #24794 ) ;
#32843 = CARTESIAN_POINT ( 'NONE',  ( -3.673643420401911275, -2.497823135841289677, -0.2484800633750114396 ) ) ;
#32844 = CARTESIAN_POINT ( 'NONE',  ( 0.8751705887134423323, -11.58504748649167837, -46.67919521768883584 ) ) ;
#32845 = FACE_OUTER_BOUND ( 'NONE', #18790, .T. ) ;
#32846 = ORIENTED_EDGE ( 'NONE', *, *, #56242, .F. ) ;
#32847 = FACE_OUTER_BOUND ( 'NONE', #38076, .T. ) ;
#32848 = ADVANCED_FACE ( 'NONE', ( #29329 ), #9325, .F. ) ;
#32850 = VECTOR ( 'NONE', #15541, 1000.000000000000114 ) ;
#32849 = CARTESIAN_POINT ( 'NONE',  ( 4.553261556744873317, 42.54662847375970358, 10.92355122382355148 ) ) ;
#32851 = CARTESIAN_POINT ( 'NONE',  ( -20.05974703543239457, -7.996306382744656993, -0.2778595553339769930 ) ) ;
#32852 = EDGE_CURVE ( 'NONE', #22147, #20219, #5197, .T. ) ;
#32853 = ORIENTED_EDGE ( 'NONE', *, *, #22963, .T. ) ;
#32854 = CARTESIAN_POINT ( 'NONE',  ( 1.227938101723756947, -11.92353943227920610, -41.23019537246722876 ) ) ;
#32855 = ADVANCED_FACE ( 'NONE', ( #5503 ), #43482, .F. ) ;
#32856 = ORIENTED_EDGE ( 'NONE', *, *, #61189, .T. ) ;
#32857 = PRESENTATION_LAYER_ASSIGNMENT (  '', '', ( #59841 ) ) ;
#32858 = CARTESIAN_POINT ( 'NONE',  ( 0.8751705887134553219, 7.160166390003662507, 47.55935879196473337 ) ) ;
#32859 = AXIS2_PLACEMENT_3D ( 'NONE', #38752, #20250, #5186 ) ;
#32860 = VERTEX_POINT ( 'NONE', #48747 ) ;
#32861 = CARTESIAN_POINT ( 'NONE',  ( 0.6041374136657476912, -44.37863742124680044, 18.57118264377460903 ) ) ;
#32862 = CARTESIAN_POINT ( 'NONE',  ( 4.956653778116988818, -45.35992544608517818, -15.97476558431931082 ) ) ;
#32863 = ORIENTED_EDGE ( 'NONE', *, *, #13734, .T. ) ;
#32864 = CARTESIAN_POINT ( 'NONE',  ( 0.8557997880470697982, -41.93815086860240626, -23.15977007032367041 ) ) ;
#32865 = DIRECTION ( 'NONE',  ( 0.000000000000000000, 0.000000000000000000, 1.000000000000000000 ) ) ;
#32866 = DIRECTION ( 'NONE',  ( 0.000000000000000000, 0.000000000000000000, 1.000000000000000000 ) ) ;
#32867 = CARTESIAN_POINT ( 'NONE',  ( 0.3622758884714600280, 22.26738722580168073, -36.91764744403298693 ) ) ;
#32868 = EDGE_CURVE ( 'NONE', #14241, #58875, #51857, .T. ) ;
#32869 = ORIENTED_EDGE ( 'NONE', *, *, #17688, .T. ) ;
#32870 = CARTESIAN_POINT ( 'NONE',  ( 0.9783242366443547500, -6.706126116610328758, -41.36861567317236421 ) ) ;
#32871 = VERTEX_POINT ( 'NONE', #19037 ) ;
#32872 = LINE ( 'NONE', #51948, #2155 ) ;
#32873 =( BOUNDED_SURFACE ( )  B_SPLINE_SURFACE ( 3, 1, ( 
 ( #19720, #38847 ),
 ( #57901, #15028 ),
 ( #34138, #29410 ),
 ( #34441, #48519 ) ),
 .UNSPECIFIED., .F., .F., .F. ) 
 B_SPLINE_SURFACE_WITH_KNOTS ( ( 4, 4 ),
 ( 2, 2 ),
 ( 0.000000000000000000, 1.000000000000000000 ),
 ( 0.000000000000000000, 1.000000000000000000 ),
 .UNSPECIFIED. ) 
 GEOMETRIC_REPRESENTATION_ITEM ( )  RATIONAL_B_SPLINE_SURFACE ( (
 ( 1.000000000000000000, 1.000000000000000000),
 ( 0.9953040768229013402, 0.8617119497784988535),
 ( 0.9953040768229013402, 0.8617119497784988535),
 ( 1.000000000000000000, 1.000000000000000000) ) ) 
 REPRESENTATION_ITEM ( '' )  SURFACE ( )  );
#32874 = ADVANCED_FACE ( 'NONE', ( #9297 ), #55882, .F. ) ;
#32875 = ORIENTED_EDGE ( 'NONE', *, *, #50279, .T. ) ;
#32876 = ORIENTED_EDGE ( 'NONE', *, *, #43963, .F. ) ;
#32877 = CARTESIAN_POINT ( 'NONE',  ( 0.9730545539215883499, -42.47233286818612896, -6.101350888305089093 ) ) ;
#32878 = CARTESIAN_POINT ( 'NONE',  ( 0.6009453534118439633, -34.32439302680990778, 33.70725662590598404 ) ) ;
#32879 = VECTOR ( 'NONE', #56560, 1000.000000000000114 ) ;
#32880 = CIRCLE ( 'NONE', #20831, 42.92674063221959813 ) ;
#32881 = CARTESIAN_POINT ( 'NONE',  ( 0.8557997880470697982, 46.50333260518559086, 11.51622788066474534 ) ) ;
#32882 = CARTESIAN_POINT ( 'NONE',  ( 0.5549461598389366923, -28.17959065316841816, -33.92828268696586491 ) ) ;
#32883 = ORIENTED_EDGE ( 'NONE', *, *, #22639, .F. ) ;
#32884 = CARTESIAN_POINT ( 'NONE',  ( 0.9749527285493296835, 0.2856147164664618043, -42.90750796893249941 ) ) ;
#32885 = CARTESIAN_POINT ( 'NONE',  ( 0.5804410086790514622, 45.08525424748445687, -12.91664435118818410 ) ) ;
#32886 = CARTESIAN_POINT ( 'NONE',  ( 3.559346040607745287, 0.6451424477637347499, 43.96605591549100467 ) ) ;
#32887 = EDGE_LOOP ( 'NONE', ( #3039, #49319, #50355, #53490 ) ) ;
#32888 = B_SPLINE_CURVE_WITH_KNOTS ( 'NONE', 3,
 ( #44564, #1290, #6589, #39872, #20423, #30118, #39552, #58928, #58606, #15736, #53911, #11034, #12587, #47024, #7860, #51376, #12279, #12896, #7535 ),
 .UNSPECIFIED., .F., .F.,
 ( 4, 3, 3, 3, 3, 3, 4 ),
 ( 8.674676106452504675E-19, 0.0002612768053151718175, 0.0003919133833142909255, 0.0005225499612322609703, 0.0006531865391693360669, 0.0008112755173415194237, 0.0009693688056799724647 ),
 .UNSPECIFIED. ) ;
#32889 = ORIENTED_EDGE ( 'NONE', *, *, #12606, .F. ) ;
#32890 = CARTESIAN_POINT ( 'NONE',  ( 0.1073791018717578927, -21.14095454447534550, -37.58707531572198235 ) ) ;
#32891 = CARTESIAN_POINT ( 'NONE',  ( 4.975801465491695552, 15.94009207552985252, 45.18341283946464415 ) ) ;
#32892 = LINE ( 'NONE', #8428, #51953 ) ;
#32893 = DIRECTION ( 'NONE',  ( 0.07836865515943412797, 0.4916162952473433490, 0.8672783706145211768 ) ) ;
#32894 = ORIENTED_EDGE ( 'NONE', *, *, #42468, .T. ) ;
#32895 = EDGE_CURVE ( 'NONE', #7638, #38559, #43690, .T. ) ;
#32896 = DIRECTION ( 'NONE',  ( 1.000000000000000000, 0.000000000000000000, 0.000000000000000000 ) ) ;
#32897 = CARTESIAN_POINT ( 'NONE',  ( 48.88223999046894619, 15.35656115023722812, 2.106076572069662589 ) ) ;
#32898 = CARTESIAN_POINT ( 'NONE',  ( 0.9762797500689124330, 10.20671408566037286, -40.64662068068250278 ) ) ;
#32899 = CARTESIAN_POINT ( 'NONE',  ( 4.956653778116968390, 48.02038484091101367, -2.599733001514498376 ) ) ;
#32900 = EDGE_CURVE ( 'NONE', #46035, #49237, #33748, .T. ) ;
#32901 = SHAPE_REPRESENTATION_RELATIONSHIP ( 'NONE' , 'NONE' ,  #2385, #48247 ) ;
#32902 = CARTESIAN_POINT ( 'NONE',  ( 4.960156602257181468, 34.56254177294268004, 30.99165383632775672 ) ) ;
#32903 = ORIENTED_EDGE ( 'NONE', *, *, #25759, .F. ) ;
#32904 = EDGE_CURVE ( 'NONE', #60819, #30020, #186, .T. ) ;
#32905 = CARTESIAN_POINT ( 'NONE',  ( 5.960721111146673579, -20.35079619394244332, -2.672857320903232470 ) ) ;
#32906 = EDGE_CURVE ( 'NONE', #22420, #17505, #503, .T. ) ;
#32907 = CARTESIAN_POINT ( 'NONE',  ( 4.553261556744875094, -4.442710778082547662, 43.70128015019636791 ) ) ;
#32908 = CONICAL_SURFACE ( 'NONE', #59755, 42.92674063221959813, 1.485477209440487556 ) ;
#32909 = EDGE_CURVE ( 'NONE', #23299, #60472, #39918, .T. ) ;
#32910 = CARTESIAN_POINT ( 'NONE',  ( 0.9788927965476033055, 29.23628500401661157, 30.02625937068571815 ) ) ;
#32911 = CARTESIAN_POINT ( 'NONE',  ( 0.5819845901640506858, -12.83441129068565445, 46.14435291605025924 ) ) ;
#32912 = CARTESIAN_POINT ( 'NONE',  ( 0.8551540677456715978, -46.03951182599418246, -13.28067116677250503 ) ) ;
#32913 = CARTESIAN_POINT ( 'NONE',  ( 3.678748215320120085, -48.77537477639203445, -4.424435525802461910 ) ) ;
#32914 = EDGE_CURVE ( 'NONE', #3462, #40188, #34688, .T. ) ;
#32915 = CARTESIAN_POINT ( 'NONE',  ( 4.335381028904201628, 31.32980982056168884, 37.65899446708290554 ) ) ;
#32916 = CIRCLE ( 'NONE', #44915, 4.000000000000000888 ) ;
#32917 = ORIENTED_EDGE ( 'NONE', *, *, #10696, .T. ) ;
#32918 = VECTOR ( 'NONE', #32096, 1000.000000000000114 ) ;
#32919 = CARTESIAN_POINT ( 'NONE',  ( 0.8753041380234471980, -49.09527960836077654, -0.8898584437169385630 ) ) ;
#32920 = CARTESIAN_POINT ( 'NONE',  ( 0.2279481005628799517, 44.07067687752851981, -2.068556653656985045 ) ) ;
#32921 = CARTESIAN_POINT ( 'NONE',  ( -2.739355103387248747, -12.11899594566302518, -8.716507570123491533 ) ) ;
#32922 = PLANE ( 'NONE',  #10702 ) ;
#32923 = ORIENTED_EDGE ( 'NONE', *, *, #8397, .F. ) ;
#32924 = CARTESIAN_POINT ( 'NONE',  ( 0.5782707292762423457, -45.81184706829309761, 10.05042396612924982 ) ) ;
#32925 = FACE_OUTER_BOUND ( 'NONE', #27384, .T. ) ;
#32926 = ORIENTED_EDGE ( 'NONE', *, *, #16407, .F. ) ;
#32927 = CARTESIAN_POINT ( 'NONE',  ( 0.1158403557922069033, 4.274622882211749797, -43.91660171733112605 ) ) ;
#32928 = CARTESIAN_POINT ( 'NONE',  ( 4.956653778116990594, 2.599733001515011743, -48.02038484091096393 ) ) ;
#32929 = CARTESIAN_POINT ( 'NONE',  ( -6.015611763856276717, 2.465697960551047618, 18.68122482568280773 ) ) ;
#32930 = VERTEX_POINT ( 'NONE', #34061 ) ;
#32931 = CARTESIAN_POINT ( 'NONE',  ( 2.282816707992322058, 31.69834551989417193, -34.66571588341096088 ) ) ;
#32932 = AXIS2_PLACEMENT_3D ( 'NONE', #40755, #39831, #2493 ) ;
#32933 = EDGE_LOOP ( 'NONE', ( #19668, #14378, #57802, #46660 ) ) ;
#32934 = ORIENTED_EDGE ( 'NONE', *, *, #6009, .T. ) ;
#32935 = CARTESIAN_POINT ( 'NONE',  ( 0.5804410086790514622, -19.24447200597980512, 42.76879877979338573 ) ) ;
#32936 = CARTESIAN_POINT ( 'NONE',  ( 0.1313383488274144917, 40.08066228784242924, 15.91164383651759806 ) ) ;
#32937 = ORIENTED_EDGE ( 'NONE', *, *, #28577, .F. ) ;
#32938 = CARTESIAN_POINT ( 'NONE',  ( 2.618530812446115519, 31.65223561859582802, -34.75432015653727547 ) ) ;
#32939 = ORIENTED_EDGE ( 'NONE', *, *, #15238, .T. ) ;
#32940 = CARTESIAN_POINT ( 'NONE',  ( 0.7764146366350234141, 11.73874228733617642, 45.41191917526355581 ) ) ;
#32941 = ORIENTED_EDGE ( 'NONE', *, *, #8706, .T. ) ;
#32942 = ADVANCED_FACE ( 'NONE', ( #30868 ), #37440, .F. ) ;
#32943 = CARTESIAN_POINT ( 'NONE',  ( 0.5988103622719989083, 48.10388392585941375, 0.6065097949915312370 ) ) ;
#32944 = CARTESIAN_POINT ( 'NONE',  ( 0.8554163680231738898, 16.00619315955181321, 44.10223637924652706 ) ) ;
#32945 =( BOUNDED_SURFACE ( )  B_SPLINE_SURFACE ( 3, 1, ( 
 ( #45312, #60288 ),
 ( #21795, #21476 ),
 ( #7355, #17401 ),
 ( #55590, #11473 ) ),
 .UNSPECIFIED., .F., .F., .F. ) 
 B_SPLINE_SURFACE_WITH_KNOTS ( ( 4, 4 ),
 ( 2, 2 ),
 ( 0.000000000000000000, 1.000000000000000000 ),
 ( 0.000000000000000000, 1.000000000000000000 ),
 .UNSPECIFIED. ) 
 GEOMETRIC_REPRESENTATION_ITEM ( )  RATIONAL_B_SPLINE_SURFACE ( (
 ( 1.000000000000000000, 1.000000000000000000),
 ( 0.7282232189291694135, 0.9929344683865672927),
 ( 0.7282232189291694135, 0.9929344683865672927),
 ( 1.000000000000000000, 1.000000000000000000) ) ) 
 REPRESENTATION_ITEM ( '' )  SURFACE ( )  );
#32946 = ORIENTED_EDGE ( 'NONE', *, *, #55214, .T. ) ;
#32947 = B_SPLINE_CURVE_WITH_KNOTS ( 'NONE', 3,
 ( #44696, #10866, #24647, #43786 ),
 .UNSPECIFIED., .F., .F.,
 ( 4, 4 ),
 ( 0.000000000000000000, 0.004446298630425077163 ),
 .UNSPECIFIED. ) ;
#32948 = CARTESIAN_POINT ( 'NONE',  ( 5.896782393890504181, -19.93422257774822626, -2.674482585249919442 ) ) ;
#32949 = CARTESIAN_POINT ( 'NONE',  ( 0.6000166863083106206, 37.05402083933937973, 32.23077754796269545 ) ) ;
#32950 = CARTESIAN_POINT ( 'NONE',  ( 0.5804410086790514622, -41.60900809504539666, 21.63816760268400330 ) ) ;
#32951 = CARTESIAN_POINT ( 'NONE',  ( 0.1154773475650540671, -23.02726780139724383, -37.63892357186712445 ) ) ;
#32952 = ORIENTED_EDGE ( 'NONE', *, *, #28353, .T. ) ;
#32953 = CARTESIAN_POINT ( 'NONE',  ( 0.5832367798473377940, -33.67436043247238331, -34.05962365606854547 ) ) ;
#32954 = CARTESIAN_POINT ( 'NONE',  ( 5.958863334805807099, 12.49619391867160445, 16.28335246510371448 ) ) ;
#32955 = ORIENTED_EDGE ( 'NONE', *, *, #58254, .T. ) ;
#32956 = CARTESIAN_POINT ( 'NONE',  ( 0.5830081025819947582, 43.06738386279880615, -18.55889225133284270 ) ) ;
#32957 = ORIENTED_EDGE ( 'NONE', *, *, #11931, .F. ) ;
#32958 = AXIS2_PLACEMENT_3D ( 'NONE', #35392, #924, #25660 ) ;
#32959 = DIRECTION ( 'NONE',  ( 0.000000000000000000, -1.047444401652941269E-14, 1.000000000000000000 ) ) ;
#32960 = CARTESIAN_POINT ( 'NONE',  ( 0.6029443199889047422, 46.60566125691656225, -15.47417140463258356 ) ) ;
#32961 = ORIENTED_EDGE ( 'NONE', *, *, #13623, .T. ) ;
#32962 = CARTESIAN_POINT ( 'NONE',  ( 0.9790850452238870627, -34.57988883937719748, -23.67633033473545012 ) ) ;
#32963 = CARTESIAN_POINT ( 'NONE',  ( 4.956445790444002242, -43.14021684453514638, 18.88014143872134554 ) ) ;
#32964 = CARTESIAN_POINT ( 'NONE',  ( 4.294001357053613965, 0.6022292657941538119, -42.05358333227729162 ) ) ;
#32965 = CARTESIAN_POINT ( 'NONE',  ( 1.227938101723747621, -20.72293514920724533, -37.58536632582800507 ) ) ;
#32966 =( BOUNDED_SURFACE ( )  B_SPLINE_SURFACE ( 3, 1, ( 
 ( #49715, #41269 ),
 ( #21835, #59724 ),
 ( #35330, #2079 ),
 ( #31535, #45972 ) ),
 .UNSPECIFIED., .F., .F., .F. ) 
 B_SPLINE_SURFACE_WITH_KNOTS ( ( 4, 4 ),
 ( 2, 2 ),
 ( 0.000000000000000000, 1.000000000000000000 ),
 ( 0.000000000000000000, 1.000000000000000000 ),
 .UNSPECIFIED. ) 
 GEOMETRIC_REPRESENTATION_ITEM ( )  RATIONAL_B_SPLINE_SURFACE ( (
 ( 1.000000000000000000, 1.000000000000000000),
 ( 0.7223157951917476005, 0.9931996967497186413),
 ( 0.7223157951917476005, 0.9931996967497186413),
 ( 1.000000000000000000, 1.000000000000000000) ) ) 
 REPRESENTATION_ITEM ( '' )  SURFACE ( )  );
#32967 = VECTOR ( 'NONE', #3805, 1000.000000000000114 ) ;
#32968 = ORIENTED_EDGE ( 'NONE', *, *, #31347, .F. ) ;
#32969 = CARTESIAN_POINT ( 'NONE',  ( 1.827326673878743257, -40.22837085190322881, 15.32882202537205707 ) ) ;
#32970 = CARTESIAN_POINT ( 'NONE',  ( 0.5786265663353153954, 38.43785771743204549, 28.58414684753499557 ) ) ;
#32971 =( BOUNDED_SURFACE ( )  B_SPLINE_SURFACE ( 3, 1, ( 
 ( #18846, #61403 ),
 ( #58175, #9417 ),
 ( #20007, #15300 ),
 ( #24685, #29377 ) ),
 .UNSPECIFIED., .F., .F., .F. ) 
 B_SPLINE_SURFACE_WITH_KNOTS ( ( 4, 4 ),
 ( 2, 2 ),
 ( 0.000000000000000000, 1.000000000000000000 ),
 ( 0.000000000000000000, 1.000000000000000000 ),
 .UNSPECIFIED. ) 
 GEOMETRIC_REPRESENTATION_ITEM ( )  RATIONAL_B_SPLINE_SURFACE ( (
 ( 1.000000000000000000, 1.000000000000000000),
 ( 0.7269869731126821222, 0.9931720237060910339),
 ( 0.7269869731126821222, 0.9931720237060910339),
 ( 1.000000000000000000, 1.000000000000000000) ) ) 
 REPRESENTATION_ITEM ( '' )  SURFACE ( )  );
#32972 = CARTESIAN_POINT ( 'NONE',  ( 5.895596859100789899, -15.78235929336518950, -12.46777118604672197 ) ) ;
#32973 = EDGE_CURVE ( 'NONE', #43495, #52417, #16172, .T. ) ;
#32974 = CARTESIAN_POINT ( 'NONE',  ( -6.000000000000001776, 4.730042041638951881E-15, 0.000000000000000000 ) ) ;
#32975 = CARTESIAN_POINT ( 'NONE',  ( 3.407937589446178528, -6.447869442558249453, 12.08659953757606864 ) ) ;
#32976 = CARTESIAN_POINT ( 'NONE',  ( 0.5832366564991501301, -46.19265750221180156, 12.65934068133968360 ) ) ;
#32977 = ADVANCED_FACE ( 'NONE', ( #25865 ), #21405, .F. ) ;
#32978 = LINE ( 'NONE', #48292, #12866 ) ;
#32979 = ADVANCED_FACE ( 'NONE', ( #11165 ), #34437, .T. ) ;
#32980 = EDGE_CURVE ( 'NONE', #29362, #8504, #26454, .T. ) ;
#32981 = FACE_OUTER_BOUND ( 'NONE', #60796, .T. ) ;
#32982 = CARTESIAN_POINT ( 'NONE',  ( 4.975801465491695552, -36.39623109580445259, -31.15993731089111662 ) ) ;
#32983 = CARTESIAN_POINT ( 'NONE',  ( 0.9756008150404602564, 30.24019526051588258, -30.44122083654187705 ) ) ;
#32984 = CARTESIAN_POINT ( 'NONE',  ( 0.1104177457020373149, -21.55798761925413842, 37.34931850022132238 ) ) ;
#32985 = CARTESIAN_POINT ( 'NONE',  ( 4.553261556744875094, 31.71129487083167220, -30.39627186743139831 ) ) ;
#32986 = CARTESIAN_POINT ( 'NONE',  ( 5.958863334805807099, -7.853699934219767975, -18.96369761673816967 ) ) ;
#32987 = CARTESIAN_POINT ( 'NONE',  ( 4.975801465491695552, 0.000000000000000000, 0.000000000000000000 ) ) ;
#32988 = CARTESIAN_POINT ( 'NONE',  ( 0.8760168074886965917, -41.20610493656892714, -24.81951362746064049 ) ) ;
#32989 = PRESENTATION_STYLE_ASSIGNMENT (( #57062 ) ) ;
#32990 = LINE ( 'NONE', #14192, #56188 ) ;
#32992 = ORIENTED_EDGE ( 'NONE', *, *, #9231, .F. ) ;
#32991 = CARTESIAN_POINT ( 'NONE',  ( 0.9740398440564321803, 39.79907313245131917, 16.03656236596764373 ) ) ;
#32993 = EDGE_CURVE ( 'NONE', #61588, #28220, #49640, .T. ) ;
#32994 = CARTESIAN_POINT ( 'NONE',  ( 4.956653778116966613, 0.000000000000000000, 0.000000000000000000 ) ) ;
#32995 = CARTESIAN_POINT ( 'NONE',  ( -6.010958268070873523, 18.20513189769815554, -4.863021950010456784 ) ) ;
#32996 = CARTESIAN_POINT ( 'NONE',  ( 4.291220156522059348, 2.567299637374572008, 47.04038658299518261 ) ) ;
#32997 = ORIENTED_EDGE ( 'NONE', *, *, #38549, .F. ) ;
#32998 = EDGE_CURVE ( 'NONE', #5623, #21984, #34984, .T. ) ;
#32999 = CARTESIAN_POINT ( 'NONE',  ( 0.5834872094924158370, -34.02770606800785202, 33.70665904794278589 ) ) ;
#33000 = B_SPLINE_CURVE_WITH_KNOTS ( 'NONE', 3,
 ( #59002, #35224, #34921, #10484 ),
 .UNSPECIFIED., .F., .F.,
 ( 4, 4 ),
 ( 5.204170427930421283E-17, 0.005004948556313862547 ),
 .UNSPECIFIED. ) ;
#33001 = UNCERTAINTY_MEASURE_WITH_UNIT (LENGTH_MEASURE( 1.000000000000000082E-05 ), #8438, 'distance_accuracy_value', 'NONE');
#33002 = ORIENTED_EDGE ( 'NONE', *, *, #13147, .T. ) ;
#33003 = VERTEX_POINT ( 'NONE', #35600 ) ;
#33004 = CARTESIAN_POINT ( 'NONE',  ( 0.000000000000000000, 0.000000000000000000, -5.600000000000000533 ) ) ;
#33005 = ORIENTED_EDGE ( 'NONE', *, *, #14169, .F. ) ;
#33006 = CONICAL_SURFACE ( 'NONE', #47982, 43.92652462719577500, 1.486293639869522343 ) ;
#33007 = CARTESIAN_POINT ( 'NONE',  ( 5.959547316686252039, 7.858107265727477753, 18.96183906913546480 ) ) ;
#33008 = CARTESIAN_POINT ( 'NONE',  ( -2.739355103387248747, 8.754959582419377995, 12.09124681996112649 ) ) ;
#33009 = VERTEX_POINT ( 'NONE', #7042 ) ;
#33010 = ORIENTED_EDGE ( 'NONE', *, *, #9858, .F. ) ;
#33011 = FACE_OUTER_BOUND ( 'NONE', #35936, .T. ) ;
#33012 = VERTEX_POINT ( 'NONE', #26172 ) ;
#33013 = CARTESIAN_POINT ( 'NONE',  ( 0.9730545539215883499, 11.59290486963565137, -41.31259007387218674 ) ) ;
#33014 = FACE_OUTER_BOUND ( 'NONE', #51200, .T. ) ;
#33015 = DIRECTION ( 'NONE',  ( 0.000000000000000000, 0.000000000000000000, -1.000000000000000000 ) ) ;
#33016 = ORIENTED_EDGE ( 'NONE', *, *, #12127, .F. ) ;
#33017 = CARTESIAN_POINT ( 'NONE',  ( 4.303969348037258058, 25.89994482339369952, 40.54345935592787953 ) ) ;
#33018 = B_SPLINE_CURVE_WITH_KNOTS ( 'NONE', 3,
 ( #25878, #3902, #8294, #32753, #22413, #12727 ),
 .UNSPECIFIED., .F., .F.,
 ( 4, 2, 4 ),
 ( 1.736958732247374613E-17, 0.0002293319059085092493, 0.0004586638118170010972 ),
 .UNSPECIFIED. ) ;
#33019 = ADVANCED_FACE ( 'NONE', ( #6413 ), #13838, .F. ) ;
#33020 = CARTESIAN_POINT ( 'NONE',  ( 0.9762797500689124330, -39.42083772998332591, 14.22400568939802845 ) ) ;
#33021 = ORIENTED_EDGE ( 'NONE', *, *, #28147, .F. ) ;
#33022 = VERTEX_POINT ( 'NONE', #5805 ) ;
#33023 = CARTESIAN_POINT ( 'NONE',  ( 0.7048096507298579061, -29.95256433478753877, 37.64898672361901077 ) ) ;
#33024 = VECTOR ( 'NONE', #22402, 1000.000000000000114 ) ;
#33025 = ORIENTED_EDGE ( 'NONE', *, *, #25500, .T. ) ;
#33026 = CARTESIAN_POINT ( 'NONE',  ( 0.2885700199627507789, 41.43179222486418922, -11.93479339212623636 ) ) ;
#33027 = CARTESIAN_POINT ( 'NONE',  ( 0.7764139734771250412, -14.74570975091260117, 44.52644736388372593 ) ) ;
#33028 = CARTESIAN_POINT ( 'NONE',  ( 0.9736507210033062965, -0.4504567742783994189, 42.90603603725247694 ) ) ;
#33029 = CARTESIAN_POINT ( 'NONE',  ( 0.1104177457020373149, 5.633723015004302503, 42.75487793940126124 ) ) ;
#33030 = CARTESIAN_POINT ( 'NONE',  ( 0.5848930533535030563, -38.76613696830671074, -26.39052305169494872 ) ) ;
#33031 = ORIENTED_EDGE ( 'NONE', *, *, #44663, .T. ) ;
#33032 = DIRECTION ( 'NONE',  ( 0.000000000000000000, 0.000000000000000000, 1.000000000000000000 ) ) ;
#33033 = CARTESIAN_POINT ( 'NONE',  ( 2.528100132419514257, -16.56545499686994916, 38.57252233622727999 ) ) ;
#33034 = CARTESIAN_POINT ( 'NONE',  ( 5.838029081930955932, -45.55059156558374411, -12.49834653777416626 ) ) ;
#33035 = VERTEX_POINT ( 'NONE', #49362 ) ;
#33036 = CARTESIAN_POINT ( 'NONE',  ( 4.956653778116980824, -40.28700667097698584, 26.26162724282358951 ) ) ;
#33037 = CARTESIAN_POINT ( 'NONE',  ( 0.9754402186311945666, 30.47320128434260766, 30.20795797590407972 ) ) ;
#33038 = CARTESIAN_POINT ( 'NONE',  ( 0.5997462898726536595, -25.00873172704203640, -42.26245340191634625 ) ) ;
#33039 = ORIENTED_EDGE ( 'NONE', *, *, #15646, .T. ) ;
#33040 = B_SPLINE_CURVE_WITH_KNOTS ( 'NONE', 3,
 ( #9819, #5700, #14537, #34254 ),
 .UNSPECIFIED., .F., .F.,
 ( 4, 4 ),
 ( 0.000000000000000000, 0.004444103432399266161 ),
 .UNSPECIFIED. ) ;
#33041 = ORIENTED_EDGE ( 'NONE', *, *, #23680, .F. ) ;
#33042 = CARTESIAN_POINT ( 'NONE',  ( 0.8744876279028306332, -47.25615711918273121, 13.31186180466906954 ) ) ;
#33043 = CARTESIAN_POINT ( 'NONE',  ( -6.016761891674565099, 14.95139917749719949, -11.46828378093544210 ) ) ;
#33044 = CARTESIAN_POINT ( 'NONE',  ( 0.9722240750034545353, -16.95645446544459034, -39.41582016107722097 ) ) ;
#33045 = CARTESIAN_POINT ( 'NONE',  ( 4.335381028904201628, -43.68634339260519539, 22.16439145674265276 ) ) ;
#33046 = CARTESIAN_POINT ( 'NONE',  ( -4.938558936750251149, -0.8708011863679817610, 8.896908036367455278E-17 ) ) ;
#33047 = CARTESIAN_POINT ( 'NONE',  ( 1.830465331921977246, -38.97216206803106076, 20.53160099995884380 ) ) ;
#33048 =( BOUNDED_SURFACE ( )  B_SPLINE_SURFACE ( 3, 1, ( 
 ( #4184, #28324 ),
 ( #18329, #18949 ),
 ( #23627, #38070 ),
 ( #4800, #33357 ) ),
 .UNSPECIFIED., .F., .F., .F. ) 
 B_SPLINE_SURFACE_WITH_KNOTS ( ( 4, 4 ),
 ( 2, 2 ),
 ( 0.000000000000000000, 1.000000000000000000 ),
 ( 0.000000000000000000, 1.000000000000000000 ),
 .UNSPECIFIED. ) 
 GEOMETRIC_REPRESENTATION_ITEM ( )  RATIONAL_B_SPLINE_SURFACE ( (
 ( 1.000000000000000000, 1.000000000000000000),
 ( 0.7269869731126817891, 0.9931720237060910339),
 ( 0.7269869731126817891, 0.9931720237060910339),
 ( 1.000000000000000000, 1.000000000000000000) ) ) 
 REPRESENTATION_ITEM ( '' )  SURFACE ( )  );
#33049 = CARTESIAN_POINT ( 'NONE',  ( -6.063463321072276813, -14.65282214633766422, 12.49460906260241444 ) ) ;
#33050 = CARTESIAN_POINT ( 'NONE',  ( 0.6039202388192952409, 22.55960655125555903, 43.61912269981525014 ) ) ;
#33051 = CARTESIAN_POINT ( 'NONE',  ( 0.8554163680231816613, 39.89400665120465561, -24.69157156653778529 ) ) ;
#33052 = EDGE_CURVE ( 'NONE', #6436, #41264, #25683, .T. ) ;
#33053 = CARTESIAN_POINT ( 'NONE',  ( -6.890143360408123030, -11.60930335864404306, 0.000000000000000000 ) ) ;
#33054 =( BOUNDED_SURFACE ( )  B_SPLINE_SURFACE ( 3, 1, ( 
 ( #40048, #59098 ),
 ( #6768, #45650 ),
 ( #37181, #42199 ),
 ( #3617, #7713 ) ),
 .UNSPECIFIED., .F., .F., .F. ) 
 B_SPLINE_SURFACE_WITH_KNOTS ( ( 4, 4 ),
 ( 2, 2 ),
 ( 0.000000000000000000, 1.000000000000000000 ),
 ( 0.000000000000000000, 1.000000000000000000 ),
 .UNSPECIFIED. ) 
 GEOMETRIC_REPRESENTATION_ITEM ( )  RATIONAL_B_SPLINE_SURFACE ( (
 ( 1.000000000000000000, 1.000000000000000000),
 ( 0.9754377213608244057, 0.9999580625633939235),
 ( 0.9754377213608244057, 0.9999580625633939235),
 ( 1.000000000000000000, 1.000000000000000000) ) ) 
 REPRESENTATION_ITEM ( '' )  SURFACE ( )  );
#33055 = CARTESIAN_POINT ( 'NONE',  ( 0.5807400328401574052, -23.47602859900685601, -41.75144119563910294 ) ) ;
#33056 = VERTEX_POINT ( 'NONE', #24955 ) ;
#33057 = B_SPLINE_CURVE_WITH_KNOTS ( 'NONE', 3,
 ( #49455, #2129, #11249, #40396 ),
 .UNSPECIFIED., .F., .F.,
 ( 4, 4 ),
 ( 8.673617379884035472E-19, 0.004042984057420974560 ),
 .UNSPECIFIED. ) ;
#33058 = EDGE_CURVE ( 'NONE', #21453, #35725, #47442, .T. ) ;
#33059 = CARTESIAN_POINT ( 'NONE',  ( -6.016489644550736315, -9.425415887800975057, -16.31649074174286795 ) ) ;
#33060 = CARTESIAN_POINT ( 'NONE',  ( -6.078726893082806448, 0.6137717894417996645, 19.24622886331775717 ) ) ;
#33061 = CARTESIAN_POINT ( 'NONE',  ( 0.1135584504625008345, -35.10173505342547884, -26.73612253813879036 ) ) ;
#33062 = CARTESIAN_POINT ( 'NONE',  ( 0.6029442701453591180, -39.40744528971698202, -29.30185115135630269 ) ) ;
#33063 = CARTESIAN_POINT ( 'NONE',  ( 1.112077966505211624, -23.74200319157113981, -37.13956932410471978 ) ) ;
#33065 = B_SPLINE_CURVE_WITH_KNOTS ( 'NONE', 3,
 ( #4985, #10964, #19136, #47625 ),
 .UNSPECIFIED., .F., .F.,
 ( 4, 4 ),
 ( 2.170598744017606518E-17, 0.001844835322069226938 ),
 .UNSPECIFIED. ) ;
#33064 = CARTESIAN_POINT ( 'NONE',  ( 5.960721111146673579, 0.006321279846536711350, 20.52557019979492026 ) ) ;
#33066 = CARTESIAN_POINT ( 'NONE',  ( -90.00000000000000000, 0.000000000000000000, 0.000000000000000000 ) ) ;
#33067 = VECTOR ( 'NONE', #10497, 1000.000000000000227 ) ;
#33068 = CARTESIAN_POINT ( 'NONE',  ( 2.618530812446115519, 9.522253559614673790, -46.03317799527428633 ) ) ;
#33069 = CARTESIAN_POINT ( 'NONE',  ( 4.549368137175248350, 42.14271863032822552, 8.166781970325878603 ) ) ;
#33070 = B_SPLINE_CURVE_WITH_KNOTS ( 'NONE', 3,
 ( #25388, #53880, #960, #48579, #44228, #10685, #15083, #39839, #43923, #1881, #34192, #29781, #21009, #16010, #58265, #35124, #10381, #40153, #24780 ),
 .UNSPECIFIED., .F., .F.,
 ( 4, 3, 3, 3, 3, 3, 4 ),
 ( 1.250973872328959318E-17, 0.0002732106629380648714, 0.0004098138914053863283, 0.0005464171197651537370, 0.0006830203481512621628, 0.0008196235766963708971, 0.001011968216111137908 ),
 .UNSPECIFIED. ) ;
#33072 = VERTEX_POINT ( 'NONE', #6112 ) ;
#33071 = CARTESIAN_POINT ( 'NONE',  ( 3.680974057930773924, 4.423547572561673746, 47.77138393978997755 ) ) ;
#33073 = VERTEX_POINT ( 'NONE', #2661 ) ;
#33074 = VECTOR ( 'NONE', #51744, 1000.000000000000114 ) ;
#33075 = CARTESIAN_POINT ( 'NONE',  ( 0.5848930533535030563, -25.08041605097227134, -39.62632727237903651 ) ) ;
#33076 = CARTESIAN_POINT ( 'NONE',  ( 0.5980271706414734822, -7.146479349118088464, 48.58988655835998571 ) ) ;
#33077 = CARTESIAN_POINT ( 'NONE',  ( 5.910764540655177868, 17.95751408178366759, -9.056982194511830286 ) ) ;
#33078 = EDGE_CURVE ( 'NONE', #12519, #2779, #16045, .T. ) ;
#33079 = VERTEX_POINT ( 'NONE', #50585 ) ;
#33080 = DIRECTION ( 'NONE',  ( 0.000000000000000000, -1.224646799147364547E-16, 1.000000000000000000 ) ) ;
#33081 = CARTESIAN_POINT ( 'NONE',  ( -2.739355103387247858, -0.7412303453949566912, 14.90966614401820323 ) ) ;
#33082 = LINE ( 'NONE', #51527, #5009 ) ;
#33083 = VERTEX_POINT ( 'NONE', #55277 ) ;
#33084 = ORIENTED_EDGE ( 'NONE', *, *, #44635, .F. ) ;
#33085 = CARTESIAN_POINT ( 'NONE',  ( 0.9757787079277433495, 41.43615150473016229, 11.14366644276425333 ) ) ;
#33086 = CARTESIAN_POINT ( 'NONE',  ( 4.390527457369402420, -39.72119411615135931, 18.77264165256562833 ) ) ;
#33087 = CARTESIAN_POINT ( 'NONE',  ( 1.227938101723756947, -34.55893248994489397, -25.45152231597092651 ) ) ;
#33088 = CARTESIAN_POINT ( 'NONE',  ( 0.7948878604505666967, -47.70571118704327063, -11.61308604277228262 ) ) ;
#33089 = CARTESIAN_POINT ( 'NONE',  ( 0.7242003506640013466, 48.03330260386865547, -10.18889174990159319 ) ) ;
#33090 = ADVANCED_FACE ( 'NONE', ( #23034 ), #3363, .F. ) ;
#33091 = DIRECTION ( 'NONE',  ( 0.000000000000000000, 0.000000000000000000, 1.000000000000000000 ) ) ;
#33092 = ORIENTED_EDGE ( 'NONE', *, *, #47739, .F. ) ;
#33093 = CIRCLE ( 'NONE', #3900, 47.91270532121795611 ) ;
#33094 = CARTESIAN_POINT ( 'NONE',  ( 0.8760168074887090262, 23.27577685234598448, -42.09738177923931346 ) ) ;
#33095 = CARTESIAN_POINT ( 'NONE',  ( 4.553261556744875094, 43.92594400279101308, 0.2258523573163287723 ) ) ;
#33096 = ORIENTED_EDGE ( 'NONE', *, *, #52825, .F. ) ;
#33097 = CARTESIAN_POINT ( 'NONE',  ( 0.9790850452238886170, -37.42709535634217843, -18.85602989630809745 ) ) ;
#33098 = CARTESIAN_POINT ( 'NONE',  ( 0.5804410086790514622, -2.113107284888626758, -46.85141011173459447 ) ) ;
#33099 = DIRECTION ( 'NONE',  ( 0.000000000000000000, 3.491481338843138088E-15, -1.000000000000000000 ) ) ;
#33100 = CARTESIAN_POINT ( 'NONE',  ( -17.97369999999976642, 0.000000000000000000, -1.381000053334577907E-15 ) ) ;
#33101 = ORIENTED_EDGE ( 'NONE', *, *, #57332, .F. ) ;
#33102 = ORIENTED_EDGE ( 'NONE', *, *, #26303, .F. ) ;
#33103 = CARTESIAN_POINT ( 'NONE',  ( 0.1135584504625008068, -44.12216505757947260, -0.4319754240288274927 ) ) ;
#33104 = CARTESIAN_POINT ( 'NONE',  ( -6.077587904424778920, 18.62786028128793347, 4.878405757493543327 ) ) ;
#33105 = CARTESIAN_POINT ( 'NONE',  ( 0.6041374136657475802, 6.106202762792853456, 47.71861871402591504 ) ) ;
#33106 = VECTOR ( 'NONE', #30434, 1000.000000000000227 ) ;
#33107 = VERTEX_POINT ( 'NONE', #42163 ) ;
#33108 = DIRECTION ( 'NONE',  ( -0.000000000000000000, 1.000000000000000000, -0.000000000000000000 ) ) ;
#33109 = ORIENTED_EDGE ( 'NONE', *, *, #55588, .F. ) ;
#33110 = CARTESIAN_POINT ( 'NONE',  ( 0.3676999524040366896, 43.44964275340416293, 7.620966337964807380 ) ) ;
#33111 = CARTESIAN_POINT ( 'NONE',  ( 0.5817217712918332229, 27.44989446949152523, 38.02286480030341664 ) ) ;
#33112 = B_SPLINE_CURVE_WITH_KNOTS ( 'NONE', 3,
 ( #50514, #60830, #12030, #61133 ),
 .UNSPECIFIED., .F., .F.,
 ( 4, 4 ),
 ( 0.000000000000000000, 0.004444103432399266161 ),
 .UNSPECIFIED. ) ;
#33113 = ORIENTED_EDGE ( 'NONE', *, *, #24112, .F. ) ;
#33114 = CARTESIAN_POINT ( 'NONE',  ( 0.5839880159502339740, -47.48028790449882308, -6.296669079378655276 ) ) ;
#33115 = CARTESIAN_POINT ( 'NONE',  ( 0.5806925824938499181, -46.06186276235273169, 8.804950948514585818 ) ) ;
#33116 = CARTESIAN_POINT ( 'NONE',  ( 0.9736507210033066295, 26.47691119766837531, -33.76542629919376992 ) ) ;
#33117 = ORIENTED_EDGE ( 'NONE', *, *, #33773, .T. ) ;
#33118 = DIRECTION ( 'NONE',  ( -1.000000000000000000, -0.000000000000000000, -0.000000000000000000 ) ) ;
#33119 = B_SPLINE_CURVE_WITH_KNOTS ( 'NONE', 3,
 ( #16723, #46170, #54911, #26113, #3216, #40866, #21726, #30487, #40251, #7604, #35533, #12046, #50531, #45868, #2913, #7930 ),
 .UNSPECIFIED., .F., .F.,
 ( 4, 3, 3, 3, 3, 4 ),
 ( 2.194378057379452319E-17, 0.0002612764279487740844, 0.0003919131003184766972, 0.0005225497727000625453, 0.0007837925190632439448, 0.001045051706266715433 ),
 .UNSPECIFIED. ) ;
#33120 = DIRECTION ( 'NONE',  ( 1.000000000000000000, 1.836909530733573776E-16, 0.000000000000000000 ) ) ;
#33121 = CARTESIAN_POINT ( 'NONE',  ( 4.291220156522059348, 44.81988414002803012, 14.51092633087771411 ) ) ;
#33122 = CARTESIAN_POINT ( 'NONE',  ( 0.3622758884714730732, 10.35929834645922831, -41.85013935980092015 ) ) ;
#33123 = CARTESIAN_POINT ( 'NONE',  ( 0.1104177457020372594, 16.49849172082163662, -39.84367193872661517 ) ) ;
#33124 = EDGE_LOOP ( 'NONE', ( #58141, #3463, #61395, #19614 ) ) ;
#33125 = EDGE_CURVE ( 'NONE', #6666, #21601, #22036, .T. ) ;
#33126 = CARTESIAN_POINT ( 'NONE',  ( 0.8554163680231720024, -46.15020320557298561, -8.447734441620465162 ) ) ;
#33127 = CYLINDRICAL_SURFACE ( 'NONE', #43865, 85.00000000000001421 ) ;
#33128 = ORIENTED_EDGE ( 'NONE', *, *, #49782, .F. ) ;
#33129 = EDGE_CURVE ( 'NONE', #34855, #46145, #55620, .T. ) ;
#33130 = CARTESIAN_POINT ( 'NONE',  ( 0.5839879882104919151, -5.421203860810959572E-16, -47.89596766822081975 ) ) ;
#33131 = CARTESIAN_POINT ( 'NONE',  ( 5.965394784446460541, 5.298374383010361122, 19.82972329408687884 ) ) ;
#33132 = CARTESIAN_POINT ( 'NONE',  ( 5.895596859100789899, -17.30698493747188849, 10.24677781483567607 ) ) ;
#33133 = CARTESIAN_POINT ( 'NONE',  ( 0.7056759521544990754, -6.968496825407635598, -46.38091074042502271 ) ) ;
#33134 = CARTESIAN_POINT ( 'NONE',  ( 4.549368137175248350, 0.000000000000000000, 0.000000000000000000 ) ) ;
#33135 = CARTESIAN_POINT ( 'NONE',  ( -6.016489644550737204, 4.881234076340629890, -18.19999694163059090 ) ) ;
#33136 = EDGE_CURVE ( 'NONE', #19210, #9240, #57845, .T. ) ;
#33137 = CARTESIAN_POINT ( 'NONE',  ( 0.5837799406558236148, 10.96004523085180615, 45.59737885136471647 ) ) ;
#33138 = B_SPLINE_CURVE_WITH_KNOTS ( 'NONE', 3,
 ( #56605, #42239, #38157, #33445, #14339, #9611 ),
 .UNSPECIFIED., .F., .F.,
 ( 4, 2, 4 ),
 ( 0.000000000000000000, 0.0002291966416970781027, 0.0004583932833941562054 ),
 .UNSPECIFIED. ) ;
#33139 = CARTESIAN_POINT ( 'NONE',  ( -6.001507490154110336, 18.19774963328914907, -4.892199142591112881 ) ) ;
#33140 = CARTESIAN_POINT ( 'NONE',  ( 3.240649175237395152, -3.235903588307554646, 43.87247252395092545 ) ) ;
#33141 = CARTESIAN_POINT ( 'NONE',  ( 0.1073791018717578927, 21.98088480513665388, -37.10214135362866728 ) ) ;
#33142 = VERTEX_POINT ( 'NONE', #32123 ) ;
#33143 = CARTESIAN_POINT ( 'NONE',  ( 1.091591847532195736, -2.180174137653107191, 41.85696873503080440 ) ) ;
#33144 = DIRECTION ( 'NONE',  ( 1.000000000000000000, -0.000000000000000000, -0.000000000000000000 ) ) ;
#33145 = EDGE_CURVE ( 'NONE', #31335, #38495, #20471, .T. ) ;
#33146 = CARTESIAN_POINT ( 'NONE',  ( -6.063463321072278589, 3.088760411028451003, -19.00736729804350134 ) ) ;
#33147 = CARTESIAN_POINT ( 'NONE',  ( 0.5997462898726536595, -35.63787911784747564, -33.78599121124021565 ) ) ;
#33148 = CARTESIAN_POINT ( 'NONE',  ( 4.390527457369401532, 31.78221389532359709, -30.33275814265031656 ) ) ;
#33149 = ORIENTED_EDGE ( 'NONE', *, *, #16564, .F. ) ;
#33150 = CARTESIAN_POINT ( 'NONE',  ( 0.000000000000000000, 0.000000000000000000, -5.600000000000000533 ) ) ;
#33151 = CARTESIAN_POINT ( 'NONE',  ( 5.896278296736517710, 10.81775449038653925, 16.95591835908941647 ) ) ;
#33152 = CARTESIAN_POINT ( 'NONE',  ( -6.072942160501519027, 0.6026766405721472042, 19.24684242040572002 ) ) ;
#33153 = ORIENTED_EDGE ( 'NONE', *, *, #43822, .F. ) ;
#33154 = CARTESIAN_POINT ( 'NONE',  ( 0.9972139404380286898, -11.74016833743892008, -41.27214627875022046 ) ) ;
#33155 = CARTESIAN_POINT ( 'NONE',  ( 0.5835226383429280572, 43.24565384930013323, 18.13989795154533624 ) ) ;
#33156 = ORIENTED_EDGE ( 'NONE', *, *, #28129, .T. ) ;
#33157 = APPLICATION_CONTEXT ( 'automotive_design' ) ;
#33158 =( BOUNDED_SURFACE ( )  B_SPLINE_SURFACE ( 3, 1, ( 
 ( #59683, #59369 ),
 ( #16473, #12108 ),
 ( #35604, #54665 ),
 ( #31184, #28641 ) ),
 .UNSPECIFIED., .F., .F., .F. ) 
 B_SPLINE_SURFACE_WITH_KNOTS ( ( 4, 4 ),
 ( 2, 2 ),
 ( 0.000000000000000000, 1.000000000000000000 ),
 ( 0.000000000000000000, 1.000000000000000000 ),
 .UNSPECIFIED. ) 
 GEOMETRIC_REPRESENTATION_ITEM ( )  RATIONAL_B_SPLINE_SURFACE ( (
 ( 1.000000000000000000, 1.000000000000000000),
 ( 0.7282232189291693025, 0.9929344683865674037),
 ( 0.7282232189291693025, 0.9929344683865674037),
 ( 1.000000000000000000, 1.000000000000000000) ) ) 
 REPRESENTATION_ITEM ( '' )  SURFACE ( )  );
#33159 = B_SPLINE_CURVE_WITH_KNOTS ( 'NONE', 3,
 ( #17949, #42081, #61132, #18253, #37364, #55554 ),
 .UNSPECIFIED., .F., .F.,
 ( 4, 2, 4 ),
 ( 3.471140604459641645E-18, 0.0002291966416970821143, 0.0004583932833941607591 ),
 .UNSPECIFIED. ) ;
#33160 = CARTESIAN_POINT ( 'NONE',  ( 3.221118495291109163, -25.92278810600130612, 35.53548193669403332 ) ) ;
#33161 = ORIENTED_EDGE ( 'NONE', *, *, #18089, .F. ) ;
#33162 = CARTESIAN_POINT ( 'NONE',  ( 0.2285344041767058687, 42.10476663782116447, 13.17914248614367168 ) ) ;
#33163 = CARTESIAN_POINT ( 'NONE',  ( -6.016489644550736315, 7.206912786933527215, -17.41053539857192334 ) ) ;
#33164 = B_SPLINE_CURVE_WITH_KNOTS ( 'NONE', 3,
 ( #19342, #38458, #14649, #47232 ),
 .UNSPECIFIED., .F., .F.,
 ( 4, 4 ),
 ( 0.000000000000000000, 0.005013413432710139839 ),
 .UNSPECIFIED. ) ;
#33165 = EDGE_LOOP ( 'NONE', ( #38053, #9468, #12937, #35027, #53873, #9318, #16728, #8971, #6618, #5984, #48605, #22040, #8580, #22345, #9511, #23509, #51440, #56937, #46990, #12579, #31606, #25004, #46436, #45812, #40659, #30056, #50359, #46796, #28763, #48181, #49480, #12314, #13533, #53689, #60872, #26765, #34636, #2023, #58304, #39810, #29806, #52934, #3963, #53018, #58218, #21842, #39103, #22289, #34687, #34432, #44837, #41509, #22287, #24561, #21682, #6307, #34258, #46426, #37886, #61026, #5310, #56471, #25676, #51895, #3009, #3644, #55228, #15701, #42195, #10582, #3165, #19459, #21072, #53125, #28977, #47173, #57463, #6836, #31177, #9822, #12164, #44105, #53790, #54419, #57148, #57951, #27128, #3449, #4192, #31770, #26834, #26606, #33536, #39243, #17443, #2060, #34622, #22851, #56768, #51328, #40203, #59191, #36979, #8689, #15431, #53553, #53991, #34127, #31762, #4706, #44964, #61365, #2457, #23319, #56769, #20875, #54383, #24511, #29383, #15050, #30572, #19986, #124, #15913, #49870, #55645, #16309, #23893, #2884, #57276, #12590, #34265, #59183, #1670, #37274, #35165, #20314, #4615, #24128, #28704, #41971, #61875, #49503, #37406, #49295, #50910, #19898, #27133 ) ) ;
#33166 = CARTESIAN_POINT ( 'NONE',  ( 4.975610109902397937, 0.000000000000000000, 0.000000000000000000 ) ) ;
#33167 = CARTESIAN_POINT ( 'NONE',  ( 0.5819845901640484653, -29.51612926147643279, 37.72030663501146819 ) ) ;
#33168 = CARTESIAN_POINT ( 'NONE',  ( -16.60577576646022990, 5.000000000000008882, 10.00000000000000711 ) ) ;
#33169 = CARTESIAN_POINT ( 'NONE',  ( 0.5997462898726536595, -43.04230894295751852, 23.64130434225888777 ) ) ;
#33170 = EDGE_CURVE ( 'NONE', #60259, #461, #31813, .T. ) ;
#33171 = ORIENTED_EDGE ( 'NONE', *, *, #53666, .F. ) ;
#33172 = B_SPLINE_CURVE_WITH_KNOTS ( 'NONE', 3,
 ( #58975, #16085, #6631, #49576 ),
 .UNSPECIFIED., .F., .F.,
 ( 4, 4 ),
 ( 1.084202172485504434E-19, 0.004446298630425088438 ),
 .UNSPECIFIED. ) ;
#33173 = EDGE_CURVE ( 'NONE', #14400, #3122, #16397, .T. ) ;
#33174 = CARTESIAN_POINT ( 'NONE',  ( 0.9790850452238877288, -7.020569879040508887, -41.31644864744191636 ) ) ;
#33175 = ORIENTED_EDGE ( 'NONE', *, *, #32181, .T. ) ;
#33176 = CARTESIAN_POINT ( 'NONE',  ( 0.5807400328401637335, -28.72484455891667565, 38.33001520688940644 ) ) ;
#33177 = ORIENTED_EDGE ( 'NONE', *, *, #24991, .F. ) ;
#33178 = EDGE_CURVE ( 'NONE', #14690, #1876, #6339, .T. ) ;
#33179 = ORIENTED_EDGE ( 'NONE', *, *, #5894, .T. ) ;
#33180 = CARTESIAN_POINT ( 'NONE',  ( 1.088313998177379505, -42.43756598879024722, -6.373602917100628318 ) ) ;
#33181 = CARTESIAN_POINT ( 'NONE',  ( 0.9785694773339239649, -37.50411832126101785, 18.70231308313300289 ) ) ;
#33182 = B_SPLINE_CURVE_WITH_KNOTS ( 'NONE', 3,
 ( #54712, #30928, #34716, #53779 ),
 .UNSPECIFIED., .F., .F.,
 ( 4, 4 ),
 ( 0.000000000000000000, 0.004445488388166993383 ),
 .UNSPECIFIED. ) ;
#33183 = CARTESIAN_POINT ( 'NONE',  ( 0.1092355843206037486, -16.78033551728689687, 39.72582785521888837 ) ) ;
#33184 = CARTESIAN_POINT ( 'NONE',  ( 1.479689385636123067, -28.38236120443074029, -33.70497615677716396 ) ) ;
#33185 = VERTEX_POINT ( 'NONE', #51506 ) ;
#33186 = CARTESIAN_POINT ( 'NONE',  ( -6.078726893082806448, -1.852420388636693227, 19.16670498475111373 ) ) ;
#33187 = CARTESIAN_POINT ( 'NONE',  ( 5.838029081930957709, -32.82243551873150267, 33.96693664096945042 ) ) ;
#33188 = CARTESIAN_POINT ( 'NONE',  ( 0.1139756605157203756, -38.24967839416645177, 21.99812088424507195 ) ) ;
#33189 = ORIENTED_EDGE ( 'NONE', *, *, #52756, .T. ) ;
#33190 = AXIS2_PLACEMENT_3D ( 'NONE', #60962, #27153, #13376 ) ;
#33191 = ORIENTED_EDGE ( 'NONE', *, *, #41972, .T. ) ;
#33192 = CONICAL_SURFACE ( 'NONE', #12186, 43.08621763946400307, 1.568696531533066763 ) ;
#33193 = DIRECTION ( 'NONE',  ( 0.000000000000000000, 0.000000000000000000, 1.000000000000000000 ) ) ;
#33194 = CARTESIAN_POINT ( 'NONE',  ( 5.960721111146673579, -19.82781442290494311, -5.306302591836510985 ) ) ;
#33195 = DIRECTION ( 'NONE',  ( 1.000000000000000000, 1.836909530733573776E-16, 0.000000000000000000 ) ) ;
#33196 = CARTESIAN_POINT ( 'NONE',  ( 0.2224561200757623480, -42.64482917976811649, -6.380320192201828000 ) ) ;
#33197 = CARTESIAN_POINT ( 'NONE',  ( 1.227938101723756947, 33.52879263017899092, -26.79402671879293507 ) ) ;
#33198 = ORIENTED_EDGE ( 'NONE', *, *, #45861, .T. ) ;
#33199 = EDGE_CURVE ( 'NONE', #17422, #34160, #6230, .T. ) ;
#33200 = ORIENTED_EDGE ( 'NONE', *, *, #21284, .F. ) ;
#33201 = ADVANCED_FACE ( 'NONE', ( #17710 ), #60262, .F. ) ;
#33202 = DIRECTION ( 'NONE',  ( 0.000000000000000000, 0.000000000000000000, 1.000000000000000000 ) ) ;
#33203 = CARTESIAN_POINT ( 'NONE',  ( -6.015611763856276717, -14.95313250337422062, -11.46610900684738432 ) ) ;
#33204 = B_SPLINE_CURVE_WITH_KNOTS ( 'NONE', 3,
 ( #33702, #13985, #58084, #15203, #34311, #52777 ),
 .UNSPECIFIED., .F., .F.,
 ( 4, 2, 4 ),
 ( 6.345130535746553974E-19, 0.0002293801035737092365, 0.0004587602071474178767 ),
 .UNSPECIFIED. ) ;
#33205 = LINE ( 'NONE', #51663, #4980 ) ;
#33206 = CARTESIAN_POINT ( 'NONE',  ( 0.8744876279028263033, -2.462621419133342204, 49.03351451941333750 ) ) ;
#33207 = ADVANCED_FACE ( 'NONE', ( #59990 ), #22400, .F. ) ;
#33208 =( LENGTH_UNIT ( ) NAMED_UNIT ( * ) SI_UNIT ( .MILLI., .METRE. ) );
#33209 = CARTESIAN_POINT ( 'NONE',  ( 0.6067099128993264090, -34.36589933408221498, -33.36330296770427850 ) ) ;
#33210 = ORIENTED_EDGE ( 'NONE', *, *, #46906, .T. ) ;
#33211 = CARTESIAN_POINT ( 'NONE',  ( 2.648799415243696664, 48.82680556394801386, 4.523330820315231371 ) ) ;
#33212 = CARTESIAN_POINT ( 'NONE',  ( 1.157644175074336923, -39.86048670168759855, 12.96703032246667853 ) ) ;
#33213 = CARTESIAN_POINT ( 'NONE',  ( -5.995132425357893702, -9.414704407577920264, 16.32377331145317712 ) ) ;
#33214 = CARTESIAN_POINT ( 'NONE',  ( 0.1092355843206037486, -16.22491322981600348, -39.95589129953361152 ) ) ;
#33215 = CARTESIAN_POINT ( 'NONE',  ( 0.9791128995231609400, 29.13826394149679189, 30.12140449450908619 ) ) ;
#33216 = EDGE_CURVE ( 'NONE', #21472, #28471, #14259, .T. ) ;
#33217 = PLANE ( 'NONE',  #15166 ) ;
#33218 = CARTESIAN_POINT ( 'NONE',  ( 4.962356264823608143, 0.000000000000000000, 0.000000000000000000 ) ) ;
#33219 =( BOUNDED_SURFACE ( )  B_SPLINE_SURFACE ( 3, 1, ( 
 ( #40221, #25452 ),
 ( #54559, #21386 ),
 ( #17011, #55191 ),
 ( #20772, #16079 ) ),
 .UNSPECIFIED., .F., .F., .F. ) 
 B_SPLINE_SURFACE_WITH_KNOTS ( ( 4, 4 ),
 ( 2, 2 ),
 ( 0.000000000000000000, 1.000000000000000000 ),
 ( 0.000000000000000000, 1.000000000000000000 ),
 .UNSPECIFIED. ) 
 GEOMETRIC_REPRESENTATION_ITEM ( )  RATIONAL_B_SPLINE_SURFACE ( (
 ( 1.000000000000000000, 1.000000000000000000),
 ( 0.9952954269826590483, 0.8620686068821307169),
 ( 0.9952954269826590483, 0.8620686068821307169),
 ( 1.000000000000000000, 1.000000000000000000) ) ) 
 REPRESENTATION_ITEM ( '' )  SURFACE ( )  );
#33220 = CARTESIAN_POINT ( 'NONE',  ( -1.114299999999999624, 0.000000000000000000, 0.000000000000000000 ) ) ;
#33221 = ORIENTED_EDGE ( 'NONE', *, *, #14948, .T. ) ;
#33222 = CARTESIAN_POINT ( 'NONE',  ( 4.000000000000003553, -2.309401076758539784, -5.599999999999999645 ) ) ;
#33223 = B_SPLINE_CURVE_WITH_KNOTS ( 'NONE', 3,
 ( #12838, #51016, #34101, #29677 ),
 .UNSPECIFIED., .F., .F.,
 ( 4, 4 ),
 ( 0.000000000000000000, 0.005014147105413711662 ),
 .UNSPECIFIED. ) ;
#33224 = CARTESIAN_POINT ( 'NONE',  ( 4.390527457369401532, 23.04872909145247561, -37.40242537453222127 ) ) ;
#33225 = CARTESIAN_POINT ( 'NONE',  ( 4.834790513006555379, -44.98626621068886067, -14.45078521553118733 ) ) ;
#33226 = CARTESIAN_POINT ( 'NONE',  ( 0.5797568599927133137, -2.195683865110441779, 46.84446905490015212 ) ) ;
#33227 = ORIENTED_EDGE ( 'NONE', *, *, #25597, .T. ) ;
#33228 = CARTESIAN_POINT ( 'NONE',  ( 0.5809828226811617480, 41.74875432577682233, -23.47450554821666202 ) ) ;
#33229 = CARTESIAN_POINT ( 'NONE',  ( 0.5848930533535030563, -44.36099898510395434, 15.21101086158195237 ) ) ;
#33230 = VECTOR ( 'NONE', #28558, 1000.000000000000114 ) ;
#33231 = DIRECTION ( 'NONE',  ( -1.000000000000000000, -0.000000000000000000, -0.000000000000000000 ) ) ;
#33232 =( BOUNDED_SURFACE ( )  B_SPLINE_SURFACE ( 3, 1, ( 
 ( #56117, #50806 ),
 ( #55190, #23240 ),
 ( #3188, #13540 ),
 ( #56424, #41138 ) ),
 .UNSPECIFIED., .F., .F., .F. ) 
 B_SPLINE_SURFACE_WITH_KNOTS ( ( 4, 4 ),
 ( 2, 2 ),
 ( 0.000000000000000000, 1.000000000000000000 ),
 ( 0.000000000000000000, 1.000000000000000000 ),
 .UNSPECIFIED. ) 
 GEOMETRIC_REPRESENTATION_ITEM ( )  RATIONAL_B_SPLINE_SURFACE ( (
 ( 1.000000000000000000, 1.000000000000000000),
 ( 0.9953040768229013402, 0.8617119497784988535),
 ( 0.9953040768229013402, 0.8617119497784988535),
 ( 1.000000000000000000, 1.000000000000000000) ) ) 
 REPRESENTATION_ITEM ( '' )  SURFACE ( )  );
#33233 = AXIS2_PLACEMENT_3D ( 'NONE', #17630, #32351, #41455 ) ;
#33234 = ORIENTED_EDGE ( 'NONE', *, *, #50084, .F. ) ;
#33235 = CARTESIAN_POINT ( 'NONE',  ( 5.965394784446460541, -19.82972329408689305, 5.298374383010291844 ) ) ;
#33236 = CARTESIAN_POINT ( 'NONE',  ( 0.5830081025819932039, -46.00989229531988656, -9.073138671667642541 ) ) ;
#33237 = CARTESIAN_POINT ( 'NONE',  ( -6.078075953587585900, 17.84675544569229899, 7.231078364171431794 ) ) ;
#33238 = ORIENTED_EDGE ( 'NONE', *, *, #7532, .F. ) ;
#33239 = FACE_OUTER_BOUND ( 'NONE', #7866, .T. ) ;
#33240 = ORIENTED_EDGE ( 'NONE', *, *, #21171, .F. ) ;
#33241 = DIRECTION ( 'NONE',  ( 1.836909530733573776E-16, -1.000000000000000000, 0.000000000000000000 ) ) ;
#33242 = ORIENTED_EDGE ( 'NONE', *, *, #30680, .F. ) ;
#33243 = CARTESIAN_POINT ( 'NONE',  ( 4.962356264823600149, -32.75738977283805298, 26.42326651140453109 ) ) ;
#33244 = CARTESIAN_POINT ( 'NONE',  ( 2.643462169533600914, -43.83256147628719646, -19.65219740572174345 ) ) ;
#33245 = EDGE_CURVE ( 'NONE', #33948, #31234, #19059, .T. ) ;
#33246 = EDGE_LOOP ( 'NONE', ( #24055, #60578, #49785, #30193 ) ) ;
#33247 = CARTESIAN_POINT ( 'NONE',  ( -6.015611763856276717, 4.870987357968176390, 18.20278301740938431 ) ) ;
#33248 = ORIENTED_EDGE ( 'NONE', *, *, #51418, .T. ) ;
#33249 = EDGE_CURVE ( 'NONE', #29382, #3160, #27394, .T. ) ;
#33250 = CARTESIAN_POINT ( 'NONE',  ( 5.860006189529234355, -40.09484204000618490, 26.81109398084693396 ) ) ;
#33251 = CARTESIAN_POINT ( 'NONE',  ( 0.6029303876144825880, -38.24575311130019628, 29.18200390283984191 ) ) ;
#33252 = B_SPLINE_CURVE_WITH_KNOTS ( 'NONE', 3,
 ( #3348, #47221, #46930, #46303 ),
 .UNSPECIFIED., .F., .F.,
 ( 4, 4 ),
 ( 5.969062235490920269E-17, 0.005004741218457481322 ),
 .UNSPECIFIED. ) ;
#33253 = DIRECTION ( 'NONE',  ( 0.000000000000000000, 0.000000000000000000, 1.000000000000000000 ) ) ;
#33254 = EDGE_CURVE ( 'NONE', #17733, #59505, #52635, .T. ) ;
#33255 = ORIENTED_EDGE ( 'NONE', *, *, #39405, .F. ) ;
#33256 = EDGE_CURVE ( 'NONE', #33762, #44988, #7017, .T. ) ;
#33257 = CARTESIAN_POINT ( 'NONE',  ( 0.9756008150404599233, -16.55159915785250035, -39.58764833544695705 ) ) ;
#33258 = CARTESIAN_POINT ( 'NONE',  ( 0.6845945791218023269, 21.77999332122274012, -41.54561844095520939 ) ) ;
#33259 = DIRECTION ( 'NONE',  ( 0.1736481776669315247, -0.9848077530122079093, 5.551115123125782702E-17 ) ) ;
#33260 = LINE ( 'NONE', #57628, #4654 ) ;
#33262 = ADVANCED_FACE ( 'NONE', ( #33980 ), #17483, .F. ) ;
#33261 = EDGE_LOOP ( 'NONE', ( #55174, #28758, #46579, #40654 ) ) ;
#33263 = CARTESIAN_POINT ( 'NONE',  ( 0.1157991065609915993, -17.93514196423987528, 40.31467534608533754 ) ) ;
#33264 = ORIENTED_EDGE ( 'NONE', *, *, #7861, .F. ) ;
#33265 = CARTESIAN_POINT ( 'NONE',  ( 0.5830082357119578118, 43.28068137227774770, -18.05587591034304396 ) ) ;
#33266 = ORIENTED_EDGE ( 'NONE', *, *, #42404, .F. ) ;
#33267 = CARTESIAN_POINT ( 'NONE',  ( 0.5980894510889448457, -46.28687279963683920, -13.12879507229272136 ) ) ;
#33268 = EDGE_CURVE ( 'NONE', #31990, #17395, #13955, .T. ) ;
#33269 = CARTESIAN_POINT ( 'NONE',  ( 0.5837157313716030416, 10.95998063749551044, -45.59732325485506976 ) ) ;
#33270 = ORIENTED_EDGE ( 'NONE', *, *, #33256, .T. ) ;
#33271 = CARTESIAN_POINT ( 'NONE',  ( 0.6845945791218034371, 39.91187923413946237, 24.64646864590162068 ) ) ;
#33272 = CARTESIAN_POINT ( 'NONE',  ( -6.077587904424778920, -12.94128980615176872, -14.25899854643104803 ) ) ;
#33273 = CARTESIAN_POINT ( 'NONE',  ( 0.2285344041767088386, -0.6544525949336760240, 44.11431584073858403 ) ) ;
#33274 = DIRECTION ( 'NONE',  ( -0.07500201931887527651, 0.9652320423656555182, 0.2504032777116073083 ) ) ;
#33275 = EDGE_CURVE ( 'NONE', #10036, #41130, #57713, .T. ) ;
#33276 = ORIENTED_EDGE ( 'NONE', *, *, #38868, .T. ) ;
#33277 = CARTESIAN_POINT ( 'NONE',  ( 4.694002226626921015, -45.47116547585233803, -3.264641130934661017 ) ) ;
#33278 = CARTESIAN_POINT ( 'NONE',  ( 0.5807400328401637335, 29.58941477093015493, 37.66660715020876893 ) ) ;
#33279 = FACE_OUTER_BOUND ( 'NONE', #27009, .T. ) ;
#33280 = AXIS2_PLACEMENT_3D ( 'NONE', #3440, #17267, #45177 ) ;
#33281 = ADVANCED_BREP_SHAPE_REPRESENTATION ( '', ( #7748, #14677 ), #12915 ) ;
#33282 = CARTESIAN_POINT ( 'NONE',  ( -6.077587904424778920, 9.976910903712887801, 16.46988980574263906 ) ) ;
#33283 = CARTESIAN_POINT ( 'NONE',  ( 0.6000166863083106206, -39.04292238714129581, -29.79049669240368203 ) ) ;
#33284 = FACE_OUTER_BOUND ( 'NONE', #34073, .T. ) ;
#33285 = CARTESIAN_POINT ( 'NONE',  ( 0.5800708119828335008, 33.42085299104068952, -34.30831427709716763 ) ) ;
#33286 = CARTESIAN_POINT ( 'NONE',  ( 3.407937589446174087, 4.815089211105057387, 12.82481284928205234 ) ) ;
#33287 = CARTESIAN_POINT ( 'NONE',  ( 4.691466044806103852, -33.74235639413308263, -29.14742760351097672 ) ) ;
#33288 = CARTESIAN_POINT ( 'NONE',  ( 5.917102823773431552, -4.653982686479870345, -19.56604618224355363 ) ) ;
#33289 = EDGE_CURVE ( 'NONE', #44428, #26819, #38353, .T. ) ;
#33290 = CARTESIAN_POINT ( 'NONE',  ( 0.5806925824938511393, 32.99217760300656010, 33.32774488853447536 ) ) ;
#33291 = CARTESIAN_POINT ( 'NONE',  ( 0.9968887458511651589, -34.43855515351788910, 25.59699785741774392 ) ) ;
#33292 = CARTESIAN_POINT ( 'NONE',  ( -2.601141883200662974, 14.91765895884288362, 0.5088011959923715022 ) ) ;
#33293 = DIRECTION ( 'NONE',  ( -0.07500201931887527651, -0.9463514676414596094, -0.3143144870841088623 ) ) ;
#33294 = EDGE_CURVE ( 'NONE', #52389, #37253, #18148, .T. ) ;
#33295 = CARTESIAN_POINT ( 'NONE',  ( 0.9730545539215883499, -36.90443313492315980, -21.89037132892475057 ) ) ;
#33296 = B_SPLINE_CURVE_WITH_KNOTS ( 'NONE', 3,
 ( #13039, #49679, #30878, #59689, #54981, #31190 ),
 .UNSPECIFIED., .F., .F.,
 ( 4, 2, 4 ),
 ( 0.000000000000000000, 0.0002447195606305758303, 0.0004894391212611516606 ),
 .UNSPECIFIED. ) ;
#33297 = CARTESIAN_POINT ( 'NONE',  ( 0.8751705887134423323, 11.58504748649134974, 46.67919521768892110 ) ) ;
#33298 = CARTESIAN_POINT ( 'NONE',  ( 0.1152339509894530906, 37.10134772748614296, 23.88373269108917896 ) ) ;
#33299 = VERTEX_POINT ( 'NONE', #44315 ) ;
#33300 = CARTESIAN_POINT ( 'NONE',  ( 0.6029442701453591180, -39.30324803684850110, 29.44146597763503337 ) ) ;
#33301 = CARTESIAN_POINT ( 'NONE',  ( 0.09136607875274982415, 0.000000000000000000, 0.000000000000000000 ) ) ;
#33302 = CARTESIAN_POINT ( 'NONE',  ( 2.301430502907646058, -33.04218380901196639, -34.86297247504463570 ) ) ;
#33303 = ORIENTED_EDGE ( 'NONE', *, *, #28036, .T. ) ;
#33304 = CARTESIAN_POINT ( 'NONE',  ( 0.5839254288179541730, -33.93171296845864049, 33.80331890503256176 ) ) ;
#33305 = CARTESIAN_POINT ( 'NONE',  ( -6.077587904424778920, 15.42837212129427193, -11.52221137980032495 ) ) ;
#33306 = ORIENTED_EDGE ( 'NONE', *, *, #43181, .T. ) ;
#33307 = ORIENTED_EDGE ( 'NONE', *, *, #12776, .T. ) ;
#33308 = CARTESIAN_POINT ( 'NONE',  ( 0.6009452777970414328, -38.43042656245054900, -28.93864923253884669 ) ) ;
#33310 = ORIENTED_EDGE ( 'NONE', *, *, #10654, .F. ) ;
#33309 =( BOUNDED_SURFACE ( )  B_SPLINE_SURFACE ( 3, 1, ( 
 ( #60153, #13805 ),
 ( #27572, #46702 ),
 ( #55449, #56993 ),
 ( #10322, #14116 ) ),
 .UNSPECIFIED., .F., .F., .F. ) 
 B_SPLINE_SURFACE_WITH_KNOTS ( ( 4, 4 ),
 ( 2, 2 ),
 ( 0.000000000000000000, 1.000000000000000000 ),
 ( 0.000000000000000000, 1.000000000000000000 ),
 .UNSPECIFIED. ) 
 GEOMETRIC_REPRESENTATION_ITEM ( )  RATIONAL_B_SPLINE_SURFACE ( (
 ( 1.000000000000000000, 1.000000000000000000),
 ( 0.7223157951917480446, 0.9931996967497186413),
 ( 0.7223157951917480446, 0.9931996967497186413),
 ( 1.000000000000000000, 1.000000000000000000) ) ) 
 REPRESENTATION_ITEM ( '' )  SURFACE ( )  );
#33311 = CARTESIAN_POINT ( 'NONE',  ( 5.958863334805807099, 7.853699934219627643, 18.96369761673823007 ) ) ;
#33312 = LINE ( 'NONE', #28584, #9963 ) ;
#33313 = ORIENTED_EDGE ( 'NONE', *, *, #61913, .T. ) ;
#33314 = EDGE_LOOP ( 'NONE', ( #39253, #14912, #44205, #58348 ) ) ;
#33315 = CARTESIAN_POINT ( 'NONE',  ( 0.5834872094924180574, -12.17696997821490434, -46.32218741137609186 ) ) ;
#33316 = EDGE_CURVE ( 'NONE', #20594, #40325, #42446, .T. ) ;
#33317 = ORIENTED_EDGE ( 'NONE', *, *, #29840, .F. ) ;
#33318 = LINE ( 'NONE', #4449, #22578 ) ;
#33319 = CARTESIAN_POINT ( 'NONE',  ( 2.648799415243696664, 21.44335952302192183, 44.09875049994073493 ) ) ;
#33320 = B_SPLINE_CURVE_WITH_KNOTS ( 'NONE', 3,
 ( #4031, #18171, #13169, #51042 ),
 .UNSPECIFIED., .F., .F.,
 ( 4, 4 ),
 ( 0.000000000000000000, 0.005013413432710144176 ),
 .UNSPECIFIED. ) ;
#33321 = AXIS2_PLACEMENT_3D ( 'NONE', #13241, #41765, #37061 ) ;
#33322 = CARTESIAN_POINT ( 'NONE',  ( -6.079354080745853928, 17.84913307564918128, 7.225053888790617052 ) ) ;
#33323 = ORIENTED_EDGE ( 'NONE', *, *, #25246, .F. ) ;
#33324 = EDGE_CURVE ( 'NONE', #37740, #9990, #6335, .T. ) ;
#33325 = CARTESIAN_POINT ( 'NONE',  ( 0.8751705887134553219, -44.76769609654225235, -17.57879340691528469 ) ) ;
#33326 = LINE ( 'NONE', #44898, #22982 ) ;
#33327 = ORIENTED_EDGE ( 'NONE', *, *, #37298, .T. ) ;
#33328 = ORIENTED_EDGE ( 'NONE', *, *, #61154, .F. ) ;
#33329 = EDGE_CURVE ( 'NONE', #8407, #52560, #53289, .T. ) ;
#33330 =( BOUNDED_SURFACE ( )  B_SPLINE_SURFACE ( 3, 1, ( 
 ( #28182, #14114 ),
 ( #42613, #23482 ),
 ( #47610, #42929 ),
 ( #49960, #9692 ) ),
 .UNSPECIFIED., .F., .F., .F. ) 
 B_SPLINE_SURFACE_WITH_KNOTS ( ( 4, 4 ),
 ( 2, 2 ),
 ( 0.000000000000000000, 1.000000000000000000 ),
 ( 0.000000000000000000, 1.000000000000000000 ),
 .UNSPECIFIED. ) 
 GEOMETRIC_REPRESENTATION_ITEM ( )  RATIONAL_B_SPLINE_SURFACE ( (
 ( 1.000000000000000000, 1.000000000000000000),
 ( 0.9754377213608244057, 0.9999580625633939235),
 ( 0.9754377213608244057, 0.9999580625633939235),
 ( 1.000000000000000000, 1.000000000000000000) ) ) 
 REPRESENTATION_ITEM ( '' )  SURFACE ( )  );
#33331 = CARTESIAN_POINT ( 'NONE',  ( 0.8760168074886965917, -38.69913431881842314, 28.57146030081914390 ) ) ;
#33332 = VERTEX_POINT ( 'NONE', #5726 ) ;
#33333 = CARTESIAN_POINT ( 'NONE',  ( 0.5549461598389366923, 34.14561923851002234, 27.91584464574730973 ) ) ;
#33334 = FACE_OUTER_BOUND ( 'NONE', #11304, .T. ) ;
#33335 = CARTESIAN_POINT ( 'NONE',  ( 0.1129192098497455998, -31.35755906439593943, -31.04279751098591689 ) ) ;
#33336 = EDGE_CURVE ( 'NONE', #51465, #7789, #1342, .T. ) ;
#33337 = CARTESIAN_POINT ( 'NONE',  ( 2.282803330402979114, 43.74200375098541116, -17.12115694997745052 ) ) ;
#33338 =( BOUNDED_SURFACE ( )  B_SPLINE_SURFACE ( 3, 1, ( 
 ( #17375, #3249 ),
 ( #60885, #7966 ),
 ( #37121, #7640 ),
 ( #41819, #32716 ) ),
 .UNSPECIFIED., .F., .F., .F. ) 
 B_SPLINE_SURFACE_WITH_KNOTS ( ( 4, 4 ),
 ( 2, 2 ),
 ( 0.000000000000000000, 1.000000000000000000 ),
 ( 0.000000000000000000, 1.000000000000000000 ),
 .UNSPECIFIED. ) 
 GEOMETRIC_REPRESENTATION_ITEM ( )  RATIONAL_B_SPLINE_SURFACE ( (
 ( 1.000000000000000000, 1.000000000000000000),
 ( 0.7211978278499970862, 0.9934217856018976445),
 ( 0.7211978278499970862, 0.9934217856018976445),
 ( 1.000000000000000000, 1.000000000000000000) ) ) 
 REPRESENTATION_ITEM ( '' )  SURFACE ( )  );
#33339 = VECTOR ( 'NONE', #53663, 1000.000000000000114 ) ;
#33340 = VERTEX_POINT ( 'NONE', #53651 ) ;
#33341 = CARTESIAN_POINT ( 'NONE',  ( 4.958415959904820092, -42.01301765298963176, 17.26587100357872373 ) ) ;
#33342 = CARTESIAN_POINT ( 'NONE',  ( -79.49999999999975842, 2.999999999999996891, 1.500000000000000000 ) ) ;
#33343 = CARTESIAN_POINT ( 'NONE',  ( 0.8557997880470606944, 47.37054680076706603, 7.156447707085862753 ) ) ;
#33344 = CIRCLE ( 'NONE', #17320, 0.09999999999999939493 ) ;
#33345 = ORIENTED_EDGE ( 'NONE', *, *, #40204, .T. ) ;
#33346 = CARTESIAN_POINT ( 'NONE',  ( 5.910764540655178756, -19.93482381198522191, -2.665340138569558537 ) ) ;
#33347 = CARTESIAN_POINT ( 'NONE',  ( 4.962356264823603702, 41.96072444189417183, -3.245489512195726789 ) ) ;
#33348 = CARTESIAN_POINT ( 'NONE',  ( 3.660087539127307554, -4.399983418616474573, 47.83637163185230889 ) ) ;
#33349 = VERTEX_POINT ( 'NONE', #11391 ) ;
#33350 = ORIENTED_EDGE ( 'NONE', *, *, #11463, .F. ) ;
#33351 = CARTESIAN_POINT ( 'NONE',  ( 0.2940133293163002537, 19.68859035591863105, 39.47910788473912902 ) ) ;
#33352 = CARTESIAN_POINT ( 'NONE',  ( 0.5980894510889457338, -37.73932204245538458, 29.84264441023714198 ) ) ;
#33353 = CARTESIAN_POINT ( 'NONE',  ( 2.281448460670576939, 43.80196084514306420, -19.56578495220123060 ) ) ;
#33354 = CARTESIAN_POINT ( 'NONE',  ( 0.7048096507298635682, -24.78213711671570607, -41.23648859290917557 ) ) ;
#33355 = LINE ( 'NONE', #42447, #42589 ) ;
#33356 = CARTESIAN_POINT ( 'NONE',  ( 0.9740398440564302929, -42.48528956276141599, 6.011466167923952497 ) ) ;
#33357 = CARTESIAN_POINT ( 'NONE',  ( 0.8551540677456834771, -23.16399837394575911, 41.94570365541195400 ) ) ;
#33358 = CARTESIAN_POINT ( 'NONE',  ( 0.7762777257811898091, 0.8897018348892672401, -47.89627391089018005 ) ) ;
#33359 = CARTESIAN_POINT ( 'NONE',  ( 4.553261556744875094, 42.43205150231973732, 11.36048287389764688 ) ) ;
#33360 = CARTESIAN_POINT ( 'NONE',  ( 5.860006189529234355, -47.30964106197851038, -9.393028332205226150 ) ) ;
#33361 = DIRECTION ( 'NONE',  ( 0.000000000000000000, -1.000000000000000000, 0.000000000000000000 ) ) ;
#33362 = DIRECTION ( 'NONE',  ( -1.000000000000000000, -0.000000000000000000, -0.000000000000000000 ) ) ;
#33363 = ORIENTED_EDGE ( 'NONE', *, *, #39926, .T. ) ;
#33364 = CARTESIAN_POINT ( 'NONE',  ( 5.960221823109900008, -10.26751639438380259, 17.77295928189537833 ) ) ;
#33365 = CARTESIAN_POINT ( 'NONE',  ( 0.1073791018717578927, -33.91564619577789585, -26.63563652260155123 ) ) ;
#33366 = CARTESIAN_POINT ( 'NONE',  ( 0.5980894510889448457, 29.84264441023778502, -37.73932204245488720 ) ) ;
#33367 = CARTESIAN_POINT ( 'NONE',  ( -2.601141883200662974, -10.40580972892359490, 10.70114719807309811 ) ) ;
#33368 = AXIS2_PLACEMENT_3D ( 'NONE', #13792, #32896, #28170 ) ;
#33369 = CARTESIAN_POINT ( 'NONE',  ( 0.1073791018717578927, 42.68962945260945929, 6.109314776652849943 ) ) ;
#33370 = ITEM_DEFINED_TRANSFORMATION ( 'NONE', 'NONE', #47920,  #14677 ) ;
#33371 = CARTESIAN_POINT ( 'NONE',  ( 4.967162193818130511, 0.000000000000000000, 0.000000000000000000 ) ) ;
#33372 = DIRECTION ( 'NONE',  ( 0.1024043820194936449, -0.6159418278945547609, -0.7811075516170102873 ) ) ;
#33373 = ADVANCED_FACE ( 'NONE', ( #16393 ), #43859, .F. ) ;
#33374 = DIRECTION ( 'NONE',  ( -1.000000000000000000, -0.000000000000000000, -0.000000000000000000 ) ) ;
#33375 = CARTESIAN_POINT ( 'NONE',  ( 2.624215991343608501, 1.411420423866143414, -47.98682984381859740 ) ) ;
#33377 = ORIENTED_EDGE ( 'NONE', *, *, #52735, .F. ) ;
#33376 = CARTESIAN_POINT ( 'NONE',  ( 4.960156602257182357, 3.546989772329889767, 46.28683144126594584 ) ) ;
#33378 = ORIENTED_EDGE ( 'NONE', *, *, #26320, .F. ) ;
#33379 = CARTESIAN_POINT ( 'NONE',  ( 4.553261556744875094, -24.94552653848424129, -36.15605442441715667 ) ) ;
#33380 = CARTESIAN_POINT ( 'NONE',  ( 0.1081432562775997003, 39.67792926340376880, 16.89351827868236100 ) ) ;
#33381 = CARTESIAN_POINT ( 'NONE',  ( 5.981074661064941900, -5.320466518161074632, 19.82308078259081796 ) ) ;
#33382 = ORIENTED_EDGE ( 'NONE', *, *, #59393, .T. ) ;
#33383 = CARTESIAN_POINT ( 'NONE',  ( 4.553261556744875094, 0.000000000000000000, 0.000000000000000000 ) ) ;
#33385 = CARTESIAN_POINT ( 'NONE',  ( 4.549368137175248350, -3.018832571116875751, 42.82045902618767030 ) ) ;
#33384 = CIRCLE ( 'NONE', #6310, 43.92652462719577500 ) ;
#33386 = CARTESIAN_POINT ( 'NONE',  ( 0.5804410086790514622, 45.37396088368723213, -11.86269470150086924 ) ) ;
#33387 = ORIENTED_EDGE ( 'NONE', *, *, #10654, .T. ) ;
#33388 = ORIENTED_EDGE ( 'NONE', *, *, #15430, .F. ) ;
#33389 = CARTESIAN_POINT ( 'NONE',  ( 1.092182651088186240, 33.37207687231951070, 25.35873951264696302 ) ) ;
#33390 = CARTESIAN_POINT ( 'NONE',  ( 0.5807400328401637335, -17.82553128098375339, -44.45848844984462289 ) ) ;
#33391 = CARTESIAN_POINT ( 'NONE',  ( 0.5837799406558226156, 16.76978727848185002, -43.79517991984587155 ) ) ;
#33392 = CARTESIAN_POINT ( 'NONE',  ( 4.956445790443994248, 24.88142650099509723, 39.98065363916922621 ) ) ;
#33393 = CARTESIAN_POINT ( 'NONE',  ( -6.016761891674565099, -7.207804629151182141, -17.41015286184810407 ) ) ;
#33394 = EDGE_CURVE ( 'NONE', #40478, #46978, #34561, .T. ) ;
#33395 = DIRECTION ( 'NONE',  ( -1.000000000000000000, -0.000000000000000000, -0.000000000000000000 ) ) ;
#33396 = EDGE_CURVE ( 'NONE', #37740, #30745, #36450, .T. ) ;
#33397 = ORIENTED_EDGE ( 'NONE', *, *, #16994, .T. ) ;
#33398 = CARTESIAN_POINT ( 'NONE',  ( 0.8751705887134553219, 23.27176129838425922, -42.09020928323351995 ) ) ;
#33399 = CARTESIAN_POINT ( 'NONE',  ( 3.221118495291109163, 43.97607529046792507, 0.9307103248849385446 ) ) ;
#33400 = ORIENTED_EDGE ( 'NONE', *, *, #61234, .F. ) ;
#33401 = DIRECTION ( 'NONE',  ( 1.000000000000000000, 1.836970198721027962E-16, -2.033782021272921061E-31 ) ) ;
#33402 = CARTESIAN_POINT ( 'NONE',  ( 0.8753041380234524160, -45.84117188851829638, -17.59901382919792212 ) ) ;
#33403 = EDGE_CURVE ( 'NONE', #56700, #22536, #40571, .T. ) ;
#33404 = CARTESIAN_POINT ( 'NONE',  ( 2.618530812446115519, 33.67725335819500287, 32.79587467115556620 ) ) ;
#33405 = CARTESIAN_POINT ( 'NONE',  ( 4.960156602257181468, -14.43621227656559824, 44.12083041402459571 ) ) ;
#33406 = AXIS2_PLACEMENT_3D ( 'NONE', #58351, #58662, #39928 ) ;
#33407 = ORIENTED_EDGE ( 'NONE', *, *, #58285, .T. ) ;
#33408 = ORIENTED_EDGE ( 'NONE', *, *, #3414, .T. ) ;
#33409 = CARTESIAN_POINT ( 'NONE',  ( -6.016489644550737204, -11.47450955518498361, 14.94663725562912049 ) ) ;
#33410 = CARTESIAN_POINT ( 'NONE',  ( 0.9757402383260936896, -42.53022961222599463, -5.684842778069664426 ) ) ;
#33411 = CARTESIAN_POINT ( 'NONE',  ( 0.6001305935487422083, 5.760103278697394025, 47.76436356026970032 ) ) ;
#33412 =( BOUNDED_SURFACE ( )  B_SPLINE_SURFACE ( 3, 1, ( 
 ( #40993, #50960 ),
 ( #12462, #17160 ),
 ( #27166, #46291 ),
 ( #55340, #8347 ) ),
 .UNSPECIFIED., .F., .F., .F. ) 
 B_SPLINE_SURFACE_WITH_KNOTS ( ( 4, 4 ),
 ( 2, 2 ),
 ( 0.000000000000000000, 1.000000000000000000 ),
 ( 0.000000000000000000, 1.000000000000000000 ),
 .UNSPECIFIED. ) 
 GEOMETRIC_REPRESENTATION_ITEM ( )  RATIONAL_B_SPLINE_SURFACE ( (
 ( 1.000000000000000000, 1.000000000000000000),
 ( 0.7211978278499968642, 0.9934217856018975334),
 ( 0.7211978278499968642, 0.9934217856018975334),
 ( 1.000000000000000000, 1.000000000000000000) ) ) 
 REPRESENTATION_ITEM ( '' )  SURFACE ( )  );
#33413 = ORIENTED_EDGE ( 'NONE', *, *, #32895, .F. ) ;
#33414 = CARTESIAN_POINT ( 'NONE',  ( 0.8557997880470690211, 41.93815086860257679, 23.15977007032337553 ) ) ;
#33415 = ORIENTED_EDGE ( 'NONE', *, *, #43378, .F. ) ;
#33416 = CARTESIAN_POINT ( 'NONE',  ( 0.5806925824938499181, -44.11884900496058748, -15.89809815106991309 ) ) ;
#33417 = CARTESIAN_POINT ( 'NONE',  ( -2.601141883200662974, 0.9866742854875989455, -14.89368662634427132 ) ) ;
#33418 = ADVANCED_FACE ( 'NONE', ( #25792 ), #50220, .F. ) ;
#33419 = VERTEX_POINT ( 'NONE', #30170 ) ;
#33420 = CARTESIAN_POINT ( 'NONE',  ( 4.960386119450153508, -20.61356833094577823, -38.59426466896047003 ) ) ;
#33421 = CARTESIAN_POINT ( 'NONE',  ( 0.1156495703730067715, -27.40426530387594894, 34.58249841156435878 ) ) ;
#33422 = EDGE_CURVE ( 'NONE', #41654, #46648, #29869, .T. ) ;
#33423 = CARTESIAN_POINT ( 'NONE',  ( 0.9758171775293924544, 26.11633498242675699, -34.04519363167607082 ) ) ;
#33424 = B_SPLINE_CURVE_WITH_KNOTS ( 'NONE', 3,
 ( #31590, #54758, #26263, #35073, #21890, #21265 ),
 .UNSPECIFIED., .F., .F.,
 ( 4, 2, 4 ),
 ( 1.520533924285649780E-16, 0.0002445252820015233640, 0.0004890505640028946143 ),
 .UNSPECIFIED. ) ;
#33425 = AXIS2_PLACEMENT_3D ( 'NONE', #10365, #39197, #43906 ) ;
#33426 = VERTEX_POINT ( 'NONE', #46460 ) ;
#33427 = CARTESIAN_POINT ( 'NONE',  ( 0.5819845079324649229, -18.74766465427192585, -44.07435181061359941 ) ) ;
#33428 = CARTESIAN_POINT ( 'NONE',  ( 0.5806925824938502512, 22.05663578530182889, -41.38510819338409163 ) ) ;
#33429 = CARTESIAN_POINT ( 'NONE',  ( 4.691466044806102076, 44.46979273209130668, 3.249105306918581348 ) ) ;
#33430 = CARTESIAN_POINT ( 'NONE',  ( 0.1129192098497455998, -7.520259262076605999, 43.47870154933683295 ) ) ;
#33431 = CARTESIAN_POINT ( 'NONE',  ( 0.1098349054025746369, 16.69989664087454884, -39.75970464594248455 ) ) ;
#33432 = ORIENTED_EDGE ( 'NONE', *, *, #12606, .T. ) ;
#33433 = DIRECTION ( 'NONE',  ( -1.000000000000000000, -0.000000000000000000, -0.000000000000000000 ) ) ;
#33434 = CARTESIAN_POINT ( 'NONE',  ( 0.7762777257811878107, -24.71864134625259268, 41.03453903600424724 ) ) ;
#33435 = ORIENTED_EDGE ( 'NONE', *, *, #56207, .F. ) ;
#33436 = LINE ( 'NONE', #37846, #9890 ) ;
#33437 = CARTESIAN_POINT ( 'NONE',  ( 5.896782393890504181, -19.93252920631901404, -2.687073932226577533 ) ) ;
#33438 = LINE ( 'NONE', #4577, #36863 ) ;
#33439 = CARTESIAN_POINT ( 'NONE',  ( 1.227938101723756947, 34.55893248994507161, 25.45152231597068848 ) ) ;
#33440 = PLANE ( 'NONE',  #17682 ) ;
#33441 = CARTESIAN_POINT ( 'NONE',  ( 0.2285344041767091994, -40.60359876977020122, 17.25830053159842947 ) ) ;
#33442 = CARTESIAN_POINT ( 'NONE',  ( 0.1119898979215349089, 3.677941539627681333, -43.97083185798182114 ) ) ;
#33443 = B_SPLINE_CURVE_WITH_KNOTS ( 'NONE', 3,
 ( #34626, #6074, #49950, #53691 ),
 .UNSPECIFIED., .F., .F.,
 ( 4, 4 ),
 ( 2.030441771438897580E-17, 0.004444306975806115896 ),
 .UNSPECIFIED. ) ;
#33444 = CARTESIAN_POINT ( 'NONE',  ( -5.340429604346025094, -0.4766853659346310113, -0.7079763230230761151 ) ) ;
#33445 = CARTESIAN_POINT ( 'NONE',  ( 1.088313998177381503, -41.64627086748864571, 10.35171213034677962 ) ) ;
#33446 = B_SPLINE_CURVE_WITH_KNOTS ( 'NONE', 3,
 ( #34464, #52616, #928, #48539, #20059, #44194 ),
 .UNSPECIFIED., .F., .F.,
 ( 4, 2, 4 ),
 ( 3.471140604459641645E-18, 0.0002291459268755719424, 0.0004582918537511404154 ),
 .UNSPECIFIED. ) ;
#33447 = EDGE_CURVE ( 'NONE', #4858, #18906, #59951, .T. ) ;
#33448 = FACE_OUTER_BOUND ( 'NONE', #54287, .T. ) ;
#33449 = CARTESIAN_POINT ( 'NONE',  ( 0.5850706913938534814, -46.21698775168654549, 12.57184842332001296 ) ) ;
#33451 = VERTEX_POINT ( 'NONE', #37067 ) ;
#33450 = DIRECTION ( 'NONE',  ( -1.000000000000000000, -0.000000000000000000, -0.000000000000000000 ) ) ;
#33452 = ORIENTED_EDGE ( 'NONE', *, *, #43108, .F. ) ;
#33453 = FACE_OUTER_BOUND ( 'NONE', #48334, .T. ) ;
#33454 = LINE ( 'NONE', #29048, #33802 ) ;
#33455 = B_SPLINE_CURVE_WITH_KNOTS ( 'NONE', 3,
 ( #19160, #52020, #38270, #4085 ),
 .UNSPECIFIED., .F., .F.,
 ( 4, 4 ),
 ( 2.168404344971008868E-19, 0.004048833967417087357 ),
 .UNSPECIFIED. ) ;
#33456 = VECTOR ( 'NONE', #9862, 1000.000000000000227 ) ;
#33457 = DIRECTION ( 'NONE',  ( 0.000000000000000000, -1.000000000000000000, 0.000000000000000000 ) ) ;
#33458 = CARTESIAN_POINT ( 'NONE',  ( 0.9747592971366234593, 42.49794971112902431, -5.921534893733704230 ) ) ;
#33459 = CARTESIAN_POINT ( 'NONE',  ( 0.1135584504625007790, 10.23925027504970764, -42.91980668572665536 ) ) ;
#33460 = ORIENTED_EDGE ( 'NONE', *, *, #17266, .F. ) ;
#33461 = CYLINDRICAL_SURFACE ( 'NONE', #41335, 2.649999999999992806 ) ;
#33462 = CARTESIAN_POINT ( 'NONE',  ( 5.880360259849752858, -26.69116321728600383, 39.86101557989624666 ) ) ;
#33463 = CARTESIAN_POINT ( 'NONE',  ( 4.967162193818130511, -7.970725651239513709, -42.34252806656601820 ) ) ;
#33464 = EDGE_LOOP ( 'NONE', ( #59173, #95, #55073, #27289 ) ) ;
#33465 = B_SPLINE_CURVE_WITH_KNOTS ( 'NONE', 3,
 ( #59973, #22080, #41207, #50882, #41513, #2020 ),
 .UNSPECIFIED., .F., .F.,
 ( 4, 2, 4 ),
 ( 8.672106141451628927E-17, 0.0002293366620881450661, 0.0004586733241762034501 ),
 .UNSPECIFIED. ) ;
#33466 = VECTOR ( 'NONE', #46590, 1000.000000000000000 ) ;
#33467 = CARTESIAN_POINT ( 'NONE',  ( 0.5830082357119554803, 43.06739319212223194, 18.55887061686358663 ) ) ;
#33468 = CARTESIAN_POINT ( 'NONE',  ( 1.154321485836933947, -20.73950273457868931, 37.57248783354764754 ) ) ;
#33469 = ORIENTED_EDGE ( 'NONE', *, *, #39926, .F. ) ;
#33470 = CARTESIAN_POINT ( 'NONE',  ( -0.2111111111111110827, -9.497654031326126400, -1.199999999999999956 ) ) ;
#33471 = ADVANCED_FACE ( 'NONE', ( #60833 ), #56135, .F. ) ;
#33472 = VERTEX_POINT ( 'NONE', #55207 ) ;
#33473 = CARTESIAN_POINT ( 'NONE',  ( 0.8557997880470690211, -29.88293891557446003, -37.44587306708127983 ) ) ;
#33474 = CARTESIAN_POINT ( 'NONE',  ( 0.5998501479064699549, -47.62484632993692912, 6.798102206413326520 ) ) ;
#33475 = VERTEX_POINT ( 'NONE', #31734 ) ;
#33476 = FACE_BOUND ( 'NONE', #28126, .T. ) ;
#33477 = CARTESIAN_POINT ( 'NONE',  ( 0.5804410086790514622, 10.33990028284824803, -45.74501408892724896 ) ) ;
#33478 = EDGE_CURVE ( 'NONE', #20821, #23099, #54376, .T. ) ;
#33479 = CARTESIAN_POINT ( 'NONE',  ( 3.514385190458181096, -13.03453477240704039, -1.199999999999999956 ) ) ;
#33480 = LINE ( 'NONE', #51319, #50391 ) ;
#33481 = ORIENTED_EDGE ( 'NONE', *, *, #55143, .T. ) ;
#33482 = CARTESIAN_POINT ( 'NONE',  ( 0.6029442701453591180, -7.923526166500598045, -48.46403778315481503 ) ) ;
#33483 = ADVANCED_FACE ( 'NONE', ( #8519 ), #49854, .F. ) ;
#33484 = ORIENTED_EDGE ( 'NONE', *, *, #7494, .F. ) ;
#33485 = CARTESIAN_POINT ( 'NONE',  ( -6.077587904424778920, 17.84644683124317055, -7.231898567702747194 ) ) ;
#33486 = AXIS2_PLACEMENT_3D ( 'NONE', #27499, #18111, #8086 ) ;
#33487 = B_SPLINE_CURVE_WITH_KNOTS ( 'NONE', 3,
 ( #41625, #56308, #56620, #3678 ),
 .UNSPECIFIED., .F., .F.,
 ( 4, 4 ),
 ( 2.120273707634171297E-17, 0.004559932413162188537 ),
 .UNSPECIFIED. ) ;
#33488 = VERTEX_POINT ( 'NONE', #45536 ) ;
#33489 = ORIENTED_EDGE ( 'NONE', *, *, #40009, .T. ) ;
#33490 = CARTESIAN_POINT ( 'NONE',  ( 0.1365634738349438548, 25.76331610226886326, -35.82058295223323796 ) ) ;
#33492 = CARTESIAN_POINT ( 'NONE',  ( 0.9772918015221170318, -37.21531972239668562, 19.27062099960642172 ) ) ;
#33491 = B_SPLINE_CURVE_WITH_KNOTS ( 'NONE', 3,
 ( #59693, #50601, #31194, #60300, #40944, #50912, #12416, #17726, #7365, #45621, #2678, #7682, #22111, #9867, #61233, #56229 ),
 .UNSPECIFIED., .F., .F.,
 ( 4, 3, 3, 3, 3, 4 ),
 ( 1.040890552917501732E-17, 0.0002732102107931913006, 0.0004098135523333824013, 0.0005464168938824995759, 0.0008195847345945435521, 0.001092771384553107867 ),
 .UNSPECIFIED. ) ;
#33493 = CARTESIAN_POINT ( 'NONE',  ( 0.9752132459055858904, 34.18286753639641518, 25.93579301218368371 ) ) ;
#33494 = CARTESIAN_POINT ( 'NONE',  ( 0.8744876279028263033, 48.01195819035220325, 10.25679877483054625 ) ) ;
#33495 = ORIENTED_EDGE ( 'NONE', *, *, #46010, .F. ) ;
#33496 = CARTESIAN_POINT ( 'NONE',  ( 5.896278296736517710, -4.657235598391419096, -19.56622437251140667 ) ) ;
#33497 = DIRECTION ( 'NONE',  ( 1.000000000000000000, 0.000000000000000000, 0.000000000000000000 ) ) ;
#33498 = EDGE_CURVE ( 'NONE', #22273, #15900, #30108, .T. ) ;
#33499 = LINE ( 'NONE', #57562, #48033 ) ;
#33500 = ORIENTED_EDGE ( 'NONE', *, *, #20742, .F. ) ;
#33501 = EDGE_LOOP ( 'NONE', ( #17469, #55611, #18441, #9312 ) ) ;
#33502 = CARTESIAN_POINT ( 'NONE',  ( 1.227938101723748288, 17.20315230597897482, -39.32113113558949635 ) ) ;
#33503 = FACE_OUTER_BOUND ( 'NONE', #17073, .T. ) ;
#33504 = CARTESIAN_POINT ( 'NONE',  ( 0.1103744047535531458, 30.46616790811179953, 30.52096488484638215 ) ) ;
#33505 = LINE ( 'NONE', #13166, #14596 ) ;
#33506 = FACE_OUTER_BOUND ( 'NONE', #20555, .T. ) ;
#33507 = ORIENTED_EDGE ( 'NONE', *, *, #61491, .T. ) ;
#33508 = ORIENTED_EDGE ( 'NONE', *, *, #11314, .F. ) ;
#33509 = AXIS2_PLACEMENT_3D ( 'NONE', #37541, #43476, #61911 ) ;
#33510 = CARTESIAN_POINT ( 'NONE',  ( -6.077587904424778920, 18.62786028128800098, -4.878405757493267103 ) ) ;
#33511 = CARTESIAN_POINT ( 'NONE',  ( 0.9783242366443567484, -41.12142888775412075, 8.084712514115880211 ) ) ;
#33512 = CONICAL_SURFACE ( 'NONE', #12498, 42.92674063221959813, 1.485477209440487556 ) ;
#33513 = CARTESIAN_POINT ( 'NONE',  ( 4.975610109902397937, 0.000000000000000000, 0.000000000000000000 ) ) ;
#33514 = CARTESIAN_POINT ( 'NONE',  ( 0.8744876279028263033, 44.61213666265857825, -20.49651952824592982 ) ) ;
#33515 = CARTESIAN_POINT ( 'NONE',  ( 0.7948884756798504370, 37.94263149402783597, -31.16176118111038917 ) ) ;
#33516 = CARTESIAN_POINT ( 'NONE',  ( 0.5998501479064699549, 0.5236536531308225717, 48.10473956285920138 ) ) ;
#33517 = ORIENTED_EDGE ( 'NONE', *, *, #54918, .F. ) ;
#33518 = CARTESIAN_POINT ( 'NONE',  ( 0.1152339509894530906, 20.21078498592564898, -39.22329487317357888 ) ) ;
#33519 = CARTESIAN_POINT ( 'NONE',  ( 4.962356264823601926, -38.57439820587641321, 16.83007429920694875 ) ) ;
#33520 = CARTESIAN_POINT ( 'NONE',  ( 4.322998006666165516, 25.80712523194275221, -40.45864630878492818 ) ) ;
#33521 = CARTESIAN_POINT ( 'NONE',  ( 5.895596859100789899, 20.06821053248683029, 1.339816866691926567 ) ) ;
#33522 = CARTESIAN_POINT ( 'NONE',  ( 4.975610109902397937, 2.142807115709817189, -48.86571174967818365 ) ) ;
#33523 = EDGE_CURVE ( 'NONE', #22531, #50798, #18934, .T. ) ;
#33524 = CARTESIAN_POINT ( 'NONE',  ( 4.335381028904201628, -17.86707742387175912, -45.61276566920401621 ) ) ;
#33525 = CARTESIAN_POINT ( 'NONE',  ( 0.5782707292762442330, -7.086273146447505944, -46.36292793387357847 ) ) ;
#33526 = EDGE_CURVE ( 'NONE', #12115, #3984, #15148, .T. ) ;
#33527 = VECTOR ( 'NONE', #15575, 1000.000000000000000 ) ;
#33528 =( BOUNDED_SURFACE ( )  B_SPLINE_SURFACE ( 3, 1, ( 
 ( #5771, #25518 ),
 ( #53398, #34945 ),
 ( #44060, #54008 ),
 ( #39040, #49025 ) ),
 .UNSPECIFIED., .F., .F., .F. ) 
 B_SPLINE_SURFACE_WITH_KNOTS ( ( 4, 4 ),
 ( 2, 2 ),
 ( 0.000000000000000000, 1.000000000000000000 ),
 ( 0.000000000000000000, 1.000000000000000000 ),
 .UNSPECIFIED. ) 
 GEOMETRIC_REPRESENTATION_ITEM ( )  RATIONAL_B_SPLINE_SURFACE ( (
 ( 1.000000000000000000, 1.000000000000000000),
 ( 0.7223157951917480446, 0.9931996967497186413),
 ( 0.7223157951917480446, 0.9931996967497186413),
 ( 1.000000000000000000, 1.000000000000000000) ) ) 
 REPRESENTATION_ITEM ( '' )  SURFACE ( )  );
#33529 = ORIENTED_EDGE ( 'NONE', *, *, #32835, .F. ) ;
#33530 = EDGE_CURVE ( 'NONE', #19827, #51524, #59283, .T. ) ;
#33531 = CARTESIAN_POINT ( 'NONE',  ( 3.783198216974388739, -39.06945274417380176, -18.05208553945188754 ) ) ;
#33532 = CARTESIAN_POINT ( 'NONE',  ( 0.3622758884714600280, 4.808133778521302304, 42.84426538328732903 ) ) ;
#33533 = CARTESIAN_POINT ( 'NONE',  ( 0.5809828226811544205, 17.82437196699742188, -44.45562576850583270 ) ) ;
#33534 = CARTESIAN_POINT ( 'NONE',  ( 0.8560838555295158248, -14.76796170096741534, 44.52280473286123907 ) ) ;
#33535 = CARTESIAN_POINT ( 'NONE',  ( 5.200000000000002842, 0.000000000000000000, 0.000000000000000000 ) ) ;
#33536 = ORIENTED_EDGE ( 'NONE', *, *, #45283, .T. ) ;
#33537 = CARTESIAN_POINT ( 'NONE',  ( 0.9747592971366226822, -36.99691261380223750, 21.73404615330606759 ) ) ;
#33538 = DIRECTION ( 'NONE',  ( 4.437342591868191405E-31, -1.000000000000000000, -4.551914400963141816E-15 ) ) ;
#33539 = B_SPLINE_CURVE_WITH_KNOTS ( 'NONE', 3,
 ( #33290, #43313, #52360, #9453, #19492, #53285 ),
 .UNSPECIFIED., .F., .F.,
 ( 4, 2, 4 ),
 ( 1.007374941650268034E-17, 0.0002448709889506589456, 0.0004897419779013078081 ),
 .UNSPECIFIED. ) ;
#33540 = ORIENTED_EDGE ( 'NONE', *, *, #29958, .T. ) ;
#33541 = LINE ( 'NONE', #20062, #13072 ) ;
#33542 = VECTOR ( 'NONE', #27169, 1000.000000000000114 ) ;
#33543 = CARTESIAN_POINT ( 'NONE',  ( 5.960221823109900008, -2.673723662181196392, -20.35070456576733733 ) ) ;
#33544 = EDGE_CURVE ( 'NONE', #25119, #46714, #10413, .T. ) ;
#33545 = VERTEX_POINT ( 'NONE', #343 ) ;
#33546 = CARTESIAN_POINT ( 'NONE',  ( 4.962356264823609031, -33.29728444345293781, 25.73958909062332268 ) ) ;
#33547 = VECTOR ( 'NONE', #4065, 1000.000000000000000 ) ;
#33548 = ORIENTED_EDGE ( 'NONE', *, *, #38011, .F. ) ;
#33549 = CARTESIAN_POINT ( 'NONE',  ( 4.975610109902397937, 45.55079628452109830, 17.82061629079735354 ) ) ;
#33551 = VERTEX_POINT ( 'NONE', #9146 ) ;
#33550 = EDGE_CURVE ( 'NONE', #6988, #33784, #21128, .T. ) ;
#33552 = CARTESIAN_POINT ( 'NONE',  ( 0.2230388203127596503, -42.84312106681679921, -4.873876086128098528 ) ) ;
#33553 = FACE_OUTER_BOUND ( 'NONE', #59576, .T. ) ;
#33554 = VERTEX_POINT ( 'NONE', #14182 ) ;
#33555 = CARTESIAN_POINT ( 'NONE',  ( 1.231276596079887264, 38.91607545535247681, 15.58254928345742840 ) ) ;
#33556 = CIRCLE ( 'NONE', #40537, 10.00000000000000000 ) ;
#33557 = ORIENTED_EDGE ( 'NONE', *, *, #52043, .T. ) ;
#33558 = CARTESIAN_POINT ( 'NONE',  ( 4.975610109902397937, -37.61482235126130291, -31.26618855282533360 ) ) ;
#33559 = ADVANCED_FACE ( 'NONE', ( #52358 ), #42383, .T. ) ;
#33560 = CARTESIAN_POINT ( 'NONE',  ( 1.227938101723756947, 42.91134962331487657, -0.8460948827226678626 ) ) ;
#33561 = ORIENTED_EDGE ( 'NONE', *, *, #61613, .T. ) ;
#33562 = CARTESIAN_POINT ( 'NONE',  ( 5.895881250540457863, -19.93402233083542185, -2.676272654655299288 ) ) ;
#33563 = CARTESIAN_POINT ( 'NONE',  ( 0.7246131072078572100, 5.464103862700868675, 47.79072675905346301 ) ) ;
#33564 = CARTESIAN_POINT ( 'NONE',  ( 0.1156867017252034557, -22.76669660009247309, -37.79709424273940499 ) ) ;
#33565 = ORIENTED_EDGE ( 'NONE', *, *, #44629, .F. ) ;
#33566 = CARTESIAN_POINT ( 'NONE',  ( 0.5806925824938499181, 23.01490136172973067, -40.85996423950240342 ) ) ;
#33567 = EDGE_CURVE ( 'NONE', #30011, #4680, #61745, .T. ) ;
#33568 = CARTESIAN_POINT ( 'NONE',  ( -6.078726893082806448, -1.845620846545631188, 19.16736092839899186 ) ) ;
#33569 = ORIENTED_EDGE ( 'NONE', *, *, #35453, .F. ) ;
#33570 = CARTESIAN_POINT ( 'NONE',  ( 0.5809828226811544205, 47.55412398569205834, 5.711058609465488267 ) ) ;
#33571 = EDGE_LOOP ( 'NONE', ( #53076, #28765, #16663, #53904 ) ) ;
#33572 = CARTESIAN_POINT ( 'NONE',  ( 0.9754292589017192761, 25.32584946409135540, 33.39054979807107770 ) ) ;
#33573 = CARTESIAN_POINT ( 'NONE',  ( 0.9762797500689124330, 40.28286501695585997, -11.55922018180369548 ) ) ;
#33574 = ORIENTED_EDGE ( 'NONE', *, *, #31967, .F. ) ;
#33575 = CARTESIAN_POINT ( 'NONE',  ( 0.5837157313716032636, 4.603500525675801924, 46.66952802945544221 ) ) ;
#33576 = CARTESIAN_POINT ( 'NONE',  ( 0.1147471544378677183, 24.98894974753881115, -36.36625604854348381 ) ) ;
#33577 = FACE_OUTER_BOUND ( 'NONE', #10734, .T. ) ;
#33578 = CARTESIAN_POINT ( 'NONE',  ( 0.9780106845699478857, -22.28528844046299184, -35.49221274562640360 ) ) ;
#33579 = VERTEX_POINT ( 'NONE', #38303 ) ;
#33580 = CARTESIAN_POINT ( 'NONE',  ( 0.1158516988532803521, -40.88093175327997386, 16.60396271425774728 ) ) ;
#33581 = CARTESIAN_POINT ( 'NONE',  ( 0.5848930533535030563, 36.91687493861116565, 28.92088219875909516 ) ) ;
#33582 = CARTESIAN_POINT ( 'NONE',  ( -6.016761891674564211, -18.84319130225482297, 0.003433883959717882409 ) ) ;
#33584 = PLANE ( 'NONE',  #16928 ) ;
#33583 =( BOUNDED_SURFACE ( )  B_SPLINE_SURFACE ( 3, 1, ( 
 ( #38732, #5164 ),
 ( #14920, #43746 ),
 ( #39342, #57786 ),
 ( #61864, #4856 ) ),
 .UNSPECIFIED., .F., .F., .F. ) 
 B_SPLINE_SURFACE_WITH_KNOTS ( ( 4, 4 ),
 ( 2, 2 ),
 ( 0.000000000000000000, 1.000000000000000000 ),
 ( 0.000000000000000000, 1.000000000000000000 ),
 .UNSPECIFIED. ) 
 GEOMETRIC_REPRESENTATION_ITEM ( )  RATIONAL_B_SPLINE_SURFACE ( (
 ( 1.000000000000000000, 1.000000000000000000),
 ( 0.9953040768229013402, 0.8617119497784988535),
 ( 0.9953040768229013402, 0.8617119497784988535),
 ( 1.000000000000000000, 1.000000000000000000) ) ) 
 REPRESENTATION_ITEM ( '' )  SURFACE ( )  );
#33585 = CARTESIAN_POINT ( 'NONE',  ( -6.001507490154111224, 14.94036486426013433, 11.48377994779706235 ) ) ;
#33586 = DIRECTION ( 'NONE',  ( 1.000000000000000000, 0.000000000000000000, 0.000000000000000000 ) ) ;
#33587 = EDGE_CURVE ( 'NONE', #43871, #40367, #4416, .T. ) ;
#33588 = AXIS2_PLACEMENT_3D ( 'NONE', #28062, #14290, #19920 ) ;
#33589 = CARTESIAN_POINT ( 'NONE',  ( 5.974727161628367256, -0.01551142186635440928, -20.52494643607030156 ) ) ;
#33590 = CARTESIAN_POINT ( 'NONE',  ( 0.3622758884714730732, -36.91764744403337062, 22.26738722580103413 ) ) ;
#33591 = EDGE_CURVE ( 'NONE', #1548, #42575, #4378, .T. ) ;
#33592 = CARTESIAN_POINT ( 'NONE',  ( 2.643462169533600914, 42.27470921730940034, -22.81120928486451405 ) ) ;
#33593 = AXIS2_PLACEMENT_3D ( 'NONE', #12244, #46074, #16943 ) ;
#33594 = CARTESIAN_POINT ( 'NONE',  ( 0.1098349054025746091, -21.74670956129786603, 37.23978094195813782 ) ) ;
#33595 = CARTESIAN_POINT ( 'NONE',  ( 4.975610109902397937, -41.30423662854469313, 26.19941685746003301 ) ) ;
#33596 = CARTESIAN_POINT ( 'NONE',  ( 4.962356264823608143, -36.43094049105388166, 21.07183363638861096 ) ) ;
#33598 = ADVANCED_FACE ( 'NONE', ( #27956 ), #22389, .T. ) ;
#33597 = CARTESIAN_POINT ( 'NONE',  ( 0.9268187852002115479, -22.00118040109542505, 38.20605179637225746 ) ) ;
#33599 =( BOUNDED_SURFACE ( )  B_SPLINE_SURFACE ( 3, 1, ( 
 ( #12335, #55835 ),
 ( #12957, #21099 ),
 ( #60218, #21407 ),
 ( #45857, #50828 ) ),
 .UNSPECIFIED., .F., .F., .F. ) 
 B_SPLINE_SURFACE_WITH_KNOTS ( ( 4, 4 ),
 ( 2, 2 ),
 ( 0.000000000000000000, 1.000000000000000000 ),
 ( 0.000000000000000000, 1.000000000000000000 ),
 .UNSPECIFIED. ) 
 GEOMETRIC_REPRESENTATION_ITEM ( )  RATIONAL_B_SPLINE_SURFACE ( (
 ( 1.000000000000000000, 1.000000000000000000),
 ( 0.7269869731126821222, 0.9931720237060910339),
 ( 0.7269869731126821222, 0.9931720237060910339),
 ( 1.000000000000000000, 1.000000000000000000) ) ) 
 REPRESENTATION_ITEM ( '' )  SURFACE ( )  );
#33600 = FACE_OUTER_BOUND ( 'NONE', #5079, .T. ) ;
#33601 = EDGE_CURVE ( 'NONE', #21910, #1315, #42141, .T. ) ;
#33602 = CARTESIAN_POINT ( 'NONE',  ( 5.896278296736517710, -4.657235598391687326, 19.56622437251134627 ) ) ;
#33603 = B_SPLINE_CURVE_WITH_KNOTS ( 'NONE', 3,
 ( #31737, #25794, #55210, #45540 ),
 .UNSPECIFIED., .F., .F.,
 ( 4, 4 ),
 ( 0.000000000000000000, 0.004444103432399266161 ),
 .UNSPECIFIED. ) ;
#33604 = ORIENTED_EDGE ( 'NONE', *, *, #17583, .F. ) ;
#33605 = DIRECTION ( 'NONE',  ( 0.09835009131224552170, -0.4908642831975423837, 0.8656670924898530739 ) ) ;
#33606 = CARTESIAN_POINT ( 'NONE',  ( 0.8744876279028263033, 5.599149760998344050, -48.77498920895221346 ) ) ;
#33607 = DIRECTION ( 'NONE',  ( 0.07439287786467665975, 0.9597484305373172875, 0.2708295585865166943 ) ) ;
#33608 = ORIENTED_EDGE ( 'NONE', *, *, #18601, .T. ) ;
#33609 = CARTESIAN_POINT ( 'NONE',  ( 0.9741495583595187746, 5.208308905148107293, 42.59115242362807408 ) ) ;
#33610 = CARTESIAN_POINT ( 'NONE',  ( 4.060580049360325461, 27.00639131667134052, 34.67163858847787594 ) ) ;
#33611 = ORIENTED_EDGE ( 'NONE', *, *, #5955, .T. ) ;
#33612 = ORIENTED_EDGE ( 'NONE', *, *, #50202, .F. ) ;
#33613 = ADVANCED_FACE ( 'NONE', ( #19489 ), #39453, .F. ) ;
#33614 = DIRECTION ( 'NONE',  ( 1.000000000000000000, 1.836909530733573776E-16, 0.000000000000000000 ) ) ;
#33615 = EDGE_CURVE ( 'NONE', #52459, #59097, #28871, .T. ) ;
#33616 = VERTEX_POINT ( 'NONE', #19189 ) ;
#33617 = CARTESIAN_POINT ( 'NONE',  ( 4.967162193818130511, 0.000000000000000000, 0.000000000000000000 ) ) ;
#33618 = ORIENTED_EDGE ( 'NONE', *, *, #61572, .T. ) ;
#33619 = ORIENTED_EDGE ( 'NONE', *, *, #41591, .T. ) ;
#33620 = CARTESIAN_POINT ( 'NONE',  ( -6.079354080745853928, -17.34853647870684057, 8.355910321152332898 ) ) ;
#33621 = ORIENTED_EDGE ( 'NONE', *, *, #29828, .F. ) ;
#33622 = CARTESIAN_POINT ( 'NONE',  ( 0.5809828226811617480, -41.20389530892290253, -24.41822904836968178 ) ) ;
#33623 = CARTESIAN_POINT ( 'NONE',  ( 4.549368137175248350, -32.41327393324159800, 28.14399996863441800 ) ) ;
#33624 = DIRECTION ( 'NONE',  ( -1.000000000000000000, -0.000000000000000000, -0.000000000000000000 ) ) ;
#33625 = ORIENTED_EDGE ( 'NONE', *, *, #46090, .T. ) ;
#33626 = CARTESIAN_POINT ( 'NONE',  ( 0.7954190325252789018, -44.76287681188620837, -17.60078418394979138 ) ) ;
#33627 = EDGE_CURVE ( 'NONE', #44423, #43089, #16703, .T. ) ;
#33628 = CARTESIAN_POINT ( 'NONE',  ( 3.678834586032788234, 48.39168880843644160, -7.540346404231043742 ) ) ;
#33629 = VERTEX_POINT ( 'NONE', #33905 ) ;
#33630 = ORIENTED_EDGE ( 'NONE', *, *, #59977, .T. ) ;
#33631 = CARTESIAN_POINT ( 'NONE',  ( 4.975610109902397937, -47.89734868211972696, -9.914302615979444511 ) ) ;
#33632 = AXIS2_PLACEMENT_3D ( 'NONE', #14297, #28682, #38118 ) ;
#33633 = ORIENTED_EDGE ( 'NONE', *, *, #20376, .T. ) ;
#33634 = CARTESIAN_POINT ( 'NONE',  ( 2.533389852662419894, 34.52020495688822166, 27.30944857495383005 ) ) ;
#33635 = DIRECTION ( 'NONE',  ( 0.07836865515943411409, -0.6131273243286340380, 0.7860872967108117892 ) ) ;
#33636 = CARTESIAN_POINT ( 'NONE',  ( 0.9754642270333683252, -0.1757168848622158996, 42.90808635884411615 ) ) ;
#33637 = CARTESIAN_POINT ( 'NONE',  ( 0.7764146366350251904, 39.89513471720565718, -24.66614480548544819 ) ) ;
#33638 = EDGE_CURVE ( 'NONE', #11233, #33142, #27129, .T. ) ;
#33639 = B_SPLINE_CURVE_WITH_KNOTS ( 'NONE', 3,
 ( #35908, #49670, #6725, #54664 ),
 .UNSPECIFIED., .F., .F.,
 ( 4, 4 ),
 ( 2.303004670188525934E-17, 0.004564976165746187711 ),
 .UNSPECIFIED. ) ;
#33640 = ORIENTED_EDGE ( 'NONE', *, *, #53116, .T. ) ;
#33641 = CARTESIAN_POINT ( 'NONE',  ( 0.1147471544378676767, -1.724555973322355662, -44.09056696355949612 ) ) ;
#33642 = CARTESIAN_POINT ( 'NONE',  ( 4.962356264823608143, -15.53171314616189846, 39.11523340857994668 ) ) ;
#33643 = EDGE_CURVE ( 'NONE', #22365, #34842, #56749, .T. ) ;
#33644 = CARTESIAN_POINT ( 'NONE',  ( 2.618530812446111078, -24.09540528802407522, -40.36258457041695635 ) ) ;
#33645 = EDGE_LOOP ( 'NONE', ( #41932, #43639, #40752, #9186 ) ) ;
#33646 = CARTESIAN_POINT ( 'NONE',  ( 0.3622758884714600280, -41.85013935980108357, 10.35929834645850001 ) ) ;
#33647 = CARTESIAN_POINT ( 'NONE',  ( 3.678834586032788234, -29.06827489512433615, -39.41633879814102670 ) ) ;
#33648 = AXIS2_PLACEMENT_3D ( 'NONE', #11016, #48904, #24480 ) ;
#33649 = ORIENTED_EDGE ( 'NONE', *, *, #52100, .T. ) ;
#33650 = ORIENTED_EDGE ( 'NONE', *, *, #51022, .F. ) ;
#33651 = CARTESIAN_POINT ( 'NONE',  ( 5.896782393890504181, -15.78060201202832324, 12.46991126736593003 ) ) ;
#33652 = CARTESIAN_POINT ( 'NONE',  ( 0.3622758884714600280, 37.74294673546586409, -20.83792692158932525 ) ) ;
#33653 = DIRECTION ( 'NONE',  ( -1.000000000000000000, -0.000000000000000000, -0.000000000000000000 ) ) ;
#33654 = LINE ( 'NONE', #28020, #14803 ) ;
#33655 = CARTESIAN_POINT ( 'NONE',  ( 5.895596859100789899, 19.00119700155552493, 6.594141014610245932 ) ) ;
#33656 = CARTESIAN_POINT ( 'NONE',  ( 0.1145239942831223490, -17.56161902965139276, -40.47882184256428673 ) ) ;
#33657 = B_SPLINE_CURVE_WITH_KNOTS ( 'NONE', 3,
 ( #20734, #31059, #29813, #49533 ),
 .UNSPECIFIED., .F., .F.,
 ( 4, 4 ),
 ( 0.000000000000000000, 0.005014147105413699519 ),
 .UNSPECIFIED. ) ;
#33658 = CARTESIAN_POINT ( 'NONE',  ( 0.9730545539215883499, -21.89037132892409687, -36.90443313492354349 ) ) ;
#33659 = CARTESIAN_POINT ( 'NONE',  ( 2.301529144917016101, -30.25186323939247757, -37.31001381748723134 ) ) ;
#33660 = FACE_OUTER_BOUND ( 'NONE', #29149, .T. ) ;
#33661 = CARTESIAN_POINT ( 'NONE',  ( 0.8554163680231708922, -44.01281378489781559, -16.25046755781901098 ) ) ;
#33662 = CARTESIAN_POINT ( 'NONE',  ( 0.6001305935487315502, -44.24520387813816313, -18.89378601236050059 ) ) ;
#33663 = ORIENTED_EDGE ( 'NONE', *, *, #7690, .T. ) ;
#33664 = CARTESIAN_POINT ( 'NONE',  ( 3.407937589446174087, -6.447869442558080699, -12.08659953757615568 ) ) ;
#33665 = CARTESIAN_POINT ( 'NONE',  ( 0.6029443449137436017, 41.13259312748885321, 26.82628040917691337 ) ) ;
#33666 = ADVANCED_FACE ( 'NONE', ( #13874 ), #56618, .F. ) ;
#33667 = CARTESIAN_POINT ( 'NONE',  ( 0.6064782688330866423, -45.81047758530520753, -10.03666228509350411 ) ) ;
#33668 = DIRECTION ( 'NONE',  ( 0.000000000000000000, 0.000000000000000000, -1.000000000000000000 ) ) ;
#33669 = CARTESIAN_POINT ( 'NONE',  ( 0.6017666602106488405, -23.75081624637651245, 41.83584962818275699 ) ) ;
#33670 = CARTESIAN_POINT ( 'NONE',  ( 0.5827357941260215002, -41.29633147056626541, 24.26189667804985461 ) ) ;
#33671 = CONTEXT_DEPENDENT_SHAPE_REPRESENTATION ( #19992, #55266 ) ;
#33673 = EDGE_CURVE ( 'NONE', #27525, #10594, #43938, .T. ) ;
#33672 = CARTESIAN_POINT ( 'NONE',  ( 0.5806925824938499181, -25.69265091980040339, 39.23149310256803801 ) ) ;
#33674 = CARTESIAN_POINT ( 'NONE',  ( 0.6016118706126977189, 48.26733626538113242, -9.045181293293902414 ) ) ;
#33675 = CARTESIAN_POINT ( 'NONE',  ( 0.6029443199889047422, -30.61794975149917519, 38.39373379692413124 ) ) ;
#33676 = AXIS2_PLACEMENT_3D ( 'NONE', #5625, #10994, #20384 ) ;
#33677 = EDGE_CURVE ( 'NONE', #4311, #59715, #44348, .T. ) ;
#33679 =( BOUNDED_SURFACE ( )  B_SPLINE_SURFACE ( 3, 1, ( 
 ( #18119, #27204 ),
 ( #17197, #3373 ),
 ( #36317, #61012 ),
 ( #26899, #60383 ) ),
 .UNSPECIFIED., .F., .F., .F. ) 
 B_SPLINE_SURFACE_WITH_KNOTS ( ( 4, 4 ),
 ( 2, 2 ),
 ( 0.000000000000000000, 1.000000000000000000 ),
 ( 0.000000000000000000, 1.000000000000000000 ),
 .UNSPECIFIED. ) 
 GEOMETRIC_REPRESENTATION_ITEM ( )  RATIONAL_B_SPLINE_SURFACE ( (
 ( 1.000000000000000000, 1.000000000000000000),
 ( 0.7223157951917480446, 0.9931996967497186413),
 ( 0.7223157951917480446, 0.9931996967497186413),
 ( 1.000000000000000000, 1.000000000000000000) ) ) 
 REPRESENTATION_ITEM ( '' )  SURFACE ( )  );
#33678 = CARTESIAN_POINT ( 'NONE',  ( 0.3622758884714600280, -36.91764744403305087, -22.26738722580154217 ) ) ;
#33680 = CARTESIAN_POINT ( 'NONE',  ( -6.016761891674565099, 4.873659902332367011, 18.20201388312097279 ) ) ;
#33681 = EDGE_CURVE ( 'NONE', #40146, #16747, #55419, .T. ) ;
#33683 = ORIENTED_EDGE ( 'NONE', *, *, #40789, .T. ) ;
#33682 = CARTESIAN_POINT ( 'NONE',  ( 2.299652685299201416, -18.66303054524520633, -45.34283863770990308 ) ) ;
#33684 = VERTEX_POINT ( 'NONE', #59216 ) ;
#33685 = CONICAL_SURFACE ( 'NONE', #42708, 43.92652462719577500, 1.486293639869522343 ) ;
#33686 = CARTESIAN_POINT ( 'NONE',  ( 5.901463166500146684, 19.70672075163023251, -4.020326797401311048 ) ) ;
#33687 = CARTESIAN_POINT ( 'NONE',  ( 0.8557997880470690211, -38.55640757422419540, -28.43566216845010075 ) ) ;
#33688 = AXIS2_PLACEMENT_3D ( 'NONE', #53413, #48726, #34640 ) ;
#33689 = EDGE_CURVE ( 'NONE', #61163, #37784, #26405, .T. ) ;
#33690 = DIRECTION ( 'NONE',  ( 1.000000000000000000, 0.000000000000000000, 0.000000000000000000 ) ) ;
#33691 = ORIENTED_EDGE ( 'NONE', *, *, #34446, .T. ) ;
#33692 = CARTESIAN_POINT ( 'NONE',  ( 0.5835871038041865466, 22.41749763088149905, 41.19090012212553376 ) ) ;
#33693 = CARTESIAN_POINT ( 'NONE',  ( 0.000000000000000000, 0.000000000000000000, -5.600000000000000533 ) ) ;
#33694 = CARTESIAN_POINT ( 'NONE',  ( 0.7048096507298635682, -44.76417498422303964, -17.62869676200394053 ) ) ;
#33695 = B_SPLINE_CURVE_WITH_KNOTS ( 'NONE', 3,
 ( #765, #35227, #59005, #28973 ),
 .UNSPECIFIED., .F., .F.,
 ( 4, 4 ),
 ( 1.301042606982605321E-18, 0.004048833967417087357 ),
 .UNSPECIFIED. ) ;
#33696 = VERTEX_POINT ( 'NONE', #19803 ) ;
#33697 = ORIENTED_EDGE ( 'NONE', *, *, #12914, .T. ) ;
#33698 = EDGE_CURVE ( 'NONE', #52962, #37659, #49520, .T. ) ;
#33699 = CARTESIAN_POINT ( 'NONE',  ( 0.1073791018717578927, 16.95003405440313315, -39.65380858626198091 ) ) ;
#33700 = CIRCLE ( 'NONE', #35715, 42.88844316795388778 ) ;
#33701 = CARTESIAN_POINT ( 'NONE',  ( 0.6846871229502932144, -17.53234844287709038, -44.58493949244024890 ) ) ;
#33702 = CARTESIAN_POINT ( 'NONE',  ( 0.3676999524040366896, -44.10520818713899871, 0.8253448321555690859 ) ) ;
#33703 =( BOUNDED_SURFACE ( )  B_SPLINE_SURFACE ( 3, 1, ( 
 ( #61194, #56801 ),
 ( #3556, #22377 ),
 ( #51797, #46204 ),
 ( #22689, #50875 ) ),
 .UNSPECIFIED., .F., .F., .F. ) 
 B_SPLINE_SURFACE_WITH_KNOTS ( ( 4, 4 ),
 ( 2, 2 ),
 ( 0.000000000000000000, 1.000000000000000000 ),
 ( 0.000000000000000000, 1.000000000000000000 ),
 .UNSPECIFIED. ) 
 GEOMETRIC_REPRESENTATION_ITEM ( )  RATIONAL_B_SPLINE_SURFACE ( (
 ( 1.000000000000000000, 1.000000000000000000),
 ( 0.7211978278499970862, 0.9934217856018976445),
 ( 0.7211978278499970862, 0.9934217856018976445),
 ( 1.000000000000000000, 1.000000000000000000) ) ) 
 REPRESENTATION_ITEM ( '' )  SURFACE ( )  );
#33704 = DIRECTION ( 'NONE',  ( 0.000000000000000000, 0.000000000000000000, 1.000000000000000000 ) ) ;
#33705 = CARTESIAN_POINT ( 'NONE',  ( -6.016104459813374383, -7.206059014949953934, -17.41090761020844013 ) ) ;
#33706 = CARTESIAN_POINT ( 'NONE',  ( 0.5832367798473380160, 38.16362489683130121, -28.94059862654955495 ) ) ;
#33707 = ORIENTED_EDGE ( 'NONE', *, *, #39386, .T. ) ;
#33708 = VERTEX_POINT ( 'NONE', #10396 ) ;
#33709 = CARTESIAN_POINT ( 'NONE',  ( 0.5809828226811560858, -11.86925843957200222, 46.40184912890835278 ) ) ;
#33710 = CARTESIAN_POINT ( 'NONE',  ( -6.077587904424778920, 19.09876248768967955, 2.456276212633274003 ) ) ;
#33711 = ORIENTED_EDGE ( 'NONE', *, *, #55771, .F. ) ;
#33712 = CARTESIAN_POINT ( 'NONE',  ( 0.1158816050234199174, 41.87450319480698369, -13.90927832395560593 ) ) ;
#33713 = LINE ( 'NONE', #9893, #43661 ) ;
#33714 = CARTESIAN_POINT ( 'NONE',  ( 0.5997462898726536595, -39.66574928371259290, 28.95133786038155321 ) ) ;
#33715 = CARTESIAN_POINT ( 'NONE',  ( 0.1145239942831223490, -40.77578764147322943, -16.86062344405307201 ) ) ;
#33716 = ORIENTED_EDGE ( 'NONE', *, *, #5786, .F. ) ;
#33717 = ORIENTED_EDGE ( 'NONE', *, *, #11123, .F. ) ;
#33718 = CARTESIAN_POINT ( 'NONE',  ( 5.974727161628367256, 19.82959049719567801, 5.297264154381005063 ) ) ;
#33719 = FACE_OUTER_BOUND ( 'NONE', #29134, .T. ) ;
#33720 = CARTESIAN_POINT ( 'NONE',  ( 0.1103878639767399417, -37.37111717125858235, -21.52017980327885027 ) ) ;
#33721 = EDGE_CURVE ( 'NONE', #31232, #19850, #39229, .T. ) ;
#33722 = DIRECTION ( 'NONE',  ( 0.09722883295013595717, -0.3959434903494524760, -0.9131129757554907744 ) ) ;
#33723 = B_SPLINE_CURVE_WITH_KNOTS ( 'NONE', 3,
 ( #29635, #54342, #29950, #30554 ),
 .UNSPECIFIED., .F., .F.,
 ( 4, 4 ),
 ( 1.898592485710544765E-17, 0.004444306975806117631 ),
 .UNSPECIFIED. ) ;
#33724 = ORIENTED_EDGE ( 'NONE', *, *, #15018, .F. ) ;
#33725 = CARTESIAN_POINT ( 'NONE',  ( 4.956653778116970166, 36.51451553856417576, 31.29546495791861460 ) ) ;
#33726 = AXIS2_PLACEMENT_3D ( 'NONE', #5413, #43684, #39285 ) ;
#33727 = ORIENTED_EDGE ( 'NONE', *, *, #42197, .T. ) ;
#33728 = CARTESIAN_POINT ( 'NONE',  ( 0.9762797500689124330, -34.26226594605912368, -24.13341909939868657 ) ) ;
#33729 = CARTESIAN_POINT ( 'NONE',  ( -6.016104459813374383, 16.31603998697569580, 9.426230926598698545 ) ) ;
#33730 = AXIS2_PLACEMENT_3D ( 'NONE', #17278, #44565, #58931 ) ;
#33731 = EDGE_LOOP ( 'NONE', ( #47169, #46383, #46815, #25900 ) ) ;
#33732 = DIRECTION ( 'NONE',  ( -1.000000000000000000, -0.000000000000000000, -0.000000000000000000 ) ) ;
#33733 = AXIS2_PLACEMENT_3D ( 'NONE', #14212, #55311, #46807 ) ;
#33734 = CARTESIAN_POINT ( 'NONE',  ( 0.1129192098497455998, -27.88830454350494392, 34.19348267541455044 ) ) ;
#33735 = CARTESIAN_POINT ( 'NONE',  ( 4.549368137175248350, -24.02461520945246320, -35.57418903283107880 ) ) ;
#33736 = ORIENTED_EDGE ( 'NONE', *, *, #23694, .T. ) ;
#33737 = CARTESIAN_POINT ( 'NONE',  ( 0.5827359174754822568, -17.99288944686860248, -44.38786494726115706 ) ) ;
#33738 = DIRECTION ( 'NONE',  ( -1.000000000000000000, -0.000000000000000000, -0.000000000000000000 ) ) ;
#33739 = FACE_OUTER_BOUND ( 'NONE', #13145, .T. ) ;
#33740 = CARTESIAN_POINT ( 'NONE',  ( 0.8753041380234471980, -35.88662119133365991, 33.51550010581227212 ) ) ;
#33741 = LINE ( 'NONE', #23098, #769 ) ;
#33742 = VERTEX_POINT ( 'NONE', #38926 ) ;
#33743 = CARTESIAN_POINT ( 'NONE',  ( 0.9758171775293909000, 39.64000636436386316, -16.42583507057825187 ) ) ;
#33744 = CARTESIAN_POINT ( 'NONE',  ( -6.001507490154110336, -9.435425682280705217, -16.31148204059957152 ) ) ;
#33745 = CARTESIAN_POINT ( 'NONE',  ( 0.5824936645240103017, 28.11017874027236374, -37.53739509116535089 ) ) ;
#33746 = ORIENTED_EDGE ( 'NONE', *, *, #14938, .F. ) ;
#33747 = DIRECTION ( 'NONE',  ( -0.07906939808003035641, 0.9592846432126468370, -0.2711475679102552938 ) ) ;
#33748 = LINE ( 'NONE', #9602, #57327 ) ;
#33749 = CARTESIAN_POINT ( 'NONE',  ( 0.8753041380234471980, 36.80657072176690292, 32.50253343320412824 ) ) ;
#33750 = DIRECTION ( 'NONE',  ( 0.000000000000000000, 3.491481338843138088E-15, -1.000000000000000000 ) ) ;
#33751 = CARTESIAN_POINT ( 'NONE',  ( 0.8560838555295158248, 46.89922841446242074, 0.9138972643637033322 ) ) ;
#33752 = CARTESIAN_POINT ( 'NONE',  ( 0.5997462898726536595, -20.35457962188229430, 44.69052157405150183 ) ) ;
#33753 = CARTESIAN_POINT ( 'NONE',  ( 0.5827359174754810356, -47.89462060834306811, -0.3632382226755718757 ) ) ;
#33754 = DIRECTION ( 'NONE',  ( -0.9848077530122077983, -0.09698383872753986445, -0.1440410519008965273 ) ) ;
#33756 = EDGE_CURVE ( 'NONE', #24624, #8570, #35138, .T. ) ;
#33755 = CARTESIAN_POINT ( 'NONE',  ( 0.9730545539215892381, -10.61654491617593266, 41.57420493492382008 ) ) ;
#33757 = FACE_OUTER_BOUND ( 'NONE', #28274, .T. ) ;
#33758 = ADVANCED_FACE ( 'NONE', ( #49838 ), #39094, .F. ) ;
#33759 = CARTESIAN_POINT ( 'NONE',  ( 0.1073791018717483448, -34.50606437925530656, -25.86618856530698451 ) ) ;
#33760 = EDGE_CURVE ( 'NONE', #355, #13139, #39139, .T. ) ;
#33762 = VERTEX_POINT ( 'NONE', #15409 ) ;
#33761 = CARTESIAN_POINT ( 'NONE',  ( 5.719999999999996199, 6.882900011658699842E-15, 0.000000000000000000 ) ) ;
#33763 = ORIENTED_EDGE ( 'NONE', *, *, #11426, .F. ) ;
#33764 = CARTESIAN_POINT ( 'NONE',  ( 5.974727161628369032, -10.27590650342049550, 17.76736931401842412 ) ) ;
#33765 = EDGE_CURVE ( 'NONE', #15772, #48535, #53583, .T. ) ;
#33766 = CARTESIAN_POINT ( 'NONE',  ( 2.624215991343608501, 7.662883702705343580, -47.39206852872448650 ) ) ;
#33767 = CARTESIAN_POINT ( 'NONE',  ( -6.072942160501519027, 3.087637228658090205, -19.00712126107541167 ) ) ;
#33768 = CARTESIAN_POINT ( 'NONE',  ( 0.7242003506640004584, -35.83729897872414227, -33.56634737405257596 ) ) ;
#33769 = CARTESIAN_POINT ( 'NONE',  ( 0.1145239942831223490, 10.13668889349744973, -42.94406849590660613 ) ) ;
#33770 = ORIENTED_EDGE ( 'NONE', *, *, #11262, .T. ) ;
#33771 = AXIS2_PLACEMENT_3D ( 'NONE', #32309, #51386, #56703 ) ;
#33772 = CARTESIAN_POINT ( 'NONE',  ( 0.1365634738349378596, -22.32623199351180432, -38.05787677465910690 ) ) ;
#33773 = EDGE_CURVE ( 'NONE', #26516, #56097, #61493, .T. ) ;
#33774 = CONICAL_SURFACE ( 'NONE', #6705, 2.055000000000000160, 0.7853981633974639331 ) ;
#33775 = CARTESIAN_POINT ( 'NONE',  ( -25.39999999999999858, 1.530808498934191324E-15, -12.49999999999999822 ) ) ;
#33776 = VECTOR ( 'NONE', #36642, 1000.000000000000114 ) ;
#33777 = CARTESIAN_POINT ( 'NONE',  ( 0.8753041380234524160, -2.462982411634174085, -49.04153388213872944 ) ) ;
#33778 = ORIENTED_EDGE ( 'NONE', *, *, #49508, .F. ) ;
#33779 = EDGE_CURVE ( 'NONE', #2725, #38521, #10713, .T. ) ;
#33780 = CARTESIAN_POINT ( 'NONE',  ( 2.618530812446115519, 6.104648047582319492, 46.60965631082630267 ) ) ;
#33781 = CARTESIAN_POINT ( 'NONE',  ( 0.5809828226811553087, 47.41188724015889022, -6.791453954329836229 ) ) ;
#33782 =( BOUNDED_SURFACE ( )  B_SPLINE_SURFACE ( 3, 1, ( 
 ( #2894, #8213 ),
 ( #17950, #31105 ),
 ( #37065, #41150 ),
 ( #12327, #7591 ) ),
 .UNSPECIFIED., .F., .F., .F. ) 
 B_SPLINE_SURFACE_WITH_KNOTS ( ( 4, 4 ),
 ( 2, 2 ),
 ( 0.000000000000000000, 1.000000000000000000 ),
 ( 0.000000000000000000, 1.000000000000000000 ),
 .UNSPECIFIED. ) 
 GEOMETRIC_REPRESENTATION_ITEM ( )  RATIONAL_B_SPLINE_SURFACE ( (
 ( 1.000000000000000000, 1.000000000000000000),
 ( 0.7282232189291693025, 0.9929344683865674037),
 ( 0.7282232189291693025, 0.9929344683865674037),
 ( 1.000000000000000000, 1.000000000000000000) ) ) 
 REPRESENTATION_ITEM ( '' )  SURFACE ( )  );
#33783 = B_SPLINE_CURVE_WITH_KNOTS ( 'NONE', 3,
 ( #39950, #59623, #20502, #58685, #11732, #59007, #40258, #35229, #30810, #2294, #54290, #6668, #36781, #27973, #41792, #32071 ),
 .UNSPECIFIED., .F., .F.,
 ( 4, 3, 3, 3, 3, 4 ),
 ( 1.995049841954898532E-17, 0.0002618515315864414347, 0.0003927756766341991296, 0.0005236998216950568058, 0.0007855159896329902240, 0.001047349442285928304 ),
 .UNSPECIFIED. ) ;
#33784 = VERTEX_POINT ( 'NONE', #48909 ) ;
#33785 = CARTESIAN_POINT ( 'NONE',  ( 0.5809828226811617480, 28.72298383114487663, 38.32755012159156394 ) ) ;
#33786 = ORIENTED_EDGE ( 'NONE', *, *, #48779, .F. ) ;
#33787 = CARTESIAN_POINT ( 'NONE',  ( 50.84796438615735781, 15.27481071999428508, -2.632742199681755491 ) ) ;
#33788 = CARTESIAN_POINT ( 'NONE',  ( 4.975610109902397937, 42.89797504594955058, -23.49921581872176191 ) ) ;
#33789 = ORIENTED_EDGE ( 'NONE', *, *, #53281, .T. ) ;
#33790 = FACE_BOUND ( 'NONE', #3377, .T. ) ;
#33791 = CARTESIAN_POINT ( 'NONE',  ( 0.5848930533535030563, 10.69427347779520332, -45.66076649783362029 ) ) ;
#33792 = CARTESIAN_POINT ( 'NONE',  ( 4.967162193818130511, 38.83676580803767564, 18.65818244221271627 ) ) ;
#33793 = CARTESIAN_POINT ( 'NONE',  ( -6.078726893082806448, -1.845620846545350080, -19.16736092839902383 ) ) ;
#33794 = CIRCLE ( 'NONE', #30764, 0.05882000000000109363 ) ;
#33795 = ORIENTED_EDGE ( 'NONE', *, *, #48655, .F. ) ;
#33796 = B_SPLINE_CURVE_WITH_KNOTS ( 'NONE', 3,
 ( #4399, #29469, #38909, #47355 ),
 .UNSPECIFIED., .F., .F.,
 ( 4, 4 ),
 ( 0.000000000000000000, 0.004447772540403843212 ),
 .UNSPECIFIED. ) ;
#33797 = CARTESIAN_POINT ( 'NONE',  ( 0.9775691876210974574, -6.597867306536943310, -41.38601038992914738 ) ) ;
#33798 = ORIENTED_EDGE ( 'NONE', *, *, #34774, .T. ) ;
#33799 = CARTESIAN_POINT ( 'NONE',  ( 45.00000000000001421, 0.000000000000000000, 0.000000000000000000 ) ) ;
#33800 = EDGE_CURVE ( 'NONE', #4875, #33073, #23422, .T. ) ;
#33801 = ORIENTED_EDGE ( 'NONE', *, *, #11743, .T. ) ;
#33802 = VECTOR ( 'NONE', #48160, 1000.000000000000114 ) ;
#33803 = ORIENTED_EDGE ( 'NONE', *, *, #17407, .T. ) ;
#33804 = CARTESIAN_POINT ( 'NONE',  ( 0.8560838555295223751, -0.6537497281626496459, 46.90357604036880446 ) ) ;
#33805 = CARTESIAN_POINT ( 'NONE',  ( 0.9784957157296372277, -37.29867915761859365, 19.10867839724658168 ) ) ;
#33806 = CARTESIAN_POINT ( 'NONE',  ( 0.9762797500689124330, 38.77779312671030709, 15.89363222827819300 ) ) ;
#33807 = ORIENTED_EDGE ( 'NONE', *, *, #25129, .T. ) ;
#33808 = CARTESIAN_POINT ( 'NONE',  ( 0.9757402383260946888, 0.08489923450698490248, -42.90839848328081274 ) ) ;
#33809 = CARTESIAN_POINT ( 'NONE',  ( 4.691466044806102076, -25.04870410140817327, 36.88741755356026175 ) ) ;
#33810 = CARTESIAN_POINT ( 'NONE',  ( -6.072942160501519027, 19.25627044167812230, 0.01452466776899024453 ) ) ;
#33811 = ORIENTED_EDGE ( 'NONE', *, *, #12198, .T. ) ;
#33812 = ORIENTED_EDGE ( 'NONE', *, *, #33837, .F. ) ;
#33813 = CARTESIAN_POINT ( 'NONE',  ( 0.6253024248130479856, -49.10165524324679609, -0.6867894808279696450 ) ) ;
#33814 = LINE ( 'NONE', #20624, #35828 ) ;
#33815 = CARTESIAN_POINT ( 'NONE',  ( 1.157644175074336257, 38.90537128965222280, -15.60046025902721389 ) ) ;
#33816 = CARTESIAN_POINT ( 'NONE',  ( 0.9762797500689124330, -26.66896101499549587, -32.32787193067855469 ) ) ;
#33817 = CARTESIAN_POINT ( 'NONE',  ( 4.553261556744873317, -36.93702150832076825, -23.77385134801438937 ) ) ;
#33818 = ORIENTED_EDGE ( 'NONE', *, *, #27942, .T. ) ;
#33819 = VERTEX_POINT ( 'NONE', #53894 ) ;
#33820 = CIRCLE ( 'NONE', #23786, 42.92674063221959813 ) ;
#33821 = CARTESIAN_POINT ( 'NONE',  ( 4.553261556744873317, -9.554252317234828595, 42.87488575474283437 ) ) ;
#33822 = CARTESIAN_POINT ( 'NONE',  ( 0.9787284016396613495, -41.03117890019433389, 8.531023208799519253 ) ) ;
#33823 = DIRECTION ( 'NONE',  ( 0.000000000000000000, 0.000000000000000000, 1.000000000000000000 ) ) ;
#33824 = CARTESIAN_POINT ( 'NONE',  ( 0.9747592971366239034, -21.17324310849259916, 37.32069240268765498 ) ) ;
#33825 = CARTESIAN_POINT ( 'NONE',  ( 0.7762777257811885878, 7.133808567472943452, -47.37038525518526910 ) ) ;
#33826 = PRESENTATION_STYLE_ASSIGNMENT (( #14105 ) ) ;
#33827 = LINE ( 'NONE', #43539, #7837 ) ;
#33828 = ORIENTED_EDGE ( 'NONE', *, *, #49160, .F. ) ;
#33829 = CARTESIAN_POINT ( 'NONE',  ( -2.739355103387248747, 14.70078895384969186, 2.595066682262317848 ) ) ;
#33830 = CARTESIAN_POINT ( 'NONE',  ( 0.6067099128993220791, 43.97493306231487509, -18.98236771638412179 ) ) ;
#33831 = EDGE_CURVE ( 'NONE', #7571, #23099, #21918, .T. ) ;
#33832 = CARTESIAN_POINT ( 'NONE',  ( -90.00000000000000000, 0.000000000000000000, -5.612499999999999822 ) ) ;
#33833 = CARTESIAN_POINT ( 'NONE',  ( 0.1095718737110177865, -16.26534146842179851, -39.93945841550369380 ) ) ;
#33834 = VECTOR ( 'NONE', #58126, 1000.000000000000000 ) ;
#33835 = B_SPLINE_CURVE_WITH_KNOTS ( 'NONE', 3,
 ( #58521, #15653, #30342, #23879 ),
 .UNSPECIFIED., .F., .F.,
 ( 4, 4 ),
 ( 0.000000000000000000, 0.004446090762761371190 ),
 .UNSPECIFIED. ) ;
#33836 = CARTESIAN_POINT ( 'NONE',  ( 4.549368137175248350, 35.57418903283081590, 24.02461520945284690 ) ) ;
#33837 = EDGE_CURVE ( 'NONE', #2091, #8650, #7693, .T. ) ;
#33838 = DIRECTION ( 'NONE',  ( 2.218671295934095703E-31, -1.000000000000000000, 1.110223024625156540E-16 ) ) ;
#33839 = CARTESIAN_POINT ( 'NONE',  ( 0.000000000000000000, 0.6959691356230525150, 0.000000000000000000 ) ) ;
#33840 = B_SPLINE_CURVE_WITH_KNOTS ( 'NONE', 3,
 ( #11466, #44392, #53722, #50281 ),
 .UNSPECIFIED., .F., .F.,
 ( 4, 4 ),
 ( 0.000000000000000000, 0.004444878191957665238 ),
 .UNSPECIFIED. ) ;
#33841 = ORIENTED_EDGE ( 'NONE', *, *, #57631, .T. ) ;
#33842 = PRESENTATION_LAYER_ASSIGNMENT (  '', '', ( #60818 ) ) ;
#33843 = CARTESIAN_POINT ( 'NONE',  ( -90.00000000000000000, 0.000000000000000000, -6.887500000000022382 ) ) ;
#33844 = B_SPLINE_CURVE_WITH_KNOTS ( 'NONE', 3,
 ( #56423, #28536, #37665, #47660 ),
 .UNSPECIFIED., .F., .F.,
 ( 4, 4 ),
 ( 0.000000000000000000, 0.004445488388166996853 ),
 .UNSPECIFIED. ) ;
#33845 = CARTESIAN_POINT ( 'NONE',  ( 0.1097557419366048670, 37.45792859959197330, 21.36873056345907074 ) ) ;
#33846 = CARTESIAN_POINT ( 'NONE',  ( 0.6021448801613057400, -47.43444021936057453, -12.70885595570491589 ) ) ;
#33847 = CARTESIAN_POINT ( 'NONE',  ( 4.956653778116966613, 0.000000000000000000, 0.000000000000000000 ) ) ;
#33848 = CARTESIAN_POINT ( 'NONE',  ( 0.1119899015040010382, 4.795286430103810282, -43.86304294329986675 ) ) ;
#33849 = VERTEX_POINT ( 'NONE', #15723 ) ;
#33850 = EDGE_CURVE ( 'NONE', #18146, #58874, #45786, .T. ) ;
#33851 = LINE ( 'NONE', #5904, #23313 ) ;
#33852 = CARTESIAN_POINT ( 'NONE',  ( 0.5804410086790514622, -44.48029469925801749, 14.86685021524587746 ) ) ;
#33853 = CARTESIAN_POINT ( 'NONE',  ( -6.063463321072278589, -6.635954031850681112, -18.07718359055509794 ) ) ;
#33854 = ORIENTED_EDGE ( 'NONE', *, *, #19292, .T. ) ;
#33855 = CARTESIAN_POINT ( 'NONE',  ( 0.5988103622719991304, -44.67429504351072467, 17.84821742497916830 ) ) ;
#33856 = CARTESIAN_POINT ( 'NONE',  ( 1.157643937452369265, 15.83273913728741888, 38.81142416873363032 ) ) ;
#33857 = ORIENTED_EDGE ( 'NONE', *, *, #30916, .F. ) ;
#33858 = AXIS2_PLACEMENT_3D ( 'NONE', #42552, #27199, #9317 ) ;
#33859 = CARTESIAN_POINT ( 'NONE',  ( 0.8744876279028306332, -31.30103973185180521, -37.82320666052162039 ) ) ;
#33860 = VECTOR ( 'NONE', #22800, 1000.000000000000000 ) ;
#33861 = VERTEX_POINT ( 'NONE', #12264 ) ;
#33862 = CARTESIAN_POINT ( 'NONE',  ( -6.015611763856276717, 17.41126425312547710, -7.205255340944423992 ) ) ;
#33863 = ORIENTED_EDGE ( 'NONE', *, *, #30334, .F. ) ;
#33864 = CARTESIAN_POINT ( 'NONE',  ( 0.1157506346131639274, 29.59596297817652299, -32.72643633512880257 ) ) ;
#33865 = CARTESIAN_POINT ( 'NONE',  ( 0.1064266379913940547, 40.05351204369885210, 15.98292486309350124 ) ) ;
#33866 = ORIENTED_EDGE ( 'NONE', *, *, #39144, .F. ) ;
#33867 = CARTESIAN_POINT ( 'NONE',  ( 42.00000000000000711, 0.000000000000000000, 0.000000000000000000 ) ) ;
#33868 = ORIENTED_EDGE ( 'NONE', *, *, #26365, .F. ) ;
#33869 = CARTESIAN_POINT ( 'NONE',  ( 0.5837374860065638327, 0.1816420316515440225, 47.89569815517036488 ) ) ;
#33870 = CARTESIAN_POINT ( 'NONE',  ( -90.00000000000000000, 0.000000000000000000, -6.728125000000023448 ) ) ;
#33871 = EDGE_CURVE ( 'NONE', #38401, #2370, #42791, .T. ) ;
#33872 = ORIENTED_EDGE ( 'NONE', *, *, #56716, .T. ) ;
#33873 = DIRECTION ( 'NONE',  ( 0.000000000000000000, 0.000000000000000000, 1.000000000000000000 ) ) ;
#33874 = CIRCLE ( 'NONE', #60848, 2.649999999999985700 ) ;
#33875 = CARTESIAN_POINT ( 'NONE',  ( 0.5998501479064708430, 5.759754759340140140, 47.76154736470759588 ) ) ;
#33876 = CARTESIAN_POINT ( 'NONE',  ( 0.5824935313925951874, 17.19420832410670030, 43.63023466772849446 ) ) ;
#33877 = ORIENTED_EDGE ( 'NONE', *, *, #24309, .F. ) ;
#33878 = CARTESIAN_POINT ( 'NONE',  ( 0.7044674535452954967, 5.553212498071502523, -48.79512838144981401 ) ) ;
#33879 = ORIENTED_EDGE ( 'NONE', *, *, #53896, .F. ) ;
#33880 = CARTESIAN_POINT ( 'NONE',  ( 3.782625744892852637, 26.30387422842974843, 32.79244279815019070 ) ) ;
#33881 = ADVANCED_FACE ( 'NONE', ( #11964 ), #20233, .F. ) ;
#33882 = ORIENTED_EDGE ( 'NONE', *, *, #28804, .F. ) ;
#33883 = CARTESIAN_POINT ( 'NONE',  ( 4.549368137175248350, -3.018832571116246477, -42.82045902618772004 ) ) ;
#33884 = CARTESIAN_POINT ( 'NONE',  ( 0.9780303403264780648, 40.33289069370958657, -11.38409160558530608 ) ) ;
#33885 = ORIENTED_EDGE ( 'NONE', *, *, #21424, .T. ) ;
#33886 = CARTESIAN_POINT ( 'NONE',  ( 0.5837800304671231233, 4.648813602424494817, 46.66503899354860607 ) ) ;
#33887 = CARTESIAN_POINT ( 'NONE',  ( 0.1158403557922069033, 25.27520615740563414, -36.16772402134896680 ) ) ;
#33888 = EDGE_CURVE ( 'NONE', #45432, #57208, #38238, .T. ) ;
#33889 = CARTESIAN_POINT ( 'NONE',  ( -6.017396004339686577, -18.68211039806562113, -2.458362590802985359 ) ) ;
#33890 = CARTESIAN_POINT ( 'NONE',  ( -25.39999999999999858, 0.000000000000000000, 0.000000000000000000 ) ) ;
#33891 = B_SPLINE_CURVE_WITH_KNOTS ( 'NONE', 3,
 ( #30918, #40349, #55017, #50028 ),
 .UNSPECIFIED., .F., .F.,
 ( 4, 4 ),
 ( 0.000000000000000000, 0.004442905043737215703 ),
 .UNSPECIFIED. ) ;
#33892 = VERTEX_POINT ( 'NONE', #18727 ) ;
#33893 = CARTESIAN_POINT ( 'NONE',  ( 0.1129192098497455998, -41.07894348801367812, 16.10814047907867064 ) ) ;
#33894 = CARTESIAN_POINT ( 'NONE',  ( -5.995132425357893702, 7.203480333239314248, -17.41298668506963310 ) ) ;
#33895 = CARTESIAN_POINT ( 'NONE',  ( 2.624215991343608501, 25.21574086439763107, -40.85210347989505664 ) ) ;
#33896 = CARTESIAN_POINT ( 'NONE',  ( 0.6001305935487315502, 0.5236757026889412581, -48.10757715638248300 ) ) ;
#33897 = LINE ( 'NONE', #57049, #38859 ) ;
#33898 = CARTESIAN_POINT ( 'NONE',  ( 4.226256110419179812, -9.374554497711095280, -42.92953503075280253 ) ) ;
#33899 = EDGE_CURVE ( 'NONE', #13696, #11002, #26336, .T. ) ;
#33900 = CIRCLE ( 'NONE', #57874, 42.92674063221959813 ) ;
#33901 = CARTESIAN_POINT ( 'NONE',  ( 3.407937589446174087, -8.699069120706843350, 10.58239600294635885 ) ) ;
#33902 = CIRCLE ( 'NONE', #49893, 42.88844316795388778 ) ;
#33903 = CARTESIAN_POINT ( 'NONE',  ( -17.04189967907673520, -7.774469338339614843, -1.886945943481975085 ) ) ;
#33904 = ADVANCED_FACE ( 'NONE', ( #55754 ), #624, .F. ) ;
#33905 = CARTESIAN_POINT ( 'NONE',  ( 0.5997462898726536595, 44.01516392039513903, -21.77652348757843015 ) ) ;
#33906 = CARTESIAN_POINT ( 'NONE',  ( 0.2279481005628771206, 34.08161525712255013, -28.01690540617190095 ) ) ;
#33907 = CARTESIAN_POINT ( 'NONE',  ( 0.1129192098497447394, -43.82135468580274562, -5.161459220630158384 ) ) ;
#33908 = DIRECTION ( 'NONE',  ( 0.000000000000000000, 0.000000000000000000, 1.000000000000000000 ) ) ;
#33909 = CARTESIAN_POINT ( 'NONE',  ( 0.8557997880470697982, 44.60232077416686991, 17.48760788519232889 ) ) ;
#33910 = CARTESIAN_POINT ( 'NONE',  ( 0.1368894036331284314, -17.27553727570517594, 40.60070366088567795 ) ) ;
#33911 = EDGE_CURVE ( 'NONE', #48869, #47737, #5347, .T. ) ;
#33912 = CARTESIAN_POINT ( 'NONE',  ( 3.680974057930773036, 47.94008194857087801, 1.849713332883914818 ) ) ;
#33913 = CARTESIAN_POINT ( 'NONE',  ( 0.3622758884714600280, 26.89560658783384994, -33.69533458712316332 ) ) ;
#33914 = VERTEX_POINT ( 'NONE', #60151 ) ;
#33915 = CARTESIAN_POINT ( 'NONE',  ( 0.5809828226811565299, 28.72298383114543796, -38.32755012159114472 ) ) ;
#33916 = CARTESIAN_POINT ( 'NONE',  ( 2.185380717157383579, 19.08024733508938198, -39.68329578927402679 ) ) ;
#33917 = CARTESIAN_POINT ( 'NONE',  ( 1.000433927950261870, 38.32221909574490581, -16.96544138036415461 ) ) ;
#33918 = ORIENTED_EDGE ( 'NONE', *, *, #48583, .F. ) ;
#33919 = EDGE_CURVE ( 'NONE', #29140, #13648, #4583, .T. ) ;
#33920 = CARTESIAN_POINT ( 'NONE',  ( 3.240649175237395596, -21.22199265827904213, -38.53429569889141248 ) ) ;
#33921 = CARTESIAN_POINT ( 'NONE',  ( 2.359973842542475886, 26.40990395922420220, 35.22290259897746267 ) ) ;
#33922 = AXIS2_PLACEMENT_3D ( 'NONE', #16474, #40010, #21176 ) ;
#33923 = ORIENTED_EDGE ( 'NONE', *, *, #16969, .T. ) ;
#33924 = VERTEX_POINT ( 'NONE', #1133 ) ;
#33925 = CARTESIAN_POINT ( 'NONE',  ( 4.553261556744875094, -41.61700166486733110, -14.05577241741153216 ) ) ;
#33926 = ORIENTED_EDGE ( 'NONE', *, *, #10075, .T. ) ;
#33927 = CARTESIAN_POINT ( 'NONE',  ( 0.5797568665920712627, 28.32170371298940736, 37.37788660953842168 ) ) ;
#33928 = ORIENTED_EDGE ( 'NONE', *, *, #55433, .T. ) ;
#33929 = VERTEX_POINT ( 'NONE', #20270 ) ;
#33930 = CARTESIAN_POINT ( 'NONE',  ( 1.227938101723756947, -41.66816631169184859, -10.28900963485423858 ) ) ;
#33931 = ORIENTED_EDGE ( 'NONE', *, *, #17919, .T. ) ;
#33932 = CARTESIAN_POINT ( 'NONE',  ( 0.5980271706414711508, 33.53334604750737924, -35.88264128655782059 ) ) ;
#33933 = DIRECTION ( 'NONE',  ( 1.000000000000000000, 0.000000000000000000, 0.000000000000000000 ) ) ;
#33934 = CARTESIAN_POINT ( 'NONE',  ( 0.1100053167205930632, -30.62023953839061718, -30.36644426605129610 ) ) ;
#33935 = ORIENTED_EDGE ( 'NONE', *, *, #29628, .T. ) ;
#33936 = DIRECTION ( 'NONE',  ( 0.000000000000000000, 0.000000000000000000, 1.000000000000000000 ) ) ;
#33937 = CARTESIAN_POINT ( 'NONE',  ( 4.291220156522059348, 24.50578158393244976, -40.23500548361207052 ) ) ;
#33938 = VERTEX_POINT ( 'NONE', #23726 ) ;
#33939 = ORIENTED_EDGE ( 'NONE', *, *, #36302, .F. ) ;
#33940 = VECTOR ( 'NONE', #55621, 1000.000000000000114 ) ;
#33941 = B_SPLINE_CURVE_WITH_KNOTS ( 'NONE', 3,
 ( #14336, #9607, #33133, #18719, #18411, #61598 ),
 .UNSPECIFIED., .F., .F.,
 ( 4, 2, 4 ),
 ( 1.210102227977247116E-16, 0.0002448718616795922832, 0.0004897437233590635694 ),
 .UNSPECIFIED. ) ;
#33942 = ORIENTED_EDGE ( 'NONE', *, *, #51350, .T. ) ;
#33943 = CARTESIAN_POINT ( 'NONE',  ( -5.995132425357893702, 17.40647075750126760, -7.219211173946302296 ) ) ;
#33944 = CARTESIAN_POINT ( 'NONE',  ( 0.7048096507298635682, 5.442192462019463051, -47.80151517212782153 ) ) ;
#33945 = DIRECTION ( 'NONE',  ( 1.000000000000000000, 0.000000000000000000, 0.000000000000000000 ) ) ;
#33946 = CARTESIAN_POINT ( 'NONE',  ( 0.5797568665920713737, 40.02504847250913400, -24.43810146830487895 ) ) ;
#33947 = EDGE_CURVE ( 'NONE', #28202, #37398, #27011, .T. ) ;
#33948 = VERTEX_POINT ( 'NONE', #33759 ) ;
#33949 = FACE_OUTER_BOUND ( 'NONE', #9344, .T. ) ;
#33950 = DIRECTION ( 'NONE',  ( -1.000000000000000000, -0.000000000000000000, -0.000000000000000000 ) ) ;
#33951 = EDGE_CURVE ( 'NONE', #39805, #6056, #42855, .T. ) ;
#33952 =( BOUNDED_SURFACE ( )  B_SPLINE_SURFACE ( 3, 1, ( 
 ( #49222, #39543 ),
 ( #40473, #30728 ),
 ( #34523, #58287 ),
 ( #34835, #53591 ) ),
 .UNSPECIFIED., .F., .F., .F. ) 
 B_SPLINE_SURFACE_WITH_KNOTS ( ( 4, 4 ),
 ( 2, 2 ),
 ( 0.000000000000000000, 1.000000000000000000 ),
 ( 0.000000000000000000, 1.000000000000000000 ),
 .UNSPECIFIED. ) 
 GEOMETRIC_REPRESENTATION_ITEM ( )  RATIONAL_B_SPLINE_SURFACE ( (
 ( 1.000000000000000000, 1.000000000000000000),
 ( 0.9952954269826590483, 0.8620686068821307169),
 ( 0.9952954269826590483, 0.8620686068821307169),
 ( 1.000000000000000000, 1.000000000000000000) ) ) 
 REPRESENTATION_ITEM ( '' )  SURFACE ( )  );
#33953 = CARTESIAN_POINT ( 'NONE',  ( 0.5837157313716038187, 36.86032209105336932, -28.99230447766828433 ) ) ;
#33954 = ORIENTED_EDGE ( 'NONE', *, *, #16758, .T. ) ;
#33955 = CARTESIAN_POINT ( 'NONE',  ( -99.49999999999975842, 4.769696007084730738, -1.500000000000008438 ) ) ;
#33956 = CARTESIAN_POINT ( 'NONE',  ( 0.7948878604505683620, 33.64624533417287466, 35.75791971313581286 ) ) ;
#33957 = B_SPLINE_CURVE_WITH_KNOTS ( 'NONE', 3,
 ( #61349, #23777, #61655, #33813, #51652, #52578 ),
 .UNSPECIFIED., .F., .F.,
 ( 4, 2, 4 ),
 ( 2.521789927402474235E-18, 0.0002447193893791697623, 0.0004894387787583369225 ),
 .UNSPECIFIED. ) ;
#33958 = EDGE_CURVE ( 'NONE', #16449, #22415, #44425, .T. ) ;
#33959 = CARTESIAN_POINT ( 'NONE',  ( 3.783198216974394956, -20.00646744835639268, -38.10565824507919785 ) ) ;
#33960 = CARTESIAN_POINT ( 'NONE',  ( 1.092182651088185130, 41.90646141200330277, -0.7808177550258036392 ) ) ;
#33961 = B_SPLINE_CURVE_WITH_KNOTS ( 'NONE', 3,
 ( #14619, #54019, #25843, #15842 ),
 .UNSPECIFIED., .F., .F.,
 ( 4, 4 ),
 ( 2.189128766608093472E-17, 0.004559932413162186803 ),
 .UNSPECIFIED. ) ;
#33962 = VECTOR ( 'NONE', #6482, 1000.000000000000227 ) ;
#33963 = ORIENTED_EDGE ( 'NONE', *, *, #26689, .F. ) ;
#33964 = EDGE_LOOP ( 'NONE', ( #18050, #8482, #48112, #53913 ) ) ;
#33965 = CARTESIAN_POINT ( 'NONE',  ( -2.708315649062910779, 4.041664582652797044, -14.06540004355478857 ) ) ;
#33966 = CARTESIAN_POINT ( 'NONE',  ( 0.7762777257811885878, 13.25585385760172130, -46.03397617421214960 ) ) ;
#33967 = CARTESIAN_POINT ( 'NONE',  ( 4.962356264823609031, -32.75738977283769771, -26.42326651140497873 ) ) ;
#33968 = CARTESIAN_POINT ( 'NONE',  ( 1.830465331921978578, 43.45643058836503769, -7.205185382556205553 ) ) ;
#33969 = CARTESIAN_POINT ( 'NONE',  ( 0.8560838555295158248, 46.35895890951125153, 7.156798369940231552 ) ) ;
#33970 = CARTESIAN_POINT ( 'NONE',  ( 0.1310142868023690677, -43.11885108606330164, -0.6370537502134987484 ) ) ;
#33971 =( BOUNDED_SURFACE ( )  B_SPLINE_SURFACE ( 3, 1, ( 
 ( #46096, #2830 ),
 ( #3140, #22269 ),
 ( #6577, #58917 ),
 ( #30408, #49524 ) ),
 .UNSPECIFIED., .F., .F., .F. ) 
 B_SPLINE_SURFACE_WITH_KNOTS ( ( 4, 4 ),
 ( 2, 2 ),
 ( 0.000000000000000000, 1.000000000000000000 ),
 ( 0.000000000000000000, 1.000000000000000000 ),
 .UNSPECIFIED. ) 
 GEOMETRIC_REPRESENTATION_ITEM ( )  RATIONAL_B_SPLINE_SURFACE ( (
 ( 1.000000000000000000, 1.000000000000000000),
 ( 0.9953040768229013402, 0.8617119497784988535),
 ( 0.9953040768229013402, 0.8617119497784988535),
 ( 1.000000000000000000, 1.000000000000000000) ) ) 
 REPRESENTATION_ITEM ( '' )  SURFACE ( )  );
#33972 = CARTESIAN_POINT ( 'NONE',  ( 4.975801465491694664, -31.15993731089097452, -36.39623109580456628 ) ) ;
#33973 = CARTESIAN_POINT ( 'NONE',  ( 0.6000166863083106206, 44.47108027094602534, 20.83618250168510144 ) ) ;
#33974 = CARTESIAN_POINT ( 'NONE',  ( -6.063463321072278589, 19.10058954492600236, -2.447025033736572652 ) ) ;
#33975 = EDGE_CURVE ( 'NONE', #48896, #58618, #30767, .T. ) ;
#33976 = CARTESIAN_POINT ( 'NONE',  ( 0.6025881611877910160, -18.20817581200385504, -44.52856035602900420 ) ) ;
#33977 = ORIENTED_EDGE ( 'NONE', *, *, #56001, .T. ) ;
#33978 = ADVANCED_FACE ( 'NONE', ( #10246 ), #7014, .F. ) ;
#33979 = DIRECTION ( 'NONE',  ( -0.1736481776669312471, 0.9848077530122077983, -5.551115123125779621E-17 ) ) ;
#33980 = FACE_OUTER_BOUND ( 'NONE', #26358, .T. ) ;
#33981 = CARTESIAN_POINT ( 'NONE',  ( -6.072942160501519027, 16.77122109808123085, 9.462045506564395581 ) ) ;
#33982 = CARTESIAN_POINT ( 'NONE',  ( 7.000000000000016875, -56.56854249492331377, -56.56854249492430142 ) ) ;
#33983 = CARTESIAN_POINT ( 'NONE',  ( 0.5988103622719992414, -34.44344971428051139, 33.58571533649100616 ) ) ;
#33984 = CARTESIAN_POINT ( 'NONE',  ( 0.6031356755773454870, -46.46821530722348115, 12.45114731045949519 ) ) ;
#33985 = CARTESIAN_POINT ( 'NONE',  ( 1.231276596079887264, 10.53918392497828727, 40.57341954055075917 ) ) ;
#33986 = DIRECTION ( 'NONE',  ( 1.000000000000000000, 0.000000000000000000, 0.000000000000000000 ) ) ;
#33987 = EDGE_CURVE ( 'NONE', #40429, #24828, #24013, .T. ) ;
#33988 = B_SPLINE_CURVE_WITH_KNOTS ( 'NONE', 3,
 ( #14991, #57543, #28760, #43501 ),
 .UNSPECIFIED., .F., .F.,
 ( 4, 4 ),
 ( 2.175771182130668512E-17, 0.004559932413162186803 ),
 .UNSPECIFIED. ) ;
#33989 = AXIS2_PLACEMENT_3D ( 'NONE', #33617, #5982, #52694 ) ;
#33990 = CARTESIAN_POINT ( 'NONE',  ( 0.6008122571543326185, 22.32719153875445528, -43.73843925492870710 ) ) ;
#33991 = CARTESIAN_POINT ( 'NONE',  ( 0.9758171775293941197, -11.09981579996835421, 41.44794628856071483 ) ) ;
#33992 = CARTESIAN_POINT ( 'NONE',  ( 4.975801465491694664, -47.10002938642148251, 8.787181743659342459 ) ) ;
#33994 = ORIENTED_EDGE ( 'NONE', *, *, #39656, .F. ) ;
#33993 = CARTESIAN_POINT ( 'NONE',  ( 0.5988103564986352323, -6.880138274944628485, -47.61318305157292485 ) ) ;
#33995 = ORIENTED_EDGE ( 'NONE', *, *, #9619, .F. ) ;
#33996 = AXIS2_PLACEMENT_3D ( 'NONE', #30825, #12065, #1688 ) ;
#33997 = CARTESIAN_POINT ( 'NONE',  ( 0.5809828226811617480, 17.82437196699680726, 44.45562576850608139 ) ) ;
#33998 = CARTESIAN_POINT ( 'NONE',  ( 3.894904216938897878, 43.66689113967132840, -5.032588863824957848 ) ) ;
#33999 = CARTESIAN_POINT ( 'NONE',  ( 0.1158403557922069033, 41.86432774633747300, 13.93981239224752500 ) ) ;
#34000 = EDGE_CURVE ( 'NONE', #56250, #25196, #38774, .T. ) ;
#34001 = ORIENTED_EDGE ( 'NONE', *, *, #31839, .F. ) ;
#34002 = CARTESIAN_POINT ( 'NONE',  ( 0.1101816497532063233, -11.03018586750523689, 41.68997876247028245 ) ) ;
#34003 = DIRECTION ( 'NONE',  ( -2.249565377136137858E-32, 1.224646799147353207E-16, 1.000000000000000000 ) ) ;
#34004 = CARTESIAN_POINT ( 'NONE',  ( 4.967162193818130511, 40.93989340068610261, 13.42934394584178648 ) ) ;
#34006 = EDGE_CURVE ( 'NONE', #31680, #32580, #3142, .T. ) ;
#34005 = ORIENTED_EDGE ( 'NONE', *, *, #44839, .F. ) ;
#34007 = ORIENTED_EDGE ( 'NONE', *, *, #60310, .F. ) ;
#34008 = DIRECTION ( 'NONE',  ( 1.000000000000000000, 1.836909530733573776E-16, -1.925929944387235853E-32 ) ) ;
#34009 = CARTESIAN_POINT ( 'NONE',  ( 4.960156602257181468, -44.12083041402475203, 14.43621227656513284 ) ) ;
#34010 = AXIS2_PLACEMENT_3D ( 'NONE', #38527, #10624, #14711 ) ;
#34011 = FACE_OUTER_BOUND ( 'NONE', #41717, .T. ) ;
#34012 = B_SPLINE_CURVE_WITH_KNOTS ( 'NONE', 3,
 ( #12290, #59559, #50780, #7871, #7548, #54855 ),
 .UNSPECIFIED., .F., .F.,
 ( 4, 2, 4 ),
 ( 1.177386153108680874E-16, 0.0002448718616795951563, 0.0004897437233590725683 ),
 .UNSPECIFIED. ) ;
#34013 = CARTESIAN_POINT ( 'NONE',  ( 0.5832655196449119117, 46.89545140795105738, 0.2276405452299705978 ) ) ;
#34014 = CARTESIAN_POINT ( 'NONE',  ( 0.6845945791218023269, 5.556290360844593934, 46.57825842751027068 ) ) ;
#34015 = CARTESIAN_POINT ( 'NONE',  ( 5.000000000000007994, -58.44237546506768410, -54.69470952477996661 ) ) ;
#34016 = CARTESIAN_POINT ( 'NONE',  ( -0.5999999999999992006, -11.64055411052240352, -1.199999999999999956 ) ) ;
#34017 = ORIENTED_EDGE ( 'NONE', *, *, #52556, .F. ) ;
#34018 = ORIENTED_EDGE ( 'NONE', *, *, #286, .F. ) ;
#34019 = CARTESIAN_POINT ( 'NONE',  ( -6.001507490154111224, -9.435425682280932591, 16.31148204059944007 ) ) ;
#34020 = LINE ( 'NONE', #29294, #16544 ) ;
#34021 = ORIENTED_EDGE ( 'NONE', *, *, #26461, .T. ) ;
#34022 = CARTESIAN_POINT ( 'NONE',  ( 3.680974057930773924, -47.28851186371002768, -8.091325130366254115 ) ) ;
#34023 = LINE ( 'NONE', #57163, #39684 ) ;
#34024 = CARTESIAN_POINT ( 'NONE',  ( 0.8744876279028263033, -19.05609938968970241, -45.24616145519706834 ) ) ;
#34025 = CARTESIAN_POINT ( 'NONE',  ( 0.1158816050234198480, -40.90156038422842499, -16.55307824667295336 ) ) ;
#34026 = EDGE_CURVE ( 'NONE', #54823, #49884, #12826, .T. ) ;
#34027 = B_SPLINE_CURVE_WITH_KNOTS ( 'NONE', 3,
 ( #20719, #39859, #58914, #16027, #6574, #25721 ),
 .UNSPECIFIED., .F., .F.,
 ( 4, 2, 4 ),
 ( 0.000000000000000000, 0.0002293801035737086402, 0.0004587602071474172804 ),
 .UNSPECIFIED. ) ;
#34028 = ORIENTED_EDGE ( 'NONE', *, *, #9346, .T. ) ;
#34029 = ORIENTED_EDGE ( 'NONE', *, *, #11739, .F. ) ;
#34030 = CARTESIAN_POINT ( 'NONE',  ( 0.5837800005270559200, -13.89411067738082473, 44.79050063491671807 ) ) ;
#34031 = CARTESIAN_POINT ( 'NONE',  ( 0.9730545539215883499, -42.47233286818612896, -6.101350888305089093 ) ) ;
#34032 = EDGE_CURVE ( 'NONE', #2702, #9808, #42015, .T. ) ;
#34033 = CARTESIAN_POINT ( 'NONE',  ( 3.319141568766058814, -12.31039395171775830, -1.199999999999999956 ) ) ;
#34034 = CARTESIAN_POINT ( 'NONE',  ( 5.981074661064941900, -17.77917279944639262, 10.25489689131099702 ) ) ;
#34035 = ORIENTED_EDGE ( 'NONE', *, *, #28199, .T. ) ;
#34036 = CARTESIAN_POINT ( 'NONE',  ( 4.553261556744873317, -20.51767157960462384, -38.84024612145397981 ) ) ;
#34038 = ORIENTED_EDGE ( 'NONE', *, *, #19813, .T. ) ;
#34037 = EDGE_CURVE ( 'NONE', #59362, #22451, #31561, .T. ) ;
#34039 = CARTESIAN_POINT ( 'NONE',  ( 0.5782707292762442330, 23.17211662964134433, -40.77731433787561599 ) ) ;
#34040 = CARTESIAN_POINT ( 'NONE',  ( 0.1129192098497455998, 9.345467776858411568, 43.12324222292260600 ) ) ;
#34041 = EDGE_CURVE ( 'NONE', #14890, #56157, #56175, .T. ) ;
#34042 = VERTEX_POINT ( 'NONE', #16180 ) ;
#34043 = LINE ( 'NONE', #19944, #18879 ) ;
#34044 = EDGE_CURVE ( 'NONE', #7116, #16048, #407, .T. ) ;
#34045 = CARTESIAN_POINT ( 'NONE',  ( 0.6028618097248862329, -47.67286800277447867, 6.452328974162811370 ) ) ;
#34046 = CARTESIAN_POINT ( 'NONE',  ( 4.833616638992208614, -26.07076047129108787, -38.20222678111930037 ) ) ;
#34047 = CARTESIAN_POINT ( 'NONE',  ( 0.6001305935487422083, 17.92615948558540495, -44.64600790884038162 ) ) ;
#34048 = CARTESIAN_POINT ( 'NONE',  ( -2.601141883200662974, 11.65089574274766981, 9.330169122851570407 ) ) ;
#34049 = AXIS2_PLACEMENT_3D ( 'NONE', #4064, #42333, #27905 ) ;
#34050 = EDGE_CURVE ( 'NONE', #19158, #5629, #55392, .T. ) ;
#34051 = CARTESIAN_POINT ( 'NONE',  ( 0.6028618097248862329, 29.14732267129573273, -38.27229381545022591 ) ) ;
#34052 = CARTESIAN_POINT ( 'NONE',  ( -6.015611763856276717, -2.453375430804198398, 18.68284711750057525 ) ) ;
#34053 = EDGE_LOOP ( 'NONE', ( #55421, #30535, #18270, #25282 ) ) ;
#34054 = CARTESIAN_POINT ( 'NONE',  ( 0.5837374860065644988, -23.79054246377998538, 41.56971235019474875 ) ) ;
#34055 = FACE_OUTER_BOUND ( 'NONE', #13512, .T. ) ;
#34056 =( BOUNDED_SURFACE ( )  B_SPLINE_SURFACE ( 3, 1, ( 
 ( #4687, #9410 ),
 ( #8799, #32311 ),
 ( #51388, #56400 ),
 ( #60790, #32623 ) ),
 .UNSPECIFIED., .F., .F., .F. ) 
 B_SPLINE_SURFACE_WITH_KNOTS ( ( 4, 4 ),
 ( 2, 2 ),
 ( 0.000000000000000000, 1.000000000000000000 ),
 ( 0.000000000000000000, 1.000000000000000000 ),
 .UNSPECIFIED. ) 
 GEOMETRIC_REPRESENTATION_ITEM ( )  RATIONAL_B_SPLINE_SURFACE ( (
 ( 1.000000000000000000, 1.000000000000000000),
 ( 0.9952954269826590483, 0.8620686068821339365),
 ( 0.9952954269826590483, 0.8620686068821339365),
 ( 1.000000000000000000, 1.000000000000000000) ) ) 
 REPRESENTATION_ITEM ( '' )  SURFACE ( )  );
#34057 = DIRECTION ( 'NONE',  ( 1.836766033387207149E-16, -1.000000000000000000, 0.000000000000000000 ) ) ;
#34058 = AXIS2_PLACEMENT_3D ( 'NONE', #45619, #26183, #26493 ) ;
#34059 = VERTEX_POINT ( 'NONE', #20566 ) ;
#34060 = CARTESIAN_POINT ( 'NONE',  ( 0.5804410086790514622, -24.77328595090333252, -39.82215658462223473 ) ) ;
#34061 = CARTESIAN_POINT ( 'NONE',  ( -4.908599999999998964, 5.921523664636232727E-15, -48.35291015139245019 ) ) ;
#34062 = CARTESIAN_POINT ( 'NONE',  ( 4.962356264823608143, -42.08379584346670299, -0.4355746408611892995 ) ) ;
#34063 = DIRECTION ( 'NONE',  ( 1.000000000000000000, 0.000000000000000000, 0.000000000000000000 ) ) ;
#34064 = CARTESIAN_POINT ( 'NONE',  ( -2.708315649062916552, -2.171184472130592624, -14.47261168455368896 ) ) ;
#34065 = ADVANCED_BREP_SHAPE_REPRESENTATION ( '', ( #31769, #14677 ), #14881 ) ;
#34066 = CARTESIAN_POINT ( 'NONE',  ( 3.678748215320120085, -23.78921895854951885, 42.80988058429586118 ) ) ;
#34067 = CARTESIAN_POINT ( 'NONE',  ( 11.99999999999999645, -8.456776945386927190E-17, -2.775557561562889872E-16 ) ) ;
#34068 = CARTESIAN_POINT ( 'NONE',  ( 5.910764540655177868, 20.06626233353475541, 1.358806252166760986 ) ) ;
#34069 = B_SPLINE_CURVE_WITH_KNOTS ( 'NONE', 3,
 ( #9703, #24420, #10333, #48846 ),
 .UNSPECIFIED., .F., .F.,
 ( 4, 4 ),
 ( 1.734723475976807094E-18, 0.004042984057420971090 ),
 .UNSPECIFIED. ) ;
#34070 = LINE ( 'NONE', #44698, #26706 ) ;
#34071 = DIRECTION ( 'NONE',  ( 0.000000000000000000, 0.000000000000000000, 1.000000000000000000 ) ) ;
#34073 = EDGE_LOOP ( 'NONE', ( #32992, #20418, #38481, #39449 ) ) ;
#34072 = CARTESIAN_POINT ( 'NONE',  ( 0.3622758884714730732, 22.26738722580116558, 36.91764744403329246 ) ) ;
#34074 = EDGE_LOOP ( 'NONE', ( #53776, #11821, #53108, #35160 ) ) ;
#34075 = CARTESIAN_POINT ( 'NONE',  ( -6.078726893082806448, 18.62537590944121391, -4.887679766589349661 ) ) ;
#34076 = CARTESIAN_POINT ( 'NONE',  ( -48.95476116535499500, 1.530808498934191127E-15, 12.50000000000000000 ) ) ;
#34077 = CARTESIAN_POINT ( 'NONE',  ( 0.6845945791218034371, 46.59746449482855724, -5.392849280958651903 ) ) ;
#34078 = EDGE_CURVE ( 'NONE', #24199, #31934, #10593, .T. ) ;
#34079 = DIRECTION ( 'NONE',  ( 3.273063162220391312E-16, -1.000000000000000000, -5.236901059552626099E-15 ) ) ;
#34080 = CARTESIAN_POINT ( 'NONE',  ( 0.1064266379913940824, 17.02047542254793555, 39.62374453032503396 ) ) ;
#34081 = CARTESIAN_POINT ( 'NONE',  ( 0.1140933569871964842, 10.18798020565364126, -42.93198119599321672 ) ) ;
#34082 =( BOUNDED_SURFACE ( )  B_SPLINE_SURFACE ( 3, 1, ( 
 ( #27447, #41570 ),
 ( #32162, #61255 ),
 ( #41267, #55321 ),
 ( #28071, #17439 ) ),
 .UNSPECIFIED., .F., .F., .F. ) 
 B_SPLINE_SURFACE_WITH_KNOTS ( ( 4, 4 ),
 ( 2, 2 ),
 ( 0.000000000000000000, 1.000000000000000000 ),
 ( 0.000000000000000000, 1.000000000000000000 ),
 .UNSPECIFIED. ) 
 GEOMETRIC_REPRESENTATION_ITEM ( )  RATIONAL_B_SPLINE_SURFACE ( (
 ( 1.000000000000000000, 1.000000000000000000),
 ( 0.7282232189291693025, 0.9929344683865674037),
 ( 0.7282232189291693025, 0.9929344683865674037),
 ( 1.000000000000000000, 1.000000000000000000) ) ) 
 REPRESENTATION_ITEM ( '' )  SURFACE ( )  );
#34083 = EDGE_CURVE ( 'NONE', #11994, #41909, #137, .T. ) ;
#34084 = ORIENTED_EDGE ( 'NONE', *, *, #42492, .T. ) ;
#34085 = B_SPLINE_CURVE_WITH_KNOTS ( 'NONE', 3,
 ( #13486, #19724, #38234, #32907 ),
 .UNSPECIFIED., .F., .F.,
 ( 4, 4 ),
 ( 7.046480070129584215E-18, 0.005013413432710147645 ),
 .UNSPECIFIED. ) ;
#34086 = CARTESIAN_POINT ( 'NONE',  ( 0.1129192098497455998, -22.45785791439690371, -37.98152716363461678 ) ) ;
#34087 = CARTESIAN_POINT ( 'NONE',  ( 0.1073791018717483448, -10.69234304550083081, 41.77800844988496465 ) ) ;
#34088 = DIRECTION ( 'NONE',  ( 0.000000000000000000, 0.000000000000000000, 1.000000000000000000 ) ) ;
#34089 = VERTEX_POINT ( 'NONE', #59066 ) ;
#34090 = CARTESIAN_POINT ( 'NONE',  ( 1.154321485836934169, -30.92445806269057940, -29.75729673892731597 ) ) ;
#34091 = CARTESIAN_POINT ( 'NONE',  ( 0.5830081025819922047, -25.46374175752871594, -39.38057757433394812 ) ) ;
#34092 = ORIENTED_EDGE ( 'NONE', *, *, #40584, .T. ) ;
#34093 = AXIS2_PLACEMENT_3D ( 'NONE', #30822, #26130, #28288 ) ;
#34094 = CYLINDRICAL_SURFACE ( 'NONE', #38029, 2.649999999999992806 ) ;
#34095 = VERTEX_POINT ( 'NONE', #40318 ) ;
#34096 = CARTESIAN_POINT ( 'NONE',  ( 2.299746137290197723, 36.48830940075291096, -32.75491741343678598 ) ) ;
#34097 = CARTESIAN_POINT ( 'NONE',  ( 0.6023142530420679819, 34.20176999054661593, 33.83147280953699010 ) ) ;
#34098 = ORIENTED_EDGE ( 'NONE', *, *, #57238, .T. ) ;
#34099 = CARTESIAN_POINT ( 'NONE',  ( 0.5800708119828337228, -24.48933355903736242, -41.16171018093183420 ) ) ;
#34100 = LINE ( 'NONE', #29370, #57596 ) ;
#34101 = CARTESIAN_POINT ( 'NONE',  ( 4.833616638992208614, -43.64812679991131716, 15.29495699393648067 ) ) ;
#34102 = CARTESIAN_POINT ( 'NONE',  ( 0.5827357941260206120, -37.77622264066033608, 29.44458568814497212 ) ) ;
#34103 = ORIENTED_EDGE ( 'NONE', *, *, #3730, .F. ) ;
#34104 = FACE_OUTER_BOUND ( 'NONE', #34120, .T. ) ;
#34105 = EDGE_CURVE ( 'NONE', #22050, #34186, #53182, .T. ) ;
#34106 = VERTEX_POINT ( 'NONE', #45015 ) ;
#34107 = PLANE ( 'NONE',  #55155 ) ;
#34109 = ADVANCED_FACE ( 'NONE', ( #53737 ), #13462, .F. ) ;
#34108 = ORIENTED_EDGE ( 'NONE', *, *, #60077, .F. ) ;
#34110 = ORIENTED_EDGE ( 'NONE', *, *, #9277, .F. ) ;
#34111 = CARTESIAN_POINT ( 'NONE',  ( 0.5809828226811617480, -47.41188724015875522, -6.791453954330822107 ) ) ;
#34112 = CARTESIAN_POINT ( 'NONE',  ( 0.6028777368367060907, -30.54986267508339637, -38.44796119230016274 ) ) ;
#34113 = EDGE_CURVE ( 'NONE', #16660, #9776, #20873, .T. ) ;
#34114 = LINE ( 'NONE', #558, #29276 ) ;
#34115 = ORIENTED_EDGE ( 'NONE', *, *, #49786, .T. ) ;
#34116 = CARTESIAN_POINT ( 'NONE',  ( 4.322998006666179727, 20.30542865297587340, 43.48102276965709478 ) ) ;
#34117 = EDGE_CURVE ( 'NONE', #18772, #58158, #39024, .T. ) ;
#34118 = LINE ( 'NONE', #25306, #23787 ) ;
#34119 = CARTESIAN_POINT ( 'NONE',  ( 0.1157506346131639274, -38.40058778857950017, 21.73328132828619630 ) ) ;
#34120 = EDGE_LOOP ( 'NONE', ( #3492, #58481, #53931, #20235 ) ) ;
#34121 = EDGE_LOOP ( 'NONE', ( #1922, #34818, #11046, #42299 ) ) ;
#34122 = CARTESIAN_POINT ( 'NONE',  ( 0.9789233960466705575, -30.99329158749494084, -28.20908724870154671 ) ) ;
#34123 = CARTESIAN_POINT ( 'NONE',  ( 0.1365634738349374988, 24.71873689235127358, 36.54923618996653545 ) ) ;
#34124 = CARTESIAN_POINT ( 'NONE',  ( 4.975610109902397937, -4.123593823331679786, -48.73854102369041641 ) ) ;
#34125 = CARTESIAN_POINT ( 'NONE',  ( 3.680882792899937694, -14.19444521819999139, -45.82784180332832591 ) ) ;
#34126 = CARTESIAN_POINT ( 'NONE',  ( 0.9722240750034587542, -26.58024222649022406, -33.68410530487897603 ) ) ;
#34127 = ORIENTED_EDGE ( 'NONE', *, *, #1408, .T. ) ;
#34128 = CARTESIAN_POINT ( 'NONE',  ( 3.376099380956838925, 0.8831717405835582957, 13.37641175011825823 ) ) ;
#34129 = EDGE_CURVE ( 'NONE', #1954, #56408, #28552, .T. ) ;
#34130 = ORIENTED_EDGE ( 'NONE', *, *, #4919, .F. ) ;
#34131 = CARTESIAN_POINT ( 'NONE',  ( 0.6031356755773454870, 12.45114731045965684, 46.46821530722343851 ) ) ;
#34132 = CARTESIAN_POINT ( 'NONE',  ( 47.98582422161447880, 15.47721683621552202, 0.8553894437622007185 ) ) ;
#34133 = CARTESIAN_POINT ( 'NONE',  ( 0.1156495703730068131, -42.64630798246201238, 11.32410564663129904 ) ) ;
#34134 = FACE_OUTER_BOUND ( 'NONE', #7493, .T. ) ;
#34135 = CARTESIAN_POINT ( 'NONE',  ( 4.549368137175248350, 32.41327393324141326, -28.14399996863463116 ) ) ;
#34136 = CARTESIAN_POINT ( 'NONE',  ( 0.3676999524040366896, -23.56959980820299094, -37.28839696479317212 ) ) ;
#34137 = VECTOR ( 'NONE', #55756, 1000.000000000000227 ) ;
#34138 = CARTESIAN_POINT ( 'NONE',  ( -6.016104459813371719, 2.454244026261361178, -18.68271063303492241 ) ) ;
#34139 = CARTESIAN_POINT ( 'NONE',  ( 2.299746137290199055, -45.91772730306088590, -17.20010630803993479 ) ) ;
#34140 = CARTESIAN_POINT ( 'NONE',  ( 0.1147471544378676628, 29.89391364686623831, 32.45467786540100263 ) ) ;
#34141 = CARTESIAN_POINT ( 'NONE',  ( 0.5998501479064708430, -48.10473956285919428, -0.5236536531313246146 ) ) ;
#34142 = DIRECTION ( 'NONE',  ( 0.07439287786467665975, -0.8569499480574984673, -0.5100024374914908787 ) ) ;
#34143 = CARTESIAN_POINT ( 'NONE',  ( -2.500000000000002220, 3.061616997868386099E-16, -5.600000000000000533 ) ) ;
#34144 = CARTESIAN_POINT ( 'NONE',  ( 0.8560838555295223751, 9.983184696771347788, -45.83349056521751663 ) ) ;
#34145 =( BOUNDED_SURFACE ( )  B_SPLINE_SURFACE ( 3, 1, ( 
 ( #25355, #44493 ),
 ( #49776, #11902 ),
 ( #1522, #20663 ),
 ( #25659, #58850 ) ),
 .UNSPECIFIED., .F., .F., .F. ) 
 B_SPLINE_SURFACE_WITH_KNOTS ( ( 4, 4 ),
 ( 2, 2 ),
 ( 0.000000000000000000, 1.000000000000000000 ),
 ( 0.000000000000000000, 1.000000000000000000 ),
 .UNSPECIFIED. ) 
 GEOMETRIC_REPRESENTATION_ITEM ( )  RATIONAL_B_SPLINE_SURFACE ( (
 ( 1.000000000000000000, 1.000000000000000000),
 ( 0.7269869731126817891, 0.9931720237060910339),
 ( 0.7269869731126817891, 0.9931720237060910339),
 ( 1.000000000000000000, 1.000000000000000000) ) ) 
 REPRESENTATION_ITEM ( '' )  SURFACE ( )  );
#34146 = EDGE_CURVE ( 'NONE', #4009, #52432, #33018, .T. ) ;
#34147 = ORIENTED_EDGE ( 'NONE', *, *, #42824, .T. ) ;
#34148 = LINE ( 'NONE', #33843, #4256 ) ;
#34149 = CARTESIAN_POINT ( 'NONE',  ( 5.896278296736517710, 16.57877312360428235, -11.38732898139155481 ) ) ;
#34150 = CARTESIAN_POINT ( 'NONE',  ( 0.5838002273316428292, 18.45474575185574295, -44.19779719735679180 ) ) ;
#34151 = CARTESIAN_POINT ( 'NONE',  ( 0.5549461598389366923, 40.10986404279688600, 18.34166028295022954 ) ) ;
#34152 = CARTESIAN_POINT ( 'NONE',  ( 5.895596859100789899, -17.30698493747188849, 10.24677781483567607 ) ) ;
#34153 = EDGE_LOOP ( 'NONE', ( #19696, #18150, #67, #442 ) ) ;
#34154 = CARTESIAN_POINT ( 'NONE',  ( 0.9752132459055851132, -37.04276540031525400, 21.65565338840803022 ) ) ;
#34155 = CARTESIAN_POINT ( 'NONE',  ( 0.8751705887134423323, -44.76769609654249393, 17.57879340691464165 ) ) ;
#34156 = CARTESIAN_POINT ( 'NONE',  ( 2.618530812446115519, -24.09540528802465076, 40.36258457041660108 ) ) ;
#34157 = ORIENTED_EDGE ( 'NONE', *, *, #55926, .F. ) ;
#34158 = DIRECTION ( 'NONE',  ( 1.000000000000000000, 0.000000000000000000, 0.000000000000000000 ) ) ;
#34159 = CARTESIAN_POINT ( 'NONE',  ( 0.9968887458511644928, -41.27232779986113798, -11.73947777183265018 ) ) ;
#34160 = VERTEX_POINT ( 'NONE', #2983 ) ;
#34161 = CARTESIAN_POINT ( 'NONE',  ( 0.5987334308729317378, -31.08900172172731402, -38.01364069010184465 ) ) ;
#34162 = ORIENTED_EDGE ( 'NONE', *, *, #16204, .T. ) ;
#34163 = CARTESIAN_POINT ( 'NONE',  ( 0.5809828226811626362, 29.58751527316234231, -37.66417181417519799 ) ) ;
#34164 = EDGE_LOOP ( 'NONE', ( #24131, #33400, #21150, #16504 ) ) ;
#34165 = CARTESIAN_POINT ( 'NONE',  ( 3.678834586032787790, 48.72167542788264427, 4.981035347034825200 ) ) ;
#34166 = CARTESIAN_POINT ( 'NONE',  ( 5.959547316686252039, -17.77749189599210311, -10.25972575517523744 ) ) ;
#34167 = EDGE_LOOP ( 'NONE', ( #54093, #52814, #42727, #46054 ) ) ;
#34168 = CARTESIAN_POINT ( 'NONE',  ( 0.8751705887134423323, -19.22545746485690188, 44.08562551107050353 ) ) ;
#34169 = B_SPLINE_CURVE_WITH_KNOTS ( 'NONE', 3,
 ( #57724, #33966, #53040, #31411, #45841, #12021 ),
 .UNSPECIFIED., .F., .F.,
 ( 4, 2, 4 ),
 ( 1.506943126379255764E-16, 0.0002445252820015211413, 0.0004890505640028915786 ),
 .UNSPECIFIED. ) ;
#34170 = ORIENTED_EDGE ( 'NONE', *, *, #19201, .F. ) ;
#34171 = DIRECTION ( 'NONE',  ( 0.000000000000000000, 0.000000000000000000, -1.000000000000000000 ) ) ;
#34172 = EDGE_CURVE ( 'NONE', #9042, #60259, #7569, .T. ) ;
#34173 = CARTESIAN_POINT ( 'NONE',  ( 1.154321713695928953, 22.16897764010656502, -36.74718012229632791 ) ) ;
#34174 = FACE_OUTER_BOUND ( 'NONE', #9209, .T. ) ;
#34175 = EDGE_CURVE ( 'NONE', #53602, #1542, #31823, .T. ) ;
#34176 = ORIENTED_EDGE ( 'NONE', *, *, #57751, .F. ) ;
#34177 = CARTESIAN_POINT ( 'NONE',  ( 5.440000000000000391, 6.831466544798160849E-15, 0.000000000000000000 ) ) ;
#34178 = CARTESIAN_POINT ( 'NONE',  ( 4.956445790443998689, -5.251077430596073903, 46.79705371022326688 ) ) ;
#34179 = CARTESIAN_POINT ( 'NONE',  ( 16.60577576646022990, -4.999999999999989342, 10.00000000000000711 ) ) ;
#34180 = CARTESIAN_POINT ( 'NONE',  ( 0.8760168074886965917, 34.63873394077487688, -33.37827814204089094 ) ) ;
#34181 = VERTEX_POINT ( 'NONE', #37461 ) ;
#34182 = EDGE_CURVE ( 'NONE', #19553, #44510, #50906, .T. ) ;
#34183 = CARTESIAN_POINT ( 'NONE',  ( 0.7044674535453004927, 27.40191655692358452, -40.75460332058581514 ) ) ;
#34184 = CARTESIAN_POINT ( 'NONE',  ( 4.549368137175248350, -38.59302160394740611, -18.79584381673521065 ) ) ;
#34185 = B_SPLINE_CURVE_WITH_KNOTS ( 'NONE', 3,
 ( #15051, #53234, #5909, #1227, #48541, #29741 ),
 .UNSPECIFIED., .F., .F.,
 ( 4, 2, 4 ),
 ( 8.651749916829332779E-17, 0.0002293366620881423013, 0.0004586733241761980833 ),
 .UNSPECIFIED. ) ;
#34186 = VERTEX_POINT ( 'NONE', #22106 ) ;
#34187 = CARTESIAN_POINT ( 'NONE',  ( 0.6064515330803599280, 46.37855968485794733, -6.954389807535533485 ) ) ;
#34188 = ORIENTED_EDGE ( 'NONE', *, *, #53744, .T. ) ;
#34189 = CARTESIAN_POINT ( 'NONE',  ( 3.783198216974388739, -36.37893817280271236, -22.99723434398829980 ) ) ;
#34190 = DIRECTION ( 'NONE',  ( -1.000000000000000000, -0.000000000000000000, -0.000000000000000000 ) ) ;
#34191 = ORIENTED_EDGE ( 'NONE', *, *, #61036, .T. ) ;
#34192 = CARTESIAN_POINT ( 'NONE',  ( 0.9790320750461907195, -12.33438343446691476, -40.05246706301296911 ) ) ;
#34193 = CARTESIAN_POINT ( 'NONE',  ( -6.078726893082806448, -19.21623043802547315, 1.237145513439503297 ) ) ;
#34194 = CARTESIAN_POINT ( 'NONE',  ( 4.549368137175248350, 13.99871866169365653, -40.58005590356676606 ) ) ;
#34195 = CARTESIAN_POINT ( 'NONE',  ( 0.8557997880470606944, -13.27832040216671317, 46.03118133706021808 ) ) ;
#34196 = EDGE_CURVE ( 'NONE', #35035, #8488, #22577, .T. ) ;
#34197 = ORIENTED_EDGE ( 'NONE', *, *, #7507, .T. ) ;
#34198 = CARTESIAN_POINT ( 'NONE',  ( 0.1158816050234198897, -40.89729701497818581, 16.56360885114767001 ) ) ;
#34199 = CARTESIAN_POINT ( 'NONE',  ( 4.553261556744875094, 35.06776520399859010, 26.45357082552112260 ) ) ;
#34200 = EDGE_CURVE ( 'NONE', #52454, #27212, #56224, .T. ) ;
#34202 = B_SPLINE_CURVE_WITH_KNOTS ( 'NONE', 3,
 ( #10400, #14489, #19494, #52673 ),
 .UNSPECIFIED., .F., .F.,
 ( 4, 4 ),
 ( 1.111881969766579830E-16, 0.005004948556313921527 ),
 .UNSPECIFIED. ) ;
#34201 = CARTESIAN_POINT ( 'NONE',  ( 0.5809828226811617480, -5.711058609464997105, -47.55412398569212939 ) ) ;
#34203 = CARTESIAN_POINT ( 'NONE',  ( 0.7048096507298579061, 0.8437160066907277711, -48.10291524268441066 ) ) ;
#34204 = CARTESIAN_POINT ( 'NONE',  ( 0.8760168074887076939, 41.20610493656909057, -24.81951362746035628 ) ) ;
#34205 = DIRECTION ( 'NONE',  ( -1.000000000000000000, -0.000000000000000000, -0.000000000000000000 ) ) ;
#34206 = CARTESIAN_POINT ( 'NONE',  ( 0.9968887458511647148, -42.62316256128687542, 4.948372828380621868 ) ) ;
#34207 = FACE_OUTER_BOUND ( 'NONE', #50649, .T. ) ;
#34208 = CARTESIAN_POINT ( 'NONE',  ( -2.739355103387248747, -6.282164585816906843, -13.54186010368313120 ) ) ;
#34209 = CARTESIAN_POINT ( 'NONE',  ( 0.9752132459055834479, 30.17566824627289890, -30.50512806189381010 ) ) ;
#34210 = CARTESIAN_POINT ( 'NONE',  ( 0.1081432562775999084, -21.92800090985295824, 37.13343246403887576 ) ) ;
#34211 = FACE_OUTER_BOUND ( 'NONE', #49231, .T. ) ;
#34212 = CIRCLE ( 'NONE', #44207, 2.698940690764988215 ) ;
#34213 = CARTESIAN_POINT ( 'NONE',  ( 0.5807400328401637335, -28.72484455891615696, -38.33001520688979724 ) ) ;
#34214 = B_SPLINE_CURVE_WITH_KNOTS ( 'NONE', 3,
 ( #14148, #38572, #5319, #24446, #39195, #43583, #33251, #47646, #8695, #27815, #32220, #19056, #41939, #23425, #46324, #46948 ),
 .UNSPECIFIED., .F., .F.,
 ( 4, 3, 3, 3, 3, 4 ),
 ( 2.221635811791082109E-17, 0.0002618515315864455005, 0.0003927756766341994007, 0.0005236998216950557216, 0.0007855159896329911998, 0.001047349442285927870 ),
 .UNSPECIFIED. ) ;
#34215 = EDGE_CURVE ( 'NONE', #21941, #14444, #9804, .T. ) ;
#34217 =( BOUNDED_SURFACE ( )  B_SPLINE_SURFACE ( 3, 1, ( 
 ( #18614, #33034 ),
 ( #37745, #56803 ),
 ( #13931, #28309 ),
 ( #4471, #23612 ) ),
 .UNSPECIFIED., .F., .F., .F. ) 
 B_SPLINE_SURFACE_WITH_KNOTS ( ( 4, 4 ),
 ( 2, 2 ),
 ( 0.000000000000000000, 1.000000000000000000 ),
 ( 0.000000000000000000, 1.000000000000000000 ),
 .UNSPECIFIED. ) 
 GEOMETRIC_REPRESENTATION_ITEM ( )  RATIONAL_B_SPLINE_SURFACE ( (
 ( 1.000000000000000000, 1.000000000000000000),
 ( 0.7282232189291693025, 0.9929344683865674037),
 ( 0.7282232189291693025, 0.9929344683865674037),
 ( 1.000000000000000000, 1.000000000000000000) ) ) 
 REPRESENTATION_ITEM ( '' )  SURFACE ( )  );
#34216 = CARTESIAN_POINT ( 'NONE',  ( 2.301430502907645170, 48.01619648598871493, 1.287492012859562163 ) ) ;
#34218 = CARTESIAN_POINT ( 'NONE',  ( 0.3622758884714600280, 17.25816669464994746, -39.50828911766980411 ) ) ;
#34219 = ORIENTED_EDGE ( 'NONE', *, *, #30885, .T. ) ;
#34220 = LINE ( 'NONE', #15731, #7850 ) ;
#34221 = DIRECTION ( 'NONE',  ( -1.000000000000000000, -0.000000000000000000, -0.000000000000000000 ) ) ;
#34222 = CARTESIAN_POINT ( 'NONE',  ( 1.231276596079887931, 38.25526645152051941, -17.14092645516095104 ) ) ;
#34223 = ORIENTED_EDGE ( 'NONE', *, *, #33170, .T. ) ;
#34224 = CARTESIAN_POINT ( 'NONE',  ( 0.3622758884714600280, 39.50828911766974016, 17.25816669465007891 ) ) ;
#34225 = CARTESIAN_POINT ( 'NONE',  ( 0.2500000000000002220, 4.898587196589412829E-16, -4.000000000000000000 ) ) ;
#34226 = B_SPLINE_CURVE_WITH_KNOTS ( 'NONE', 3,
 ( #5694, #33027, #24842, #52096, #31082, #1312 ),
 .UNSPECIFIED., .F., .F.,
 ( 4, 2, 4 ),
 ( 1.222833943671018430E-16, 0.0002448718616795911990, 0.0004897437233590601000 ),
 .UNSPECIFIED. ) ;
#34227 = PRODUCT_DEFINITION_CONTEXT ( 'detailed design', #36008, 'design' ) ;
#34228 = ORIENTED_EDGE ( 'NONE', *, *, #24059, .F. ) ;
#34229 = CARTESIAN_POINT ( 'NONE',  ( 4.962356264823603702, 30.91935898304086550, -28.55221248765493414 ) ) ;
#34230 = CARTESIAN_POINT ( 'NONE',  ( 2.643462169533613793, -13.76277278785528857, -46.02269433264228127 ) ) ;
#34231 = VERTEX_POINT ( 'NONE', #32438 ) ;
#34233 = CARTESIAN_POINT ( 'NONE',  ( 0.1073791018717483448, -40.02496097243048467, -16.05399293000801819 ) ) ;
#34232 = B_SPLINE_CURVE_WITH_KNOTS ( 'NONE', 3,
 ( #1200, #20332, #53807, #44470 ),
 .UNSPECIFIED., .F., .F.,
 ( 4, 4 ),
 ( 0.000000000000000000, 0.004048833967417087357 ),
 .UNSPECIFIED. ) ;
#34234 = ORIENTED_EDGE ( 'NONE', *, *, #16007, .F. ) ;
#34235 = ORIENTED_EDGE ( 'NONE', *, *, #25961, .T. ) ;
#34236 = CARTESIAN_POINT ( 'NONE',  ( 0.8753041380234530822, -20.68664920503281834, -44.53314352862253855 ) ) ;
#34237 = ORIENTED_EDGE ( 'NONE', *, *, #33145, .F. ) ;
#34238 = CARTESIAN_POINT ( 'NONE',  ( 4.967162193818130511, 42.34252806656603241, -7.970725651239366272 ) ) ;
#34239 = CARTESIAN_POINT ( 'NONE',  ( 0.1073791018717578927, -30.14884492832369745, -30.83464511437127697 ) ) ;
#34240 = ORIENTED_EDGE ( 'NONE', *, *, #26743, .T. ) ;
#34241 = CARTESIAN_POINT ( 'NONE',  ( 5.965394784446460541, -10.25014670152102880, -17.78272165951797490 ) ) ;
#34242 = CARTESIAN_POINT ( 'NONE',  ( 2.299652685299201860, 48.35891399284305692, -8.105378602567647306 ) ) ;
#34243 = ORIENTED_EDGE ( 'NONE', *, *, #48947, .F. ) ;
#34244 = EDGE_CURVE ( 'NONE', #43756, #32260, #38465, .T. ) ;
#34245 = VERTEX_POINT ( 'NONE', #17107 ) ;
#34246 = CARTESIAN_POINT ( 'NONE',  ( 0.5998501479064708430, -18.89267974119696447, 44.24259072156053918 ) ) ;
#34247 = CARTESIAN_POINT ( 'NONE',  ( 1.000110580585050979, 14.44681620832066216, 39.34090726222393641 ) ) ;
#34248 = CYLINDRICAL_SURFACE ( 'NONE', #49616, 10.00000000000000711 ) ;
#34249 = CARTESIAN_POINT ( 'NONE',  ( 0.5797568599927140909, -0.9380848280338333067, -46.88651517788902368 ) ) ;
#34250 = ADVANCED_FACE ( 'NONE', ( #46863 ), #26253, .F. ) ;
#34251 = ORIENTED_EDGE ( 'NONE', *, *, #11664, .T. ) ;
#34252 = FACE_OUTER_BOUND ( 'NONE', #15362, .T. ) ;
#34253 = AXIS2_PLACEMENT_3D ( 'NONE', #46025, #39785, #20955 ) ;
#34254 = CARTESIAN_POINT ( 'NONE',  ( 0.8744876279028263033, 33.66006955981258386, -35.74003032466635688 ) ) ;
#34255 = EDGE_CURVE ( 'NONE', #27042, #4984, #18812, .T. ) ;
#34256 = CARTESIAN_POINT ( 'NONE',  ( 0.6845945791218034371, -46.13320409389251608, 8.493173773401963444 ) ) ;
#34257 = CARTESIAN_POINT ( 'NONE',  ( 0.5998501479064708430, -38.48283596222049141, 28.86886762351059588 ) ) ;
#34258 = ORIENTED_EDGE ( 'NONE', *, *, #30598, .T. ) ;
#34259 = CARTESIAN_POINT ( 'NONE',  ( 2.185380717157383579, -42.93410716945229666, -9.771501656817383363 ) ) ;
#34260 = CARTESIAN_POINT ( 'NONE',  ( 0.5997462898726536595, -13.47075269803089803, -47.22383351542737984 ) ) ;
#34261 = CARTESIAN_POINT ( 'NONE',  ( 2.526552050251864134, 1.212569781798530588, -42.96196914573629755 ) ) ;
#34262 = CARTESIAN_POINT ( 'NONE',  ( 0.6064782688330851990, -35.25406363906476770, 30.92709885119426616 ) ) ;
#34263 = B_SPLINE_CURVE_WITH_KNOTS ( 'NONE', 3,
 ( #52147, #9238, #30488, #49297, #35223, #6353 ),
 .UNSPECIFIED., .F., .F.,
 ( 4, 2, 4 ),
 ( 0.000000000000000000, 0.0002447195606305754508, 0.0004894391212611509017 ),
 .UNSPECIFIED. ) ;
#34264 = ORIENTED_EDGE ( 'NONE', *, *, #50707, .T. ) ;
#34265 = ORIENTED_EDGE ( 'NONE', *, *, #33125, .T. ) ;
#34266 = CARTESIAN_POINT ( 'NONE',  ( -49.49999999999975842, 4.769696007084739620, 1.500000000000005329 ) ) ;
#34267 = CARTESIAN_POINT ( 'NONE',  ( 0.5809828226811626362, -12.92184523170236510, 46.11980934799335330 ) ) ;
#34268 = CARTESIAN_POINT ( 'NONE',  ( 0.9762797500689124330, 14.58899758184696971, -39.28722355604386252 ) ) ;
#34269 = ADVANCED_FACE ( 'NONE', ( #31500 ), #19870, .F. ) ;
#34270 = CARTESIAN_POINT ( 'NONE',  ( -6.015611763856276717, 9.416239407363303116, 16.32183393015600004 ) ) ;
#34271 = CARTESIAN_POINT ( 'NONE',  ( 1.227938101723756947, 6.439911493064564674, 42.43379953535188065 ) ) ;
#34272 = CARTESIAN_POINT ( 'NONE',  ( 0.1145239942831223490, -31.92292654912315442, 30.46099540796330274 ) ) ;
#34273 = CARTESIAN_POINT ( 'NONE',  ( 0.5807400328401574052, -29.58941477093041428, 37.66660715020855577 ) ) ;
#34274 = CARTESIAN_POINT ( 'NONE',  ( 4.975801465491695552, 36.39623109580423943, 31.15993731089136887 ) ) ;
#34275 = CARTESIAN_POINT ( 'NONE',  ( 0.8551540677456739292, -47.37911285756614888, -7.157691013574849492 ) ) ;
#34276 = DIRECTION ( 'NONE',  ( 0.000000000000000000, 0.000000000000000000, 1.000000000000000000 ) ) ;
#34277 = CARTESIAN_POINT ( 'NONE',  ( 0.9730545539215883499, -0.5054011016609686324, -42.90536227157002713 ) ) ;
#34278 = EDGE_LOOP ( 'NONE', ( #58163, #53429, #14361, #25621 ) ) ;
#34279 = CARTESIAN_POINT ( 'NONE',  ( 0.1154773475650540948, -7.219714285311297886, -43.52952280561541443 ) ) ;
#34280 = CARTESIAN_POINT ( 'NONE',  ( 0.6016117650947689910, 41.34545092125629395, 26.49725914811730121 ) ) ;
#34281 = DIRECTION ( 'NONE',  ( -1.000000000000000000, -1.836909530733573776E-16, 0.000000000000000000 ) ) ;
#34282 = CARTESIAN_POINT ( 'NONE',  ( 0.6001305935487315502, 38.48510059944048578, -28.87057754790896880 ) ) ;
#34283 = CARTESIAN_POINT ( 'NONE',  ( -6.010958268070873523, 7.224487401384534380, -17.40352239307050297 ) ) ;
#34284 = CARTESIAN_POINT ( 'NONE',  ( 0.6026777506516366456, 32.88586037763411696, -36.47007784280113185 ) ) ;
#34285 = CARTESIAN_POINT ( 'NONE',  ( -2.601141883200662974, 12.74835759521958778, 7.763685084661515745 ) ) ;
#34286 = CARTESIAN_POINT ( 'NONE',  ( 4.553261556744875094, -9.554252317234240621, -42.87488575474295516 ) ) ;
#34287 = CARTESIAN_POINT ( 'NONE',  ( 4.956445790443998689, -17.42806872899825521, 43.74700527484080936 ) ) ;
#34288 = CARTESIAN_POINT ( 'NONE',  ( 0.6001305935487315502, -12.95698906763843006, 46.33281397023041848 ) ) ;
#34289 = CARTESIAN_POINT ( 'NONE',  ( 4.975801465491695552, -43.22084481528207078, -20.67815041659126862 ) ) ;
#34291 = ORIENTED_EDGE ( 'NONE', *, *, #38868, .F. ) ;
#34290 = CARTESIAN_POINT ( 'NONE',  ( 3.376099380956838925, 7.576724406378373189, 11.05900677736737237 ) ) ;
#34292 = VERTEX_POINT ( 'NONE', #23649 ) ;
#34293 = CARTESIAN_POINT ( 'NONE',  ( 0.5797568665920705966, -24.70127861128346325, 39.86316775633390819 ) ) ;
#34294 = DIRECTION ( 'NONE',  ( -1.000000000000000000, -0.000000000000000000, -0.000000000000000000 ) ) ;
#34295 = CARTESIAN_POINT ( 'NONE',  ( 4.553261556744875094, 1.182159483579356074, 43.91061448874314976 ) ) ;
#34296 = EDGE_CURVE ( 'NONE', #47270, #3479, #10169, .T. ) ;
#34297 = ORIENTED_EDGE ( 'NONE', *, *, #48568, .F. ) ;
#34298 = CARTESIAN_POINT ( 'NONE',  ( 0.1100053167205931187, -10.98799238780980225, 41.70112744323650134 ) ) ;
#34299 = CARTESIAN_POINT ( 'NONE',  ( 0.3622758884714730732, -4.808133778522197588, 42.84426538328723666 ) ) ;
#34301 = B_SPLINE_CURVE_WITH_KNOTS ( 'NONE', 3,
 ( #35780, #21354, #44880, #26053, #1920, #55464 ),
 .UNSPECIFIED., .F., .F.,
 ( 4, 2, 4 ),
 ( 1.867170871510376464E-17, 0.0002293755540694311830, 0.0004587511081388436635 ),
 .UNSPECIFIED. ) ;
#34300 = CARTESIAN_POINT ( 'NONE',  ( 0.5782707292762442330, 45.42077932512039951, -11.69141390963183902 ) ) ;
#34302 = VECTOR ( 'NONE', #27652, 1000.000000000000000 ) ;
#34303 = EDGE_CURVE ( 'NONE', #10899, #9817, #46440, .T. ) ;
#34304 = EDGE_LOOP ( 'NONE', ( #38725, #912, #21902, #55728 ) ) ;
#34305 = ORIENTED_EDGE ( 'NONE', *, *, #38146, .T. ) ;
#34306 = CARTESIAN_POINT ( 'NONE',  ( -6.072942160501519915, -18.90394509709858539, -3.666745430883196377 ) ) ;
#34307 = CARTESIAN_POINT ( 'NONE',  ( 4.553261556744873317, -43.15908619232978083, -8.175135770535248980 ) ) ;
#34308 = ADVANCED_FACE ( 'NONE', ( #10478 ), #38722, .F. ) ;
#34309 = CARTESIAN_POINT ( 'NONE',  ( 1.000433927950264534, 36.39033293409891456, 20.78851477615176435 ) ) ;
#34310 = CARTESIAN_POINT ( 'NONE',  ( 4.956653778116975495, -20.77844580450591394, 43.37017594958047084 ) ) ;
#34311 = CARTESIAN_POINT ( 'NONE',  ( 0.1119898979215349505, -44.12081468618291069, 0.5612661394878653009 ) ) ;
#34312 = CARTESIAN_POINT ( 'NONE',  ( 2.281448460670567613, 13.68109378871710469, 45.98107640562100329 ) ) ;
#34313 = CARTESIAN_POINT ( 'NONE',  ( 0.6000166863083106206, 40.87138819217380359, -27.22780029589406681 ) ) ;
#34314 =( BOUNDED_SURFACE ( )  B_SPLINE_SURFACE ( 3, 1, ( 
 ( #57031, #52023 ),
 ( #10058, #28528 ),
 ( #14156, #19163 ),
 ( #47651, #23228 ) ),
 .UNSPECIFIED., .F., .F., .F. ) 
 B_SPLINE_SURFACE_WITH_KNOTS ( ( 4, 4 ),
 ( 2, 2 ),
 ( 0.000000000000000000, 1.000000000000000000 ),
 ( 0.000000000000000000, 1.000000000000000000 ),
 .UNSPECIFIED. ) 
 GEOMETRIC_REPRESENTATION_ITEM ( )  RATIONAL_B_SPLINE_SURFACE ( (
 ( 1.000000000000000000, 1.000000000000000000),
 ( 0.9729067724841187204, 0.9999501103223794596),
 ( 0.9729067724841187204, 0.9999501103223794596),
 ( 1.000000000000000000, 1.000000000000000000) ) ) 
 REPRESENTATION_ITEM ( '' )  SURFACE ( )  );
#34315 = VECTOR ( 'NONE', #29737, 999.9999999999998863 ) ;
#34316 = CARTESIAN_POINT ( 'NONE',  ( 0.5839879327111915375, 37.94312859586454323, -29.22928252017475970 ) ) ;
#34317 = VERTEX_POINT ( 'NONE', #24886 ) ;
#34318 = EDGE_CURVE ( 'NONE', #31692, #1874, #14269, .T. ) ;
#34319 = ORIENTED_EDGE ( 'NONE', *, *, #4210, .T. ) ;
#34320 = CARTESIAN_POINT ( 'NONE',  ( 1.227938101723748288, 11.92353943228006585, -41.23019537246697297 ) ) ;
#34321 = CARTESIAN_POINT ( 'NONE',  ( 4.962356264823601926, -42.08379584346671720, 0.4355746408606013254 ) ) ;
#34322 = ORIENTED_EDGE ( 'NONE', *, *, #11907, .T. ) ;
#34323 = DIRECTION ( 'NONE',  ( 0.000000000000000000, 0.000000000000000000, 1.000000000000000000 ) ) ;
#34324 = CARTESIAN_POINT ( 'NONE',  ( -6.072942160501519027, 17.84350912780779197, 7.239706091745748751 ) ) ;
#34325 = CARTESIAN_POINT ( 'NONE',  ( 4.291220156522060236, 34.26497439135391687, 32.33110773335113208 ) ) ;
#34326 = CARTESIAN_POINT ( 'NONE',  ( 0.1073791018717578927, -42.81622261970997556, 5.147744207006151207 ) ) ;
#34327 = B_SPLINE_CURVE_WITH_KNOTS ( 'NONE', 3,
 ( #3248, #40285, #59337, #40586 ),
 .UNSPECIFIED., .F., .F.,
 ( 4, 4 ),
 ( 1.734723475976807094E-18, 0.004042984057420972825 ),
 .UNSPECIFIED. ) ;
#34328 = ORIENTED_EDGE ( 'NONE', *, *, #13780, .F. ) ;
#34329 = CARTESIAN_POINT ( 'NONE',  ( 0.5837800005270565862, 46.47757032468152971, -6.250657193932968703 ) ) ;
#34330 = CARTESIAN_POINT ( 'NONE',  ( 4.967162193818130511, -28.74031574029989855, -32.10009971360102554 ) ) ;
#34331 = B_SPLINE_CURVE_WITH_KNOTS ( 'NONE', 3,
 ( #37330, #7313, #13212, #11750, #42646, #27607 ),
 .UNSPECIFIED., .F., .F.,
 ( 4, 2, 4 ),
 ( 7.040638946443416885E-18, 0.0002445244328975362097, 0.0004890488657950653722 ),
 .UNSPECIFIED. ) ;
#34332 = EDGE_CURVE ( 'NONE', #41577, #6162, #1575, .T. ) ;
#34333 = CARTESIAN_POINT ( 'NONE',  ( 4.962356264823608143, -14.71877352713578269, -39.42833123173278409 ) ) ;
#34334 =( BOUNDED_SURFACE ( )  B_SPLINE_SURFACE ( 3, 1, ( 
 ( #57898, #61363 ),
 ( #584, #23476 ),
 ( #47919, #19718 ),
 ( #38844, #47292 ) ),
 .UNSPECIFIED., .F., .F., .F. ) 
 B_SPLINE_SURFACE_WITH_KNOTS ( ( 4, 4 ),
 ( 2, 2 ),
 ( 0.000000000000000000, 1.000000000000000000 ),
 ( 0.000000000000000000, 1.000000000000000000 ),
 .UNSPECIFIED. ) 
 GEOMETRIC_REPRESENTATION_ITEM ( )  RATIONAL_B_SPLINE_SURFACE ( (
 ( 1.000000000000000000, 1.000000000000000000),
 ( 0.7269869731126821222, 0.9931720237060910339),
 ( 0.7269869731126821222, 0.9931720237060910339),
 ( 1.000000000000000000, 1.000000000000000000) ) ) 
 REPRESENTATION_ITEM ( '' )  SURFACE ( )  );
#34335 = DIRECTION ( 'NONE',  ( -0.07836865515943411409, -0.9893941468723549404, -0.1223011693452953769 ) ) ;
#34336 = ORIENTED_EDGE ( 'NONE', *, *, #17358, .T. ) ;
#34337 = ORIENTED_EDGE ( 'NONE', *, *, #14457, .T. ) ;
#34338 = CARTESIAN_POINT ( 'NONE',  ( 4.322998006666165516, 45.75942687572278800, 14.45630056002956110 ) ) ;
#34339 = CARTESIAN_POINT ( 'NONE',  ( 0.1140933569871965120, 9.448435536941939716, 43.10077744064668792 ) ) ;
#34340 = VERTEX_POINT ( 'NONE', #18973 ) ;
#34341 = CARTESIAN_POINT ( 'NONE',  ( 0.1310142868023699003, 39.59283406808307149, 17.08943085418600916 ) ) ;
#34342 = LINE ( 'NONE', #48425, #45709 ) ;
#34343 = CARTESIAN_POINT ( 'NONE',  ( 2.624215991343608501, 47.76052319582223049, -4.864192649744909502 ) ) ;
#34344 = EDGE_CURVE ( 'NONE', #14306, #43794, #44472, .T. ) ;
#34345 = AXIS2_PLACEMENT_3D ( 'NONE', #59152, #16261, #35385 ) ;
#34346 = CARTESIAN_POINT ( 'NONE',  ( 4.335381028904216727, 48.97680438974856543, 1.014632658971305945 ) ) ;
#34347 = CARTESIAN_POINT ( 'NONE',  ( 5.901463166500146684, -7.215136289071354625, 18.77390952014955872 ) ) ;
#34348 = CARTESIAN_POINT ( 'NONE',  ( 0.7413678028165009426, 21.21902926989227822, 38.65538628203963611 ) ) ;
#34349 = CARTESIAN_POINT ( 'NONE',  ( 0.3622758884714730732, -20.83792692158999316, 37.74294673546550172 ) ) ;
#34350 = DIRECTION ( 'NONE',  ( 1.000000000000000000, 0.000000000000000000, 0.000000000000000000 ) ) ;
#34351 = VERTEX_POINT ( 'NONE', #14575 ) ;
#34352 = CARTESIAN_POINT ( 'NONE',  ( 0.9757402383260935785, 39.67468066200785870, -16.34189654378392120 ) ) ;
#34353 = CARTESIAN_POINT ( 'NONE',  ( 0.9790320750461911636, 41.52319970619036837, 5.671068567917366465 ) ) ;
#34354 = CARTESIAN_POINT ( 'NONE',  ( 2.359973842542475886, -16.42991230730133267, 40.84352918403218524 ) ) ;
#34355 = ORIENTED_EDGE ( 'NONE', *, *, #41951, .F. ) ;
#34356 = B_SPLINE_CURVE_WITH_KNOTS ( 'NONE', 3,
 ( #3721, #56660, #52579, #9673, #61054, #56968 ),
 .UNSPECIFIED., .F., .F.,
 ( 4, 2, 4 ),
 ( 1.265936389305167544E-16, 0.0002450741128632346190, 0.0004901482257263427116 ),
 .UNSPECIFIED. ) ;
#34357 = FACE_OUTER_BOUND ( 'NONE', #46495, .T. ) ;
#34358 = CARTESIAN_POINT ( 'NONE',  ( 1.157643937452369043, 32.37803415880393487, -26.62076592823879650 ) ) ;
#34359 = CARTESIAN_POINT ( 'NONE',  ( 1.140000000000008784, 0.000000000000000000, -5.633200000000004870 ) ) ;
#34360 = CARTESIAN_POINT ( 'NONE',  ( 0.8760168074886965917, 17.58183840866335856, 44.77533136581888584 ) ) ;
#34361 = AXIS2_PLACEMENT_3D ( 'NONE', #44405, #10552, #29649 ) ;
#34362 = CARTESIAN_POINT ( 'NONE',  ( 5.895596859100789899, -13.97974974393973291, 14.46010996878324129 ) ) ;
#34363 = CARTESIAN_POINT ( 'NONE',  ( 0.6031357023905875581, 38.19275261685275069, -29.25135304925241186 ) ) ;
#34364 = DIRECTION ( 'NONE',  ( 1.000000000000000000, 0.000000000000000000, 0.000000000000000000 ) ) ;
#34365 = CARTESIAN_POINT ( 'NONE',  ( 0.6254311100348624031, 17.77188277739556455, 44.70341307176162360 ) ) ;
#34366 = DIRECTION ( 'NONE',  ( 0.000000000000000000, 0.000000000000000000, -1.000000000000000000 ) ) ;
#34367 = CARTESIAN_POINT ( 'NONE',  ( 4.967162193818130511, 38.44485641567099776, -19.45289607368781759 ) ) ;
#34369 = ORIENTED_EDGE ( 'NONE', *, *, #57354, .F. ) ;
#34368 = CARTESIAN_POINT ( 'NONE',  ( 0.3622758884714730732, -33.69533458712361806, 26.89560658783328861 ) ) ;
#34370 = ORIENTED_EDGE ( 'NONE', *, *, #25870, .F. ) ;
#34371 = CARTESIAN_POINT ( 'NONE',  ( 0.5839880159502356394, -12.44022138820718126, 46.25220722086343272 ) ) ;
#34372 = CARTESIAN_POINT ( 'NONE',  ( 0.6001305935487315502, 0.5236757026882711274, 48.10757715638249010 ) ) ;
#34373 = CARTESIAN_POINT ( 'NONE',  ( 0.5807400328401574052, 38.33001520688949881, 28.72484455891654420 ) ) ;
#34374 = ADVANCED_FACE ( 'NONE', ( #57753 ), #37995, .F. ) ;
#34375 = LINE ( 'NONE', #6431, #33527 ) ;
#34376 = DIRECTION ( 'NONE',  ( 0.000000000000000000, 0.000000000000000000, 1.000000000000000000 ) ) ;
#34377 = CARTESIAN_POINT ( 'NONE',  ( 0.7954190325252784577, 11.60747917225584835, -46.67728753507131501 ) ) ;
#34378 = EDGE_CURVE ( 'NONE', #34651, #23287, #23306, .T. ) ;
#34379 = ORIENTED_EDGE ( 'NONE', *, *, #20742, .T. ) ;
#34380 = ORIENTED_EDGE ( 'NONE', *, *, #37118, .T. ) ;
#34381 = FACE_OUTER_BOUND ( 'NONE', #710, .T. ) ;
#34382 = EDGE_CURVE ( 'NONE', #10602, #20520, #38089, .T. ) ;
#34383 = B_SPLINE_CURVE_WITH_KNOTS ( 'NONE', 3,
 ( #38878, #57931, #48549, #4998 ),
 .UNSPECIFIED., .F., .F.,
 ( 4, 4 ),
 ( 1.028564492747080581E-18, 0.004444878191957681718 ),
 .UNSPECIFIED. ) ;
#34384 = CARTESIAN_POINT ( 'NONE',  ( 0.8744876279028263033, 48.35212675551510841, -8.510105087370661181 ) ) ;
#34385 = EDGE_CURVE ( 'NONE', #4231, #54025, #6068, .T. ) ;
#34386 = ORIENTED_EDGE ( 'NONE', *, *, #20922, .T. ) ;
#34387 = VECTOR ( 'NONE', #55269, 1000.000000000000114 ) ;
#34388 = CARTESIAN_POINT ( 'NONE',  ( 4.833616638992208614, 25.31740731790898735, -38.70560126501837317 ) ) ;
#34389 = CARTESIAN_POINT ( 'NONE',  ( 0.5837800304671217910, -25.19555850426963417, -39.55276430083521433 ) ) ;
#34390 = ORIENTED_EDGE ( 'NONE', *, *, #17195, .F. ) ;
#34391 = EDGE_CURVE ( 'NONE', #23436, #41057, #32296, .T. ) ;
#34392 = CARTESIAN_POINT ( 'NONE',  ( 3.680882792899938138, 45.82784180332838275, -14.19444521819982796 ) ) ;
#34393 = VERTEX_POINT ( 'NONE', #28963 ) ;
#34394 = EDGE_CURVE ( 'NONE', #29077, #7813, #46463, .T. ) ;
#34395 = CARTESIAN_POINT ( 'NONE',  ( 0.5835871038041858805, -34.87197729266512169, 31.35569569633796405 ) ) ;
#34396 = CARTESIAN_POINT ( 'NONE',  ( 0.7048096507298579061, -19.18768066167151432, 44.11842270945940214 ) ) ;
#34397 = VERTEX_POINT ( 'NONE', #34597 ) ;
#34398 = CYLINDRICAL_SURFACE ( 'NONE', #54480, 2.649999999999992806 ) ;
#34399 = CARTESIAN_POINT ( 'NONE',  ( 2.618530812446111078, 46.98662296661650828, 1.408563591474228938 ) ) ;
#34400 = CARTESIAN_POINT ( 'NONE',  ( 0.8751705887134423323, 17.57879340691479797, 44.76769609654243709 ) ) ;
#34401 = CARTESIAN_POINT ( 'NONE',  ( 0.7242003506639993482, 28.75993203985512636, 39.79796456087851197 ) ) ;
#34402 = CIRCLE ( 'NONE', #33425, 6.887500000000022382 ) ;
#34403 = B_SPLINE_CURVE_WITH_KNOTS ( 'NONE', 3,
 ( #49109, #1170, #58790, #15914 ),
 .UNSPECIFIED., .F., .F.,
 ( 4, 4 ),
 ( 0.000000000000000000, 0.005004948556313788821 ),
 .UNSPECIFIED. ) ;
#34404 = ORIENTED_EDGE ( 'NONE', *, *, #128, .F. ) ;
#34405 = CARTESIAN_POINT ( 'NONE',  ( 3.238018933889920792, -5.387504234938196745, -12.26304572633470791 ) ) ;
#34406 = CARTESIAN_POINT ( 'NONE',  ( 0.6031356755852232965, 5.421189728766411748E-15, -48.10744332413860747 ) ) ;
#34407 = ORIENTED_EDGE ( 'NONE', *, *, #50208, .T. ) ;
#34408 = CARTESIAN_POINT ( 'NONE',  ( 4.549368137175248350, -24.02461520945246320, -35.57418903283107880 ) ) ;
#34409 = EDGE_LOOP ( 'NONE', ( #58078, #18841, #33303, #18059 ) ) ;
#34410 = CARTESIAN_POINT ( 'NONE',  ( 5.959828726073459926, -14.51059719297126627, 14.51699876360174812 ) ) ;
#34411 = ORIENTED_EDGE ( 'NONE', *, *, #26170, .F. ) ;
#34412 = CARTESIAN_POINT ( 'NONE',  ( 4.956653778116949738, -36.51451553856396970, -31.29546495791881000 ) ) ;
#34413 = CARTESIAN_POINT ( 'NONE',  ( 0.9790850452238872847, 36.03246141061279673, -21.40091247951577813 ) ) ;
#34414 = CARTESIAN_POINT ( 'NONE',  ( 0.8751705887134553219, -42.09020928323357680, -23.27176129838411001 ) ) ;
#34415 = EDGE_LOOP ( 'NONE', ( #61404, #52155, #57403, #37503 ) ) ;
#34416 = CARTESIAN_POINT ( 'NONE',  ( 0.5809828226811617480, 5.711058609465307967, 47.55412398569209387 ) ) ;
#34417 = CARTESIAN_POINT ( 'NONE',  ( 0.5834872094924170582, -6.476680342366908150, 47.45604551759235079 ) ) ;
#34418 = CARTESIAN_POINT ( 'NONE',  ( 0.1119899015040009826, -27.94769331548668845, 34.14509842621640701 ) ) ;
#34420 = VERTEX_POINT ( 'NONE', #53977 ) ;
#34419 = EDGE_CURVE ( 'NONE', #18115, #3927, #43522, .T. ) ;
#34421 = B_SPLINE_CURVE_WITH_KNOTS ( 'NONE', 3,
 ( #17321, #24098, #42921, #14407 ),
 .UNSPECIFIED., .F., .F.,
 ( 4, 4 ),
 ( 0.000000000000000000, 0.004446090762761357312 ),
 .UNSPECIFIED. ) ;
#34422 = ORIENTED_EDGE ( 'NONE', *, *, #15470, .F. ) ;
#34423 = CARTESIAN_POINT ( 'NONE',  ( 0.9790850452238869517, -31.11560338686072669, -28.07412609743672860 ) ) ;
#34425 = ADVANCED_FACE ( 'NONE', ( #6974 ), #49121, .F. ) ;
#34424 = CARTESIAN_POINT ( 'NONE',  ( 1.827119703190779321, 9.946884032291105626, -41.88501940447984850 ) ) ;
#34426 = PRODUCT ( 'hex nut gradec_iso_ISO - 4034 - M5 - N', 'hex nut gradec_iso_ISO - 4034 - M5 - N', '', ( #3276 ) ) ;
#34427 = CARTESIAN_POINT ( 'NONE',  ( 4.549368137175248350, 0.000000000000000000, 0.000000000000000000 ) ) ;
#34428 = DIRECTION ( 'NONE',  ( 0.000000000000000000, 0.000000000000000000, 1.000000000000000000 ) ) ;
#34429 = LINE ( 'NONE', #53798, #55803 ) ;
#34430 = ORIENTED_EDGE ( 'NONE', *, *, #4309, .T. ) ;
#34431 = CARTESIAN_POINT ( 'NONE',  ( 4.956445790444004018, -43.56224489968086999, -17.88487823385623443 ) ) ;
#34432 = ORIENTED_EDGE ( 'NONE', *, *, #33058, .T. ) ;
#34433 = CARTESIAN_POINT ( 'NONE',  ( 0.6031357023905875581, 12.40899271757774081, 46.47951061918815441 ) ) ;
#34434 = CARTESIAN_POINT ( 'NONE',  ( 47.85000000000000853, 15.50000000000000711, 1.598617397282144235E-15 ) ) ;
#34435 = CARTESIAN_POINT ( 'NONE',  ( -6.001507490154110336, -17.41542759839258991, -7.196845540359352533 ) ) ;
#34436 = B_SPLINE_CURVE_WITH_KNOTS ( 'NONE', 3,
 ( #28494, #23814, #42942, #22962, #56384, #32603 ),
 .UNSPECIFIED., .F., .F.,
 ( 4, 2, 4 ),
 ( 1.889500315511339631E-17, 0.0002448709889506574277, 0.0004897419779012958819 ),
 .UNSPECIFIED. ) ;
#34437 = CONICAL_SURFACE ( 'NONE', #30380, 47.91270532121795611, 0.04450589592585343229 ) ;
#34438 = CARTESIAN_POINT ( 'NONE',  ( -6.077587904424778920, -4.278847002849007097, -18.77465018902190863 ) ) ;
#34439 = CARTESIAN_POINT ( 'NONE',  ( 4.999999999999986677, 58.44237546506882808, -54.69470952477875159 ) ) ;
#34440 = CARTESIAN_POINT ( 'NONE',  ( 5.896278296736517710, -13.98624301437808448, -14.45378794493484520 ) ) ;
#34441 = CARTESIAN_POINT ( 'NONE',  ( -6.015611763856276717, 2.453375430804336954, -18.68284711750055749 ) ) ;
#34442 = CARTESIAN_POINT ( 'NONE',  ( 4.975610109902397937, 48.58133226360784818, -5.683622315980244366 ) ) ;
#34443 = FACE_OUTER_BOUND ( 'NONE', #33501, .T. ) ;
#34444 = CARTESIAN_POINT ( 'NONE',  ( 0.3676999524040366896, -2.238562284875889041, -44.05609404179596567 ) ) ;
#34445 = CARTESIAN_POINT ( 'NONE',  ( 4.975801465491694664, -39.51822597168476392, -27.09127437476367106 ) ) ;
#34446 = EDGE_CURVE ( 'NONE', #41967, #20220, #27074, .T. ) ;
#34447 = CARTESIAN_POINT ( 'NONE',  ( 0.9769922540276052558, -34.79934705825704100, 23.35245167868034244 ) ) ;
#34448 = AXIS2_PLACEMENT_3D ( 'NONE', #18867, #13234, #61423 ) ;
#34449 = CARTESIAN_POINT ( 'NONE',  ( 5.959828726073459926, 20.52560994243598813, -0.004526594003165452379 ) ) ;
#34450 = EDGE_CURVE ( 'NONE', #4022, #27996, #29287, .T. ) ;
#34451 = EDGE_LOOP ( 'NONE', ( #8395, #10905, #45145, #56459 ) ) ;
#34452 = CARTESIAN_POINT ( 'NONE',  ( 4.549368137175248350, -42.82045902618774136, 3.018832571115817487 ) ) ;
#34453 = ADVANCED_FACE ( 'NONE', ( #21103 ), #3410, .T. ) ;
#34454 = EDGE_CURVE ( 'NONE', #15076, #57080, #4628, .T. ) ;
#34455 = DIRECTION ( 'NONE',  ( 0.000000000000000000, 0.000000000000000000, 1.000000000000000000 ) ) ;
#34456 = CARTESIAN_POINT ( 'NONE',  ( 0.7413678028165009426, 24.45722514617033383, -36.69237291208864349 ) ) ;
#34457 = CARTESIAN_POINT ( 'NONE',  ( 0.3622758884714730732, -29.89648521331652731, 31.06363466427676201 ) ) ;
#34458 = CARTESIAN_POINT ( 'NONE',  ( 0.8554163680231720024, 46.61139063278402972, 5.346376005279848798 ) ) ;
#34459 = EDGE_CURVE ( 'NONE', #54112, #17050, #26291, .T. ) ;
#34460 = ORIENTED_EDGE ( 'NONE', *, *, #18696, .F. ) ;
#34461 = CARTESIAN_POINT ( 'NONE',  ( 4.962356264823608143, 0.000000000000000000, 0.000000000000000000 ) ) ;
#34462 = CARTESIAN_POINT ( 'NONE',  ( 0.9730545539215883499, 15.95224156741883270, -39.83279466599022811 ) ) ;
#34463 = APPLICATION_CONTEXT ( 'automotive_design' ) ;
#34464 = CARTESIAN_POINT ( 'NONE',  ( 0.9762797500689124330, 38.38274741215467145, 16.82526333465357382 ) ) ;
#34465 = ORIENTED_EDGE ( 'NONE', *, *, #14479, .T. ) ;
#34466 = DIRECTION ( 'NONE',  ( 0.000000000000000000, 0.000000000000000000, -1.000000000000000000 ) ) ;
#34467 = EDGE_CURVE ( 'NONE', #46849, #56041, #60673, .T. ) ;
#34468 = CARTESIAN_POINT ( 'NONE',  ( 3.376099380956838925, -11.75009321188407618, -6.453192476914276554 ) ) ;
#34469 = ORIENTED_EDGE ( 'NONE', *, *, #25957, .T. ) ;
#34470 = CARTESIAN_POINT ( 'NONE',  ( 0.1129192098497455998, 41.72114954716776936, 14.36305915353748297 ) ) ;
#34471 = ORIENTED_EDGE ( 'NONE', *, *, #51958, .F. ) ;
#34472 = CARTESIAN_POINT ( 'NONE',  ( 3.514385190458181096, -13.03453477240704039, 0.000000000000000000 ) ) ;
#34473 = ORIENTED_EDGE ( 'NONE', *, *, #46215, .F. ) ;
#34474 = CARTESIAN_POINT ( 'NONE',  ( 0.1119898979215347701, -13.09165672777951883, -42.13751098930518424 ) ) ;
#34475 = CARTESIAN_POINT ( 'NONE',  ( 0.6001305935487315502, 24.50730504006400068, 41.40054608060301433 ) ) ;
#34476 = VERTEX_POINT ( 'NONE', #22650 ) ;
#34477 = DIRECTION ( 'NONE',  ( -1.558861125776144859E-16, 1.000000000000000000, 0.000000000000000000 ) ) ;
#34478 = ORIENTED_EDGE ( 'NONE', *, *, #2961, .F. ) ;
#34479 = DIRECTION ( 'NONE',  ( 1.000000000000000000, 0.000000000000000000, 0.000000000000000000 ) ) ;
#34480 = CIRCLE ( 'NONE', #35471, 15.99999999999999645 ) ;
#34481 = ORIENTED_EDGE ( 'NONE', *, *, #19225, .F. ) ;
#34482 = CARTESIAN_POINT ( 'NONE',  ( 0.5804410086790514622, -38.35366574781983218, -26.99103880105228370 ) ) ;
#34483 = DIRECTION ( 'NONE',  ( 0.000000000000000000, 0.000000000000000000, -1.000000000000000000 ) ) ;
#34484 = B_SPLINE_CURVE_WITH_KNOTS ( 'NONE', 3,
 ( #7135, #26262, #45400, #3364, #2447, #21573 ),
 .UNSPECIFIED., .F., .F.,
 ( 4, 2, 4 ),
 ( 1.734723475976807094E-18, 0.0002447193893791696538, 0.0004894387787583375730 ),
 .UNSPECIFIED. ) ;
#34485 = CARTESIAN_POINT ( 'NONE',  ( 0.2940135542859031448, -32.24540453331401579, -30.10771388156783601 ) ) ;
#34486 = CARTESIAN_POINT ( 'NONE',  ( 0.6001305935487315502, 34.38748867424713751, -33.64689939321905854 ) ) ;
#34487 = VERTEX_POINT ( 'NONE', #26412 ) ;
#34488 = LINE ( 'NONE', #6867, #61759 ) ;
#34489 = CARTESIAN_POINT ( 'NONE',  ( -6.015611763856276717, 16.31561949997088945, -9.427003116184000220 ) ) ;
#34490 = VECTOR ( 'NONE', #10527, 1000.000000000000000 ) ;
#34491 = EDGE_LOOP ( 'NONE', ( #40016, #200, #54920, #43421 ) ) ;
#34492 = CARTESIAN_POINT ( 'NONE',  ( 4.909518593422035337, 0.8656805902944597619, 8.896908036367455278E-17 ) ) ;
#34493 = B_SPLINE_CURVE_WITH_KNOTS ( 'NONE', 3,
 ( #57920, #14972, #7454, #54142, #16903, #59469 ),
 .UNSPECIFIED., .F., .F.,
 ( 4, 2, 4 ),
 ( 3.529906531158615134E-18, 0.0002445244328975414139, 0.0004890488657950793584 ),
 .UNSPECIFIED. ) ;
#34494 = ORIENTED_EDGE ( 'NONE', *, *, #38642, .F. ) ;
#34495 = CARTESIAN_POINT ( 'NONE',  ( -2.739355103387247858, 14.87824819718636782, 1.218727834234354157 ) ) ;
#34496 = EDGE_CURVE ( 'NONE', #55928, #28003, #3864, .T. ) ;
#34497 = CARTESIAN_POINT ( 'NONE',  ( 0.5807400328401637335, 0.5448834511089987176, 47.89582301953903709 ) ) ;
#34498 = ORIENTED_EDGE ( 'NONE', *, *, #58759, .T. ) ;
#34499 = CARTESIAN_POINT ( 'NONE',  ( 4.549368137175248350, 0.000000000000000000, 0.000000000000000000 ) ) ;
#34500 = CARTESIAN_POINT ( 'NONE',  ( 4.960386119450145515, -26.33153931528478608, -34.94404816216851373 ) ) ;
#34501 = DIRECTION ( 'NONE',  ( 0.000000000000000000, 0.000000000000000000, 1.000000000000000000 ) ) ;
#34502 = DIRECTION ( 'NONE',  ( 1.000000000000000000, 0.000000000000000000, 0.000000000000000000 ) ) ;
#34503 = VERTEX_POINT ( 'NONE', #60222 ) ;
#34504 = CARTESIAN_POINT ( 'NONE',  ( 5.896782393890504181, 0.6784186533438157918, 20.10138888258240186 ) ) ;
#34505 = LINE ( 'NONE', #29789, #39824 ) ;
#34506 = CARTESIAN_POINT ( 'NONE',  ( 0.5827357941260211671, -44.10984861950467462, 18.66407988912473925 ) ) ;
#34507 = CARTESIAN_POINT ( 'NONE',  ( 5.917102823773431552, 17.94639498788077248, -9.078360258918451109 ) ) ;
#34508 =( BOUNDED_SURFACE ( )  B_SPLINE_SURFACE ( 3, 1, ( 
 ( #36143, #23257 ),
 ( #42085, #31735 ),
 ( #8216, #42384 ),
 ( #32355, #61437 ) ),
 .UNSPECIFIED., .F., .F., .F. ) 
 B_SPLINE_SURFACE_WITH_KNOTS ( ( 4, 4 ),
 ( 2, 2 ),
 ( 0.000000000000000000, 1.000000000000000000 ),
 ( 0.000000000000000000, 1.000000000000000000 ),
 .UNSPECIFIED. ) 
 GEOMETRIC_REPRESENTATION_ITEM ( )  RATIONAL_B_SPLINE_SURFACE ( (
 ( 1.000000000000000000, 1.000000000000000000),
 ( 0.7211978278499968642, 0.9934217856018975334),
 ( 0.7211978278499968642, 0.9934217856018975334),
 ( 1.000000000000000000, 1.000000000000000000) ) ) 
 REPRESENTATION_ITEM ( '' )  SURFACE ( )  );
#34509 = CIRCLE ( 'NONE', #61475, 15.43999999999999240 ) ;
#34510 = DIRECTION ( 'NONE',  ( 1.000000000000000000, 0.000000000000000000, 0.000000000000000000 ) ) ;
#34511 = CARTESIAN_POINT ( 'NONE',  ( 0.5980271706414734822, -47.67913160907356485, -11.77920421107915949 ) ) ;
#34512 = CARTESIAN_POINT ( 'NONE',  ( 5.860006189529234355, -3.137522369585849624, 48.13093674595583593 ) ) ;
#34513 = DIRECTION ( 'NONE',  ( -1.000000000000000000, -0.000000000000000000, -0.000000000000000000 ) ) ;
#34514 = ADVANCED_FACE ( 'NONE', ( #60531 ), #41461, .F. ) ;
#34515 = DIRECTION ( 'NONE',  ( 0.000000000000000000, 0.000000000000000000, 1.000000000000000000 ) ) ;
#34516 = CARTESIAN_POINT ( 'NONE',  ( 0.1157506346131639274, -43.77365856608008698, -5.550448229024145697 ) ) ;
#34517 = CARTESIAN_POINT ( 'NONE',  ( -6.016761891674565099, -17.40752468084777504, -7.214149619366543753 ) ) ;
#34518 = LINE ( 'NONE', #29801, #42681 ) ;
#34519 = EDGE_CURVE ( 'NONE', #47731, #36259, #57414, .T. ) ;
#34520 = CIRCLE ( 'NONE', #2480, 42.08604991992415023 ) ;
#34521 = EDGE_CURVE ( 'NONE', #27525, #20977, #9092, .T. ) ;
#34522 = CARTESIAN_POINT ( 'NONE',  ( 0.5839254288179537289, 33.80331890503270387, 33.93171296845855522 ) ) ;
#34523 = CARTESIAN_POINT ( 'NONE',  ( 5.895881250540457863, 20.06765451668684008, 1.347933161250673972 ) ) ;
#34524 = EDGE_LOOP ( 'NONE', ( #56643, #17237, #52175, #10348 ) ) ;
#34525 = CARTESIAN_POINT ( 'NONE',  ( 0.5839879882012687373, 29.15719377327500439, -37.99844431214138041 ) ) ;
#34526 = VECTOR ( 'NONE', #32841, 1000.000000000000000 ) ;
#34527 = CARTESIAN_POINT ( 'NONE',  ( 1.296416391601052265, 19.39309367396150918, -39.57543798657334833 ) ) ;
#34528 = CARTESIAN_POINT ( 'NONE',  ( 3.782625744892852193, 5.920320325620187951, 41.61956164277864190 ) ) ;
#34529 = EDGE_CURVE ( 'NONE', #6221, #55702, #13565, .T. ) ;
#34530 = ORIENTED_EDGE ( 'NONE', *, *, #3288, .F. ) ;
#34531 = DIRECTION ( 'NONE',  ( -1.000000000000000000, -5.380183451256491399E-17, -1.298891185607892835E-16 ) ) ;
#34532 = AXIS2_PLACEMENT_3D ( 'NONE', #17450, #22763, #40981 ) ;
#34533 = CARTESIAN_POINT ( 'NONE',  ( 4.975610109902397937, 25.84633036597824329, 41.52609557555928177 ) ) ;
#34534 = ORIENTED_EDGE ( 'NONE', *, *, #56431, .F. ) ;
#34535 = VERTEX_POINT ( 'NONE', #59927 ) ;
#34536 = CARTESIAN_POINT ( 'NONE',  ( -6.078075953587585900, -8.911363828324937231, 17.06993757945112478 ) ) ;
#34537 = ORIENTED_EDGE ( 'NONE', *, *, #48849, .T. ) ;
#34538 = ADVANCED_FACE ( 'NONE', ( #17036 ), #42376, .F. ) ;
#34539 = CARTESIAN_POINT ( 'NONE',  ( -6.015611763856276717, -9.416239407363420355, 16.32183393015593609 ) ) ;
#34540 = ORIENTED_EDGE ( 'NONE', *, *, #50619, .T. ) ;
#34541 = ORIENTED_EDGE ( 'NONE', *, *, #39849, .F. ) ;
#34543 = VERTEX_POINT ( 'NONE', #34218 ) ;
#34542 = EDGE_CURVE ( 'NONE', #2015, #5057, #32990, .T. ) ;
#34544 = CARTESIAN_POINT ( 'NONE',  ( 5.901463166500145796, 3.331057597887998156, 19.83486641296556385 ) ) ;
#34545 = CARTESIAN_POINT ( 'NONE',  ( 0.1129192098497455998, -12.08918212651712132, -42.43587472053631160 ) ) ;
#34546 = CARTESIAN_POINT ( 'NONE',  ( 0.7948884756798507700, 41.61600058688303960, -26.05392753027271624 ) ) ;
#34547 = VERTEX_POINT ( 'NONE', #24489 ) ;
#34548 = DIRECTION ( 'NONE',  ( -0.07836865515943411409, -0.007886984708650450482, -0.9968932487286225053 ) ) ;
#34549 = CARTESIAN_POINT ( 'NONE',  ( 0.3622758884714730732, 41.42293301073625855, -11.95365414648454205 ) ) ;
#34550 = ORIENTED_EDGE ( 'NONE', *, *, #2227, .F. ) ;
#34551 = ORIENTED_EDGE ( 'NONE', *, *, #39281, .T. ) ;
#34552 = CARTESIAN_POINT ( 'NONE',  ( 0.2285344041767079226, 43.44439842031292898, 7.686703857477898083 ) ) ;
#34553 = CARTESIAN_POINT ( 'NONE',  ( 47.84992101484482419, 12.50001674485125669, -0.1737107653014904884 ) ) ;
#34554 = CARTESIAN_POINT ( 'NONE',  ( 0.1081432562775997974, -30.79166192943866420, 30.19275717928070080 ) ) ;
#34555 = CARTESIAN_POINT ( 'NONE',  ( 0.9791128995231614951, 36.06089395152650212, 21.35297079244299567 ) ) ;
#34556 = ORIENTED_EDGE ( 'NONE', *, *, #17120, .F. ) ;
#34557 = CARTESIAN_POINT ( 'NONE',  ( 0.6009452777970414328, -12.02913818029345272, 46.57942614304337070 ) ) ;
#34558 = CARTESIAN_POINT ( 'NONE',  ( 0.1100247026804066219, 41.61078157869235383, 11.32523219034922590 ) ) ;
#34559 = B_SPLINE_CURVE_WITH_KNOTS ( 'NONE', 3,
 ( #12561, #31651, #7832, #26952 ),
 .UNSPECIFIED., .F., .F.,
 ( 4, 4 ),
 ( 0.000000000000000000, 0.004444103432399266161 ),
 .UNSPECIFIED. ) ;
#34560 = CARTESIAN_POINT ( 'NONE',  ( -6.078457390727109555, -18.90176508385429344, -3.676654423833525254 ) ) ;
#34561 = B_SPLINE_CURVE_WITH_KNOTS ( 'NONE', 3,
 ( #26099, #34904, #24875, #6964 ),
 .UNSPECIFIED., .F., .F.,
 ( 4, 4 ),
 ( 2.297383214701472214E-17, 0.004564976165746188579 ),
 .UNSPECIFIED. ) ;
#34562 = EDGE_CURVE ( 'NONE', #34535, #32393, #59177, .T. ) ;
#34563 = LINE ( 'NONE', #53627, #52040 ) ;
#34564 = AXIS2_PLACEMENT_3D ( 'NONE', #5382, #695, #24508 ) ;
#34565 = ORIENTED_EDGE ( 'NONE', *, *, #41261, .F. ) ;
#34566 = CARTESIAN_POINT ( 'NONE',  ( 4.060580049360325461, -43.03904816311536763, -8.894269366971370161 ) ) ;
#34567 = CARTESIAN_POINT ( 'NONE',  ( 0.1158516988532803244, 36.95306216529235144, -24.11251449850959361 ) ) ;
#34568 = CARTESIAN_POINT ( 'NONE',  ( 4.962356264823609031, -35.98698831890617100, -21.82137185415387037 ) ) ;
#34569 = CARTESIAN_POINT ( 'NONE',  ( 0.9762797500689124330, 41.90547441298052433, -0.5059638413352701702 ) ) ;
#34571 = ORIENTED_EDGE ( 'NONE', *, *, #60382, .T. ) ;
#34570 = AXIS2_PLACEMENT_3D ( 'NONE', #42704, #37707, #18584 ) ;
#34572 = ORIENTED_EDGE ( 'NONE', *, *, #56171, .T. ) ;
#34573 = CARTESIAN_POINT ( 'NONE',  ( 5.000000000000000888, 4.250000000000000000, 0.000000000000000000 ) ) ;
#34574 = CARTESIAN_POINT ( 'NONE',  ( 4.975610109902397937, -4.123593823331679786, -48.73854102369041641 ) ) ;
#34575 = CARTESIAN_POINT ( 'NONE',  ( 0.3676999524040323597, -42.45338881270421894, -11.98584004733086061 ) ) ;
#34576 = VECTOR ( 'NONE', #17546, 1000.000000000000341 ) ;
#34577 = DIRECTION ( 'NONE',  ( -0.07906939808003032866, -0.9443293062557420736, -0.3193590324913493372 ) ) ;
#34578 = DIRECTION ( 'NONE',  ( -1.000000000000000000, -0.000000000000000000, -0.000000000000000000 ) ) ;
#34579 = CARTESIAN_POINT ( 'NONE',  ( 2.624215991343620935, -34.92983774302943090, -32.93378783738885573 ) ) ;
#34580 = CARTESIAN_POINT ( 'NONE',  ( 1.231276596079887931, 8.892602616354244205, -40.96581977363174332 ) ) ;
#34581 = CARTESIAN_POINT ( 'NONE',  ( 0.8751705887134423323, 19.22545746485661766, -44.08562551107063143 ) ) ;
#34582 = CARTESIAN_POINT ( 'NONE',  ( 0.9769922540276043676, -0.9586864849378278208, -41.89764283715400239 ) ) ;
#34583 =( BOUNDED_SURFACE ( )  B_SPLINE_SURFACE ( 3, 1, ( 
 ( #40046, #25594 ),
 ( #50321, #10898 ),
 ( #20900, #15902 ),
 ( #11201, #55012 ) ),
 .UNSPECIFIED., .F., .F., .F. ) 
 B_SPLINE_SURFACE_WITH_KNOTS ( ( 4, 4 ),
 ( 2, 2 ),
 ( 0.000000000000000000, 1.000000000000000000 ),
 ( 0.000000000000000000, 1.000000000000000000 ),
 .UNSPECIFIED. ) 
 GEOMETRIC_REPRESENTATION_ITEM ( )  RATIONAL_B_SPLINE_SURFACE ( (
 ( 1.000000000000000000, 1.000000000000000000),
 ( 0.7269869731126817891, 0.9931720237060910339),
 ( 0.7269869731126817891, 0.9931720237060910339),
 ( 1.000000000000000000, 1.000000000000000000) ) ) 
 REPRESENTATION_ITEM ( '' )  SURFACE ( )  );
#34584 = CARTESIAN_POINT ( 'NONE',  ( 0.6031357023905875581, -6.322524267548935484, 47.69018446756497553 ) ) ;
#34585 = ORIENTED_EDGE ( 'NONE', *, *, #39217, .F. ) ;
#34586 = CARTESIAN_POINT ( 'NONE',  ( 1.091591847532196402, 15.78966934106792053, -38.82583332081330241 ) ) ;
#34587 = CARTESIAN_POINT ( 'NONE',  ( 5.917102823773431552, -17.30871814525804808, -10.24197218409408094 ) ) ;
#34588 = CARTESIAN_POINT ( 'NONE',  ( 0.1157506346131639274, -35.30612916330391471, 26.46540956242572307 ) ) ;
#34589 = DIRECTION ( 'NONE',  ( 0.09722883295013595717, -0.7201826484181221844, 0.6869377751737153481 ) ) ;
#34590 = CARTESIAN_POINT ( 'NONE',  ( 0.6031356755773454870, -24.05369945659562703, 41.66228085015284677 ) ) ;
#34591 = CARTESIAN_POINT ( 'NONE',  ( 0.6554360035617794455, -4.240386000424091861, -0.1586754815285204845 ) ) ;
#34592 = CARTESIAN_POINT ( 'NONE',  ( 2.528100132419517365, 10.90475753638862066, 40.53813071300465509 ) ) ;
#34593 = CARTESIAN_POINT ( 'NONE',  ( 1.154321485836933725, 6.418927614506086954, 42.43366804742919385 ) ) ;
#34594 = FACE_OUTER_BOUND ( 'NONE', #14050, .T. ) ;
#34595 = EDGE_CURVE ( 'NONE', #31849, #14207, #56906, .T. ) ;
#34596 = CARTESIAN_POINT ( 'NONE',  ( 3.782625744892855302, -25.80136476166733672, 33.18927056339735060 ) ) ;
#34597 = CARTESIAN_POINT ( 'NONE',  ( 0.5806925824938499181, 10.33919002968644385, 45.74192291403583965 ) ) ;
#34599 = ORIENTED_EDGE ( 'NONE', *, *, #28016, .T. ) ;
#34598 = CARTESIAN_POINT ( 'NONE',  ( 0.6254087463353912302, -6.960754339421479031, -47.60024110474246584 ) ) ;
#34600 = ORIENTED_EDGE ( 'NONE', *, *, #12970, .T. ) ;
#34601 = CARTESIAN_POINT ( 'NONE',  ( 4.540110984502054414, 10.44709687487745065, 3.997669511110601399E-16 ) ) ;
#34602 = CARTESIAN_POINT ( 'NONE',  ( 0.6845945791218023269, 31.98229355120883710, -34.31529425661756960 ) ) ;
#34603 = CARTESIAN_POINT ( 'NONE',  ( 0.5997462898726536595, -34.91088276334701135, -34.53667463477266608 ) ) ;
#34604 = EDGE_CURVE ( 'NONE', #23510, #47692, #59908, .T. ) ;
#34605 = ORIENTED_EDGE ( 'NONE', *, *, #25584, .F. ) ;
#34606 = VERTEX_POINT ( 'NONE', #14801 ) ;
#34607 = CARTESIAN_POINT ( 'NONE',  ( 4.975801465491694664, -32.01766832630337944, 35.64402118370901462 ) ) ;
#34608 = CARTESIAN_POINT ( 'NONE',  ( 3.238741278300274029, 1.828728677531826108, -42.95313747363662316 ) ) ;
#34609 = CARTESIAN_POINT ( 'NONE',  ( 0.5836750258453369256, -41.38803015411989605, -24.10509086647793353 ) ) ;
#34610 = ORIENTED_EDGE ( 'NONE', *, *, #49430, .F. ) ;
#34611 = ORIENTED_EDGE ( 'NONE', *, *, #46265, .T. ) ;
#34612 = CARTESIAN_POINT ( 'NONE',  ( -6.063463321072276813, -18.90456390296425582, -3.665776332267282722 ) ) ;
#34613 = DIRECTION ( 'NONE',  ( 0.000000000000000000, 0.000000000000000000, 1.000000000000000000 ) ) ;
#34614 = CIRCLE ( 'NONE', #22625, 46.67105333295396719 ) ;
#34615 = CARTESIAN_POINT ( 'NONE',  ( 0.8751705887134553219, -46.21789262997766201, 13.30665218149281870 ) ) ;
#34616 = CARTESIAN_POINT ( 'NONE',  ( 4.226256110419179812, -10.18024542482925909, 42.74564133426272150 ) ) ;
#34617 = EDGE_CURVE ( 'NONE', #17781, #2801, #19812, .T. ) ;
#34619 = CARTESIAN_POINT ( 'NONE',  ( 0.9790850452238881729, -41.07895617916494757, -8.297993100349147610 ) ) ;
#34618 = AXIS2_PLACEMENT_3D ( 'NONE', #32747, #4505, #56218 ) ;
#34620 = CARTESIAN_POINT ( 'NONE',  ( 3.678834586032788678, 43.29171918419824294, 22.90064234262600351 ) ) ;
#34621 = CARTESIAN_POINT ( 'NONE',  ( 0.1145239942831223490, 15.54503240824534060, -41.29524728260233957 ) ) ;
#34622 = ORIENTED_EDGE ( 'NONE', *, *, #40922, .T. ) ;
#34623 = VECTOR ( 'NONE', #57582, 999.9999999999998863 ) ;
#34624 = ORIENTED_EDGE ( 'NONE', *, *, #13002, .T. ) ;
#34625 = CARTESIAN_POINT ( 'NONE',  ( 0.7044674535453004927, -19.10600803152214411, 45.24116687167030904 ) ) ;
#34626 = CARTESIAN_POINT ( 'NONE',  ( 0.8751705887134553219, 44.76769609654211735, 17.57879340691559378 ) ) ;
#34627 = ORIENTED_EDGE ( 'NONE', *, *, #5659, .T. ) ;
#34628 = CARTESIAN_POINT ( 'NONE',  ( 4.975610109902397937, 0.000000000000000000, 0.000000000000000000 ) ) ;
#34629 = CARTESIAN_POINT ( 'NONE',  ( 3.661933894777869014, 2.831097433652313367, 46.95333909609433221 ) ) ;
#34630 = CARTESIAN_POINT ( 'NONE',  ( 0.5806925824938502512, -13.37132486740698134, 44.94919391528425479 ) ) ;
#34631 = CARTESIAN_POINT ( 'NONE',  ( 5.895596859100789899, 3.341829471546786667, 19.83331437242874884 ) ) ;
#34632 = ORIENTED_EDGE ( 'NONE', *, *, #17695, .T. ) ;
#34633 = CARTESIAN_POINT ( 'NONE',  ( 4.956653778116966613, 0.000000000000000000, 0.000000000000000000 ) ) ;
#34634 = CARTESIAN_POINT ( 'NONE',  ( 0.1129192098497447394, 43.21532672376840623, -8.909956450123800664 ) ) ;
#34635 = CARTESIAN_POINT ( 'NONE',  ( 6.189768672335216770, 1.091423221276722755, -1.945113688487589062E-17 ) ) ;
#34636 = ORIENTED_EDGE ( 'NONE', *, *, #1739, .T. ) ;
#34637 = CARTESIAN_POINT ( 'NONE',  ( 0.5800708057587392608, -46.42229836006543309, 11.78915002112706212 ) ) ;
#34638 = CARTESIAN_POINT ( 'NONE',  ( 3.050102900204245682, -28.82147234748848774, -33.23774933567278822 ) ) ;
#34639 = ORIENTED_EDGE ( 'NONE', *, *, #15957, .T. ) ;
#34640 = DIRECTION ( 'NONE',  ( 0.000000000000000000, 0.000000000000000000, 1.000000000000000000 ) ) ;
#34641 = CARTESIAN_POINT ( 'NONE',  ( 0.5827359174754822568, 24.26188383263427184, -41.29633904010488266 ) ) ;
#34642 = EDGE_LOOP ( 'NONE', ( #30612, #17977, #50865, #8873 ) ) ;
#34643 = CARTESIAN_POINT ( 'NONE',  ( 3.407937589446174087, -10.00592723328967715, 9.356405769959017960 ) ) ;
#34644 = CARTESIAN_POINT ( 'NONE',  ( 5.981074661064941900, -20.34795181394750685, 2.687517936919654016 ) ) ;
#34645 = ADVANCED_FACE ( 'NONE', ( #8852 ), #51117, .F. ) ;
#34646 = LINE ( 'NONE', #30236, #34490 ) ;
#34647 = CARTESIAN_POINT ( 'NONE',  ( 0.1157991065609915993, 33.65088663166012850, -28.54050094936765092 ) ) ;
#34648 = CARTESIAN_POINT ( 'NONE',  ( 0.7056555295713298204, 5.417452459790411012, -47.59410019435323136 ) ) ;
#34649 = CARTESIAN_POINT ( 'NONE',  ( 0.1119898979215348395, -41.10694714348719714, -16.03683899009958580 ) ) ;
#34650 = DIRECTION ( 'NONE',  ( 0.09835009131224552170, -0.3879606369183575265, -0.9164135549743768205 ) ) ;
#34651 = VERTEX_POINT ( 'NONE', #33913 ) ;
#34652 = EDGE_CURVE ( 'NONE', #37577, #45332, #14335, .T. ) ;
#34653 = CARTESIAN_POINT ( 'NONE',  ( 6.999999999999995559, 58.44237546506882808, -54.69470952477875869 ) ) ;
#34654 = CIRCLE ( 'NONE', #33676, 11.40403086437694569 ) ;
#34655 = DIRECTION ( 'NONE',  ( 0.000000000000000000, 0.000000000000000000, -1.000000000000000000 ) ) ;
#34656 = FACE_OUTER_BOUND ( 'NONE', #53530, .T. ) ;
#34657 = ORIENTED_EDGE ( 'NONE', *, *, #10768, .T. ) ;
#34658 = AXIS2_PLACEMENT_3D ( 'NONE', #32018, #12004, #42053 ) ;
#34659 = B_SPLINE_CURVE_WITH_KNOTS ( 'NONE', 3,
 ( #10585, #48791, #43823, #9973, #44436, #545 ),
 .UNSPECIFIED., .F., .F.,
 ( 4, 2, 4 ),
 ( 1.951563910473907981E-18, 0.0002447193893791689491, 0.0004894387787583359467 ),
 .UNSPECIFIED. ) ;
#34660 = VECTOR ( 'NONE', #40594, 1000.000000000000114 ) ;
#34661 = CARTESIAN_POINT ( 'NONE',  ( 2.528190830796657185, -31.93279228743793041, 27.24978739147064744 ) ) ;
#34662 = CARTESIAN_POINT ( 'NONE',  ( 0.8560838555295158248, 23.34035564869604684, -40.68907263964262455 ) ) ;
#34663 = CARTESIAN_POINT ( 'NONE',  ( 0.6029443199889047422, 22.71407876865105280, 43.53858366490483434 ) ) ;
#34664 = CARTESIAN_POINT ( 'NONE',  ( 5.965394784446458765, 2.693446924985354318, 20.34787558161487908 ) ) ;
#34665 = B_SPLINE_CURVE_WITH_KNOTS ( 'NONE', 3,
 ( #30178, #58059, #10789, #52754 ),
 .UNSPECIFIED., .F., .F.,
 ( 4, 4 ),
 ( 1.734723475976807094E-18, 0.005014147105413696050 ),
 .UNSPECIFIED. ) ;
#34666 = CARTESIAN_POINT ( 'NONE',  ( 0.6021447746440204973, -19.63869024154479348, 45.00958769734666731 ) ) ;
#34667 = CARTESIAN_POINT ( 'NONE',  ( 43.00000000000000000, 0.000000000000000000, 0.000000000000000000 ) ) ;
#34668 = DIRECTION ( 'NONE',  ( 1.844239498168834692E-16, -0.9999920064717846557, 0.003998373736180944708 ) ) ;
#34669 = CARTESIAN_POINT ( 'NONE',  ( 5.838029081930955932, 25.39899213859815319, 39.82406629786000707 ) ) ;
#34670 = CARTESIAN_POINT ( 'NONE',  ( 0.6029303876144825880, -0.1308990448399069417, 48.10727438003475953 ) ) ;
#34671 = EDGE_CURVE ( 'NONE', #2855, #56952, #28880, .T. ) ;
#34672 = CIRCLE ( 'NONE', #18667, 43.92652462719577500 ) ;
#34673 = CARTESIAN_POINT ( 'NONE',  ( 0.6031356755852232965, 5.421189728766411748E-15, -48.10744332413860747 ) ) ;
#34675 = ORIENTED_EDGE ( 'NONE', *, *, #10604, .F. ) ;
#34674 = FACE_OUTER_BOUND ( 'NONE', #57263, .T. ) ;
#34676 = ORIENTED_EDGE ( 'NONE', *, *, #3949, .F. ) ;
#34677 = CARTESIAN_POINT ( 'NONE',  ( 0.6000166863083090663, -47.63401213562571002, 11.95091500980225518 ) ) ;
#34678 = CARTESIAN_POINT ( 'NONE',  ( 5.965394784446460541, 20.34787558161483645, 2.693446924985696267 ) ) ;
#34679 = CARTESIAN_POINT ( 'NONE',  ( 5.894904586330512508, -9.666977479134521545, 17.63743060878054436 ) ) ;
#34680 = EDGE_CURVE ( 'NONE', #55527, #20220, #350, .T. ) ;
#34681 = CARTESIAN_POINT ( 'NONE',  ( 0.1158816050234199035, -22.86878204857423214, 37.73540577388786232 ) ) ;
#34682 = CARTESIAN_POINT ( 'NONE',  ( 5.910764540655178756, 14.90587032029975667, -13.50245416446839286 ) ) ;
#34683 = CARTESIAN_POINT ( 'NONE',  ( 2.643462169533600914, -47.78621045426879022, 4.896978544601340744 ) ) ;
#34684 = EDGE_CURVE ( 'NONE', #54546, #14082, #9883, .T. ) ;
#34685 =( BOUNDED_SURFACE ( )  B_SPLINE_SURFACE ( 3, 1, ( 
 ( #23489, #56683 ),
 ( #19129, #57287 ),
 ( #13186, #32915 ),
 ( #23809, #14420 ) ),
 .UNSPECIFIED., .F., .F., .F. ) 
 B_SPLINE_SURFACE_WITH_KNOTS ( ( 4, 4 ),
 ( 2, 2 ),
 ( 0.000000000000000000, 1.000000000000000000 ),
 ( 0.000000000000000000, 1.000000000000000000 ),
 .UNSPECIFIED. ) 
 GEOMETRIC_REPRESENTATION_ITEM ( )  RATIONAL_B_SPLINE_SURFACE ( (
 ( 1.000000000000000000, 1.000000000000000000),
 ( 0.7211978278499970862, 0.9934217856018976445),
 ( 0.7211978278499970862, 0.9934217856018976445),
 ( 1.000000000000000000, 1.000000000000000000) ) ) 
 REPRESENTATION_ITEM ( '' )  SURFACE ( )  );
#34686 = VERTEX_POINT ( 'NONE', #37694 ) ;
#34687 = ORIENTED_EDGE ( 'NONE', *, *, #3335, .T. ) ;
#34688 = B_SPLINE_CURVE_WITH_KNOTS ( 'NONE', 3,
 ( #20262, #21169, #59679, #11787 ),
 .UNSPECIFIED., .F., .F.,
 ( 4, 4 ),
 ( 4.443059973708341306E-17, 0.005004948556313854741 ),
 .UNSPECIFIED. ) ;
#34689 = CARTESIAN_POINT ( 'NONE',  ( 4.962356264823608143, 30.91935898304044272, 28.55221248765537467 ) ) ;
#34690 = FACE_OUTER_BOUND ( 'NONE', #12077, .T. ) ;
#34691 = CARTESIAN_POINT ( 'NONE',  ( 2.624215991343620935, -17.05978231157435943, 44.87417713512083139 ) ) ;
#34692 = ORIENTED_EDGE ( 'NONE', *, *, #16924, .F. ) ;
#34693 = EDGE_CURVE ( 'NONE', #21937, #5016, #3091, .T. ) ;
#34694 = CARTESIAN_POINT ( 'NONE',  ( 1.092182651088187795, -27.65225184159188387, -31.49784361716628212 ) ) ;
#34695 = CARTESIAN_POINT ( 'NONE',  ( 0.5848930533535030563, -25.08041605097284332, 39.62632727237867414 ) ) ;
#34696 = ORIENTED_EDGE ( 'NONE', *, *, #38941, .T. ) ;
#34697 =( BOUNDED_SURFACE ( )  B_SPLINE_SURFACE ( 3, 1, ( 
 ( #24971, #34373 ),
 ( #44110, #6429 ),
 ( #20880, #30570 ),
 ( #1436, #59380 ) ),
 .UNSPECIFIED., .F., .F., .F. ) 
 B_SPLINE_SURFACE_WITH_KNOTS ( ( 4, 4 ),
 ( 2, 2 ),
 ( 0.000000000000000000, 1.000000000000000000 ),
 ( 0.000000000000000000, 1.000000000000000000 ),
 .UNSPECIFIED. ) 
 GEOMETRIC_REPRESENTATION_ITEM ( )  RATIONAL_B_SPLINE_SURFACE ( (
 ( 1.000000000000000000, 1.000000000000000000),
 ( 0.9732289882329797637, 0.9999525324661233672),
 ( 0.9732289882329797637, 0.9999525324661233672),
 ( 1.000000000000000000, 1.000000000000000000) ) ) 
 REPRESENTATION_ITEM ( '' )  SURFACE ( )  );
#34698 = CARTESIAN_POINT ( 'NONE',  ( 0.7057020205114994393, -44.57024707370723604, 17.55108080125430448 ) ) ;
#34699 = EDGE_LOOP ( 'NONE', ( #6467, #10480, #29883, #6351 ) ) ;
#34700 = CARTESIAN_POINT ( 'NONE',  ( 0.5806925824938494740, -34.41156632303759011, 31.86010774524702072 ) ) ;
#34701 = FACE_BOUND ( 'NONE', #18652, .T. ) ;
#34702 = CIRCLE ( 'NONE', #37713, 13.00000000000000178 ) ;
#34703 = ORIENTED_EDGE ( 'NONE', *, *, #41540, .T. ) ;
#34704 = CONICAL_SURFACE ( 'NONE', #12714, 44.12552607296456131, 0.04450589592585061510 ) ;
#34705 = CARTESIAN_POINT ( 'NONE',  ( 0.5800708119828335008, -41.78924007434309118, -23.40241990038080999 ) ) ;
#34706 = CARTESIAN_POINT ( 'NONE',  ( 4.962356264823608143, -40.70360067759239087, 10.69824704058788711 ) ) ;
#34707 = CARTESIAN_POINT ( 'NONE',  ( 0.9787464366903563251, 40.37245734402069530, 11.24271679335978469 ) ) ;
#34708 = CARTESIAN_POINT ( 'NONE',  ( 0.6039202388192952409, 4.542059820466225695, 48.89717175293780116 ) ) ;
#34709 = ORIENTED_EDGE ( 'NONE', *, *, #45925, .F. ) ;
#34710 = CARTESIAN_POINT ( 'NONE',  ( 4.967162193818130511, -43.02067033766017801, -2.375726030843023029 ) ) ;
#34711 = CARTESIAN_POINT ( 'NONE',  ( 4.975610109902397937, -46.23629923292386934, 15.95788333023201488 ) ) ;
#34712 = VERTEX_POINT ( 'NONE', #20118 ) ;
#34713 = CARTESIAN_POINT ( 'NONE',  ( 3.407937589446174087, 0.4592810312473891710, -13.69123696618923880 ) ) ;
#34714 = B_SPLINE_CURVE_WITH_KNOTS ( 'NONE', 3,
 ( #26901, #49462, #2134, #30349 ),
 .UNSPECIFIED., .F., .F.,
 ( 4, 4 ),
 ( 0.000000000000000000, 0.004442905043737215703 ),
 .UNSPECIFIED. ) ;
#34715 = ORIENTED_EDGE ( 'NONE', *, *, #34929, .F. ) ;
#34716 = CARTESIAN_POINT ( 'NONE',  ( 2.301430502907646058, 40.93949994354150590, 25.12309903330034544 ) ) ;
#34717 = ORIENTED_EDGE ( 'NONE', *, *, #47899, .F. ) ;
#34718 = CARTESIAN_POINT ( 'NONE',  ( 4.962356264823608143, 0.000000000000000000, 0.000000000000000000 ) ) ;
#34720 = CIRCLE ( 'NONE', #15718, 12.50000000000000000 ) ;
#34719 = CARTESIAN_POINT ( 'NONE',  ( 0.6024113833632038784, -30.44748741247445523, -38.52911080427468704 ) ) ;
#34721 = EDGE_CURVE ( 'NONE', #57622, #3838, #39754, .T. ) ;
#34723 = CARTESIAN_POINT ( 'NONE',  ( 1.227938101723748288, -39.32113113558953899, -17.20315230597885758 ) ) ;
#34722 = B_SPLINE_CURVE_WITH_KNOTS ( 'NONE', 3,
 ( #44922, #6958, #6637, #47003, #13174, #8759, #4036, #23176, #13479, #56361, #56054, #1961, #27874, #60748, #42303, #54570, #32585, #35511, #49901, #49581, #61361, #16388, #21088, #26091, #40232 ),
 .UNSPECIFIED., .F., .F.,
 ( 4, 3, 3, 3, 3, 3, 3, 3, 4 ),
 ( 6.992893892674702526E-18, 0.0005656085177311402905, 0.001131215744874500924, 0.001696821861372767000, 0.002262427090022498585, 0.002828031679238746793, 0.003393635864401606164, 0.003977030878808133357, 0.004561030005651159867 ),
 .UNSPECIFIED. ) ;
#34724 = EDGE_LOOP ( 'NONE', ( #61355, #57311, #4859, #17416 ) ) ;
#34725 = CARTESIAN_POINT ( 'NONE',  ( 0.5827359174754822568, 5.891371786504956631, 47.53228759166450601 ) ) ;
#34726 = EDGE_CURVE ( 'NONE', #5232, #41497, #41306, .T. ) ;
#34727 = CARTESIAN_POINT ( 'NONE',  ( -5.995132425357893702, 17.40647075750116457, 7.219211173946554538 ) ) ;
#34728 = CARTESIAN_POINT ( 'NONE',  ( 0.9762797500689124330, -7.469026406146330288, 41.23758515880862774 ) ) ;
#34729 = ORIENTED_EDGE ( 'NONE', *, *, #15010, .F. ) ;
#34730 = VECTOR ( 'NONE', #1202, 1000.000000000000000 ) ;
#34731 = EDGE_CURVE ( 'NONE', #43474, #43585, #6903, .T. ) ;
#34732 = ORIENTED_EDGE ( 'NONE', *, *, #44629, .T. ) ;
#34733 = CARTESIAN_POINT ( 'NONE',  ( 0.9785694773339252972, -30.93190758888828995, -28.27635935949227530 ) ) ;
#34734 = CARTESIAN_POINT ( 'NONE',  ( 3.559346040607745287, 31.04985557733589019, 31.13417334969039629 ) ) ;
#34735 = CARTESIAN_POINT ( 'NONE',  ( 0.000000000000000000, 0.000000000000000000, 3.469446951953614189E-15 ) ) ;
#34736 = CARTESIAN_POINT ( 'NONE',  ( 0.6000166863083090663, 32.62822748873757916, -36.70452632376071733 ) ) ;
#34737 = ORIENTED_EDGE ( 'NONE', *, *, #52740, .T. ) ;
#34738 = ADVANCED_FACE ( 'NONE', ( #48916 ), #33952, .F. ) ;
#34739 = CARTESIAN_POINT ( 'NONE',  ( 15.24999999999999289, 2.688986455804112996, 8.896908036367455278E-17 ) ) ;
#34740 = ORIENTED_EDGE ( 'NONE', *, *, #33987, .T. ) ;
#34741 = CARTESIAN_POINT ( 'NONE',  ( 4.967162193818130511, -42.96271701169388280, 3.259922920617591924 ) ) ;
#34742 = DIRECTION ( 'NONE',  ( -1.000000000000000000, -0.000000000000000000, -0.000000000000000000 ) ) ;
#34743 = CARTESIAN_POINT ( 'NONE',  ( 0.8760168074886960365, 44.09317760313724932, 19.22870327415319380 ) ) ;
#34744 = CARTESIAN_POINT ( 'NONE',  ( 4.975801465491694664, -31.15993731089097452, -36.39623109580456628 ) ) ;
#34745 = CARTESIAN_POINT ( 'NONE',  ( 2.301430502907645614, -37.31003439265388266, -30.25184447737420967 ) ) ;
#34746 = DIRECTION ( 'NONE',  ( 0.02222222222222222307, -0.9997530559290660479, 0.000000000000000000 ) ) ;
#34747 = CARTESIAN_POINT ( 'NONE',  ( 0.7048096507298579061, 44.76417498422313912, -17.62869676200362790 ) ) ;
#34748 = AXIS2_PLACEMENT_3D ( 'NONE', #56093, #27602, #47639 ) ;
#34749 = EDGE_CURVE ( 'NONE', #58534, #17351, #16033, .T. ) ;
#34750 = CARTESIAN_POINT ( 'NONE',  ( 0.1129192098497455998, 29.30421273086464140, 32.98810246148426728 ) ) ;
#34751 = CARTESIAN_POINT ( 'NONE',  ( 1.000433927950262536, 4.849797705185330265, 41.62809315680488709 ) ) ;
#34752 = STYLED_ITEM ( 'NONE', ( #25093 ), #48247 ) ;
#34753 = CIRCLE ( 'NONE', #15744, 48.09070567114147110 ) ;
#34754 = EDGE_CURVE ( 'NONE', #14421, #25770, #11321, .T. ) ;
#34755 = DIRECTION ( 'NONE',  ( 1.000000000000000000, 0.000000000000000000, 0.000000000000000000 ) ) ;
#34756 = CARTESIAN_POINT ( 'NONE',  ( 0.9754292580325142348, 3.614901275221697130, 41.75236467164950227 ) ) ;
#34757 = CARTESIAN_POINT ( 'NONE',  ( 0.7246131072078559887, 11.65529928397572590, 46.66866179549017346 ) ) ;
#34758 = CARTESIAN_POINT ( 'NONE',  ( 0.5804410086790514622, -7.261380058783999836, -46.33348909263461479 ) ) ;
#34759 = EDGE_CURVE ( 'NONE', #10554, #38699, #21085, .T. ) ;
#34760 = ORIENTED_EDGE ( 'NONE', *, *, #21013, .T. ) ;
#34761 = FILL_AREA_STYLE_COLOUR ( '', #45313 ) ;
#34762 = CARTESIAN_POINT ( 'NONE',  ( 0.5817217712918323347, -19.32622360567856390, -42.72858569098310255 ) ) ;
#34763 = CARTESIAN_POINT ( 'NONE',  ( 0.5819845079324660331, 17.90867223323947144, -44.42187385013345136 ) ) ;
#34764 = CARTESIAN_POINT ( 'NONE',  ( 1.112077966505211402, 40.15882174338756982, 18.17413990568401161 ) ) ;
#34765 = CARTESIAN_POINT ( 'NONE',  ( 5.895881250540457863, -17.30746725809839859, 10.24593864505115803 ) ) ;
#34766 = VERTEX_POINT ( 'NONE', #29495 ) ;
#34767 = CARTESIAN_POINT ( 'NONE',  ( 4.962356264823608143, -29.56943756613123497, 29.94802096775367772 ) ) ;
#34768 = CARTESIAN_POINT ( 'NONE',  ( -2.569797478183783568, -6.011723966604058944, -13.34095667500602644 ) ) ;
#34769 = B_SPLINE_CURVE_WITH_KNOTS ( 'NONE', 3,
 ( #43604, #19474, #57039, #37666 ),
 .UNSPECIFIED., .F., .F.,
 ( 4, 4 ),
 ( 1.734723475976807094E-18, 0.004042984057420971958 ),
 .UNSPECIFIED. ) ;
#34770 = EDGE_CURVE ( 'NONE', #13767, #52623, #48603, .T. ) ;
#34771 = CARTESIAN_POINT ( 'NONE',  ( 4.549368137175248350, 38.59302160394752690, -18.79584381673492288 ) ) ;
#34772 = VERTEX_POINT ( 'NONE', #31050 ) ;
#34773 = CARTESIAN_POINT ( 'NONE',  ( 4.694002226626920127, -30.90320716794954237, -33.51531826166844752 ) ) ;
#34774 = EDGE_CURVE ( 'NONE', #29832, #59804, #35200, .T. ) ;
#34775 = CARTESIAN_POINT ( 'NONE',  ( 1.092182651088183798, 15.79015195333629329, 38.82566529671880318 ) ) ;
#34776 = AXIS2_PLACEMENT_3D ( 'NONE', #52219, #47545, #14968 ) ;
#34777 = ORIENTED_EDGE ( 'NONE', *, *, #43766, .F. ) ;
#34778 = CARTESIAN_POINT ( 'NONE',  ( -9.500000000000000000, 1.163414459189985485E-15, -1.199999999999999956 ) ) ;
#34779 = B_SPLINE_CURVE_WITH_KNOTS ( 'NONE', 3,
 ( #4683, #27291, #42640, #61700, #47328, #23830 ),
 .UNSPECIFIED., .F., .F.,
 ( 4, 2, 4 ),
 ( 0.000000000000000000, 0.0002291459268755702348, 0.0004582918537511404696 ),
 .UNSPECIFIED. ) ;
#34780 = VERTEX_POINT ( 'NONE', #50458 ) ;
#34781 = CARTESIAN_POINT ( 'NONE',  ( 2.624215991343608501, 28.09277600149218657, 38.92973006074523568 ) ) ;
#34782 = VERTEX_POINT ( 'NONE', #11969 ) ;
#34783 = LINE ( 'NONE', #38565, #31741 ) ;
#34784 = FACE_OUTER_BOUND ( 'NONE', #40148, .T. ) ;
#34785 = ORIENTED_EDGE ( 'NONE', *, *, #9816, .T. ) ;
#34786 = FACE_BOUND ( 'NONE', #13092, .T. ) ;
#34787 = ORIENTED_EDGE ( 'NONE', *, *, #2589, .F. ) ;
#34788 = CARTESIAN_POINT ( 'NONE',  ( 4.956653778116893783, -15.97476558431863758, -45.35992544608534160 ) ) ;
#34789 = CARTESIAN_POINT ( 'NONE',  ( 0.1156495703730067159, -1.277995041157171219, 44.10566496387792768 ) ) ;
#34790 = VERTEX_POINT ( 'NONE', #46396 ) ;
#34791 = CARTESIAN_POINT ( 'NONE',  ( 0.1129192098497447394, 25.64022107388777272, 35.91003830501040994 ) ) ;
#34792 = CARTESIAN_POINT ( 'NONE',  ( 1.227938101723756947, -20.72293514920776758, 37.58536632582772086 ) ) ;
#34793 = AXIS2_PLACEMENT_3D ( 'NONE', #3042, #41294, #17465 ) ;
#34794 = CARTESIAN_POINT ( 'NONE',  ( 0.6028618097248863439, 24.20479143424832813, 41.57478760529411943 ) ) ;
#34795 = VECTOR ( 'NONE', #55416, 1000.000000000000000 ) ;
#34796 = CARTESIAN_POINT ( 'NONE',  ( 0.6023143664670691511, 44.34466302085797196, 18.65155446683267115 ) ) ;
#34797 = ORIENTED_EDGE ( 'NONE', *, *, #39713, .F. ) ;
#34798 = EDGE_CURVE ( 'NONE', #39339, #9846, #59119, .T. ) ;
#34799 = CARTESIAN_POINT ( 'NONE',  ( -6.017396004339686577, 18.20140164570668873, 4.875835690939244849 ) ) ;
#34800 = CARTESIAN_POINT ( 'NONE',  ( 0.5839880159502324197, -44.26747004398431073, 18.28706857028357291 ) ) ;
#34801 = B_SPLINE_CURVE_WITH_KNOTS ( 'NONE', 3,
 ( #10874, #42314, #61373, #53143 ),
 .UNSPECIFIED., .F., .F.,
 ( 4, 4 ),
 ( 2.183987964099526702E-17, 0.004444306975806114161 ),
 .UNSPECIFIED. ) ;
#34802 = ORIENTED_EDGE ( 'NONE', *, *, #54222, .T. ) ;
#34803 = CARTESIAN_POINT ( 'NONE',  ( 0.7762783648524383961, 47.37038525648369358, -7.133808749408959038 ) ) ;
#34804 = ADVANCED_FACE ( 'NONE', ( #50159 ), #57509, .F. ) ;
#34805 = ORIENTED_EDGE ( 'NONE', *, *, #33760, .T. ) ;
#34806 = CARTESIAN_POINT ( 'NONE',  ( 0.9740398440564311811, 33.78760696452741286, -26.44872719679335660 ) ) ;
#34807 =( BOUNDED_SURFACE ( )  B_SPLINE_SURFACE ( 3, 1, ( 
 ( #1600, #35158 ),
 ( #34536, #996 ),
 ( #39877, #38945 ),
 ( #53915, #6288 ) ),
 .UNSPECIFIED., .F., .F., .F. ) 
 B_SPLINE_SURFACE_WITH_KNOTS ( ( 4, 4 ),
 ( 2, 2 ),
 ( 0.000000000000000000, 1.000000000000000000 ),
 ( 0.000000000000000000, 1.000000000000000000 ),
 .UNSPECIFIED. ) 
 GEOMETRIC_REPRESENTATION_ITEM ( )  RATIONAL_B_SPLINE_SURFACE ( (
 ( 1.000000000000000000, 1.000000000000000000),
 ( 0.9953485035131437453, 0.8621029689291515030),
 ( 0.9953485035131437453, 0.8621029689291515030),
 ( 1.000000000000000000, 1.000000000000000000) ) ) 
 REPRESENTATION_ITEM ( '' )  SURFACE ( )  );
#34808 = B_SPLINE_CURVE_WITH_KNOTS ( 'NONE', 3,
 ( #29098, #48216, #577, #53204, #4963, #44167, #43853, #896, #34433, #34131, #5269, #20331, #10309, #5879, #57573, #1199 ),
 .UNSPECIFIED., .F., .F.,
 ( 4, 3, 3, 3, 3, 4 ),
 ( 2.030557555191247372E-17, 0.0002618515315864412721, 0.0003927756766341967986, 0.0005236998216950550710, 0.0007855159896329879472, 0.001047349442285926569 ),
 .UNSPECIFIED. ) ;
#34809 = CARTESIAN_POINT ( 'NONE',  ( 0.1158403557922069033, 25.21309394138425830, 36.21105081445097795 ) ) ;
#34810 = ORIENTED_EDGE ( 'NONE', *, *, #24819, .F. ) ;
#34811 = LINE ( 'NONE', #1566, #9561 ) ;
#34812 = CARTESIAN_POINT ( 'NONE',  ( 0.5809828226811553087, -47.89273459658654275, 0.5448590168530708100 ) ) ;
#34813 = CARTESIAN_POINT ( 'NONE',  ( 0.5998501479064699549, -0.5236536531311584142, -48.10473956285919428 ) ) ;
#34814 = CARTESIAN_POINT ( 'NONE',  ( -19.03272015457537947, -12.36519495213270936, 1.833918244462691804 ) ) ;
#34815 = EDGE_CURVE ( 'NONE', #10104, #31868, #7216, .T. ) ;
#34816 = EDGE_CURVE ( 'NONE', #20940, #5144, #44303, .T. ) ;
#34817 = CONICAL_SURFACE ( 'NONE', #56825, 43.08621763946400307, 1.568696531533066763 ) ;
#34818 = ORIENTED_EDGE ( 'NONE', *, *, #22301, .T. ) ;
#34819 = CARTESIAN_POINT ( 'NONE',  ( 4.549368137175248350, 0.000000000000000000, 0.000000000000000000 ) ) ;
#34820 = EDGE_CURVE ( 'NONE', #23477, #13696, #34212, .T. ) ;
#34821 = FILL_AREA_STYLE ('',( #37441 ) ) ;
#34822 = CARTESIAN_POINT ( 'NONE',  ( 0.8751705887134423323, 24.81530984069208401, -41.19904111682483716 ) ) ;
#34823 = CIRCLE ( 'NONE', #7781, 47.91270532121795611 ) ;
#34824 = CARTESIAN_POINT ( 'NONE',  ( 0.7764139734771235979, 17.68681948199870035, -43.44210961173568109 ) ) ;
#34825 = ADVANCED_FACE ( 'NONE', ( #51064 ), #32297, .F. ) ;
#34826 = CARTESIAN_POINT ( 'NONE',  ( -2.739355103387247858, -14.76959508014213540, -2.169476462112044146 ) ) ;
#34827 = CARTESIAN_POINT ( 'NONE',  ( 1.088313998177380837, -42.64115081428568743, 4.827222641555085403 ) ) ;
#34828 = CARTESIAN_POINT ( 'NONE',  ( -16.29483284318931879, -7.897602733921581297, -1.291116304381162649 ) ) ;
#34829 = CARTESIAN_POINT ( 'NONE',  ( 0.3676999524040323597, -2.238562284876542741, 44.05609404179593724 ) ) ;
#34830 = CARTESIAN_POINT ( 'NONE',  ( 0.9968887458511658251, -37.48500720268744857, 20.88287852258433475 ) ) ;
#34831 = CARTESIAN_POINT ( 'NONE',  ( 0.8551540677456715978, 46.51172240253119838, 11.51835730326495977 ) ) ;
#34832 = CARTESIAN_POINT ( 'NONE',  ( 0.1157991065609915993, 39.71911272509257174, 19.21807612299130952 ) ) ;
#34833 = DIRECTION ( 'NONE',  ( -1.000000000000000000, -0.000000000000000000, -0.000000000000000000 ) ) ;
#34834 = CARTESIAN_POINT ( 'NONE',  ( 0.5819845901640501307, 33.54497622115130895, 34.18710267837666095 ) ) ;
#34835 = CARTESIAN_POINT ( 'NONE',  ( 5.895596859100789899, 20.06773179721813349, 1.346968346847024822 ) ) ;
#34836 = VECTOR ( 'NONE', #2626, 1000.000000000000114 ) ;
#34837 = ORIENTED_EDGE ( 'NONE', *, *, #23352, .T. ) ;
#34838 = AXIS2_PLACEMENT_3D ( 'NONE', #6894, #34281, #48068 ) ;
#34839 = CARTESIAN_POINT ( 'NONE',  ( 4.549368137175248350, -2.596185425822241211, 42.84816078363925840 ) ) ;
#34840 = CARTESIAN_POINT ( 'NONE',  ( 2.009741617377216460, 19.14496109139358637, -39.66074308976157425 ) ) ;
#34841 = CARTESIAN_POINT ( 'NONE',  ( 3.783198216974387851, -35.16829104054189514, 24.80909581868430180 ) ) ;
#34842 = VERTEX_POINT ( 'NONE', #53794 ) ;
#34843 = CARTESIAN_POINT ( 'NONE',  ( 0.9757787079277435716, 5.561523338227147839, 42.54650880470565255 ) ) ;
#34844 = DIRECTION ( 'NONE',  ( -1.000000000000000000, -0.000000000000000000, -0.000000000000000000 ) ) ;
#34845 = ORIENTED_EDGE ( 'NONE', *, *, #9195, .F. ) ;
#34846 = ORIENTED_EDGE ( 'NONE', *, *, #9250, .F. ) ;
#34847 = ADVANCED_FACE ( 'NONE', ( #10929 ), #31933, .F. ) ;
#34848 = FACE_OUTER_BOUND ( 'NONE', #34491, .T. ) ;
#34849 = ORIENTED_EDGE ( 'NONE', *, *, #6664, .F. ) ;
#34850 = B_SPLINE_CURVE_WITH_KNOTS ( 'NONE', 3,
 ( #30163, #48359, #48058, #34894, #24865, #5418, #44305, #24554, #19869, #53958, #58342, #28941, #5108, #38984, #58040, #34272, #10458, #29549, #10773 ),
 .UNSPECIFIED., .F., .F.,
 ( 4, 3, 3, 3, 3, 3, 4 ),
 ( 7.758025766973964006E-18, 0.0002612768053151714922, 0.0003919133833142863718, 0.0005225499612322580430, 0.0006531865391693282607, 0.0008112755173415173637, 0.0009693688056799695373 ),
 .UNSPECIFIED. ) ;
#34851 = CARTESIAN_POINT ( 'NONE',  ( -6.078726893082806448, -4.281536037413855134, -18.77398440473003305 ) ) ;
#34852 = ORIENTED_EDGE ( 'NONE', *, *, #60712, .F. ) ;
#34853 = ORIENTED_EDGE ( 'NONE', *, *, #39006, .F. ) ;
#34854 = CARTESIAN_POINT ( 'NONE',  ( -6.078726893082806448, 19.09748444646205456, 2.465791776663210033 ) ) ;
#34855 = VERTEX_POINT ( 'NONE', #30620 ) ;
#34856 = CARTESIAN_POINT ( 'NONE',  ( 5.331200000000000827, 0.000000000000000000, 15.38217999999999996 ) ) ;
#34857 = CARTESIAN_POINT ( 'NONE',  ( 0.9790724872846771065, -17.60412452180793963, -38.03196037285134423 ) ) ;
#34858 = ORIENTED_EDGE ( 'NONE', *, *, #16839, .F. ) ;
#34859 = CARTESIAN_POINT ( 'NONE',  ( -90.00000000000000000, 6.873330160214519262E-16, 5.612499999999999822 ) ) ;
#34860 = STYLED_ITEM ( 'NONE', ( #32204 ), #35493 ) ;
#34861 = LINE ( 'NONE', #30135, #37042 ) ;
#34862 = VECTOR ( 'NONE', #53210, 1000.000000000000114 ) ;
#34863 = VERTEX_POINT ( 'NONE', #54413 ) ;
#34864 = CARTESIAN_POINT ( 'NONE',  ( 4.553261556744875094, 0.000000000000000000, 0.000000000000000000 ) ) ;
#34865 = FACE_OUTER_BOUND ( 'NONE', #4281, .T. ) ;
#34866 = CARTESIAN_POINT ( 'NONE',  ( 0.6067375320500725255, 24.55990317723916050, -41.12099578548227896 ) ) ;
#34867 = CARTESIAN_POINT ( 'NONE',  ( 4.960386119450139297, 42.96877549456522871, 8.253532405581891496 ) ) ;
#34868 = B_SPLINE_CURVE_WITH_KNOTS ( 'NONE', 3,
 ( #60505, #12020, #40224, #17623 ),
 .UNSPECIFIED., .F., .F.,
 ( 4, 4 ),
 ( 2.145734436807298343E-17, 0.005004948556313821781 ),
 .UNSPECIFIED. ) ;
#34869 = ORIENTED_EDGE ( 'NONE', *, *, #54120, .F. ) ;
#34870 = CARTESIAN_POINT ( 'NONE',  ( 0.6000166863083106206, -20.35571918921390377, -44.69304395538888031 ) ) ;
#34871 = CARTESIAN_POINT ( 'NONE',  ( 0.1092355843206037486, 41.57624119012373143, 11.45151637801141931 ) ) ;
#34872 = B_SPLINE_CURVE_WITH_KNOTS ( 'NONE', 3,
 ( #35251, #24921, #54308, #11431 ),
 .UNSPECIFIED., .F., .F.,
 ( 4, 4 ),
 ( 1.734723475976807094E-18, 0.004444878191957671310 ),
 .UNSPECIFIED. ) ;
#34873 = EDGE_CURVE ( 'NONE', #4009, #27049, #20322, .T. ) ;
#34874 =( BOUNDED_SURFACE ( )  B_SPLINE_SURFACE ( 3, 1, ( 
 ( #14032, #24333 ),
 ( #38453, #14644 ),
 ( #47529, #9300 ),
 ( #52517, #61899 ) ),
 .UNSPECIFIED., .F., .F., .F. ) 
 B_SPLINE_SURFACE_WITH_KNOTS ( ( 4, 4 ),
 ( 2, 2 ),
 ( 0.000000000000000000, 1.000000000000000000 ),
 ( 0.000000000000000000, 1.000000000000000000 ),
 .UNSPECIFIED. ) 
 GEOMETRIC_REPRESENTATION_ITEM ( )  RATIONAL_B_SPLINE_SURFACE ( (
 ( 1.000000000000000000, 1.000000000000000000),
 ( 0.7223157951917476005, 0.9931996967497186413),
 ( 0.7223157951917476005, 0.9931996967497186413),
 ( 1.000000000000000000, 1.000000000000000000) ) ) 
 REPRESENTATION_ITEM ( '' )  SURFACE ( )  );
#34875 = CARTESIAN_POINT ( 'NONE',  ( 3.661933894777899212, 45.82839639926445585, -10.60137955284777256 ) ) ;
#34876 = CARTESIAN_POINT ( 'NONE',  ( 4.549368137175248350, 13.99871866169305434, 40.58005590356696501 ) ) ;
#34877 = VERTEX_POINT ( 'NONE', #16234 ) ;
#34878 = CARTESIAN_POINT ( 'NONE',  ( 0.6039202388192953519, -25.30794220682954787, 42.08410357967443360 ) ) ;
#34879 = EDGE_CURVE ( 'NONE', #30382, #47787, #52469, .T. ) ;
#34880 = CARTESIAN_POINT ( 'NONE',  ( 5.910764540655178756, 20.06626233353476962, -1.358806252166474771 ) ) ;
#34881 = DIRECTION ( 'NONE',  ( -1.000000000000000000, -0.000000000000000000, -0.000000000000000000 ) ) ;
#34882 = CIRCLE ( 'NONE', #25877, 85.00000000000001421 ) ;
#34883 = EDGE_CURVE ( 'NONE', #35798, #9554, #35304, .T. ) ;
#34884 = CONICAL_SURFACE ( 'NONE', #60875, 42.92674063221959813, 1.485477209440487556 ) ;
#34885 = VERTEX_POINT ( 'NONE', #20623 ) ;
#34886 = VERTEX_POINT ( 'NONE', #50053 ) ;
#34887 = CARTESIAN_POINT ( 'NONE',  ( -2.601141883200662974, -2.823446916239099380, -14.65686102071546948 ) ) ;
#34888 = ADVANCED_FACE ( 'NONE', ( #26233 ), #40369, .F. ) ;
#34889 = CARTESIAN_POINT ( 'NONE',  ( 2.299746137290199943, -2.858736841029653419, -48.95006599954567861 ) ) ;
#34890 = CARTESIAN_POINT ( 'NONE',  ( 0.9769922540276048117, 15.47377581453935314, -38.94732105199923211 ) ) ;
#34891 = DIRECTION ( 'NONE',  ( 1.000000000000000000, 0.000000000000000000, 0.000000000000000000 ) ) ;
#34892 = PRODUCT_DEFINITION_SHAPE ( 'NONE', 'NONE',  #61997 ) ;
#34893 = CARTESIAN_POINT ( 'NONE',  ( 0.2285344041767086165, 15.94802410072414212, 41.13589305677194830 ) ) ;
#34894 = CARTESIAN_POINT ( 'NONE',  ( 0.1152339509894530906, -31.54074419499066551, 30.85650897430565465 ) ) ;
#34895 = CARTESIAN_POINT ( 'NONE',  ( 0.9789233960466710016, 9.843146567393633362, -40.73633749473739130 ) ) ;
#34896 = FACE_OUTER_BOUND ( 'NONE', #3650, .T. ) ;
#34897 = CARTESIAN_POINT ( 'NONE',  ( 4.553261556744875094, -14.95853073564453339, -41.30111286702108941 ) ) ;
#34898 = CARTESIAN_POINT ( 'NONE',  ( -1.600000000000000089, -11.64055411052240352, -1.199999999999999956 ) ) ;
#34899 = CARTESIAN_POINT ( 'NONE',  ( 0.6029303876144825880, -6.409038528276480129, 47.67862422489722007 ) ) ;
#34900 = EDGE_CURVE ( 'NONE', #47955, #14355, #35973, .T. ) ;
#34901 = CIRCLE ( 'NONE', #56863, 2.649999999999992806 ) ;
#34902 = B_SPLINE_CURVE_WITH_KNOTS ( 'NONE', 3,
 ( #29946, #20860, #10536, #43776, #5192, #53427 ),
 .UNSPECIFIED., .F., .F.,
 ( 4, 2, 4 ),
 ( 5.485677294651095664E-18, 0.0002291472222819944263, 0.0004582944445639833774 ),
 .UNSPECIFIED. ) ;
#34903 = CARTESIAN_POINT ( 'NONE',  ( 0.8751705887134553219, 37.60752970653828697, -29.98056538504921065 ) ) ;
#34904 = CARTESIAN_POINT ( 'NONE',  ( 1.827326673878743923, -41.88502433275010617, 9.946825761453776948 ) ) ;
#34905 = EDGE_CURVE ( 'NONE', #50801, #26111, #5870, .T. ) ;
#34906 = CARTESIAN_POINT ( 'NONE',  ( 0.6845945791218034371, -34.20288208893667559, -32.10248241996619356 ) ) ;
#34907 = CARTESIAN_POINT ( 'NONE',  ( 0.7246131072078570989, -34.58859703353100201, 33.42811616637859373 ) ) ;
#34908 = CARTESIAN_POINT ( 'NONE',  ( 0.6025881611877911270, -46.52425620537277950, 12.24025891548842360 ) ) ;
#34909 = CARTESIAN_POINT ( 'NONE',  ( 0.1129192098497447394, 20.83764143887560749, 38.89401608281161060 ) ) ;
#34910 = ITEM_DEFINED_TRANSFORMATION ( 'NONE', 'NONE', #16893,  #14677 ) ;
#34911 = CARTESIAN_POINT ( 'NONE',  ( -2.601141883200665639, -14.31801740503244069, -4.217796232462731609 ) ) ;
#34912 = AXIS2_PLACEMENT_3D ( 'NONE', #11794, #40314, #49368 ) ;
#34913 = CARTESIAN_POINT ( 'NONE',  ( 0.9749527285493305717, -11.38116287125083304, 41.37154756071290507 ) ) ;
#34914 = CARTESIAN_POINT ( 'NONE',  ( -6.016489644550736315, 4.872725758886445213, -18.20227673842138927 ) ) ;
#34915 = CARTESIAN_POINT ( 'NONE',  ( 4.962356264823598373, -19.84272732133986139, 37.11471096901200895 ) ) ;
#34917 = ORIENTED_EDGE ( 'NONE', *, *, #46265, .F. ) ;
#34916 = DIRECTION ( 'NONE',  ( -1.000000000000000000, 8.881784197001252323E-16, 0.000000000000000000 ) ) ;
#34918 = ORIENTED_EDGE ( 'NONE', *, *, #40545, .T. ) ;
#34919 = CARTESIAN_POINT ( 'NONE',  ( 0.3622758884714730732, -33.69533458712361806, 26.89560658783328861 ) ) ;
#34920 = PLANE ( 'NONE',  #61500 ) ;
#34921 = CARTESIAN_POINT ( 'NONE',  ( 4.960386119450151732, -25.57375555595621464, -35.50238712307299949 ) ) ;
#34922 = ORIENTED_EDGE ( 'NONE', *, *, #53365, .F. ) ;
#34923 = VERTEX_POINT ( 'NONE', #7737 ) ;
#34924 = CARTESIAN_POINT ( 'NONE',  ( -6.077587904424778920, 0.6110050725289616347, 19.24636833782608392 ) ) ;
#34925 = DIRECTION ( 'NONE',  ( 1.000000000000000000, 0.000000000000000000, 0.000000000000000000 ) ) ;
#34926 = CARTESIAN_POINT ( 'NONE',  ( 0.000000000000000000, 0.000000000000000000, -0.3080913168122707546 ) ) ;
#34927 = ORIENTED_EDGE ( 'NONE', *, *, #33316, .T. ) ;
#34928 = ORIENTED_EDGE ( 'NONE', *, *, #3532, .T. ) ;
#34929 = EDGE_CURVE ( 'NONE', #59165, #27464, #37404, .T. ) ;
#34930 = CARTESIAN_POINT ( 'NONE',  ( 0.9730545539215883499, 42.90536227157002003, -0.5054011016614180507 ) ) ;
#34931 = VECTOR ( 'NONE', #31961, 999.9999999999998863 ) ;
#34932 = CARTESIAN_POINT ( 'NONE',  ( -6.078457390727109555, -17.35098001992619743, -8.350928294844221611 ) ) ;
#34933 = CARTESIAN_POINT ( 'NONE',  ( 0.6000166863083106206, 33.40185771989302310, -36.00193581695957334 ) ) ;
#34934 = CARTESIAN_POINT ( 'NONE',  ( 1.657374760986086271, -11.34341091359688569, 42.57014771054400626 ) ) ;
#34935 = CARTESIAN_POINT ( 'NONE',  ( 0.7245667037590772797, 19.16327388244000218, 44.12005358974313651 ) ) ;
#34936 = CARTESIAN_POINT ( 'NONE',  ( -6.015611763856276717, 18.84324252354755203, 0.006214430185208092740 ) ) ;
#34937 = CIRCLE ( 'NONE', #20933, 18.99999999999999645 ) ;
#34938 = CARTESIAN_POINT ( 'NONE',  ( 0.1158403557922069033, 15.27446809072172051, -41.39602555474792922 ) ) ;
#34939 = ORIENTED_EDGE ( 'NONE', *, *, #28719, .F. ) ;
#34940 = ORIENTED_EDGE ( 'NONE', *, *, #59875, .F. ) ;
#34941 = CARTESIAN_POINT ( 'NONE',  ( 4.833616638992208614, 41.27831852777643462, -20.86133030530247012 ) ) ;
#34942 = CARTESIAN_POINT ( 'NONE',  ( 5.880360259849739535, -36.03610316515405287, 31.66572319753499443 ) ) ;
#34943 = AXIS2_PLACEMENT_3D ( 'NONE', #13532, #32637, #51721 ) ;
#34944 = ORIENTED_EDGE ( 'NONE', *, *, #10021, .F. ) ;
#34945 = CARTESIAN_POINT ( 'NONE',  ( 2.643462169533600914, 34.93025802711726158, -32.97543604874639556 ) ) ;
#34946 = CARTESIAN_POINT ( 'NONE',  ( 0.3622758884714730732, -42.84426538328728640, -4.808133778521729518 ) ) ;
#34947 = DIRECTION ( 'NONE',  ( 0.000000000000000000, 0.000000000000000000, 1.000000000000000000 ) ) ;
#34948 = CARTESIAN_POINT ( 'NONE',  ( 0.1139756605157203340, -41.04710786557956226, -16.18919873145358679 ) ) ;
#34949 = ORIENTED_EDGE ( 'NONE', *, *, #14391, .F. ) ;
#34950 = CARTESIAN_POINT ( 'NONE',  ( 5.960721111146673579, 19.82781442290490403, 5.306302591836648652 ) ) ;
#34951 = CARTESIAN_POINT ( 'NONE',  ( 0.6029443199889047422, -35.27625851169997873, 34.16318526235686193 ) ) ;
#34952 = CARTESIAN_POINT ( 'NONE',  ( 0.8557997880470599172, -41.02602466100761802, -24.73961900479294584 ) ) ;
#34953 = CARTESIAN_POINT ( 'NONE',  ( 0.5782707292762423457, -42.18185855468838952, -20.50432058323027462 ) ) ;
#34954 = ORIENTED_EDGE ( 'NONE', *, *, #30133, .F. ) ;
#34955 = CARTESIAN_POINT ( 'NONE',  ( 0.5326698147273822848, 9.797174393178825657E-16, -8.000000000000000000 ) ) ;
#34956 = EDGE_CURVE ( 'NONE', #30066, #37909, #60553, .T. ) ;
#34957 = CARTESIAN_POINT ( 'NONE',  ( -99.49999999999975842, -9.184850993605117179E-15, 3.081487911019577365E-29 ) ) ;
#34958 = EDGE_LOOP ( 'NONE', ( #51805, #51321, #49166, #5100 ) ) ;
#34959 = LINE ( 'NONE', #35578, #34660 ) ;
#34960 = CARTESIAN_POINT ( 'NONE',  ( 0.7048096507298635682, -42.08020459959966075, -23.32077812596866551 ) ) ;
#34961 =( BOUNDED_SURFACE ( )  B_SPLINE_SURFACE ( 3, 1, ( 
 ( #29293, #48404 ),
 ( #29599, #34625 ),
 ( #54005, #6073 ),
 ( #44353, #58090 ) ),
 .UNSPECIFIED., .F., .F., .F. ) 
 B_SPLINE_SURFACE_WITH_KNOTS ( ( 4, 4 ),
 ( 2, 2 ),
 ( 0.000000000000000000, 1.000000000000000000 ),
 ( 0.000000000000000000, 1.000000000000000000 ),
 .UNSPECIFIED. ) 
 GEOMETRIC_REPRESENTATION_ITEM ( )  RATIONAL_B_SPLINE_SURFACE ( (
 ( 1.000000000000000000, 1.000000000000000000),
 ( 0.9953485035131437453, 0.8621029689291515030),
 ( 0.9953485035131437453, 0.8621029689291515030),
 ( 1.000000000000000000, 1.000000000000000000) ) ) 
 REPRESENTATION_ITEM ( '' )  SURFACE ( )  );
#34962 = VERTEX_POINT ( 'NONE', #31878 ) ;
#34963 = DIRECTION ( 'NONE',  ( 0.09722883295013592941, 0.6746907015591432355, 0.7316686485512315929 ) ) ;
#34964 = EDGE_CURVE ( 'NONE', #6050, #25842, #7521, .T. ) ;
#34965 = CARTESIAN_POINT ( 'NONE',  ( 5.895881250540457863, -11.93421320881288850, -16.18957185026512846 ) ) ;
#34966 = CARTESIAN_POINT ( 'NONE',  ( 4.962356264823608143, 0.000000000000000000, 0.000000000000000000 ) ) ;
#34967 = B_SPLINE_CURVE_WITH_KNOTS ( 'NONE', 3,
 ( #58540, #29433, #10653, #61973, #43259, #30053 ),
 .UNSPECIFIED., .F., .F.,
 ( 4, 2, 4 ),
 ( 3.496446946337351263E-18, 0.0002448709889506569398, 0.0004897419779013104102 ),
 .UNSPECIFIED. ) ;
#34968 = CARTESIAN_POINT ( 'NONE',  ( 0.8760168074887090262, -48.09529047980637273, 0.8912768426704575919 ) ) ;
#34969 = CARTESIAN_POINT ( 'NONE',  ( 0.1149546198390367230, 33.77510505806843355, -28.39346479983835181 ) ) ;
#34970 = CARTESIAN_POINT ( 'NONE',  ( 50.15577769773999961, 12.80000000000000071, 3.000000000000000000 ) ) ;
#34971 = CIRCLE ( 'NONE', #15961, 48.09070567114147110 ) ;
#34972 = DIRECTION ( 'NONE',  ( 3.273063162220391312E-16, -1.000000000000000000, -5.236901059552626099E-15 ) ) ;
#34973 = CARTESIAN_POINT ( 'NONE',  ( -4.473700000000000010, 0.000000000000000000, 0.000000000000000000 ) ) ;
#34974 = CARTESIAN_POINT ( 'NONE',  ( 0.1092355843206037486, -41.57624119012380959, -11.45151637801112976 ) ) ;
#34975 = CYLINDRICAL_SURFACE ( 'NONE', #2585, 15.43999999999999240 ) ;
#34976 = CARTESIAN_POINT ( 'NONE',  ( -2.601141883200662974, -7.351091256667716678, 12.99064605035223252 ) ) ;
#34977 =( BOUNDED_SURFACE ( )  B_SPLINE_SURFACE ( 3, 1, ( 
 ( #42732, #4466 ),
 ( #31784, #629 ),
 ( #46199, #41816 ),
 ( #23304, #19769 ) ),
 .UNSPECIFIED., .F., .F., .F. ) 
 B_SPLINE_SURFACE_WITH_KNOTS ( ( 4, 4 ),
 ( 2, 2 ),
 ( 0.000000000000000000, 1.000000000000000000 ),
 ( 0.000000000000000000, 1.000000000000000000 ),
 .UNSPECIFIED. ) 
 GEOMETRIC_REPRESENTATION_ITEM ( )  RATIONAL_B_SPLINE_SURFACE ( (
 ( 1.000000000000000000, 1.000000000000000000),
 ( 0.7223157951917476005, 0.9931996967497186413),
 ( 0.7223157951917476005, 0.9931996967497186413),
 ( 1.000000000000000000, 1.000000000000000000) ) ) 
 REPRESENTATION_ITEM ( '' )  SURFACE ( )  );
#34978 = DIRECTION ( 'NONE',  ( -1.000000000000000000, -0.000000000000000000, -0.000000000000000000 ) ) ;
#34979 = B_SPLINE_CURVE_WITH_KNOTS ( 'NONE', 3,
 ( #35435, #11619, #30704, #26019, #40450, #2184, #59513, #45454, #2503, #57488, #61277, #18703, #37837, #32811, #51568, #18396 ),
 .UNSPECIFIED., .F., .F.,
 ( 4, 3, 3, 3, 3, 4 ),
 ( 2.221635811791082109E-17, 0.0002618515315864343332, 0.0003927756766341896429, 0.0005236998216950500837, 0.0007855159896329812251, 0.001047349442285922232 ),
 .UNSPECIFIED. ) ;
#34981 = ORIENTED_EDGE ( 'NONE', *, *, #51450, .T. ) ;
#34980 = EDGE_CURVE ( 'NONE', #46743, #11571, #35183, .T. ) ;
#34983 = CARTESIAN_POINT ( 'NONE',  ( -17.29576878204978385, -12.34032024113386328, 1.992322322936505241 ) ) ;
#34982 =( BOUNDED_SURFACE ( )  B_SPLINE_SURFACE ( 3, 1, ( 
 ( #7497, #60131 ),
 ( #36361, #12547 ),
 ( #31639, #50726 ),
 ( #46071, #3116 ) ),
 .UNSPECIFIED., .F., .F., .F. ) 
 B_SPLINE_SURFACE_WITH_KNOTS ( ( 4, 4 ),
 ( 2, 2 ),
 ( 0.000000000000000000, 1.000000000000000000 ),
 ( 0.000000000000000000, 1.000000000000000000 ),
 .UNSPECIFIED. ) 
 GEOMETRIC_REPRESENTATION_ITEM ( )  RATIONAL_B_SPLINE_SURFACE ( (
 ( 1.000000000000000000, 1.000000000000000000),
 ( 0.7211978278499968642, 0.9934217856018975334),
 ( 0.7211978278499968642, 0.9934217856018975334),
 ( 1.000000000000000000, 1.000000000000000000) ) ) 
 REPRESENTATION_ITEM ( '' )  SURFACE ( )  );
#34984 = LINE ( 'NONE', #11470, #43431 ) ;
#34986 = ADVANCED_FACE ( 'NONE', ( #51570 ), #61541, .F. ) ;
#34985 = CARTESIAN_POINT ( 'NONE',  ( 0.5997462898726536595, 48.97040376101519144, -3.667585803694250135 ) ) ;
#34987 = CARTESIAN_POINT ( 'NONE',  ( -1.500000000000001332, 0.000000000000000000, 0.000000000000000000 ) ) ;
#34988 = CARTESIAN_POINT ( 'NONE',  ( 0.6029443449137436017, -19.91765779110959755, 44.88681817749597514 ) ) ;
#34989 = CARTESIAN_POINT ( 'NONE',  ( 0.8744876279028306332, -24.68559978112762110, 42.43785119236699188 ) ) ;
#34990 = CARTESIAN_POINT ( 'NONE',  ( 15.00000000000001421, -56.56854249492356246, 56.56854249492405984 ) ) ;
#34991 = CARTESIAN_POINT ( 'NONE',  ( 0.5998501479064708430, 17.92509395669044636, 44.64337787626254794 ) ) ;
#34992 = CARTESIAN_POINT ( 'NONE',  ( 0.6017667736363750963, -0.3491025323183876150, 48.10631678344240925 ) ) ;
#34993 = CARTESIAN_POINT ( 'NONE',  ( 0.8751705887134423323, -29.98056538504989277, 37.60752970653777538 ) ) ;
#34995 = EDGE_LOOP ( 'NONE', ( #18765, #9642, #33841, #12594 ) ) ;
#34994 = CARTESIAN_POINT ( 'NONE',  ( 0.7764146366350236361, -29.59659202960835600, 36.38794050096938548 ) ) ;
#34996 = ORIENTED_EDGE ( 'NONE', *, *, #41663, .F. ) ;
#34998 = VECTOR ( 'NONE', #60860, 1000.000000000000114 ) ;
#34997 = CARTESIAN_POINT ( 'NONE',  ( 0.8551540677456715978, -37.45266983663517379, 29.88829867897801051 ) ) ;
#34999 = FACE_BOUND ( 'NONE', #31914, .T. ) ;
#35000 = LINE ( 'NONE', #5520, #45836 ) ;
#35001 = CARTESIAN_POINT ( 'NONE',  ( 0.9722240750034576440, 0.5819398758580140996, 42.90442369954360657 ) ) ;
#35002 = CARTESIAN_POINT ( 'NONE',  ( 2.618530812446111078, -6.426312013671601875, -46.56639671588451534 ) ) ;
#35003 = CARTESIAN_POINT ( 'NONE',  ( 0.1103744047535531458, 41.66501489234563849, -11.12399292196393397 ) ) ;
#35004 = B_SPLINE_CURVE_WITH_KNOTS ( 'NONE', 3,
 ( #14659, #20280, #58449, #843, #48766, #43171 ),
 .UNSPECIFIED., .F., .F.,
 ( 4, 2, 4 ),
 ( 4.907736672678014827E-18, 0.0002291966416970822227, 0.0004583932833941595664 ),
 .UNSPECIFIED. ) ;
#35005 = ORIENTED_EDGE ( 'NONE', *, *, #41056, .F. ) ;
#35006 = VERTEX_POINT ( 'NONE', #51269 ) ;
#35007 = EDGE_CURVE ( 'NONE', #40188, #32685, #11182, .T. ) ;
#35008 = CARTESIAN_POINT ( 'NONE',  ( 0.8557997880470690211, -43.90420959842193582, 19.17299735371994629 ) ) ;
#35009 = CARTESIAN_POINT ( 'NONE',  ( 0.1101816497532063510, -11.29256821151185086, -41.61967362528552883 ) ) ;
#35010 = CARTESIAN_POINT ( 'NONE',  ( 0.8557997880470599172, 41.93815086860288943, -23.15977007032279289 ) ) ;
#35011 = ORIENTED_EDGE ( 'NONE', *, *, #1734, .T. ) ;
#35012 = LINE ( 'NONE', #25586, #36631 ) ;
#35013 = CARTESIAN_POINT ( 'NONE',  ( 4.960386119450134856, 23.93873278148718597, 36.62476672265492539 ) ) ;
#35014 = ORIENTED_EDGE ( 'NONE', *, *, #19966, .F. ) ;
#35015 = CARTESIAN_POINT ( 'NONE',  ( 0.9762797500689124330, -40.96497924994823592, 8.842808390834631993 ) ) ;
#35016 = ORIENTED_EDGE ( 'NONE', *, *, #4988, .T. ) ;
#35017 = CARTESIAN_POINT ( 'NONE',  ( 2.624215991343620935, 13.78323291683783758, 45.98641578154036580 ) ) ;
#35019 = CARTESIAN_POINT ( 'NONE',  ( 0.6064782688330858651, -46.83443355140296660, 2.422866141161769349 ) ) ;
#35018 = CIRCLE ( 'NONE', #61011, 43.92652462719577500 ) ;
#35020 = B_SPLINE_CURVE_WITH_KNOTS ( 'NONE', 3,
 ( #3424, #22560, #35755, #36064, #46377, #26325, #41684, #31031, #32271, #36369, #45460, #51352, #3126, #55435, #22256, #31648, #26950, #41378, #12250 ),
 .UNSPECIFIED., .F., .F.,
 ( 4, 3, 3, 3, 3, 3, 4 ),
 ( 9.813676791237319219E-18, 0.0002724573126191738581, 0.0004086839781548484772, 0.0005449106435901825704, 0.0006811373090491529758, 0.0008459866663933752291, 0.001010840725717212282 ),
 .UNSPECIFIED. ) ;
#35021 = ORIENTED_EDGE ( 'NONE', *, *, #56283, .T. ) ;
#35022 = CARTESIAN_POINT ( 'NONE',  ( 4.975801465491694664, -26.14269827151650816, -40.15204426031524321 ) ) ;
#35023 = CARTESIAN_POINT ( 'NONE',  ( 0.5797568599927140909, 46.89167813021173004, 0.6291508591968832942 ) ) ;
#35024 = CARTESIAN_POINT ( 'NONE',  ( -3.344563996438217224, -2.687817229851499068, -5.441324518471498450 ) ) ;
#35025 = DIRECTION ( 'NONE',  ( 0.09722883295013597105, 0.5755877901554996567, -0.8119391909909651206 ) ) ;
#35026 = B_SPLINE_CURVE_WITH_KNOTS ( 'NONE', 3,
 ( #44449, #20311, #1478, #53784, #34719, #39433, #53186, #34112, #20612, #10290, #58485, #35343, #39126, #20915, #59112, #11524 ),
 .UNSPECIFIED., .F., .F.,
 ( 4, 3, 3, 3, 3, 4 ),
 ( 2.221635811791082109E-17, 0.0002612764279487725665, 0.0003919131003184764804, 0.0005225497727000608106, 0.0007837925190632426438, 0.001045051706266715216 ),
 .UNSPECIFIED. ) ;
#35027 = ORIENTED_EDGE ( 'NONE', *, *, #6143, .T. ) ;
#35028 = CARTESIAN_POINT ( 'NONE',  ( 4.694002226626921015, 45.58690636503205695, 0.3445860007825484739 ) ) ;
#35029 = CARTESIAN_POINT ( 'NONE',  ( 0.6017667736363750963, 44.57803721604151548, -18.08696174077343954 ) ) ;
#35030 = ORIENTED_EDGE ( 'NONE', *, *, #21230, .F. ) ;
#35031 = CARTESIAN_POINT ( 'NONE',  ( 4.956653778116975495, -14.93973939759918323, 45.71126949320244393 ) ) ;
#35032 = VERTEX_POINT ( 'NONE', #37207 ) ;
#35033 = CARTESIAN_POINT ( 'NONE',  ( 0.9788927965476041937, 4.335847588109925432, 41.68377428118113670 ) ) ;
#35034 = EDGE_CURVE ( 'NONE', #47897, #6436, #10544, .T. ) ;
#35035 = VERTEX_POINT ( 'NONE', #31559 ) ;
#35036 = DIRECTION ( 'NONE',  ( 0.07439287786467664587, -0.9161872986448699185, -0.3937848822959399420 ) ) ;
#35037 = CARTESIAN_POINT ( 'NONE',  ( 0.9790320750461898314, 36.10202571947430528, -21.28334728121043895 ) ) ;
#35038 = CARTESIAN_POINT ( 'NONE',  ( 0.9741495583595176644, 33.79932324264184729, 26.43366215195271351 ) ) ;
#35039 = VERTEX_POINT ( 'NONE', #22778 ) ;
#35040 = CARTESIAN_POINT ( 'NONE',  ( 0.5819845079324663661, 6.701571823032717923, 47.42480735454289231 ) ) ;
#35041 = ADVANCED_FACE ( 'NONE', ( #36582 ), #59535, .F. ) ;
#35042 = CARTESIAN_POINT ( 'NONE',  ( 4.962356264823608143, 34.94214251265138671, -23.45809613945485950 ) ) ;
#35043 = CARTESIAN_POINT ( 'NONE',  ( 5.880360259849752858, 39.86101557989634614, 26.69116321728584751 ) ) ;
#35044 = ORIENTED_EDGE ( 'NONE', *, *, #25341, .F. ) ;
#35045 = B_SPLINE_CURVE_WITH_KNOTS ( 'NONE', 3,
 ( #59355, #6104, #30238, #44681, #34649, #11779 ),
 .UNSPECIFIED., .F., .F.,
 ( 4, 2, 4 ),
 ( 1.029992063861229212E-18, 0.0002293801035737119199, 0.0004587602071474228098 ),
 .UNSPECIFIED. ) ;
#35046 = EDGE_CURVE ( 'NONE', #34160, #7089, #18398, .T. ) ;
#35047 = ORIENTED_EDGE ( 'NONE', *, *, #23064, .F. ) ;
#35048 = CARTESIAN_POINT ( 'NONE',  ( 2.281448460670571610, -25.11570011049342455, -40.87338159040662333 ) ) ;
#35049 = CARTESIAN_POINT ( 'NONE',  ( 4.553261556744875094, 31.39705178283641018, 30.72075365562384519 ) ) ;
#35050 = CARTESIAN_POINT ( 'NONE',  ( 0.3622758884714730732, 25.58609868863768355, -34.70015533914803285 ) ) ;
#35051 = CARTESIAN_POINT ( 'NONE',  ( 0.1100247026804066219, 30.37337782329848679, 30.61332956994592536 ) ) ;
#35052 = CARTESIAN_POINT ( 'NONE',  ( 0.9775691876210972353, -26.76781511548317383, -32.24620571374718736 ) ) ;
#35053 = CARTESIAN_POINT ( 'NONE',  ( 0.9783242366443545279, 38.47773455156494293, 16.60718019369418386 ) ) ;
#35054 = VERTEX_POINT ( 'NONE', #26549 ) ;
#35055 = CARTESIAN_POINT ( 'NONE',  ( 0.7056555295713294873, 7.085402321211779153, 47.37451042924655553 ) ) ;
#35056 = ORIENTED_EDGE ( 'NONE', *, *, #10443, .F. ) ;
#35057 = CARTESIAN_POINT ( 'NONE',  ( 0.1129192098497447394, -38.68182264534125636, -21.22895156665819627 ) ) ;
#35059 = EDGE_CURVE ( 'NONE', #19501, #45323, #56126, .T. ) ;
#35058 = CARTESIAN_POINT ( 'NONE',  ( 47.93486876061941615, 15.48568014845115748, 0.6873655611129172449 ) ) ;
#35060 = CARTESIAN_POINT ( 'NONE',  ( 3.376099380956842921, -6.821144471874572623, 11.54038005118904131 ) ) ;
#35061 = CARTESIAN_POINT ( 'NONE',  ( 0.5809828226811548646, -47.41188724015884048, 6.791453954330148868 ) ) ;
#35062 = CARTESIAN_POINT ( 'NONE',  ( 3.221118495291109163, 11.62016450294477998, 42.42326244628355880 ) ) ;
#35063 = CARTESIAN_POINT ( 'NONE',  ( 5.896782393890504181, -17.30187591025955030, -10.25529994022567237 ) ) ;
#35064 =( BOUNDED_SURFACE ( )  B_SPLINE_SURFACE ( 3, 1, ( 
 ( #36990, #8141 ),
 ( #60746, #36671 ),
 ( #12869, #9064 ),
 ( #18473, #61060 ) ),
 .UNSPECIFIED., .F., .F., .F. ) 
 B_SPLINE_SURFACE_WITH_KNOTS ( ( 4, 4 ),
 ( 2, 2 ),
 ( 0.000000000000000000, 1.000000000000000000 ),
 ( 0.000000000000000000, 1.000000000000000000 ),
 .UNSPECIFIED. ) 
 GEOMETRIC_REPRESENTATION_ITEM ( )  RATIONAL_B_SPLINE_SURFACE ( (
 ( 1.000000000000000000, 1.000000000000000000),
 ( 0.7211978278499970862, 0.9934217856018976445),
 ( 0.7211978278499970862, 0.9934217856018976445),
 ( 1.000000000000000000, 1.000000000000000000) ) ) 
 REPRESENTATION_ITEM ( '' )  SURFACE ( )  );
#35065 = CARTESIAN_POINT ( 'NONE',  ( 0.1145239942831223490, 20.69812692061546144, -38.96835925058644534 ) ) ;
#35066 = CARTESIAN_POINT ( 'NONE',  ( 0.1129192098497455998, 30.02178898772931603, -32.33641869102712718 ) ) ;
#35067 = CARTESIAN_POINT ( 'NONE',  ( 5.960721111146673579, -20.52557019979492026, 0.006321279846751705171 ) ) ;
#35068 = CARTESIAN_POINT ( 'NONE',  ( 1.231276596079887264, -0.5545928549379750550, 41.91621640586514985 ) ) ;
#35069 = CARTESIAN_POINT ( 'NONE',  ( 0.1064266379913941102, 0.5615183164811746730, 43.12102052820964104 ) ) ;
#35070 = CARTESIAN_POINT ( 'NONE',  ( 0.5549461598389363592, -22.10837605659374461, 38.16329917089240098 ) ) ;
#35071 = CARTESIAN_POINT ( 'NONE',  ( 3.376099380956838925, 12.80002687883560419, 3.983427611135065494 ) ) ;
#35072 = DIRECTION ( 'NONE',  ( 0.000000000000000000, 0.000000000000000000, -1.000000000000000000 ) ) ;
#35073 = CARTESIAN_POINT ( 'NONE',  ( 0.6067375320500714153, -47.38951440911012014, -6.954068056451214730 ) ) ;
#35074 = CIRCLE ( 'NONE', #42062, 0.05882000000000109363 ) ;
#35075 = ORIENTED_EDGE ( 'NONE', *, *, #45100, .T. ) ;
#35076 = DIRECTION ( 'NONE',  ( 0.000000000000000000, 0.000000000000000000, 1.000000000000000000 ) ) ;
#35077 = AXIS2_PLACEMENT_3D ( 'NONE', #27242, #18460, #8125 ) ;
#35078 = CARTESIAN_POINT ( 'NONE',  ( 0.1073791018717483448, 43.12183934961191056, -0.4849339620928847516 ) ) ;
#35079 = CARTESIAN_POINT ( 'NONE',  ( 0.8551540677456834771, -47.37911285756625546, 7.157691013574193128 ) ) ;
#35080 = CARTESIAN_POINT ( 'NONE',  ( -6.077587904424778920, -12.95044751835546393, 14.25068175450744157 ) ) ;
#35081 = CARTESIAN_POINT ( 'NONE',  ( 0.1092565886968784317, -41.57372480460693254, 11.46097737058291344 ) ) ;
#35082 = ORIENTED_EDGE ( 'NONE', *, *, #32155, .F. ) ;
#35083 = EDGE_CURVE ( 'NONE', #55130, #23728, #58321, .T. ) ;
#35084 = CARTESIAN_POINT ( 'NONE',  ( 4.975801465491695552, -47.10002938642136883, -8.787181743659990829 ) ) ;
#35085 = CARTESIAN_POINT ( 'NONE',  ( 0.5997462898726536595, 16.46871699354542429, -46.26373299606095202 ) ) ;
#35086 = EDGE_CURVE ( 'NONE', #2003, #35399, #32202, .T. ) ;
#35087 = CARTESIAN_POINT ( 'NONE',  ( 0.2940133293163011974, 43.96669231856046878, 3.629120574337435734 ) ) ;
#35088 = ORIENTED_EDGE ( 'NONE', *, *, #29079, .F. ) ;
#35089 = LINE ( 'NONE', #41561, #58010 ) ;
#35090 = ADVANCED_FACE ( 'NONE', ( #33739 ), #19496, .F. ) ;
#35091 = CARTESIAN_POINT ( 'NONE',  ( 0.8751705887134423323, -33.37254303619531726, -34.63284514348573850 ) ) ;
#35092 = ORIENTED_EDGE ( 'NONE', *, *, #25662, .T. ) ;
#35093 = CARTESIAN_POINT ( 'NONE',  ( 5.965394784446460541, -0.01447339372467435804, 20.52536205633085231 ) ) ;
#35094 = ORIENTED_EDGE ( 'NONE', *, *, #21221, .F. ) ;
#35095 = CARTESIAN_POINT ( 'NONE',  ( 1.199999999999992628, 0.000000000000000000, 0.000000000000000000 ) ) ;
#35096 = VERTEX_POINT ( 'NONE', #13705 ) ;
#35097 = DIRECTION ( 'NONE',  ( -1.000000000000000000, -0.000000000000000000, -0.000000000000000000 ) ) ;
#35098 = CARTESIAN_POINT ( 'NONE',  ( 0.7954190325252809002, 41.21355377862698788, -24.79809930825941677 ) ) ;
#35099 = EDGE_LOOP ( 'NONE', ( #46555, #61661, #59802, #33101 ) ) ;
#35100 = EDGE_LOOP ( 'NONE', ( #61109, #54555, #13906, #1856 ) ) ;
#35101 = CARTESIAN_POINT ( 'NONE',  ( 5.895881250540457863, 16.58446435569113220, 11.37906954206324173 ) ) ;
#35102 = B_SPLINE_CURVE_WITH_KNOTS ( 'NONE', 3,
 ( #33907, #25103, #38928, #57980, #4728, #52983, #34516, #15102, #10398, #29489, #48598, #29799, #5961, #23874, #44245, #43005, #44553, #2201, #21030 ),
 .UNSPECIFIED., .F., .F.,
 ( 4, 3, 3, 3, 3, 3, 4 ),
 ( 8.674676106452504675E-19, 0.0002612768053151721427, 0.0003919133833142923349, 0.0005225499612322608619, 0.0006531865391693370427, 0.0008112755173415195321, 0.0009693688056799730068 ),
 .UNSPECIFIED. ) ;
#35103 = CARTESIAN_POINT ( 'NONE',  ( 0.5850706913938533704, -12.57184842332050145, 46.21698775168641760 ) ) ;
#35104 = ORIENTED_EDGE ( 'NONE', *, *, #60290, .F. ) ;
#35105 = EDGE_CURVE ( 'NONE', #11373, #17098, #9756, .T. ) ;
#35106 = VERTEX_POINT ( 'NONE', #14942 ) ;
#35107 = CARTESIAN_POINT ( 'NONE',  ( 5.896782393890504181, 16.57826022845085134, 11.38803647148080778 ) ) ;
#35108 = CARTESIAN_POINT ( 'NONE',  ( 2.706805983486679779, -36.23450656517427149, -24.97672210875754928 ) ) ;
#35109 = CARTESIAN_POINT ( 'NONE',  ( 2.648799415243696664, -34.24682227764476750, -35.09519379021880070 ) ) ;
#35110 = CARTESIAN_POINT ( 'NONE',  ( -6.078457390727109555, 17.85037638348246958, -7.222089310270190410 ) ) ;
#35111 = ORIENTED_EDGE ( 'NONE', *, *, #41485, .T. ) ;
#35112 = EDGE_CURVE ( 'NONE', #56726, #41729, #30723, .T. ) ;
#35113 = CARTESIAN_POINT ( 'NONE',  ( -6.078075953587585900, -18.27338415406079619, -6.072775790794155526 ) ) ;
#35114 = CARTESIAN_POINT ( 'NONE',  ( -2.601141883200665639, -14.73982649082953600, -2.352220756992938089 ) ) ;
#35115 = ORIENTED_EDGE ( 'NONE', *, *, #30610, .T. ) ;
#35116 = CARTESIAN_POINT ( 'NONE',  ( 0.5837157313716019313, -46.78513062885863860, -3.223137543242450054 ) ) ;
#35117 = B_SPLINE_CURVE_WITH_KNOTS ( 'NONE', 3,
 ( #21602, #46053, #46656, #11922 ),
 .UNSPECIFIED., .F., .F.,
 ( 4, 4 ),
 ( 2.147596245779529078E-17, 0.004559932413162189405 ),
 .UNSPECIFIED. ) ;
#35118 = EDGE_CURVE ( 'NONE', #35637, #13776, #46392, .T. ) ;
#35119 = ORIENTED_EDGE ( 'NONE', *, *, #42025, .T. ) ;
#35120 = CIRCLE ( 'NONE', #31077, 48.09070567114147110 ) ;
#35121 = CARTESIAN_POINT ( 'NONE',  ( 0.8751705887134423323, 23.27176129838367302, 42.09020928323383259 ) ) ;
#35122 = CARTESIAN_POINT ( 'NONE',  ( 0.9762797500689124330, 40.55021165774366665, -10.58324712448374605 ) ) ;
#35123 = ORIENTED_EDGE ( 'NONE', *, *, #8137, .T. ) ;
#35124 = CARTESIAN_POINT ( 'NONE',  ( 0.9780106845699478857, -12.11659434839023142, -40.11881588297436707 ) ) ;
#35125 = CARTESIAN_POINT ( 'NONE',  ( 0.5988103564986354543, 37.79415694022860350, -29.76496605343807289 ) ) ;
#35126 = CARTESIAN_POINT ( 'NONE',  ( 52.81518117642549726, 12.43264790761136851, -1.334736769217753638 ) ) ;
#35127 = CARTESIAN_POINT ( 'NONE',  ( 3.678834586032788234, 45.86476391165511046, 17.17660621183629033 ) ) ;
#35128 = VERTEX_POINT ( 'NONE', #42521 ) ;
#35129 = CARTESIAN_POINT ( 'NONE',  ( 0.5980894510889457338, 38.59343625445407611, 28.72954109785617405 ) ) ;
#35130 = CARTESIAN_POINT ( 'NONE',  ( 0.8751705887134423323, 44.08562551107055327, 19.22545746485676688 ) ) ;
#35132 = EDGE_CURVE ( 'NONE', #58688, #59308, #52162, .T. ) ;
#35131 = CARTESIAN_POINT ( 'NONE',  ( 1.227938101723748288, 33.52879263017863565, 26.79402671879338271 ) ) ;
#35133 = CARTESIAN_POINT ( 'NONE',  ( 4.960386119450151732, 27.88794419592712615, 33.71496749512290592 ) ) ;
#35134 = DIRECTION ( 'NONE',  ( -1.000000000000000000, 1.776356839400250465E-15, 0.000000000000000000 ) ) ;
#35135 = CARTESIAN_POINT ( 'NONE',  ( 4.967162193818130511, -3.259922920617460029, -42.96271701169388280 ) ) ;
#35136 = B_SPLINE_CURVE_WITH_KNOTS ( 'NONE', 3,
 ( #9213, #4485, #43370, #57413 ),
 .UNSPECIFIED., .F., .F.,
 ( 4, 4 ),
 ( 2.189128766608093472E-17, 0.004559932413162189405 ),
 .UNSPECIFIED. ) ;
#35137 = CARTESIAN_POINT ( 'NONE',  ( -5.331200000000000827, 0.000000000000000000, 0.000000000000000000 ) ) ;
#35138 = LINE ( 'NONE', #48596, #15420 ) ;
#35139 = CARTESIAN_POINT ( 'NONE',  ( 0.8744876279028306332, 40.65405044375329879, -27.52450240960324024 ) ) ;
#35140 = DIRECTION ( 'NONE',  ( 0.09835009131224552170, 0.6981896185982721104, -0.7091251765523998163 ) ) ;
#35141 = CARTESIAN_POINT ( 'NONE',  ( 0.7056313189692707821, -6.968533899719071556, 46.38090317410846097 ) ) ;
#35142 = CARTESIAN_POINT ( 'NONE',  ( 0.6000166863083090663, -45.32251430608251042, -18.91277818522175735 ) ) ;
#35143 = CARTESIAN_POINT ( 'NONE',  ( 0.1152809850208375564, 36.85883374870061857, 24.25637353718406786 ) ) ;
#35144 = ORIENTED_EDGE ( 'NONE', *, *, #19903, .F. ) ;
#35145 = CARTESIAN_POINT ( 'NONE',  ( 4.956445790444027999, 20.31112743693101663, -42.48524629068760561 ) ) ;
#35146 = LINE ( 'NONE', #1591, #465 ) ;
#35147 = DIRECTION ( 'NONE',  ( -1.000000000000000000, -0.000000000000000000, -0.000000000000000000 ) ) ;
#35148 = ORIENTED_EDGE ( 'NONE', *, *, #9474, .T. ) ;
#35149 = ADVANCED_FACE ( 'NONE', ( #28395 ), #48755, .F. ) ;
#35150 = CARTESIAN_POINT ( 'NONE',  ( 5.974727161628367256, 5.327229920347150482, 19.82156119440447384 ) ) ;
#35151 = CARTESIAN_POINT ( 'NONE',  ( 0.9730545539215883499, -5.099196237955184507, 42.60426903087352457 ) ) ;
#35152 = B_SPLINE_CURVE_WITH_KNOTS ( 'NONE', 3,
 ( #13467, #13785, #46676, #51344, #31955, #60736 ),
 .UNSPECIFIED., .F., .F.,
 ( 4, 2, 4 ),
 ( 1.738108305489988542E-18, 0.0002291459268755697198, 0.0004582918537511377049 ),
 .UNSPECIFIED. ) ;
#35153 = EDGE_CURVE ( 'NONE', #58534, #6671, #16536, .T. ) ;
#35154 = CARTESIAN_POINT ( 'NONE',  ( 0.5998501479064708430, -11.94461217097437000, -46.60114184914313995 ) ) ;
#35156 = ORIENTED_EDGE ( 'NONE', *, *, #134, .T. ) ;
#35155 = AXIS2_PLACEMENT_3D ( 'NONE', #29565, #23952, #58056 ) ;
#35157 = CARTESIAN_POINT ( 'NONE',  ( 0.3622758884714600280, 37.74294673546586409, -20.83792692158932525 ) ) ;
#35158 = CARTESIAN_POINT ( 'NONE',  ( 0.8753041380234530822, 21.91949880997755429, -43.93943445007425908 ) ) ;
#35159 = EDGE_CURVE ( 'NONE', #37959, #25757, #37220, .T. ) ;
#35160 = ORIENTED_EDGE ( 'NONE', *, *, #45023, .F. ) ;
#35161 = ADVANCED_FACE ( 'NONE', ( #56588 ), #14739, .F. ) ;
#35162 = CARTESIAN_POINT ( 'NONE',  ( 0.6026777506516368677, 11.09719736516042943, 47.83720938010385026 ) ) ;
#35163 = EDGE_CURVE ( 'NONE', #52281, #43273, #15761, .T. ) ;
#35164 = EDGE_LOOP ( 'NONE', ( #9652, #36948, #41343, #55531 ) ) ;
#35165 = ORIENTED_EDGE ( 'NONE', *, *, #25283, .T. ) ;
#35166 = CARTESIAN_POINT ( 'NONE',  ( 3.376099380956838925, 6.842217874692699375, -11.52789825541945312 ) ) ;
#35167 = ORIENTED_EDGE ( 'NONE', *, *, #44909, .F. ) ;
#35168 = FACE_OUTER_BOUND ( 'NONE', #35475, .T. ) ;
#35169 = DIRECTION ( 'NONE',  ( 0.07439287786467665975, 0.8701500408883677817, -0.4871392060437993443 ) ) ;
#35170 = VERTEX_POINT ( 'NONE', #8410 ) ;
#35171 = CARTESIAN_POINT ( 'NONE',  ( 1.157643937452368599, -21.85425515765621540, 35.76861481940291299 ) ) ;
#35172 =( REPRESENTATION_RELATIONSHIP ('NONE','NONE', #44881, #27649 ) REPRESENTATION_RELATIONSHIP_WITH_TRANSFORMATION ( #18032 )SHAPE_REPRESENTATION_RELATIONSHIP( ) );
#35173 = EDGE_CURVE ( 'NONE', #42065, #34651, #23151, .T. ) ;
#35174 =( BOUNDED_SURFACE ( )  B_SPLINE_SURFACE ( 3, 1, ( 
 ( #46017, #60075 ),
 ( #50667, #23410 ),
 ( #8998, #60993 ),
 ( #42238, #61600 ) ),
 .UNSPECIFIED., .F., .F., .F. ) 
 B_SPLINE_SURFACE_WITH_KNOTS ( ( 4, 4 ),
 ( 2, 2 ),
 ( 0.000000000000000000, 1.000000000000000000 ),
 ( 0.000000000000000000, 1.000000000000000000 ),
 .UNSPECIFIED. ) 
 GEOMETRIC_REPRESENTATION_ITEM ( )  RATIONAL_B_SPLINE_SURFACE ( (
 ( 1.000000000000000000, 1.000000000000000000),
 ( 0.9953390228620291325, 0.8624445117760984880),
 ( 0.9953390228620291325, 0.8624445117760984880),
 ( 1.000000000000000000, 1.000000000000000000) ) ) 
 REPRESENTATION_ITEM ( '' )  SURFACE ( )  );
#35175 = DIRECTION ( 'NONE',  ( 1.000000000000000000, 0.000000000000000000, 0.000000000000000000 ) ) ;
#35176 = ADVANCED_FACE ( 'NONE', ( #37263 ), #61904, .F. ) ;
#35177 = ORIENTED_EDGE ( 'NONE', *, *, #18245, .F. ) ;
#35178 = CARTESIAN_POINT ( 'NONE',  ( 0.2940135542859015905, 43.44929869485245177, 7.641923293053564770 ) ) ;
#35179 = CARTESIAN_POINT ( 'NONE',  ( 50.50000000000000000, 12.21587082446438011, 2.649999999999992806 ) ) ;
#35180 = DIRECTION ( 'NONE',  ( -0.000000000000000000, 0.000000000000000000, -1.000000000000000000 ) ) ;
#35181 = CARTESIAN_POINT ( 'NONE',  ( 0.9787284016396613495, 36.15334032947335174, 21.19603693972311476 ) ) ;
#35182 = VERTEX_POINT ( 'NONE', #9348 ) ;
#35183 = B_SPLINE_CURVE_WITH_KNOTS ( 'NONE', 3,
 ( #3041, #36906, #12787, #41293, #50652, #45999 ),
 .UNSPECIFIED., .F., .F.,
 ( 4, 2, 4 ),
 ( 4.770489558936219510E-18, 0.0002291472222819939926, 0.0004582944445639832148 ),
 .UNSPECIFIED. ) ;
#35184 = VERTEX_POINT ( 'NONE', #24071 ) ;
#35185 = CARTESIAN_POINT ( 'NONE',  ( 4.956445790444018229, -10.39006634428234577, -45.93021414603951058 ) ) ;
#35186 = DIRECTION ( 'NONE',  ( 1.000000000000000000, 0.000000000000000000, 0.000000000000000000 ) ) ;
#35187 = CARTESIAN_POINT ( 'NONE',  ( 3.678748215320119197, 29.51641561576747463, 39.08188868896642987 ) ) ;
#35188 = VERTEX_POINT ( 'NONE', #52250 ) ;
#35189 = CARTESIAN_POINT ( 'NONE',  ( 4.975801465491694664, 8.787181743659507660, 47.10002938642145409 ) ) ;
#35190 = CARTESIAN_POINT ( 'NONE',  ( 4.967162193818130511, -38.44485641567084855, 19.45289607368810181 ) ) ;
#35191 = CARTESIAN_POINT ( 'NONE',  ( 5.901463166500146684, 20.06674442072660369, -1.357806574543771960 ) ) ;
#35192 = CARTESIAN_POINT ( 'NONE',  ( 0.3622758884714600280, 6.444611261694588755, -42.62881903538203687 ) ) ;
#35193 = ORIENTED_EDGE ( 'NONE', *, *, #42260, .F. ) ;
#35194 = ORIENTED_EDGE ( 'NONE', *, *, #57065, .F. ) ;
#35195 = CARTESIAN_POINT ( 'NONE',  ( 5.974727161628369032, 16.27409205901359002, 12.50710176110013272 ) ) ;
#35196 = CARTESIAN_POINT ( 'NONE',  ( 0.1073791018717578927, 26.63563652260167203, -33.91564619577780348 ) ) ;
#35197 = CARTESIAN_POINT ( 'NONE',  ( 0.9788927965476027504, 14.92997836612718210, -39.15906483330202548 ) ) ;
#35199 = EDGE_CURVE ( 'NONE', #50474, #36178, #21744, .T. ) ;
#35198 = FACE_OUTER_BOUND ( 'NONE', #20737, .T. ) ;
#35200 = CIRCLE ( 'NONE', #8167, 10.00000000000000000 ) ;
#35201 = CARTESIAN_POINT ( 'NONE',  ( 0.1313383488274132704, -43.11882601516400371, 0.6377633466099100756 ) ) ;
#35202 = CIRCLE ( 'NONE', #31153, 0.7500000000000015543 ) ;
#35203 = EDGE_CURVE ( 'NONE', #6434, #14965, #53131, .T. ) ;
#35204 = FACE_OUTER_BOUND ( 'NONE', #3106, .T. ) ;
#35205 = CARTESIAN_POINT ( 'NONE',  ( 4.553261556744873317, 31.71129487083125653, 30.39627186743183174 ) ) ;
#35206 = CARTESIAN_POINT ( 'NONE',  ( 4.834790513006555379, 19.54670848745931266, 43.01761881172255642 ) ) ;
#35207 = CARTESIAN_POINT ( 'NONE',  ( 2.643462169533613793, 46.73820883660191328, 11.09243630552549398 ) ) ;
#35208 = CARTESIAN_POINT ( 'NONE',  ( 5.901764892641288895, 35.14701960959055071, -34.09807149975986107 ) ) ;
#35209 = DIRECTION ( 'NONE',  ( 0.07500201931887538753, -0.7028774959225082553, 0.7073456883474977808 ) ) ;
#35210 = CARTESIAN_POINT ( 'NONE',  ( 0.5782707292762423457, 33.12197115878034026, 33.20649605520795689 ) ) ;
#35211 = PRODUCT_RELATED_PRODUCT_CATEGORY ( 'part', '', ( #3260 ) ) ;
#35212 = CARTESIAN_POINT ( 'NONE',  ( -6.010958268070873523, -14.95835081545466139, -11.45964880703842326 ) ) ;
#35213 = CARTESIAN_POINT ( 'NONE',  ( 4.975801465491695552, -47.76942479135487929, 3.702618843596635401 ) ) ;
#35214 = CARTESIAN_POINT ( 'NONE',  ( 0.5806925824938502512, -14.41498975133575300, -44.62544602368080859 ) ) ;
#35215 = FACE_OUTER_BOUND ( 'NONE', #27667, .T. ) ;
#35216 = CARTESIAN_POINT ( 'NONE',  ( -2.739355103387247858, 14.70078895384972384, -2.595066682262118896 ) ) ;
#35217 = CARTESIAN_POINT ( 'NONE',  ( 2.624215991343620935, 44.87417713512088824, 17.05978231157419955 ) ) ;
#35218 = CARTESIAN_POINT ( 'NONE',  ( 0.6026777506516367566, 48.99513320406567374, -3.320137490087010423 ) ) ;
#35220 = VERTEX_POINT ( 'NONE', #43199 ) ;
#35219 = CARTESIAN_POINT ( 'NONE',  ( 4.303969348037258058, 39.44373910178610032, 27.54579249306222977 ) ) ;
#35221 = VERTEX_POINT ( 'NONE', #13445 ) ;
#35222 = CARTESIAN_POINT ( 'NONE',  ( 0.8560838555295223751, -24.46533024579953164, 40.02274915651970133 ) ) ;
#35223 = CARTESIAN_POINT ( 'NONE',  ( 0.7948878604505663636, 49.04591925934078489, 2.279572614469686620 ) ) ;
#35224 = CARTESIAN_POINT ( 'NONE',  ( 4.958415959904820092, -26.53498967168899725, -36.86595010230982439 ) ) ;
#35225 = ORIENTED_EDGE ( 'NONE', *, *, #53172, .T. ) ;
#35226 = VERTEX_POINT ( 'NONE', #47575 ) ;
#35227 = CARTESIAN_POINT ( 'NONE',  ( 2.526552050251863246, 40.15571433620807795, -15.32056541070799405 ) ) ;
#35228 = CARTESIAN_POINT ( 'NONE',  ( 0.8557997880470599172, 24.73961900479308440, -41.02602466100753276 ) ) ;
#35229 = CARTESIAN_POINT ( 'NONE',  ( 0.6030672727741701600, 6.192762795893809624, 47.70721108823350676 ) ) ;
#35230 = B_SPLINE_CURVE_WITH_KNOTS ( 'NONE', 3,
 ( #19526, #13916, #75, #28292, #47410, #42721 ),
 .UNSPECIFIED., .F., .F.,
 ( 4, 2, 4 ),
 ( 5.421010862427522170E-19, 0.0002293801035737092907, 0.0004587602071474180393 ),
 .UNSPECIFIED. ) ;
#35231 = EDGE_CURVE ( 'NONE', #47413, #18906, #9039, .T. ) ;
#35232 =( BOUNDED_SURFACE ( )  B_SPLINE_SURFACE ( 3, 1, ( 
 ( #35516, #6640 ),
 ( #16091, #7272 ),
 ( #54895, #35207 ),
 ( #45236, #31104 ) ),
 .UNSPECIFIED., .F., .F., .F. ) 
 B_SPLINE_SURFACE_WITH_KNOTS ( ( 4, 4 ),
 ( 2, 2 ),
 ( 0.000000000000000000, 1.000000000000000000 ),
 ( 0.000000000000000000, 1.000000000000000000 ),
 .UNSPECIFIED. ) 
 GEOMETRIC_REPRESENTATION_ITEM ( )  RATIONAL_B_SPLINE_SURFACE ( (
 ( 1.000000000000000000, 1.000000000000000000),
 ( 0.7223157951917476005, 0.9931996967497186413),
 ( 0.7223157951917476005, 0.9931996967497186413),
 ( 1.000000000000000000, 1.000000000000000000) ) ) 
 REPRESENTATION_ITEM ( '' )  SURFACE ( )  );
#35233 = EDGE_LOOP ( 'NONE', ( #49734, #2374, #46125, #26456 ) ) ;
#35234 = VERTEX_POINT ( 'NONE', #9655 ) ;
#35235 = CARTESIAN_POINT ( 'NONE',  ( -6.017396004339686577, -18.20079405513553183, 4.878103249821005072 ) ) ;
#35236 = EDGE_CURVE ( 'NONE', #43286, #54532, #28766, .T. ) ;
#35237 = CARTESIAN_POINT ( 'NONE',  ( 0.8557997880470697982, -47.60865952216995822, -5.347802024197736870 ) ) ;
#35238 = CARTESIAN_POINT ( 'NONE',  ( 0.7048096507298635682, -7.115188260603519055, -47.58126109679101035 ) ) ;
#35239 = CARTESIAN_POINT ( 'NONE',  ( 3.783278058412225864, 42.41041238787303769, -7.325100730113862646 ) ) ;
#35240 = ADVANCED_FACE ( 'NONE', ( #4942 ), #5906, .F. ) ;
#35241 = VERTEX_POINT ( 'NONE', #4010 ) ;
#35242 = CARTESIAN_POINT ( 'NONE',  ( 0.8557997880470697982, 13.27832040216639520, 46.03118133706031045 ) ) ;
#35243 = CIRCLE ( 'NONE', #58226, 48.09070567114147110 ) ;
#35244 = DIRECTION ( 'NONE',  ( -1.000000000000000000, -3.673819061467147552E-16, 1.925929944387235306E-32 ) ) ;
#35245 =( BOUNDED_SURFACE ( )  B_SPLINE_SURFACE ( 3, 1, ( 
 ( #34052, #39066 ),
 ( #53424, #30239 ),
 ( #49352, #1720 ),
 ( #20857, #54336 ) ),
 .UNSPECIFIED., .F., .F., .F. ) 
 B_SPLINE_SURFACE_WITH_KNOTS ( ( 4, 4 ),
 ( 2, 2 ),
 ( 0.000000000000000000, 1.000000000000000000 ),
 ( 0.000000000000000000, 1.000000000000000000 ),
 .UNSPECIFIED. ) 
 GEOMETRIC_REPRESENTATION_ITEM ( )  RATIONAL_B_SPLINE_SURFACE ( (
 ( 1.000000000000000000, 1.000000000000000000),
 ( 0.7223157951917480446, 0.9931996967497186413),
 ( 0.7223157951917480446, 0.9931996967497186413),
 ( 1.000000000000000000, 1.000000000000000000) ) ) 
 REPRESENTATION_ITEM ( '' )  SURFACE ( )  );
#35246 = VECTOR ( 'NONE', #21501, 1000.000000000000227 ) ;
#35247 = CARTESIAN_POINT ( 'NONE',  ( -6.015611763856276717, -7.205255340944737519, 17.41126425312535275 ) ) ;
#35248 = VERTEX_POINT ( 'NONE', #56646 ) ;
#35249 = ORIENTED_EDGE ( 'NONE', *, *, #53113, .T. ) ;
#35250 = CARTESIAN_POINT ( 'NONE',  ( 0.2940135542859002027, 34.10816074289976285, 27.97988419253970349 ) ) ;
#35251 = CARTESIAN_POINT ( 'NONE',  ( 0.8557997880470690211, 19.17299735372009550, 43.90420959842187187 ) ) ;
#35252 = B_SPLINE_CURVE_WITH_KNOTS ( 'NONE', 3,
 ( #56493, #45902, #39271, #61795 ),
 .UNSPECIFIED., .F., .F.,
 ( 4, 4 ),
 ( 0.000000000000000000, 0.004444103432399267029 ),
 .UNSPECIFIED. ) ;
#35253 = ORIENTED_EDGE ( 'NONE', *, *, #24899, .F. ) ;
#35254 = CARTESIAN_POINT ( 'NONE',  ( 0.5819845901640493535, 44.42187107932970491, -17.90867915372005115 ) ) ;
#35255 = CARTESIAN_POINT ( 'NONE',  ( 5.974727161628369032, 14.52429704002363486, -14.50236057684829838 ) ) ;
#35256 = CARTESIAN_POINT ( 'NONE',  ( 0.6845945791218034371, -20.52768236698797111, 42.17843972166340905 ) ) ;
#35257 = CARTESIAN_POINT ( 'NONE',  ( 0.5827359174754813687, 12.74690115177672567, -46.16863801597752115 ) ) ;
#35258 = ORIENTED_EDGE ( 'NONE', *, *, #9615, .T. ) ;
#35259 = CARTESIAN_POINT ( 'NONE',  ( 0.8751705887134423323, 11.58504748649134974, 46.67919521768892110 ) ) ;
#35260 = CARTESIAN_POINT ( 'NONE',  ( 4.956445790444041322, 46.25174887658561573, -8.849507104743011610 ) ) ;
#35261 = DIRECTION ( 'NONE',  ( 1.000000000000000000, 0.000000000000000000, 0.000000000000000000 ) ) ;
#35262 = ORIENTED_EDGE ( 'NONE', *, *, #47533, .T. ) ;
#35263 = CARTESIAN_POINT ( 'NONE',  ( 0.8557997880470606944, -46.50333260518566902, 11.51622788066442027 ) ) ;
#35264 = CARTESIAN_POINT ( 'NONE',  ( 0.5809828226811617480, 28.72298383114487663, 38.32755012159156394 ) ) ;
#35265 = ORIENTED_EDGE ( 'NONE', *, *, #3741, .T. ) ;
#35266 = CARTESIAN_POINT ( 'NONE',  ( 0.6254087463353908971, 42.00124903776036689, 23.45485308995613849 ) ) ;
#35267 = CARTESIAN_POINT ( 'NONE',  ( 5.917102823773431552, -19.93133248418637749, 2.689182674449420052 ) ) ;
#35268 = VERTEX_POINT ( 'NONE', #13768 ) ;
#35269 = CARTESIAN_POINT ( 'NONE',  ( 0.5804410086790514622, -2.113107284888617432, -46.85141011173460157 ) ) ;
#35270 = CARTESIAN_POINT ( 'NONE',  ( 4.960156602257184133, -41.85906677498947204, -20.07163247083191493 ) ) ;
#35271 = DIRECTION ( 'NONE',  ( 0.000000000000000000, 0.000000000000000000, 1.000000000000000000 ) ) ;
#35272 = CARTESIAN_POINT ( 'NONE',  ( 4.694002226626921015, -30.90320716795002198, 33.51531826166802119 ) ) ;
#35273 = CARTESIAN_POINT ( 'NONE',  ( 3.559346040607745287, 22.13704001167854329, 37.99186414304161019 ) ) ;
#35274 = CARTESIAN_POINT ( 'NONE',  ( 0.5836750258453352602, 46.31062999473601138, -12.22088356912678186 ) ) ;
#35275 = EDGE_CURVE ( 'NONE', #31849, #59478, #32872, .T. ) ;
#35276 = FACE_BOUND ( 'NONE', #50962, .T. ) ;
#35277 = CARTESIAN_POINT ( 'NONE',  ( 0.1103310638050661874, -41.63362651001257575, -11.24099191366984662 ) ) ;
#35278 = B_SPLINE_CURVE_WITH_KNOTS ( 'NONE', 3,
 ( #49586, #6642, #39608, #38995, #58051, #44012 ),
 .UNSPECIFIED., .F., .F.,
 ( 4, 2, 4 ),
 ( 1.480053515295545178E-16, 0.0002445252820015214124, 0.0004890505640028948312 ),
 .UNSPECIFIED. ) ;
#35279 = CARTESIAN_POINT ( 'NONE',  ( -6.072942160501519027, 5.465015824218939500, 18.46450011048381867 ) ) ;
#35280 = CARTESIAN_POINT ( 'NONE',  ( 0.9785694773339237429, 41.50447357468266318, 5.806382609089985714 ) ) ;
#35281 = CARTESIAN_POINT ( 'NONE',  ( 0.5987334363312690755, 33.46066802764950410, -35.94365871214991870 ) ) ;
#35282 = ORIENTED_EDGE ( 'NONE', *, *, #27078, .T. ) ;
#35283 = CARTESIAN_POINT ( 'NONE',  ( 0.3676999524040323597, 10.61898383218351860, -42.81574203134477585 ) ) ;
#35284 = CARTESIAN_POINT ( 'NONE',  ( 1.154321713695927620, -17.18284946700656945, 39.32643513900325871 ) ) ;
#35285 = CARTESIAN_POINT ( 'NONE',  ( 4.549368137175248350, 2.596185425821941894, -42.84816078363927971 ) ) ;
#35286 = CARTESIAN_POINT ( 'NONE',  ( -6.077587904424778920, -1.842868750311569270, -19.16767738050324610 ) ) ;
#35287 = AXIS2_PLACEMENT_3D ( 'NONE', #47616, #42936, #35076 ) ;
#35288 = CARTESIAN_POINT ( 'NONE',  ( 0.8744876279028306332, -35.88078294188929362, -33.50999053799506555 ) ) ;
#35289 = DIRECTION ( 'NONE',  ( -1.000000000000000000, -3.673819061467163329E-16, -4.553275654311305981E-31 ) ) ;
#35290 = CARTESIAN_POINT ( 'NONE',  ( 0.1129192098497455998, -32.03190746135001632, 30.34647742609778831 ) ) ;
#35291 = CIRCLE ( 'NONE', #57242, 75.00000000000001421 ) ;
#35292 = CARTESIAN_POINT ( 'NONE',  ( 0.9762797500689124330, -7.469026406146330288, 41.23758515880862774 ) ) ;
#35293 = CARTESIAN_POINT ( 'NONE',  ( 5.894904586330512508, 8.465111963867252953, 18.24476065890792142 ) ) ;
#35295 = ORIENTED_EDGE ( 'NONE', *, *, #54980, .T. ) ;
#35294 = CARTESIAN_POINT ( 'NONE',  ( 0.6064515330803548210, -29.73185795686339716, 36.26776748670900474 ) ) ;
#35296 = EDGE_LOOP ( 'NONE', ( #24776, #6904, #57547, #40841 ) ) ;
#35297 = FACE_BOUND ( 'NONE', #13853, .T. ) ;
#35298 = CARTESIAN_POINT ( 'NONE',  ( 4.303969348037258058, 32.45857549159350697, -35.51084504003163289 ) ) ;
#35299 = CARTESIAN_POINT ( 'NONE',  ( 3.678748215320120085, -26.95178576869570364, -40.89271399867971013 ) ) ;
#35300 = ORIENTED_EDGE ( 'NONE', *, *, #25562, .T. ) ;
#35301 = CARTESIAN_POINT ( 'NONE',  ( 0.1156495703730067715, -22.75696492371722712, 37.80295624275665034 ) ) ;
#35302 = CARTESIAN_POINT ( 'NONE',  ( 0.6846871229502899947, 44.58493949244006416, 17.53234844287758065 ) ) ;
#35303 = CARTESIAN_POINT ( 'NONE',  ( 0.6041374136657476912, 38.05989626241430557, -29.42442150067158835 ) ) ;
#35304 = B_SPLINE_CURVE_WITH_KNOTS ( 'NONE', 3,
 ( #35666, #54729, #30944, #44461, #1488, #29700 ),
 .UNSPECIFIED., .F., .F.,
 ( 4, 2, 4 ),
 ( 1.084202172485504434E-19, 0.0002291966416970792682, 0.0004583932833941584280 ),
 .UNSPECIFIED. ) ;
#35305 = EDGE_CURVE ( 'NONE', #36038, #2801, #2305, .T. ) ;
#35306 = ORIENTED_EDGE ( 'NONE', *, *, #40471, .F. ) ;
#35307 = VERTEX_POINT ( 'NONE', #48194 ) ;
#35308 = AXIS2_PLACEMENT_3D ( 'NONE', #20056, #5594, #43879 ) ;
#35309 = EDGE_CURVE ( 'NONE', #45423, #21910, #54548, .T. ) ;
#35310 = CARTESIAN_POINT ( 'NONE',  ( -6.016104459813371719, 7.215917642689068323, 17.40682403289250857 ) ) ;
#35311 = CARTESIAN_POINT ( 'NONE',  ( 0.1095718737110179114, -39.74279513315663337, -16.74012863188490741 ) ) ;
#35312 = CARTESIAN_POINT ( 'NONE',  ( 4.549368137175248350, 0.000000000000000000, 0.000000000000000000 ) ) ;
#35313 = ORIENTED_EDGE ( 'NONE', *, *, #1861, .F. ) ;
#35314 = EDGE_CURVE ( 'NONE', #10336, #45553, #768, .T. ) ;
#35315 = B_SPLINE_CURVE_WITH_KNOTS ( 'NONE', 3,
 ( #29516, #15128, #39565, #10737 ),
 .UNSPECIFIED., .F., .F.,
 ( 4, 4 ),
 ( 0.000000000000000000, 0.004447772540403782497 ),
 .UNSPECIFIED. ) ;
#35316 = CARTESIAN_POINT ( 'NONE',  ( 0.1087620492084206275, -0.3620418170789792556, 43.12302841504342155 ) ) ;
#35317 = CARTESIAN_POINT ( 'NONE',  ( 0.5804410086790514622, -25.69437916690408130, 39.23415261073905924 ) ) ;
#35318 = ORIENTED_EDGE ( 'NONE', *, *, #47265, .F. ) ;
#35319 = CARTESIAN_POINT ( 'NONE',  ( 4.956445790444005794, -28.36659270909926533, -37.58822246682746737 ) ) ;
#35320 = CARTESIAN_POINT ( 'NONE',  ( 0.8557997880470599172, 41.02602466100778145, 24.73961900479265807 ) ) ;
#35321 = VERTEX_POINT ( 'NONE', #14688 ) ;
#35322 =( BOUNDED_SURFACE ( )  B_SPLINE_SURFACE ( 3, 1, ( 
 ( #7045, #16174 ),
 ( #11791, #59061 ),
 ( #16796, #59994 ),
 ( #40929, #36215 ) ),
 .UNSPECIFIED., .F., .F., .F. ) 
 B_SPLINE_SURFACE_WITH_KNOTS ( ( 4, 4 ),
 ( 2, 2 ),
 ( 0.000000000000000000, 1.000000000000000000 ),
 ( 0.000000000000000000, 1.000000000000000000 ),
 .UNSPECIFIED. ) 
 GEOMETRIC_REPRESENTATION_ITEM ( )  RATIONAL_B_SPLINE_SURFACE ( (
 ( 1.000000000000000000, 1.000000000000000000),
 ( 0.9732289882329797637, 0.9999525324661233672),
 ( 0.9732289882329797637, 0.9999525324661233672),
 ( 1.000000000000000000, 1.000000000000000000) ) ) 
 REPRESENTATION_ITEM ( '' )  SURFACE ( )  );
#35323 = CARTESIAN_POINT ( 'NONE',  ( 0.1310142868023712048, -37.02349354742227661, -22.11113027429274425 ) ) ;
#35324 = ADVANCED_FACE ( 'NONE', ( #14997, #19380 ), #34107, .T. ) ;
#35325 = CARTESIAN_POINT ( 'NONE',  ( 0.7764139734771234869, -46.85094005902467273, 2.242740843821329211 ) ) ;
#35326 = ORIENTED_EDGE ( 'NONE', *, *, #860, .F. ) ;
#35327 = CARTESIAN_POINT ( 'NONE',  ( 4.962356264823608143, 26.83784316460287300, 32.41860225448540689 ) ) ;
#35328 = DIRECTION ( 'NONE',  ( -1.000000000000000000, -0.000000000000000000, -0.000000000000000000 ) ) ;
#35329 = CARTESIAN_POINT ( 'NONE',  ( -5.440000000000000391, 4.832908975360033023E-15, 0.000000000000000000 ) ) ;
#35330 = CARTESIAN_POINT ( 'NONE',  ( -6.010958268070873523, 7.197664668556443601, 17.41463273278780832 ) ) ;
#35331 = EDGE_CURVE ( 'NONE', #35962, #9258, #9151, .T. ) ;
#35332 = B_SPLINE_CURVE_WITH_KNOTS ( 'NONE', 3,
 ( #16401, #40542, #26104, #22335 ),
 .UNSPECIFIED., .F., .F.,
 ( 4, 4 ),
 ( 0.000000000000000000, 0.005014147105413701254 ),
 .UNSPECIFIED. ) ;
#35333 = AXIS2_PLACEMENT_3D ( 'NONE', #54443, #30652, #49769 ) ;
#35334 = ORIENTED_EDGE ( 'NONE', *, *, #55865, .T. ) ;
#35335 = CARTESIAN_POINT ( 'NONE',  ( -6.016761891674565099, -17.41015286184807209, 7.207804629151251419 ) ) ;
#35336 = CARTESIAN_POINT ( 'NONE',  ( 0.1152809850208375564, 39.85000777899687563, -18.94524115717834434 ) ) ;
#35337 = EDGE_LOOP ( 'NONE', ( #21943, #12698, #8424, #52371 ) ) ;
#35338 = DIRECTION ( 'NONE',  ( 0.000000000000000000, 0.000000000000000000, 1.000000000000000000 ) ) ;
#35339 = VERTEX_POINT ( 'NONE', #39739 ) ;
#35340 = CARTESIAN_POINT ( 'NONE',  ( 0.9769922540276043676, 3.754999534460876198, 41.74004712003000606 ) ) ;
#35341 = VERTEX_POINT ( 'NONE', #44141 ) ;
#35342 = DIRECTION ( 'NONE',  ( 0.09722883295013598492, 0.8933953294778579357, 0.4386243715416464628 ) ) ;
#35343 = CARTESIAN_POINT ( 'NONE',  ( 0.6026777506516367566, -30.75401662176760453, -38.28494289228157044 ) ) ;
#35344 =( BOUNDED_SURFACE ( )  B_SPLINE_SURFACE ( 3, 1, ( 
 ( #45700, #3062 ),
 ( #8373, #50984 ),
 ( #36610, #30965 ),
 ( #55063, #22191 ) ),
 .UNSPECIFIED., .F., .F., .F. ) 
 B_SPLINE_SURFACE_WITH_KNOTS ( ( 4, 4 ),
 ( 2, 2 ),
 ( 0.000000000000000000, 1.000000000000000000 ),
 ( 0.000000000000000000, 1.000000000000000000 ),
 .UNSPECIFIED. ) 
 GEOMETRIC_REPRESENTATION_ITEM ( )  RATIONAL_B_SPLINE_SURFACE ( (
 ( 1.000000000000000000, 1.000000000000000000),
 ( 0.7211978278499970862, 0.9934217856018976445),
 ( 0.7211978278499970862, 0.9934217856018976445),
 ( 1.000000000000000000, 1.000000000000000000) ) ) 
 REPRESENTATION_ITEM ( '' )  SURFACE ( )  );
#35345 = CARTESIAN_POINT ( 'NONE',  ( -6.077587904424778920, 16.78120357693980935, 9.443898977818069085 ) ) ;
#35346 = VERTEX_POINT ( 'NONE', #48483 ) ;
#35347 = CARTESIAN_POINT ( 'NONE',  ( 4.960156602257182357, -8.553784487773192780, 45.62767441207047625 ) ) ;
#35348 = CARTESIAN_POINT ( 'NONE',  ( 0.5809828226811617480, 11.86925843957166471, 46.40184912890843805 ) ) ;
#35349 =( BOUNDED_SURFACE ( )  B_SPLINE_SURFACE ( 3, 1, ( 
 ( #25011, #29694 ),
 ( #21229, #39436 ),
 ( #10921, #1481 ),
 ( #20315, #25931 ) ),
 .UNSPECIFIED., .F., .F., .F. ) 
 B_SPLINE_SURFACE_WITH_KNOTS ( ( 4, 4 ),
 ( 2, 2 ),
 ( 0.000000000000000000, 1.000000000000000000 ),
 ( 0.000000000000000000, 1.000000000000000000 ),
 .UNSPECIFIED. ) 
 GEOMETRIC_REPRESENTATION_ITEM ( )  RATIONAL_B_SPLINE_SURFACE ( (
 ( 1.000000000000000000, 1.000000000000000000),
 ( 0.9751682680413298332, 0.9999560080971552356),
 ( 0.9751682680413298332, 0.9999560080971552356),
 ( 1.000000000000000000, 1.000000000000000000) ) ) 
 REPRESENTATION_ITEM ( '' )  SURFACE ( )  );
#35350 = DIRECTION ( 'NONE',  ( -0.000000000000000000, -0.000000000000000000, 1.000000000000000000 ) ) ;
#35351 = ORIENTED_EDGE ( 'NONE', *, *, #25870, .T. ) ;
#35352 = AXIS2_PLACEMENT_3D ( 'NONE', #23347, #19580, #20491 ) ;
#35353 = B_SPLINE_CURVE_WITH_KNOTS ( 'NONE', 3,
 ( #13860, #47979, #33273, #24467, #43292, #28538 ),
 .UNSPECIFIED., .F., .F.,
 ( 4, 2, 4 ),
 ( 6.345130535746553974E-19, 0.0002293801035737091281, 0.0004587602071474176598 ),
 .UNSPECIFIED. ) ;
#35354 = B_SPLINE_CURVE_WITH_KNOTS ( 'NONE', 3,
 ( #3735, #8439, #36373, #31968, #50743, #18177 ),
 .UNSPECIFIED., .F., .F.,
 ( 4, 2, 4 ),
 ( 8.558167549966217657E-17, 0.0002293366620881433855, 0.0004586733241762012275 ),
 .UNSPECIFIED. ) ;
#35355 = VERTEX_POINT ( 'NONE', #57550 ) ;
#35356 = CARTESIAN_POINT ( 'NONE',  ( 0.5836750258453348161, 18.16108240858346790, 44.31929073742199421 ) ) ;
#35357 = CARTESIAN_POINT ( 'NONE',  ( 3.727782113643637096, 31.10430010538506806, 31.06928211047236132 ) ) ;
#35358 = CARTESIAN_POINT ( 'NONE',  ( 0.9772918015221174759, 38.41934892684628977, -16.74187814398117879 ) ) ;
#35359 = CARTESIAN_POINT ( 'NONE',  ( 0.1073791018717483448, -6.109314776652422729, -42.68962945260951614 ) ) ;
#35360 = ADVANCED_FACE ( 'NONE', ( #9980 ), #24173, .T. ) ;
#35361 = DIRECTION ( 'NONE',  ( -1.000000000000000000, -1.836909530733573776E-16, 1.925929944387235853E-32 ) ) ;
#35362 = CARTESIAN_POINT ( 'NONE',  ( 5.880360259849739535, 3.184717612777296036, 47.86623372148050493 ) ) ;
#35363 = ORIENTED_EDGE ( 'NONE', *, *, #2673, .F. ) ;
#35364 = CARTESIAN_POINT ( 'NONE',  ( 4.962356264823601926, -38.91448554252674796, -16.02805081171206680 ) ) ;
#35365 = CARTESIAN_POINT ( 'NONE',  ( 3.661933894777873455, -46.43415008926496768, 7.516706089722269724 ) ) ;
#35366 = ORIENTED_EDGE ( 'NONE', *, *, #3651, .T. ) ;
#35367 = CARTESIAN_POINT ( 'NONE',  ( 0.5806925824938499181, 36.46274162637902094, 29.49052111156212774 ) ) ;
#35368 = CARTESIAN_POINT ( 'NONE',  ( 47.86731964337302969, 15.49701252645352945, 0.3483731184818048554 ) ) ;
#35369 = CARTESIAN_POINT ( 'NONE',  ( 0.5832655196449145762, 45.16907574789987478, 12.60911491952589358 ) ) ;
#35370 = CARTESIAN_POINT ( 'NONE',  ( 5.959547316686252039, -18.96456592444106448, 7.851524054666073837 ) ) ;
#35371 = CARTESIAN_POINT ( 'NONE',  ( 0.6001305935487422083, -41.92422178329185556, 23.60027211631757638 ) ) ;
#35372 = FILL_AREA_STYLE_COLOUR ( '', #42877 ) ;
#35373 = CARTESIAN_POINT ( 'NONE',  ( 0.5804410086790514622, 40.62771722849963396, 23.42879520283684514 ) ) ;
#35374 = CARTESIAN_POINT ( 'NONE',  ( 0.6024113833632039894, 37.53342516667872530, -31.66676277042214949 ) ) ;
#35375 = CARTESIAN_POINT ( 'NONE',  ( -6.016761891674565099, 18.20201388312102253, -4.873659902332176053 ) ) ;
#35376 = CARTESIAN_POINT ( 'NONE',  ( 0.1155031312995260795, 29.53975840367626660, 32.77719185629308640 ) ) ;
#35377 = CARTESIAN_POINT ( 'NONE',  ( -4.473699999999999122, 0.000000000000000000, 0.000000000000000000 ) ) ;
#35378 = CARTESIAN_POINT ( 'NONE',  ( 3.782542959838389951, -28.43539247177547935, 30.96233693332376191 ) ) ;
#35379 = CARTESIAN_POINT ( 'NONE',  ( 1.657374760986086271, -21.77053621054746202, 38.30057702381891005 ) ) ;
#35380 =( GEOMETRIC_REPRESENTATION_CONTEXT ( 3 ) GLOBAL_UNCERTAINTY_ASSIGNED_CONTEXT ( ( #43020 ) ) GLOBAL_UNIT_ASSIGNED_CONTEXT ( ( #52425, #28943, #11010 ) ) REPRESENTATION_CONTEXT ( 'NONE', 'WORKASPACE' ) );
#35381 = CARTESIAN_POINT ( 'NONE',  ( 0.5980894510889448457, 47.78766676462075935, -5.583794302584760061 ) ) ;
#35382 = CARTESIAN_POINT ( 'NONE',  ( 0.5807400328401637335, -24.41979442053199634, 41.20655774452961850 ) ) ;
#35383 = ORIENTED_EDGE ( 'NONE', *, *, #24907, .F. ) ;
#35384 = EDGE_CURVE ( 'NONE', #36659, #30629, #24687, .T. ) ;
#35385 = DIRECTION ( 'NONE',  ( 0.000000000000000000, 1.000000000000000000, 0.000000000000000000 ) ) ;
#35386 = CARTESIAN_POINT ( 'NONE',  ( 0.5834584762367742705, -19.57482590732785255, -42.61528105868828220 ) ) ;
#35387 = CARTESIAN_POINT ( 'NONE',  ( 0.9747592971366227932, -39.76507150545822356, -16.12077520819492804 ) ) ;
#35388 = CARTESIAN_POINT ( 'NONE',  ( 0.5804410086790514622, 32.20888702807411619, -34.08969709850992302 ) ) ;
#35389 = CARTESIAN_POINT ( 'NONE',  ( 0.1103310638050661735, -41.67627416617921199, 11.08182869403221815 ) ) ;
#35390 = VERTEX_POINT ( 'NONE', #58178 ) ;
#35391 = EDGE_CURVE ( 'NONE', #7563, #28286, #10592, .T. ) ;
#35392 = CARTESIAN_POINT ( 'NONE',  ( 4.967162193818130511, 0.000000000000000000, 0.000000000000000000 ) ) ;
#35393 = PRESENTATION_LAYER_ASSIGNMENT (  '', '', ( #58375 ) ) ;
#35394 = B_SPLINE_CURVE_WITH_KNOTS ( 'NONE', 3,
 ( #37141, #37447, #46848, #50582, #21789, #50895 ),
 .UNSPECIFIED., .F., .F.,
 ( 4, 2, 4 ),
 ( 2.224043620450102089E-17, 0.0002293755540694315353, 0.0004587511081388407903 ),
 .UNSPECIFIED. ) ;
#35395 = CARTESIAN_POINT ( 'NONE',  ( 4.956445790443998689, -16.41925925744477510, 44.13554095710679093 ) ) ;
#35396 = ORIENTED_EDGE ( 'NONE', *, *, #44180, .F. ) ;
#35397 = CARTESIAN_POINT ( 'NONE',  ( 4.975610109902397937, 25.84633036597884725, -41.52609557555889808 ) ) ;
#35398 = CARTESIAN_POINT ( 'NONE',  ( 4.834790513006553603, -42.36901421273557133, -20.91544825160086418 ) ) ;
#35399 = VERTEX_POINT ( 'NONE', #34408 ) ;
#35400 = B_SPLINE_CURVE_WITH_KNOTS ( 'NONE', 3,
 ( #7404, #40667, #1475, #11521, #49724, #54092 ),
 .UNSPECIFIED., .F., .F.,
 ( 4, 2, 4 ),
 ( 3.471140604459641645E-18, 0.0002291966416970819787, 0.0004583932833941604880 ),
 .UNSPECIFIED. ) ;
#35401 = CARTESIAN_POINT ( 'NONE',  ( 4.553261556744875094, 35.33793455049291765, -26.09156851415253087 ) ) ;
#35402 = ORIENTED_EDGE ( 'NONE', *, *, #33919, .T. ) ;
#35403 = CARTESIAN_POINT ( 'NONE',  ( 5.965394784446458765, 12.48356622107676728, -16.29267539192330361 ) ) ;
#35404 = VERTEX_POINT ( 'NONE', #29684 ) ;
#35405 = FACE_OUTER_BOUND ( 'NONE', #38044, .T. ) ;
#35406 = CARTESIAN_POINT ( 'NONE',  ( 0.1156495703730067437, 20.52988295744289360, 39.05722543889626763 ) ) ;
#35407 = EDGE_LOOP ( 'NONE', ( #3318, #48622, #12018, #6182 ) ) ;
#35408 = EDGE_CURVE ( 'NONE', #8175, #31646, #26191, .T. ) ;
#35409 = ORIENTED_EDGE ( 'NONE', *, *, #17821, .F. ) ;
#35410 = CARTESIAN_POINT ( 'NONE',  ( 0.8554163680231708922, -38.15570339590799165, -27.30105806512478850 ) ) ;
#35411 = CARTESIAN_POINT ( 'NONE',  ( 0.8554163680231720024, -38.15570339590837534, 27.30105806512423428 ) ) ;
#35412 = ORIENTED_EDGE ( 'NONE', *, *, #39784, .T. ) ;
#35413 = VERTEX_POINT ( 'NONE', #10909 ) ;
#35414 = DIRECTION ( 'NONE',  ( -1.000000000000000000, -0.000000000000000000, -0.000000000000000000 ) ) ;
#35415 = CARTESIAN_POINT ( 'NONE',  ( 0.5804410086790514622, -38.97211966759144985, -26.09010809617945270 ) ) ;
#35416 = DIRECTION ( 'NONE',  ( 1.000000000000000000, 0.000000000000000000, 0.000000000000000000 ) ) ;
#35417 = CARTESIAN_POINT ( 'NONE',  ( 0.5835871038041848813, 32.69977443625123925, -33.61486582926951883 ) ) ;
#35418 = CARTESIAN_POINT ( 'NONE',  ( 0.6846871229502932144, 17.53234844287741723, 44.58493949244010679 ) ) ;
#35419 = ORIENTED_EDGE ( 'NONE', *, *, #17167, .T. ) ;
#35420 = CARTESIAN_POINT ( 'NONE',  ( 0.5807400328401637335, 12.92266817606015294, 46.12278621143501312 ) ) ;
#35421 = CARTESIAN_POINT ( 'NONE',  ( -6.072942160501519915, 15.44092479507863835, 11.50573786255126763 ) ) ;
#35422 = EDGE_LOOP ( 'NONE', ( #9406, #1136, #30188, #47098 ) ) ;
#35423 = VECTOR ( 'NONE', #17326, 1000.000000000000114 ) ;
#35424 = CARTESIAN_POINT ( 'NONE',  ( 0.3676999524040323597, -38.83470403830501994, 20.92406140260764857 ) ) ;
#35425 =( BOUNDED_SURFACE ( )  B_SPLINE_SURFACE ( 3, 1, ( 
 ( #11315, #29483 ),
 ( #48593, #39854 ),
 ( #25718, #34511 ),
 ( #49211, #44856 ) ),
 .UNSPECIFIED., .F., .F., .F. ) 
 B_SPLINE_SURFACE_WITH_KNOTS ( ( 4, 4 ),
 ( 2, 2 ),
 ( 0.000000000000000000, 1.000000000000000000 ),
 ( 0.000000000000000000, 1.000000000000000000 ),
 .UNSPECIFIED. ) 
 GEOMETRIC_REPRESENTATION_ITEM ( )  RATIONAL_B_SPLINE_SURFACE ( (
 ( 1.000000000000000000, 1.000000000000000000),
 ( 0.9953485035131437453, 0.8621029689291515030),
 ( 0.9953485035131437453, 0.8621029689291515030),
 ( 1.000000000000000000, 1.000000000000000000) ) ) 
 REPRESENTATION_ITEM ( '' )  SURFACE ( )  );
#35426 = ORIENTED_EDGE ( 'NONE', *, *, #28979, .F. ) ;
#35427 = B_SPLINE_CURVE_WITH_KNOTS ( 'NONE', 3,
 ( #61472, #61176, #9801, #18597 ),
 .UNSPECIFIED., .F., .F.,
 ( 4, 4 ),
 ( 2.168404344971008868E-19, 0.004444878191957678248 ),
 .UNSPECIFIED. ) ;
#35428 = CARTESIAN_POINT ( 'NONE',  ( 3.678748215320120085, 38.46437741425435064, 30.31673604518275411 ) ) ;
#35429 = DIRECTION ( 'NONE',  ( 0.000000000000000000, 0.000000000000000000, 1.000000000000000000 ) ) ;
#35430 = CARTESIAN_POINT ( 'NONE',  ( 5.974727161628367256, 17.76736931401860531, -10.27590650342018996 ) ) ;
#35431 = VERTEX_POINT ( 'NONE', #35031 ) ;
#35432 = CARTESIAN_POINT ( 'NONE',  ( 3.680882792899937250, 4.423598386734397536, -47.77138407787918339 ) ) ;
#35433 = CARTESIAN_POINT ( 'NONE',  ( -6.078457390727109555, -14.66526260008077287, 12.47896565858644990 ) ) ;
#35434 = DIRECTION ( 'NONE',  ( 0.000000000000000000, 0.5000000000000009992, 0.8660254037844380415 ) ) ;
#35435 = CARTESIAN_POINT ( 'NONE',  ( 0.5998501479064708430, -28.86886762351098312, -38.48283596222019298 ) ) ;
#35436 = ORIENTED_EDGE ( 'NONE', *, *, #51896, .F. ) ;
#35437 = CARTESIAN_POINT ( 'NONE',  ( 4.834790513006555379, -44.69577334950041347, 15.32570342967882127 ) ) ;
#35438 = EDGE_LOOP ( 'NONE', ( #20024, #35625, #15515, #14009 ) ) ;
#35439 = EDGE_CURVE ( 'NONE', #12663, #39207, #38191, .T. ) ;
#35440 = CARTESIAN_POINT ( 'NONE',  ( 4.960156602257181468, 9.558288641082377524, -45.42786611289300680 ) ) ;
#35441 = CARTESIAN_POINT ( 'NONE',  ( 4.553261556744875094, -43.15908619232990873, 8.175135770534621926 ) ) ;
#35442 = VECTOR ( 'NONE', #40064, 1000.000000000000000 ) ;
#35443 = EDGE_CURVE ( 'NONE', #15172, #54983, #34403, .T. ) ;
#35444 = CARTESIAN_POINT ( 'NONE',  ( 4.958415959904820980, 28.93810772186849078, 35.01128211448664018 ) ) ;
#35445 = DIRECTION ( 'NONE',  ( 0.000000000000000000, 0.000000000000000000, 1.000000000000000000 ) ) ;
#35446 = EDGE_CURVE ( 'NONE', #15365, #11373, #12783, .T. ) ;
#35447 = CARTESIAN_POINT ( 'NONE',  ( 4.956653778116975495, 8.845409907520915382, 47.27023054223757015 ) ) ;
#35448 = FACE_OUTER_BOUND ( 'NONE', #56079, .T. ) ;
#35449 = CARTESIAN_POINT ( 'NONE',  ( 3.661933894777875231, -23.70323884901255695, -40.62988595871659214 ) ) ;
#35450 = CARTESIAN_POINT ( 'NONE',  ( 5.959547316686252039, 18.96183906913543282, -7.858107265727552360 ) ) ;
#35451 = CARTESIAN_POINT ( 'NONE',  ( 2.624215991343620935, 42.26352390376096935, 22.77108897942150634 ) ) ;
#35452 = CARTESIAN_POINT ( 'NONE',  ( 3.660176727303397382, 36.93665184075219798, 30.71420464230583036 ) ) ;
#35453 = EDGE_CURVE ( 'NONE', #44029, #20909, #20607, .T. ) ;
#35454 = DIRECTION ( 'NONE',  ( 1.000000000000000000, 0.000000000000000000, 0.000000000000000000 ) ) ;
#35455 = CARTESIAN_POINT ( 'NONE',  ( 2.299652685299201416, 15.71955970131786984, 46.44542138526527708 ) ) ;
#35456 = ORIENTED_EDGE ( 'NONE', *, *, #60517, .T. ) ;
#35457 = CARTESIAN_POINT ( 'NONE',  ( 4.960156602257180580, -8.553784487772583489, -45.62767441207059704 ) ) ;
#35458 = CARTESIAN_POINT ( 'NONE',  ( 2.299652685299202748, 48.99838078751366766, -1.854832892733276672 ) ) ;
#35459 = CARTESIAN_POINT ( 'NONE',  ( 0.3676999524040366896, -42.45338881270437525, 11.98584004733023534 ) ) ;
#35460 = ORIENTED_EDGE ( 'NONE', *, *, #56995, .F. ) ;
#35461 = EDGE_CURVE ( 'NONE', #12356, #2992, #10190, .T. ) ;
#35462 = CYLINDRICAL_SURFACE ( 'NONE', #52306, 2.649999999999992806 ) ;
#35463 = FACE_OUTER_BOUND ( 'NONE', #45491, .T. ) ;
#35464 = VECTOR ( 'NONE', #40621, 1000.000000000000114 ) ;
#35465 = B_SPLINE_CURVE_WITH_KNOTS ( 'NONE', 3,
 ( #6165, #4946, #9984, #20611 ),
 .UNSPECIFIED., .F., .F.,
 ( 4, 4 ),
 ( 2.602085213965210642E-18, 0.004566006591234643766 ),
 .UNSPECIFIED. ) ;
#35466 = EDGE_CURVE ( 'NONE', #59804, #6825, #25922, .T. ) ;
#35467 = CARTESIAN_POINT ( 'NONE',  ( 0.5998501479064699549, -12.95623334615470057, -46.33007877220734372 ) ) ;
#35468 = ORIENTED_EDGE ( 'NONE', *, *, #7334, .T. ) ;
#35469 = CARTESIAN_POINT ( 'NONE',  ( 7.999999999999983125, 80.00000000000001421, 2.649999999999992806 ) ) ;
#35470 = FACE_OUTER_BOUND ( 'NONE', #49725, .T. ) ;
#35471 = AXIS2_PLACEMENT_3D ( 'NONE', #21996, #13215, #2557 ) ;
#35472 = EDGE_LOOP ( 'NONE', ( #5083, #51763, #7770, #20292 ) ) ;
#35473 = CARTESIAN_POINT ( 'NONE',  ( 0.6016117650947688800, 11.26679697061805641, 47.79759764117200405 ) ) ;
#35474 = EDGE_LOOP ( 'NONE', ( #5245, #37262, #47812, #44298 ) ) ;
#35475 = EDGE_LOOP ( 'NONE', ( #644, #17128, #30279, #37030 ) ) ;
#35476 = CARTESIAN_POINT ( 'NONE',  ( 0.8753041380234524160, -20.68664920503281834, -44.53314352862253145 ) ) ;
#35477 = VERTEX_POINT ( 'NONE', #59105 ) ;
#35478 = DIRECTION ( 'NONE',  ( 0.07906939808003034253, 0.9940710100007911221, 0.07463817631258570784 ) ) ;
#35479 = ADVANCED_FACE ( 'NONE', ( #59730 ), #2264, .F. ) ;
#35480 = AXIS2_PLACEMENT_3D ( 'NONE', #48661, #23213, #9723 ) ;
#35481 = CARTESIAN_POINT ( 'NONE',  ( 0.6041374136657475802, -41.57494627055128689, -24.20487816031505801 ) ) ;
#35482 = ORIENTED_EDGE ( 'NONE', *, *, #4837, .F. ) ;
#35483 = CARTESIAN_POINT ( 'NONE',  ( 0.1101816497532063233, 0.1358190954549551299, 43.12424935764384060 ) ) ;
#35484 = CARTESIAN_POINT ( 'NONE',  ( 4.549368137175248350, 40.71620287708344677, -13.59764261105707739 ) ) ;
#35485 = ORIENTED_EDGE ( 'NONE', *, *, #5352, .F. ) ;
#35486 = CARTESIAN_POINT ( 'NONE',  ( 0.1139756605157204172, 43.23286577299607814, -8.824655049866100498 ) ) ;
#35487 = CARTESIAN_POINT ( 'NONE',  ( 0.1073791018717483448, 0.4849339620927342054, 43.12183934961191767 ) ) ;
#35488 = CARTESIAN_POINT ( 'NONE',  ( 0.5807400328401574052, 34.25275203086281550, -33.48217046439075517 ) ) ;
#35489 = CARTESIAN_POINT ( 'NONE',  ( 0.7954190325252790128, 13.28627193046304278, 46.22745637125046159 ) ) ;
#35490 = EDGE_LOOP ( 'NONE', ( #30304, #30746, #22681, #58539 ) ) ;
#35491 = ORIENTED_EDGE ( 'NONE', *, *, #5318, .F. ) ;
#35492 = CARTESIAN_POINT ( 'NONE',  ( 0.1073791018717483448, 41.77800844988500018, 10.69234304550068337 ) ) ;
#35493 = ADVANCED_BREP_SHAPE_REPRESENTATION ( '', ( #30720, #14677 ), #38903 ) ;
#35494 = CARTESIAN_POINT ( 'NONE',  ( 0.8557997880470599172, 24.73961900479308440, -41.02602466100753276 ) ) ;
#35495 = VECTOR ( 'NONE', #40544, 1000.000000000000000 ) ;
#35496 = CARTESIAN_POINT ( 'NONE',  ( 4.975610109902397937, -27.50982196586606321, 40.44328253918227034 ) ) ;
#35497 = ORIENTED_EDGE ( 'NONE', *, *, #3250, .F. ) ;
#35498 = CARTESIAN_POINT ( 'NONE',  ( 2.706805983486680223, -42.95931102688237502, -9.553727514187235315 ) ) ;
#35499 = CARTESIAN_POINT ( 'NONE',  ( 2.526552050251860582, -37.81244156771004583, 20.43086833796944290 ) ) ;
#35500 = CARTESIAN_POINT ( 'NONE',  ( 0.5987334363312688534, 46.41165631110268919, 16.04746288147003952 ) ) ;
#35501 = CARTESIAN_POINT ( 'NONE',  ( 2.281448460670564504, 42.18752512472242699, 22.83953674062028227 ) ) ;
#35502 = EDGE_CURVE ( 'NONE', #23847, #24034, #26175, .T. ) ;
#35503 = ORIENTED_EDGE ( 'NONE', *, *, #23880, .T. ) ;
#35504 = EDGE_LOOP ( 'NONE', ( #20304, #39940, #4617, #49538 ) ) ;
#35505 = CARTESIAN_POINT ( 'NONE',  ( 5.965394784446460541, -19.82223131420050422, -5.326334832595580160 ) ) ;
#35506 = CARTESIAN_POINT ( 'NONE',  ( 0.5988103564986355654, 28.80261217992921985, -38.53259703935803060 ) ) ;
#35507 = ADVANCED_FACE ( 'NONE', ( #16217 ), #3914, .F. ) ;
#35508 = CARTESIAN_POINT ( 'NONE',  ( 0.1103744047535531458, -39.85659247569272168, 16.46720136312911364 ) ) ;
#35509 = CARTESIAN_POINT ( 'NONE',  ( 4.956653778116991482, -31.29546495791826644, -36.51451553856450971 ) ) ;
#35510 = EDGE_CURVE ( 'NONE', #33332, #57526, #20208, .T. ) ;
#35511 = CARTESIAN_POINT ( 'NONE',  ( 1.657374760986086493, -41.28420722619999594, -15.37870868949730685 ) ) ;
#35512 = FACE_OUTER_BOUND ( 'NONE', #32887, .T. ) ;
#35513 = VECTOR ( 'NONE', #42520, 999.9999999999998863 ) ;
#35514 = LINE ( 'NONE', #30467, #16232 ) ;
#35515 = ADVANCED_FACE ( 'NONE', ( #7402 ), #45232, .T. ) ;
#35516 = CARTESIAN_POINT ( 'NONE',  ( -5.995132425357893702, -18.19985213254568635, -4.885449473615521399 ) ) ;
#35517 = CARTESIAN_POINT ( 'NONE',  ( 0.5850706913938534814, 33.99603398296591195, 33.73916126769462664 ) ) ;
#35518 = CIRCLE ( 'NONE', #26504, 43.08621763946400307 ) ;
#35519 = CARTESIAN_POINT ( 'NONE',  ( 0.5997462898726536595, 44.01516392039482639, 21.77652348757905898 ) ) ;
#35520 = CARTESIAN_POINT ( 'NONE',  ( 5.896278296736517710, -13.97836643676194157, -14.46140558085523509 ) ) ;
#35521 = CARTESIAN_POINT ( 'NONE',  ( 0.2230388203127593172, -11.89247826311245682, -41.44703429209680223 ) ) ;
#35522 = AXIS2_PLACEMENT_3D ( 'NONE', #32409, #55565, #8265 ) ;
#35523 = CARTESIAN_POINT ( 'NONE',  ( 0.8557997880470697982, -37.44587306708118035, 29.88293891557457371 ) ) ;
#35524 = CARTESIAN_POINT ( 'NONE',  ( 0.5832655196449125778, -13.67655705356959395, -44.85740708215072914 ) ) ;
#35525 = CARTESIAN_POINT ( 'NONE',  ( 4.975610109902397937, 0.000000000000000000, 0.000000000000000000 ) ) ;
#35526 = CARTESIAN_POINT ( 'NONE',  ( 5.901764892641307547, 45.37424261077610055, 18.41655708698313632 ) ) ;
#35527 = DIRECTION ( 'NONE',  ( 0.000000000000000000, 0.000000000000000000, 1.000000000000000000 ) ) ;
#35528 = EDGE_CURVE ( 'NONE', #55047, #57783, #19539, .T. ) ;
#35529 = CARTESIAN_POINT ( 'NONE',  ( 4.975801465491695552, 45.55012473237732706, 14.85979367497190040 ) ) ;
#35531 = ORIENTED_EDGE ( 'NONE', *, *, #4331, .T. ) ;
#35530 = CARTESIAN_POINT ( 'NONE',  ( 2.528100132419516033, 38.15966356554061178, -17.49553815110665056 ) ) ;
#35532 = EDGE_LOOP ( 'NONE', ( #2489, #11374, #20198, #47327 ) ) ;
#35533 = CARTESIAN_POINT ( 'NONE',  ( 0.6029442701453590070, 16.87823742969306551, -46.11583596146973463 ) ) ;
#35534 = CARTESIAN_POINT ( 'NONE',  ( 2.281448460670572942, -19.56578495220138336, -43.80196084514300736 ) ) ;
#35535 = CARTESIAN_POINT ( 'NONE',  ( -6.016761891674564211, 18.68243340030203115, 2.456125503350775841 ) ) ;
#35536 = ORIENTED_EDGE ( 'NONE', *, *, #45229, .F. ) ;
#35537 = ORIENTED_EDGE ( 'NONE', *, *, #10534, .F. ) ;
#35538 = CARTESIAN_POINT ( 'NONE',  ( 0.6039202388192953519, -30.48176006895493728, 38.50228585353934108 ) ) ;
#35539 = CARTESIAN_POINT ( 'NONE',  ( 45.00000000000001421, 0.000000000000000000, 0.000000000000000000 ) ) ;
#35540 = FACE_OUTER_BOUND ( 'NONE', #8296, .T. ) ;
#35541 = B_SPLINE_CURVE_WITH_KNOTS ( 'NONE', 3,
 ( #32014, #41126, #55175, #7880, #26997, #27300 ),
 .UNSPECIFIED., .F., .F.,
 ( 4, 2, 4 ),
 ( 0.006456566858647417445, 0.007625406818786684658, 0.008794246778925951871 ),
 .UNSPECIFIED. ) ;
#35542 = EDGE_CURVE ( 'NONE', #51245, #50421, #54398, .T. ) ;
#35543 = ORIENTED_EDGE ( 'NONE', *, *, #21042, .F. ) ;
#35544 = AXIS2_PLACEMENT_3D ( 'NONE', #56540, #130, #23355 ) ;
#35545 = ORIENTED_EDGE ( 'NONE', *, *, #14785, .T. ) ;
#35546 =( BOUNDED_SURFACE ( )  B_SPLINE_SURFACE ( 3, 1, ( 
 ( #17310, #36427 ),
 ( #55495, #50805 ),
 ( #27014, #27938 ),
 ( #42365, #13539 ) ),
 .UNSPECIFIED., .F., .F., .F. ) 
 B_SPLINE_SURFACE_WITH_KNOTS ( ( 4, 4 ),
 ( 2, 2 ),
 ( 0.000000000000000000, 1.000000000000000000 ),
 ( 0.000000000000000000, 1.000000000000000000 ),
 .UNSPECIFIED. ) 
 GEOMETRIC_REPRESENTATION_ITEM ( )  RATIONAL_B_SPLINE_SURFACE ( (
 ( 1.000000000000000000, 1.000000000000000000),
 ( 0.9953390228620291325, 0.8624445117761032620),
 ( 0.9953390228620291325, 0.8624445117761032620),
 ( 1.000000000000000000, 1.000000000000000000) ) ) 
 REPRESENTATION_ITEM ( '' )  SURFACE ( )  );
#35547 = CARTESIAN_POINT ( 'NONE',  ( 0.5782707292762442330, -44.53844888462766249, 14.69907904118576170 ) ) ;
#35548 = CARTESIAN_POINT ( 'NONE',  ( 0.8557997880470690211, 7.156447707085701104, 47.37054680076709445 ) ) ;
#35549 = CARTESIAN_POINT ( 'NONE',  ( 0.5835871038041867687, -38.58555166310420503, -26.65313594598980629 ) ) ;
#35550 = ORIENTED_EDGE ( 'NONE', *, *, #56374, .T. ) ;
#35551 = CARTESIAN_POINT ( 'NONE',  ( 4.549368137175248350, -40.71620287708353914, 13.59764261105679317 ) ) ;
#35552 = B_SPLINE_CURVE_WITH_KNOTS ( 'NONE', 3,
 ( #58642, #53948, #44912, #1949 ),
 .UNSPECIFIED., .F., .F.,
 ( 4, 4 ),
 ( 0.000000000000000000, 0.004048833967417085622 ),
 .UNSPECIFIED. ) ;
#35553 = EDGE_CURVE ( 'NONE', #54938, #32404, #7161, .T. ) ;
#35554 = CARTESIAN_POINT ( 'NONE',  ( 0.6001305935487315502, -48.10757715638248300, 0.5236757026887750577 ) ) ;
#35555 = ADVANCED_FACE ( 'NONE', ( #22148 ), #12364, .F. ) ;
#35556 = VECTOR ( 'NONE', #4911, 1000.000000000000114 ) ;
#35557 = CARTESIAN_POINT ( 'NONE',  ( 0.7048096507298579061, 19.18768066167122655, -44.11842270945954425 ) ) ;
#35558 = VERTEX_POINT ( 'NONE', #23686 ) ;
#35559 = VERTEX_POINT ( 'NONE', #27457 ) ;
#35560 = CARTESIAN_POINT ( 'NONE',  ( 1.231276596079881047, 29.74482033789362134, -29.53849072116746655 ) ) ;
#35561 = CARTESIAN_POINT ( 'NONE',  ( -6.010958268070873523, -9.409153349053472226, -16.32616437357121697 ) ) ;
#35562 = AXIS2_PLACEMENT_3D ( 'NONE', #40565, #30815, #32076 ) ;
#35563 = B_SPLINE_CURVE_WITH_KNOTS ( 'NONE', 3,
 ( #12098, #45603, #46225, #55273, #45303, #21164, #30862, #49660, #40608, #12397, #36207, #60589, #41525, #59986, #6718, #11783 ),
 .UNSPECIFIED., .F., .F.,
 ( 4, 3, 3, 3, 3, 4 ),
 ( 1.250973872328959318E-17, 0.0002724568934985464397, 0.0004086836638483691965, 0.0005449104342063506830, 0.0008173270854453626617, 0.001089761613562683371 ),
 .UNSPECIFIED. ) ;
#35564 = ORIENTED_EDGE ( 'NONE', *, *, #58455, .T. ) ;
#35565 = CARTESIAN_POINT ( 'NONE',  ( 4.967162193818130511, -28.74031574029989855, -32.10009971360102554 ) ) ;
#35566 = CARTESIAN_POINT ( 'NONE',  ( 0.1073791018717483448, 37.58707531572176919, 21.14095454447572564 ) ) ;
#35567 = CARTESIAN_POINT ( 'NONE',  ( 0.6017666602106489515, 46.55749120190029799, 12.11361215600196140 ) ) ;
#35568 = CARTESIAN_POINT ( 'NONE',  ( 2.528100132419519142, 41.74865220873254401, 4.393610973489210814 ) ) ;
#35569 = AXIS2_PLACEMENT_3D ( 'NONE', #32730, #3881, #35669 ) ;
#35570 = EDGE_LOOP ( 'NONE', ( #58187, #36625, #54719, #43488 ) ) ;
#35571 = DIRECTION ( 'NONE',  ( 0.000000000000000000, 1.000000000000000000, -1.287488025362403787E-15 ) ) ;
#35572 = CARTESIAN_POINT ( 'NONE',  ( 0.6027444965799114707, -35.36702213964480279, 34.06922747673207397 ) ) ;
#35573 = CARTESIAN_POINT ( 'NONE',  ( 0.9758171775293923433, -21.45936886481769079, -37.15687890897639534 ) ) ;
#35574 = ORIENTED_EDGE ( 'NONE', *, *, #59546, .F. ) ;
#35575 = CARTESIAN_POINT ( 'NONE',  ( 50.00005079999999680, 12.80000000000000071, 3.000000000000000000 ) ) ;
#35576 = CARTESIAN_POINT ( 'NONE',  ( 0.7056313189692721144, 5.532685211636314548, 46.57400603669923811 ) ) ;
#35577 = ORIENTED_EDGE ( 'NONE', *, *, #54635, .F. ) ;
#35578 = CARTESIAN_POINT ( 'NONE',  ( -2.739355103387248747, 3.064916856561631597, -14.61005994557795695 ) ) ;
#35579 = CARTESIAN_POINT ( 'NONE',  ( 5.901463166500146684, -19.93124146756676396, 2.695085138206950504 ) ) ;
#35580 = ORIENTED_EDGE ( 'NONE', *, *, #54437, .T. ) ;
#35581 = DIRECTION ( 'NONE',  ( -0.07500201931887527651, 0.7028774959224980412, 0.7073456883475078838 ) ) ;
#35582 = CARTESIAN_POINT ( 'NONE',  ( -2.739355103387247858, 12.36564479942402350, 8.362917890634497198 ) ) ;
#35583 = EDGE_CURVE ( 'NONE', #13148, #24845, #9636, .T. ) ;
#35584 = CARTESIAN_POINT ( 'NONE',  ( -1.500000000000001110, 6.245698675651501825E-16, 5.100000000000000533 ) ) ;
#35585 = B_SPLINE_CURVE_WITH_KNOTS ( 'NONE', 3,
 ( #59893, #40515, #45516, #30768, #16373, #44910, #2252, #50803, #54553, #36425, #22313, #7893, #3185, #54875, #45217, #49887, #45830, #41442, #21688, #12011, #27012, #46137, #17613, #36124, #40832 ),
 .UNSPECIFIED., .F., .F.,
 ( 4, 3, 3, 3, 3, 3, 3, 3, 4 ),
 ( 4.670885906470169154E-18, 0.0005656085177311400737, 0.001131215744874499406, 0.001696821861372765699, 0.002262427090022497717, 0.002828031679238745058, 0.003393635864401603995, 0.003977030878808130755, 0.004561030005651157265 ),
 .UNSPECIFIED. ) ;
#35586 = EDGE_CURVE ( 'NONE', #55407, #58295, #18644, .T. ) ;
#35587 = CARTESIAN_POINT ( 'NONE',  ( 0.5848930533535030563, 32.47085631013385409, 33.83661586025115042 ) ) ;
#35588 = CARTESIAN_POINT ( 'NONE',  ( 4.967162193818130511, 0.000000000000000000, 0.000000000000000000 ) ) ;
#35589 = CARTESIAN_POINT ( 'NONE',  ( 0.5838002273316427182, 46.29900743592995127, -12.26477999444020028 ) ) ;
#35590 = CARTESIAN_POINT ( 'NONE',  ( 1.830465331921976802, 36.22942041522664169, 25.05604023494431942 ) ) ;
#35591 = CARTESIAN_POINT ( 'NONE',  ( -6.078075953587585900, -19.21681836813551314, 1.228440496412283478 ) ) ;
#35592 = DIRECTION ( 'NONE',  ( 0.000000000000000000, 0.000000000000000000, 1.000000000000000000 ) ) ;
#35593 = ADVANCED_FACE ( 'NONE', ( #19010 ), #55141, .F. ) ;
#35594 = CARTESIAN_POINT ( 'NONE',  ( 0.6024113833632039894, 41.27473200771225237, -26.60711120720173639 ) ) ;
#35595 = EDGE_CURVE ( 'NONE', #37991, #29994, #49243, .T. ) ;
#35596 = CARTESIAN_POINT ( 'NONE',  ( 0.9787464366903551038, 14.89694933529458609, 39.17160825639061983 ) ) ;
#35597 = ORIENTED_EDGE ( 'NONE', *, *, #25592, .T. ) ;
#35598 = EDGE_CURVE ( 'NONE', #40951, #34089, #53009, .T. ) ;
#35599 = CARTESIAN_POINT ( 'NONE',  ( 0.8560838555295223751, 16.00311602465208694, -44.09391240957481273 ) ) ;
#35600 = CARTESIAN_POINT ( 'NONE',  ( 0.5998501479064708430, 44.64337787626247689, -17.92509395669061689 ) ) ;
#35601 = CARTESIAN_POINT ( 'NONE',  ( 0.9754292580325150119, -34.87747760158924848, 23.23551211087558244 ) ) ;
#35602 = CARTESIAN_POINT ( 'NONE',  ( 4.549368137175248350, -38.59302160394766901, 18.79584381673463866 ) ) ;
#35603 = CARTESIAN_POINT ( 'NONE',  ( 0.8751705887134553219, -28.56654290188682666, 38.69254731947783199 ) ) ;
#35604 = CARTESIAN_POINT ( 'NONE',  ( 5.901463166500145796, 5.972693816097719655, -19.20533256467548711 ) ) ;
#35605 = DIRECTION ( 'NONE',  ( -1.296729604463824202E-16, 0.7099284060911065231, 0.7042738517259753417 ) ) ;
#35606 = CARTESIAN_POINT ( 'NONE',  ( 0.6027935024548038978, -44.51201578381240864, 18.24855952726150932 ) ) ;
#35607 =( BOUNDED_SURFACE ( )  B_SPLINE_SURFACE ( 3, 1, ( 
 ( #40282, #25520 ),
 ( #16756, #54623 ),
 ( #36182, #11435 ),
 ( #20835, #2631 ) ),
 .UNSPECIFIED., .F., .F., .F. ) 
 B_SPLINE_SURFACE_WITH_KNOTS ( ( 4, 4 ),
 ( 2, 2 ),
 ( 0.000000000000000000, 1.000000000000000000 ),
 ( 0.000000000000000000, 1.000000000000000000 ),
 .UNSPECIFIED. ) 
 GEOMETRIC_REPRESENTATION_ITEM ( )  RATIONAL_B_SPLINE_SURFACE ( (
 ( 1.000000000000000000, 1.000000000000000000),
 ( 0.9953485035131437453, 0.8621029689291515030),
 ( 0.9953485035131437453, 0.8621029689291515030),
 ( 1.000000000000000000, 1.000000000000000000) ) ) 
 REPRESENTATION_ITEM ( '' )  SURFACE ( )  );
#35608 = EDGE_CURVE ( 'NONE', #57221, #52094, #22182, .T. ) ;
#35609 = CARTESIAN_POINT ( 'NONE',  ( 0.6031356755773454870, 41.66225520948404437, -24.05374386753673122 ) ) ;
#35610 = CIRCLE ( 'NONE', #8557, 0.2000000000000000944 ) ;
#35611 = CARTESIAN_POINT ( 'NONE',  ( 0.9769922540276041456, 29.45054638516204903, -29.81605058859312152 ) ) ;
#35613 = ORIENTED_EDGE ( 'NONE', *, *, #44743, .F. ) ;
#35612 = CARTESIAN_POINT ( 'NONE',  ( 0.8751705887134423323, 7.160166390004303771, -47.55935879196464100 ) ) ;
#35614 = ORIENTED_EDGE ( 'NONE', *, *, #37418, .T. ) ;
#35615 = DIRECTION ( 'NONE',  ( -0.000000000000000000, 0.000000000000000000, 1.000000000000000000 ) ) ;
#35616 = FACE_OUTER_BOUND ( 'NONE', #53478, .T. ) ;
#35617 = CARTESIAN_POINT ( 'NONE',  ( 0.1119898979215352836, -42.82020512811597968, -10.64853703744787339 ) ) ;
#35618 = AXIS2_PLACEMENT_3D ( 'NONE', #61439, #22645, #4729 ) ;
#35619 = ORIENTED_EDGE ( 'NONE', *, *, #20415, .F. ) ;
#35620 = CARTESIAN_POINT ( 'NONE',  ( 4.553261556744873317, 43.92594400279101308, -0.2258523573157051323 ) ) ;
#35621 = CARTESIAN_POINT ( 'NONE',  ( 0.5806925824938499181, 32.20670061096218006, 34.08739940358331921 ) ) ;
#35622 = CARTESIAN_POINT ( 'NONE',  ( 0.1073791018717578927, -10.69234304550026593, -41.77800844988510676 ) ) ;
#35623 =( BOUNDED_SURFACE ( )  B_SPLINE_SURFACE ( 3, 1, ( 
 ( #15350, #34458 ),
 ( #53529, #10645 ),
 ( #21582, #26272 ),
 ( #45407, #16576 ) ),
 .UNSPECIFIED., .F., .F., .F. ) 
 B_SPLINE_SURFACE_WITH_KNOTS ( ( 4, 4 ),
 ( 2, 2 ),
 ( 0.000000000000000000, 1.000000000000000000 ),
 ( 0.000000000000000000, 1.000000000000000000 ),
 .UNSPECIFIED. ) 
 GEOMETRIC_REPRESENTATION_ITEM ( )  RATIONAL_B_SPLINE_SURFACE ( (
 ( 1.000000000000000000, 1.000000000000000000),
 ( 0.9952954269826590483, 0.8620686068821307169),
 ( 0.9952954269826590483, 0.8620686068821307169),
 ( 1.000000000000000000, 1.000000000000000000) ) ) 
 REPRESENTATION_ITEM ( '' )  SURFACE ( )  );
#35624 = ORIENTED_EDGE ( 'NONE', *, *, #18545, .T. ) ;
#35625 = ORIENTED_EDGE ( 'NONE', *, *, #38299, .F. ) ;
#35626 = CARTESIAN_POINT ( 'NONE',  ( 4.975610109902397937, 42.89797504594920241, 23.49921581872238718 ) ) ;
#35627 = CARTESIAN_POINT ( 'NONE',  ( 0.1098349054025745952, -10.95525583467247266, -41.70974743324811129 ) ) ;
#35628 = DIRECTION ( 'NONE',  ( 8.032841876251139751E-16, -4.551914400963141816E-15, 1.000000000000000000 ) ) ;
#35629 = EDGE_LOOP ( 'NONE', ( #45286, #27428, #3916, #4087 ) ) ;
#35630 = ORIENTED_EDGE ( 'NONE', *, *, #33689, .F. ) ;
#35631 = FACE_OUTER_BOUND ( 'NONE', #27292, .T. ) ;
#35632 = CARTESIAN_POINT ( 'NONE',  ( 0.5998501479064699549, -11.94461217097501837, 46.60114184914296942 ) ) ;
#35633 = ORIENTED_EDGE ( 'NONE', *, *, #8843, .F. ) ;
#35634 = ADVANCED_FACE ( 'NONE', ( #18071 ), #27531, .F. ) ;
#35635 = CARTESIAN_POINT ( 'NONE',  ( 0.1129192098497447394, 33.28205046155626690, -28.96993104685574139 ) ) ;
#35636 = FACE_OUTER_BOUND ( 'NONE', #38037, .T. ) ;
#35637 = VERTEX_POINT ( 'NONE', #60641 ) ;
#35638 = CARTESIAN_POINT ( 'NONE',  ( 0.5817217712918332229, -35.08429077047930633, 31.11796097338052292 ) ) ;
#35639 = CARTESIAN_POINT ( 'NONE',  ( 0.1368894036331272379, -6.411983869493682597, 43.65487130642680569 ) ) ;
#35640 = EDGE_LOOP ( 'NONE', ( #38735, #43320, #15963, #43644 ) ) ;
#35641 = DIRECTION ( 'NONE',  ( 1.836909530733573776E-16, -1.000000000000000000, 0.000000000000000000 ) ) ;
#35642 = CARTESIAN_POINT ( 'NONE',  ( 4.956445790443988031, 0.000000000000000000, 0.000000000000000000 ) ) ;
#35643 = CARTESIAN_POINT ( 'NONE',  ( 0.8560838555295158248, 46.35895890951125153, 7.156798369940231552 ) ) ;
#35644 = CARTESIAN_POINT ( 'NONE',  ( 5.960721111146673579, -18.96557324978293124, 7.848955554238177257 ) ) ;
#35645 = ORIENTED_EDGE ( 'NONE', *, *, #12189, .F. ) ;
#35646 = DIRECTION ( 'NONE',  ( 0.000000000000000000, 0.000000000000000000, 1.000000000000000000 ) ) ;
#35647 = CARTESIAN_POINT ( 'NONE',  ( 4.553261556744875094, 0.000000000000000000, 0.000000000000000000 ) ) ;
#35648 = ORIENTED_EDGE ( 'NONE', *, *, #5608, .T. ) ;
#35649 = DIRECTION ( 'NONE',  ( -1.000000000000000000, 0.000000000000000000, 0.000000000000000000 ) ) ;
#35650 = ORIENTED_EDGE ( 'NONE', *, *, #31259, .F. ) ;
#35651 = CARTESIAN_POINT ( 'NONE',  ( 0.9790320750461913857, 4.109333313230322027, 41.70672022903462306 ) ) ;
#35652 = EDGE_LOOP ( 'NONE', ( #32313, #42857, #58008, #23909 ) ) ;
#35653 = CARTESIAN_POINT ( 'NONE',  ( 5.959547316686252039, -0.003562808153049117858, 20.52562247508876681 ) ) ;
#35654 = CARTESIAN_POINT ( 'NONE',  ( 0.9762797500689124330, 25.26481495167865532, 33.43671500974846822 ) ) ;
#35655 = AXIS2_PLACEMENT_3D ( 'NONE', #39113, #48476, #58780 ) ;
#35656 = CARTESIAN_POINT ( 'NONE',  ( 4.833616638992208614, 38.20222678111939274, -26.07076047129095642 ) ) ;
#35657 = ORIENTED_EDGE ( 'NONE', *, *, #45096, .T. ) ;
#35658 = CARTESIAN_POINT ( 'NONE',  ( 5.896782393890504181, 14.92098591823879872, -13.48666994130618235 ) ) ;
#35659 = FACE_OUTER_BOUND ( 'NONE', #14367, .T. ) ;
#35660 = CARTESIAN_POINT ( 'NONE',  ( 0.5804410086790514622, 16.34485605153927068, 43.95867983128994183 ) ) ;
#35661 = ORIENTED_EDGE ( 'NONE', *, *, #22156, .T. ) ;
#35662 = B_SPLINE_CURVE_WITH_KNOTS ( 'NONE', 3,
 ( #25758, #20757, #39892, #45207 ),
 .UNSPECIFIED., .F., .F.,
 ( 4, 4 ),
 ( 2.096810281905421196E-17, 0.004559932413162185935 ),
 .UNSPECIFIED. ) ;
#35663 = EDGE_CURVE ( 'NONE', #53844, #5378, #23164, .T. ) ;
#35664 = VERTEX_POINT ( 'NONE', #37189 ) ;
#35665 = LINE ( 'NONE', #26860, #51482 ) ;
#35666 = CARTESIAN_POINT ( 'NONE',  ( 0.9730545539215883499, -42.90536227157002003, -0.5054011016617259155 ) ) ;
#35667 = CARTESIAN_POINT ( 'NONE',  ( 4.691466044806102076, 24.49380602310761290, 37.25818859570315311 ) ) ;
#35668 = CARTESIAN_POINT ( 'NONE',  ( 0.1087620492084206414, -5.269740196867624071, -42.80136086877931945 ) ) ;
#35669 = DIRECTION ( 'NONE',  ( 0.000000000000000000, 0.000000000000000000, 1.000000000000000000 ) ) ;
#35670 = CARTESIAN_POINT ( 'NONE',  ( 0.5997462898726536595, -45.71211507932792273, 17.94308126043545215 ) ) ;
#35671 = ORIENTED_EDGE ( 'NONE', *, *, #29156, .T. ) ;
#35672 = EDGE_CURVE ( 'NONE', #13219, #14899, #32476, .T. ) ;
#35673 = CARTESIAN_POINT ( 'NONE',  ( 0.1073791018717578927, 37.58707531572206051, -21.14095454447521405 ) ) ;
#35674 = EDGE_CURVE ( 'NONE', #29310, #6759, #18688, .T. ) ;
#35675 = DIRECTION ( 'NONE',  ( -0.000000000000000000, 0.000000000000000000, 1.000000000000000000 ) ) ;
#35676 = ORIENTED_EDGE ( 'NONE', *, *, #51400, .T. ) ;
#35677 = EDGE_CURVE ( 'NONE', #43965, #5254, #37498, .T. ) ;
#35678 = DIRECTION ( 'NONE',  ( 0.000000000000000000, 0.000000000000000000, -1.000000000000000000 ) ) ;
#35679 = DIRECTION ( 'NONE',  ( 0.09835009131224567436, -0.2650256080583827112, 0.9592125346408675313 ) ) ;
#35680 = CARTESIAN_POINT ( 'NONE',  ( 0.5786265663353196143, 43.97352617418616205, 18.99608782658049932 ) ) ;
#35681 = DIRECTION ( 'NONE',  ( -0.07500201931887529039, -0.5251354798924672274, 0.8477071574878906057 ) ) ;
#35682 = B_SPLINE_CURVE_WITH_KNOTS ( 'NONE', 3,
 ( #37508, #48348, #14846, #13384 ),
 .UNSPECIFIED., .F., .F.,
 ( 4, 4 ),
 ( 7.505561329662603978E-17, 0.005004741218457486526 ),
 .UNSPECIFIED. ) ;
#35683 = FACE_OUTER_BOUND ( 'NONE', #3851, .T. ) ;
#35684 = LINE ( 'NONE', #25952, #55072 ) ;
#35685 = CARTESIAN_POINT ( 'NONE',  ( 0.5997462898726536595, -19.39900779840473888, 45.11352487427402025 ) ) ;
#35686 = CARTESIAN_POINT ( 'NONE',  ( 0.9972139404380291339, -42.62325912566429054, -4.947665363829212737 ) ) ;
#35687 = CARTESIAN_POINT ( 'NONE',  ( 3.407937589446178528, -13.34359005742687110, -3.099921468255143253 ) ) ;
#35688 = CARTESIAN_POINT ( 'NONE',  ( 4.291220156522059348, -17.85566473792906450, -43.59546116366212942 ) ) ;
#35689 = CARTESIAN_POINT ( 'NONE',  ( 2.299652685299202748, -36.10726366766370887, 33.17449676019164428 ) ) ;
#35691 = EDGE_CURVE ( 'NONE', #59165, #59626, #13687, .T. ) ;
#35690 = DIRECTION ( 'NONE',  ( 0.000000000000000000, 0.000000000000000000, -1.000000000000000000 ) ) ;
#35692 = CARTESIAN_POINT ( 'NONE',  ( 0.2885700199627513340, 0.8047882683532806558, 43.10898996868493782 ) ) ;
#35693 = CARTESIAN_POINT ( 'NONE',  ( 0.9789233960466705575, 9.587306714400842367, 40.79730722481993865 ) ) ;
#35694 = EDGE_CURVE ( 'NONE', #18038, #45374, #5171, .T. ) ;
#35695 = CARTESIAN_POINT ( 'NONE',  ( 0.6254311100348646235, 11.78487556908942224, 46.64066536338341251 ) ) ;
#35696 = CARTESIAN_POINT ( 'NONE',  ( 5.960221823109900008, 10.25807604135621531, -17.77840967225710145 ) ) ;
#35697 = VERTEX_POINT ( 'NONE', #15530 ) ;
#35698 = CARTESIAN_POINT ( 'NONE',  ( 0.1103744047535531458, 11.19884698423366842, -41.64495780681027526 ) ) ;
#35699 =( BOUNDED_SURFACE ( )  B_SPLINE_SURFACE ( 3, 1, ( 
 ( #47146, #23329 ),
 ( #28328, #36513 ),
 ( #18635, #46844 ),
 ( #47444, #46525 ) ),
 .UNSPECIFIED., .F., .F., .F. ) 
 B_SPLINE_SURFACE_WITH_KNOTS ( ( 4, 4 ),
 ( 2, 2 ),
 ( 0.000000000000000000, 1.000000000000000000 ),
 ( 0.000000000000000000, 1.000000000000000000 ),
 .UNSPECIFIED. ) 
 GEOMETRIC_REPRESENTATION_ITEM ( )  RATIONAL_B_SPLINE_SURFACE ( (
 ( 1.000000000000000000, 1.000000000000000000),
 ( 0.7282232189291693025, 0.9929344683865674037),
 ( 0.7282232189291693025, 0.9929344683865674037),
 ( 1.000000000000000000, 1.000000000000000000) ) ) 
 REPRESENTATION_ITEM ( '' )  SURFACE ( )  );
#35700 = DIRECTION ( 'NONE',  ( -1.000000000000000000, 0.000000000000000000, -0.000000000000000000 ) ) ;
#35701 = AXIS2_PLACEMENT_3D ( 'NONE', #60575, #27083, #12694 ) ;
#35702 = CARTESIAN_POINT ( 'NONE',  ( 0.9745511491811753579, -25.84997388131836260, -34.24777528633308066 ) ) ;
#35703 = LINE ( 'NONE', #12505, #43257 ) ;
#35704 = CARTESIAN_POINT ( 'NONE',  ( -1.129531546211723025, 0.000000000000000000, 0.000000000000000000 ) ) ;
#35705 = VECTOR ( 'NONE', #35342, 999.9999999999998863 ) ;
#35706 = ORIENTED_EDGE ( 'NONE', *, *, #51837, .T. ) ;
#35707 = CARTESIAN_POINT ( 'NONE',  ( 4.833616638992208614, 14.43699082351714225, -43.93936707042086454 ) ) ;
#35708 = DIRECTION ( 'NONE',  ( -1.000000000000000000, -0.000000000000000000, -0.000000000000000000 ) ) ;
#35709 = CARTESIAN_POINT ( 'NONE',  ( 4.962356264823603702, 26.83784316460332420, -32.41860225448503030 ) ) ;
#35710 = ORIENTED_EDGE ( 'NONE', *, *, #10296, .T. ) ;
#35711 = EDGE_CURVE ( 'NONE', #19244, #53602, #14186, .T. ) ;
#35712 = B_SPLINE_CURVE_WITH_KNOTS ( 'NONE', 3,
 ( #18427, #46633, #47551, #42255, #32222, #57218 ),
 .UNSPECIFIED., .F., .F.,
 ( 4, 2, 4 ),
 ( 7.770031522344853663E-18, 0.0002291966416970820058, 0.0004583932833941562054 ),
 .UNSPECIFIED. ) ;
#35713 = CARTESIAN_POINT ( 'NONE',  ( 0.8560838555295158248, 46.60258007729424889, -5.345312359545362213 ) ) ;
#35714 = VERTEX_POINT ( 'NONE', #48719 ) ;
#35715 = AXIS2_PLACEMENT_3D ( 'NONE', #21339, #49841, #40469 ) ;
#35716 = LINE ( 'NONE', #20674, #24855 ) ;
#35717 = CARTESIAN_POINT ( 'NONE',  ( 10.00000000000001599, -56.56854249492410958, 56.56854249492351983 ) ) ;
#35718 = ORIENTED_EDGE ( 'NONE', *, *, #10222, .F. ) ;
#35719 = FACE_OUTER_BOUND ( 'NONE', #18997, .T. ) ;
#35720 = ORIENTED_EDGE ( 'NONE', *, *, #57156, .F. ) ;
#35721 = CARTESIAN_POINT ( 'NONE',  ( 5.965394784446458765, 14.50338846149133154, -14.52385693118987575 ) ) ;
#35722 = CARTESIAN_POINT ( 'NONE',  ( 0.1102847568649952675, -26.32556309315093301, -34.15672344772079327 ) ) ;
#35723 =( BOUNDED_SURFACE ( )  B_SPLINE_SURFACE ( 3, 1, ( 
 ( #52798, #53406 ),
 ( #23684, #16761 ),
 ( #35875, #7322 ),
 ( #45583, #40286 ) ),
 .UNSPECIFIED., .F., .F., .F. ) 
 B_SPLINE_SURFACE_WITH_KNOTS ( ( 4, 4 ),
 ( 2, 2 ),
 ( 0.000000000000000000, 1.000000000000000000 ),
 ( 0.000000000000000000, 1.000000000000000000 ),
 .UNSPECIFIED. ) 
 GEOMETRIC_REPRESENTATION_ITEM ( )  RATIONAL_B_SPLINE_SURFACE ( (
 ( 1.000000000000000000, 1.000000000000000000),
 ( 0.9952954269826590483, 0.8620686068821307169),
 ( 0.9952954269826590483, 0.8620686068821307169),
 ( 1.000000000000000000, 1.000000000000000000) ) ) 
 REPRESENTATION_ITEM ( '' )  SURFACE ( )  );
#35724 = ORIENTED_EDGE ( 'NONE', *, *, #38138, .F. ) ;
#35725 = VERTEX_POINT ( 'NONE', #34952 ) ;
#35726 = VERTEX_POINT ( 'NONE', #29003 ) ;
#35727 = CARTESIAN_POINT ( 'NONE',  ( 0.1084644655670281010, 11.54510651093203144, 41.55047717876508528 ) ) ;
#35728 = ORIENTED_EDGE ( 'NONE', *, *, #38471, .F. ) ;
#35729 = ORIENTED_EDGE ( 'NONE', *, *, #43504, .T. ) ;
#35730 = CARTESIAN_POINT ( 'NONE',  ( 0.9740398440564311811, -0.4145941695170031194, -42.90647580953696405 ) ) ;
#35731 = CARTESIAN_POINT ( 'NONE',  ( 0.5980271706414711508, 41.53842981737997775, -26.20320764998554353 ) ) ;
#35732 = CARTESIAN_POINT ( 'NONE',  ( 3.660176727303416477, 45.06760739764710877, -16.63097650367919655 ) ) ;
#35733 = DIRECTION ( 'NONE',  ( 0.000000000000000000, 0.000000000000000000, -1.000000000000000000 ) ) ;
#35734 = ORIENTED_EDGE ( 'NONE', *, *, #3125, .F. ) ;
#35735 = CARTESIAN_POINT ( 'NONE',  ( 0.9762797500689124330, -17.18051571332144434, 38.22505284509125545 ) ) ;
#35736 = DIRECTION ( 'NONE',  ( -0.1011922191286467598, 0.9849719771322121842, 0.1399654923617988100 ) ) ;
#35737 = B_SPLINE_CURVE_WITH_KNOTS ( 'NONE', 3,
 ( #56344, #52262, #8740, #42587, #52573, #28460 ),
 .UNSPECIFIED., .F., .F.,
 ( 4, 2, 4 ),
 ( 7.023086426956682172E-18, 0.0002448709889506552593, 0.0004897419779013034713 ),
 .UNSPECIFIED. ) ;
#35738 = ORIENTED_EDGE ( 'NONE', *, *, #23694, .F. ) ;
#35739 = ORIENTED_EDGE ( 'NONE', *, *, #34044, .F. ) ;
#35740 = CARTESIAN_POINT ( 'NONE',  ( 0.9736507210033049642, 34.31386771842698380, -25.76216842460662448 ) ) ;
#35741 = CARTESIAN_POINT ( 'NONE',  ( 1.827326673878742147, -22.58371678864607901, 36.65065268305619384 ) ) ;
#35742 = CARTESIAN_POINT ( 'NONE',  ( 5.960721111146673579, 17.77250458025991975, -10.26825948882907191 ) ) ;
#35743 = VERTEX_POINT ( 'NONE', #798 ) ;
#35744 = CARTESIAN_POINT ( 'NONE',  ( -6.078075953587585900, -16.14115596471627612, -10.50039324834266452 ) ) ;
#35745 = FACE_OUTER_BOUND ( 'NONE', #56150, .T. ) ;
#35746 = DIRECTION ( 'NONE',  ( 1.000000000000000000, 0.000000000000000000, 0.000000000000000000 ) ) ;
#35747 = EDGE_CURVE ( 'NONE', #41171, #33079, #26838, .T. ) ;
#35748 = VECTOR ( 'NONE', #16516, 999.9999999999998863 ) ;
#35749 =( GEOMETRIC_REPRESENTATION_CONTEXT ( 3 ) GLOBAL_UNCERTAINTY_ASSIGNED_CONTEXT ( ( #17350 ) ) GLOBAL_UNIT_ASSIGNED_CONTEXT ( ( #20710, #31032, #21328 ) ) REPRESENTATION_CONTEXT ( 'NONE', 'WORKASPACE' ) );
#35750 = VERTEX_POINT ( 'NONE', #34634 ) ;
#35751 = CARTESIAN_POINT ( 'NONE',  ( 3.661921753702032323, 42.53630361713042163, -20.08218111723261146 ) ) ;
#35752 = EDGE_LOOP ( 'NONE', ( #3076, #12992, #40447, #5010 ) ) ;
#35753 = CIRCLE ( 'NONE', #13698, 48.09070567114147110 ) ;
#35754 = EDGE_CURVE ( 'NONE', #37975, #57176, #22404, .T. ) ;
#35755 = CARTESIAN_POINT ( 'NONE',  ( 0.9747592971366217940, -33.84353661172422534, 26.37717450293414956 ) ) ;
#35756 = CARTESIAN_POINT ( 'NONE',  ( 5.965394784446458765, -7.868087674480825022, -18.95742317323941961 ) ) ;
#35757 = EDGE_LOOP ( 'NONE', ( #21820, #34692, #28541, #21389, #12873, #8801 ) ) ;
#35758 = CARTESIAN_POINT ( 'NONE',  ( 0.9752132459055865565, 21.25214916889643035, -37.27572867006939106 ) ) ;
#35759 = CIRCLE ( 'NONE', #43775, 4.000000000000000888 ) ;
#35760 = CARTESIAN_POINT ( 'NONE',  ( 4.833616638992208614, -3.476827473557542625, -46.11947910922908989 ) ) ;
#35761 = CARTESIAN_POINT ( 'NONE',  ( 0.1145239942831223490, -35.55610539828845162, 26.12869781696891636 ) ) ;
#35762 = CARTESIAN_POINT ( 'NONE',  ( 4.956653778116960396, -3.690426056930336429, 47.94889704119049867 ) ) ;
#35763 = CARTESIAN_POINT ( 'NONE',  ( 4.691466044806102964, -40.13652286047907580, 19.42108863068307301 ) ) ;
#35764 = ADVANCED_FACE ( 'NONE', ( #19306 ), #21494, .F. ) ;
#35765 = B_SPLINE_CURVE_WITH_KNOTS ( 'NONE', 3,
 ( #59921, #7921, #54903, #31738, #16714, #31424 ),
 .UNSPECIFIED., .F., .F.,
 ( 4, 2, 4 ),
 ( 8.848046324741092137E-18, 0.0002291978881530159703, 0.0004583957763060231044 ),
 .UNSPECIFIED. ) ;
#35766 = CARTESIAN_POINT ( 'NONE',  ( 5.960221823109900008, -19.82478916873571606, -5.317678907195369398 ) ) ;
#35767 = CARTESIAN_POINT ( 'NONE',  ( 2.281351352603290472, 37.24546109640818514, 30.23585463601389023 ) ) ;
#35768 = AXIS2_PLACEMENT_3D ( 'NONE', #61827, #9532, #23644 ) ;
#35769 = CARTESIAN_POINT ( 'NONE',  ( 4.962356264823608143, 41.15374796524913847, 8.809348799718396350 ) ) ;
#35770 = CARTESIAN_POINT ( 'NONE',  ( -6.890143360408123030, -11.60930335864404306, -1.199999999999999956 ) ) ;
#35771 = EDGE_LOOP ( 'NONE', ( #12729, #46064, #57687, #28426 ) ) ;
#35772 = CARTESIAN_POINT ( 'NONE',  ( 0.8744876279028263033, -19.05609938968970241, -45.24616145519706834 ) ) ;
#35773 = CARTESIAN_POINT ( 'NONE',  ( 4.975801465491695552, 14.85979367497174408, -45.55012473237738391 ) ) ;
#35774 = CARTESIAN_POINT ( 'NONE',  ( 3.050102900204245682, -42.05946948370080207, 12.90063083448639247 ) ) ;
#35775 = VERTEX_POINT ( 'NONE', #58102 ) ;
#35776 = CARTESIAN_POINT ( 'NONE',  ( 4.967162193818130511, 18.65818244221310351, -38.83676580803746958 ) ) ;
#35777 = CARTESIAN_POINT ( 'NONE',  ( 8.000000000000012434, -85.00000000000001421, -1.540743955509788245E-31 ) ) ;
#35778 = VERTEX_POINT ( 'NONE', #39660 ) ;
#35780 = CARTESIAN_POINT ( 'NONE',  ( 0.1129192098497455998, 3.754263797494300725, 43.96427289429426821 ) ) ;
#35779 = B_SPLINE_CURVE_WITH_KNOTS ( 'NONE', 3,
 ( #54675, #11804, #60005, #30883 ),
 .UNSPECIFIED., .F., .F.,
 ( 4, 4 ),
 ( 0.000000000000000000, 0.004445488388166994251 ),
 .UNSPECIFIED. ) ;
#35781 = EDGE_CURVE ( 'NONE', #59710, #46145, #43436, .T. ) ;
#35782 = CARTESIAN_POINT ( 'NONE',  ( 0.9757892942422830007, -41.45966865212799490, -11.05594550521687935 ) ) ;
#35783 = AXIS2_PLACEMENT_3D ( 'NONE', #24216, #43352, #14227 ) ;
#35784 = ORIENTED_EDGE ( 'NONE', *, *, #47538, .F. ) ;
#35785 = VECTOR ( 'NONE', #28848, 1000.000000000000114 ) ;
#35786 = VECTOR ( 'NONE', #14756, 1000.000000000000114 ) ;
#35787 = ORIENTED_EDGE ( 'NONE', *, *, #44884, .F. ) ;
#35788 = ORIENTED_EDGE ( 'NONE', *, *, #36445, .T. ) ;
#35789 = CARTESIAN_POINT ( 'NONE',  ( 0.1129192098497447394, 44.06201484046244587, 2.343210614524684487 ) ) ;
#35790 = ORIENTED_EDGE ( 'NONE', *, *, #29576, .F. ) ;
#35791 = CARTESIAN_POINT ( 'NONE',  ( 0.5988103622719987973, 41.96244039798791903, -23.52668907282300736 ) ) ;
#35792 = EDGE_CURVE ( 'NONE', #52112, #19096, #41849, .T. ) ;
#35793 = ORIENTED_EDGE ( 'NONE', *, *, #49707, .F. ) ;
#35794 = CARTESIAN_POINT ( 'NONE',  ( 0.8560838555295158248, 11.76118766017326323, -45.40977096290972526 ) ) ;
#35795 =( BOUNDED_SURFACE ( )  B_SPLINE_SURFACE ( 3, 1, ( 
 ( #49961, #17077 ),
 ( #22931, #45284 ),
 ( #56725, #26148 ),
 ( #31154, #35876 ) ),
 .UNSPECIFIED., .F., .F., .F. ) 
 B_SPLINE_SURFACE_WITH_KNOTS ( ( 4, 4 ),
 ( 2, 2 ),
 ( 0.000000000000000000, 1.000000000000000000 ),
 ( 0.000000000000000000, 1.000000000000000000 ),
 .UNSPECIFIED. ) 
 GEOMETRIC_REPRESENTATION_ITEM ( )  RATIONAL_B_SPLINE_SURFACE ( (
 ( 1.000000000000000000, 1.000000000000000000),
 ( 0.9729067724841187204, 0.9999501103223794596),
 ( 0.9729067724841187204, 0.9999501103223794596),
 ( 1.000000000000000000, 1.000000000000000000) ) ) 
 REPRESENTATION_ITEM ( '' )  SURFACE ( )  );
#35796 = CARTESIAN_POINT ( 'NONE',  ( 0.8760168074887076939, -5.394043284319854692, 47.80016357497240165 ) ) ;
#35797 = EDGE_CURVE ( 'NONE', #54460, #16494, #53771, .T. ) ;
#35798 = VERTEX_POINT ( 'NONE', #15224 ) ;
#35799 = CARTESIAN_POINT ( 'NONE',  ( 5.910764540655178756, -19.39351348817917753, 5.328496321944423464 ) ) ;
#35800 = CARTESIAN_POINT ( 'NONE',  ( 48.11837490430890085, 12.44569835165631311, -1.174889345006233432 ) ) ;
#35801 = CARTESIAN_POINT ( 'NONE',  ( 0.1102144999581333024, -30.58258619461942729, 30.40435207217175773 ) ) ;
#35802 = CARTESIAN_POINT ( 'NONE',  ( 5.958863334805807099, 16.28483817244722687, 12.49425770716493211 ) ) ;
#35803 = ORIENTED_EDGE ( 'NONE', *, *, #22859, .F. ) ;
#35804 = ORIENTED_EDGE ( 'NONE', *, *, #3340, .T. ) ;
#35805 = CIRCLE ( 'NONE', #49778, 47.91270532121795611 ) ;
#35806 = CARTESIAN_POINT ( 'NONE',  ( 0.8560838555295158248, -46.73345513967312570, -4.044379407262746362 ) ) ;
#35807 = CARTESIAN_POINT ( 'NONE',  ( 0.5782707292762423457, -14.58551739541048953, -44.57576736317388111 ) ) ;
#35808 = DIRECTION ( 'NONE',  ( -1.000000000000000000, -0.000000000000000000, -0.000000000000000000 ) ) ;
#35809 = ORIENTED_EDGE ( 'NONE', *, *, #17507, .T. ) ;
#35810 = CARTESIAN_POINT ( 'NONE',  ( 0.5827357941260201679, -46.35666768646128588, -12.04516435546850772 ) ) ;
#35811 = CARTESIAN_POINT ( 'NONE',  ( 0.5997462898726536595, -48.63480578518805686, 6.797594896825438049 ) ) ;
#35812 = CARTESIAN_POINT ( 'NONE',  ( 4.060580049360325461, 7.510230244653757659, -43.30201076198999033 ) ) ;
#35813 = CARTESIAN_POINT ( 'NONE',  ( -6.015611763856276717, -11.47596948473801248, -14.94556629257436953 ) ) ;
#35814 = EDGE_CURVE ( 'NONE', #40338, #2450, #52230, .T. ) ;
#35815 = CIRCLE ( 'NONE', #6731, 2.700000000000000622 ) ;
#35816 = ORIENTED_EDGE ( 'NONE', *, *, #32130, .F. ) ;
#35817 = ORIENTED_EDGE ( 'NONE', *, *, #29222, .F. ) ;
#35818 = CARTESIAN_POINT ( 'NONE',  ( 4.975610109902397937, -16.35148546628954236, 46.09857188876348744 ) ) ;
#35819 = CARTESIAN_POINT ( 'NONE',  ( 1.657374760986086271, 42.18470164349173501, 12.70202324442172426 ) ) ;
#35820 = EDGE_CURVE ( 'NONE', #31862, #60706, #19193, .T. ) ;
#35821 = LINE ( 'NONE', #26704, #29819 ) ;
#35822 = CARTESIAN_POINT ( 'NONE',  ( 4.962356264823602814, 6.570263404307167932, -41.57002810511882274 ) ) ;
#35823 = EDGE_CURVE ( 'NONE', #46743, #58288, #21683, .T. ) ;
#35824 = CARTESIAN_POINT ( 'NONE',  ( 0.3676999524040366896, -13.34038000160327364, -42.04741186726791113 ) ) ;
#35825 = CARTESIAN_POINT ( 'NONE',  ( 4.975610109902397937, 20.32389311291169065, 44.49032227207074186 ) ) ;
#35826 = CARTESIAN_POINT ( 'NONE',  ( 0.6029303876144825880, 12.57751758557269994, -46.43417959025978803 ) ) ;
#35827 = CARTESIAN_POINT ( 'NONE',  ( -6.057079549204054558, -12.94019084496092731, 14.26123038155291312 ) ) ;
#35828 = VECTOR ( 'NONE', #53197, 1000.000000000000114 ) ;
#35829 = CARTESIAN_POINT ( 'NONE',  ( 4.967162193818130511, -14.26841313271309808, 40.65506779172159924 ) ) ;
#35830 = CARTESIAN_POINT ( 'NONE',  ( 0.8557997880470599172, -41.93815086860273311, 23.15977007032308421 ) ) ;
#35831 = CARTESIAN_POINT ( 'NONE',  ( 3.376099380956838925, -10.24506893069234614, 8.645631627442240230 ) ) ;
#35832 = ADVANCED_FACE ( 'NONE', ( #49332 ), #9781, .T. ) ;
#35833 = CARTESIAN_POINT ( 'NONE',  ( 3.376099380956842921, -10.24506893069222002, -8.645631627442380562 ) ) ;
#35834 = CARTESIAN_POINT ( 'NONE',  ( 3.678748215320121862, 44.89637374983790608, 19.56855739226451263 ) ) ;
#35835 = CARTESIAN_POINT ( 'NONE',  ( 2.526464513654346433, 4.405490210169002552, -42.75268905308551126 ) ) ;
#35836 = CARTESIAN_POINT ( 'NONE',  ( 0.9772918015221170318, -22.19949068734035436, 35.54601903129756124 ) ) ;
#35837 = CARTESIAN_POINT ( 'NONE',  ( -6.078075953587585900, -4.279696274496966879, 18.77443405392537201 ) ) ;
#35838 = CARTESIAN_POINT ( 'NONE',  ( 0.8557997880470606944, 29.88293891557523807, -37.44587306708065455 ) ) ;
#35839 = CARTESIAN_POINT ( 'NONE',  ( 0.5997462898726536595, 48.29911994996563607, 8.873930482212578852 ) ) ;
#35841 = VERTEX_POINT ( 'NONE', #36118 ) ;
#35840 = DIRECTION ( 'NONE',  ( -0.1736481776669312471, 0.9848077530122077983, -5.551115123125779621E-17 ) ) ;
#35842 = ORIENTED_EDGE ( 'NONE', *, *, #52467, .F. ) ;
#35843 = CONICAL_SURFACE ( 'NONE', #59832, 42.08604991992415023, 1.569615340895231137 ) ;
#35844 = FACE_BOUND ( 'NONE', #35950, .T. ) ;
#35845 = CARTESIAN_POINT ( 'NONE',  ( 0.8751705887134553219, -48.08707113907594533, 0.8911681664086766874 ) ) ;
#35846 = CARTESIAN_POINT ( 'NONE',  ( 0.5997462898726536595, 44.46857747280011353, 20.83500054451363326 ) ) ;
#35847 = VERTEX_POINT ( 'NONE', #8489 ) ;
#35848 = ORIENTED_EDGE ( 'NONE', *, *, #17850, .T. ) ;
#35849 = DIRECTION ( 'NONE',  ( -0.000000000000000000, -0.000000000000000000, 1.000000000000000000 ) ) ;
#35850 = CARTESIAN_POINT ( 'NONE',  ( 4.967162193818130511, 0.000000000000000000, 0.000000000000000000 ) ) ;
#35851 = ORIENTED_EDGE ( 'NONE', *, *, #27426, .T. ) ;
#35852 = ORIENTED_EDGE ( 'NONE', *, *, #59974, .F. ) ;
#35853 = CARTESIAN_POINT ( 'NONE',  ( 0.5832367798473397924, 47.89515946578896433, 0.2724222379462135080 ) ) ;
#35854 = CARTESIAN_POINT ( 'NONE',  ( 5.959547316686252039, -18.96183906913538308, -7.858107265727685586 ) ) ;
#35855 = CARTESIAN_POINT ( 'NONE',  ( 0.8753041380234465318, 46.87455897190349674, -14.62580080072613775 ) ) ;
#35856 = EDGE_CURVE ( 'NONE', #19448, #31565, #50031, .T. ) ;
#35857 = ORIENTED_EDGE ( 'NONE', *, *, #27497, .F. ) ;
#35858 = CARTESIAN_POINT ( 'NONE',  ( 0.6001305935487315502, 6.798494447612227098, -47.62765676940936999 ) ) ;
#35859 = EDGE_CURVE ( 'NONE', #39947, #9360, #54016, .T. ) ;
#35860 = CARTESIAN_POINT ( 'NONE',  ( 4.549368137175248350, 24.02461520945223228, 35.57418903283122802 ) ) ;
#35861 = CARTESIAN_POINT ( 'NONE',  ( 0.2285344041767098100, 43.97331108839381386, -3.584561649462690625 ) ) ;
#35862 = ORIENTED_EDGE ( 'NONE', *, *, #20449, .F. ) ;
#35863 = EDGE_CURVE ( 'NONE', #50427, #37103, #32072, .T. ) ;
#35864 = VECTOR ( 'NONE', #19996, 1000.000000000000000 ) ;
#35865 = ORIENTED_EDGE ( 'NONE', *, *, #6119, .T. ) ;
#35866 = CARTESIAN_POINT ( 'NONE',  ( 1.088313998177379949, 0.7798619649927278630, -42.90642884828984194 ) ) ;
#35867 = CARTESIAN_POINT ( 'NONE',  ( -2.569797478183790229, -7.701637110048767276, 12.44213550320639783 ) ) ;
#35868 = ORIENTED_EDGE ( 'NONE', *, *, #51133, .F. ) ;
#35869 = FACE_OUTER_BOUND ( 'NONE', #14689, .T. ) ;
#35870 = CARTESIAN_POINT ( 'NONE',  ( 0.6008122571543326185, -7.407407791708222611, 48.54569867941606276 ) ) ;
#35871 = CARTESIAN_POINT ( 'NONE',  ( 0.8560838555295223751, 16.00311602465208694, -44.09391240957481273 ) ) ;
#35872 = CARTESIAN_POINT ( 'NONE',  ( -5.440000000000000391, 4.832908975360033023E-15, 0.000000000000000000 ) ) ;
#35873 = VERTEX_POINT ( 'NONE', #55182 ) ;
#35874 = CARTESIAN_POINT ( 'NONE',  ( 0.9749527285493317930, -30.13822974582791403, -30.54214995146802281 ) ) ;
#35875 = CARTESIAN_POINT ( 'NONE',  ( 5.895881250540457863, 5.963300346357911508, -19.20850672455900821 ) ) ;
#35876 = CARTESIAN_POINT ( 'NONE',  ( 0.5804410086790514622, -35.14691939471192939, 31.05179397260356922 ) ) ;
#35877 = CARTESIAN_POINT ( 'NONE',  ( 4.291220156522060236, 44.81988414002825039, -14.51092633087706574 ) ) ;
#35878 = ORIENTED_EDGE ( 'NONE', *, *, #59116, .T. ) ;
#35879 = CARTESIAN_POINT ( 'NONE',  ( 0.5850706913938533704, -47.89601588673689037, -0.1816364388705385968 ) ) ;
#35880 = CARTESIAN_POINT ( 'NONE',  ( -6.063463321072276813, 18.63085535290907302, 4.869464169541593890 ) ) ;
#35881 = CARTESIAN_POINT ( 'NONE',  ( 4.549368137175248350, 0.000000000000000000, 0.000000000000000000 ) ) ;
#35882 = EDGE_CURVE ( 'NONE', #54794, #60972, #38081, .T. ) ;
#35883 = CIRCLE ( 'NONE', #24873, 47.09074272231896430 ) ;
#35884 = VERTEX_POINT ( 'NONE', #46433 ) ;
#35885 = CARTESIAN_POINT ( 'NONE',  ( 15.24999999999999289, 2.688986455804112996, 8.896908036367455278E-17 ) ) ;
#35886 = EDGE_CURVE ( 'NONE', #10420, #23287, #55639, .T. ) ;
#35887 = CARTESIAN_POINT ( 'NONE',  ( 0.1103878639767399555, -42.74915604780183997, 5.676988162227942780 ) ) ;
#35888 = CARTESIAN_POINT ( 'NONE',  ( 5.959547316686252039, -10.25972575517517704, -17.77749189599214219 ) ) ;
#35889 = B_SPLINE_CURVE_WITH_KNOTS ( 'NONE', 3,
 ( #18756, #56941, #33162, #52238, #47565, #4604 ),
 .UNSPECIFIED., .F., .F.,
 ( 4, 2, 4 ),
 ( 5.421010862427522170E-19, 0.0002293801035737093178, 0.0004587602071474180935 ),
 .UNSPECIFIED. ) ;
#35890 = EDGE_CURVE ( 'NONE', #6786, #51504, #6602, .T. ) ;
#35891 = CARTESIAN_POINT ( 'NONE',  ( 3.376099380956842921, -13.03750648666903089, 3.119584626537648564 ) ) ;
#35893 = CARTESIAN_POINT ( 'NONE',  ( 5.895596859100789899, -9.669028665050088733, -17.63627137143583568 ) ) ;
#35892 = STYLED_ITEM ( 'NONE', ( #24028 ), #33281 ) ;
#35894 = CARTESIAN_POINT ( 'NONE',  ( 0.9747592971366254577, 42.90728926179866676, -0.3237797888856475126 ) ) ;
#35895 = DIRECTION ( 'NONE',  ( 0.000000000000000000, 0.000000000000000000, 1.000000000000000000 ) ) ;
#35896 = FACE_OUTER_BOUND ( 'NONE', #35629, .T. ) ;
#35897 = CARTESIAN_POINT ( 'NONE',  ( 4.956653778116992370, 27.17045123668527751, -39.67974989265010777 ) ) ;
#35898 = CARTESIAN_POINT ( 'NONE',  ( 2.618530812446115519, 42.70834099002650674, -19.63986759318458297 ) ) ;
#35899 = CARTESIAN_POINT ( 'NONE',  ( 0.5997462898726536595, -14.47257175146244457, -46.92649887902442885 ) ) ;
#35900 = ORIENTED_EDGE ( 'NONE', *, *, #53573, .F. ) ;
#35901 = VECTOR ( 'NONE', #17958, 1000.000000000000000 ) ;
#35902 = CARTESIAN_POINT ( 'NONE',  ( 0.8557997880470697982, 11.51622788066522851, -46.50333260518546297 ) ) ;
#35903 = CARTESIAN_POINT ( 'NONE',  ( 5.880360259849752858, -9.405269135695570881, 47.04104239318750302 ) ) ;
#35904 = CARTESIAN_POINT ( 'NONE',  ( 0.8751705887134553219, 0.8911681664081729792, 48.08707113907595243 ) ) ;
#35905 = CARTESIAN_POINT ( 'NONE',  ( 0.3622758884714600280, 31.06363466427727360, -29.89648521331598729 ) ) ;
#35906 = ADVANCED_FACE ( 'NONE', ( #51097 ), #8189, .T. ) ;
#35907 = B_SPLINE_CURVE_WITH_KNOTS ( 'NONE', 3,
 ( #19054, #52220, #5218, #37235, #43479, #23423 ),
 .UNSPECIFIED., .F., .F.,
 ( 4, 2, 4 ),
 ( 1.569810930355577320E-17, 0.0002448709889506590540, 0.0004897419779013023871 ),
 .UNSPECIFIED. ) ;
#35908 = CARTESIAN_POINT ( 'NONE',  ( 0.3622758884714600280, -31.06363466427748321, 29.89648521331577058 ) ) ;
#35909 = CARTESIAN_POINT ( 'NONE',  ( 0.9769922540276054779, -31.37627228715922456, 27.78238817035295938 ) ) ;
#35910 = CARTESIAN_POINT ( 'NONE',  ( 0.6845945791218034371, -42.25019583682509250, 20.37958469802246597 ) ) ;
#35911 =( BOUNDED_SURFACE ( )  B_SPLINE_SURFACE ( 3, 1, ( 
 ( #15239, #34047 ),
 ( #14939, #58727 ),
 ( #38751, #30540 ),
 ( #15542, #39673 ) ),
 .UNSPECIFIED., .F., .F., .F. ) 
 B_SPLINE_SURFACE_WITH_KNOTS ( ( 4, 4 ),
 ( 2, 2 ),
 ( 0.000000000000000000, 1.000000000000000000 ),
 ( 0.000000000000000000, 1.000000000000000000 ),
 .UNSPECIFIED. ) 
 GEOMETRIC_REPRESENTATION_ITEM ( )  RATIONAL_B_SPLINE_SURFACE ( (
 ( 1.000000000000000000, 1.000000000000000000),
 ( 0.9751682680413298332, 0.9999560080971552356),
 ( 0.9751682680413298332, 0.9999560080971552356),
 ( 1.000000000000000000, 1.000000000000000000) ) ) 
 REPRESENTATION_ITEM ( '' )  SURFACE ( )  );
#35912 = CARTESIAN_POINT ( 'NONE',  ( 1.834102595619085507, 36.18890472896515575, -25.11097209140993414 ) ) ;
#35913 = CIRCLE ( 'NONE', #17887, 2.649999999999992806 ) ;
#35914 = CARTESIAN_POINT ( 'NONE',  ( 4.553261556744875094, 0.000000000000000000, 0.000000000000000000 ) ) ;
#35916 = ORIENTED_EDGE ( 'NONE', *, *, #24714, .T. ) ;
#35915 = CARTESIAN_POINT ( 'NONE',  ( 5.838029081930955932, 44.61407408311357159, 15.51288019225876447 ) ) ;
#35917 = ORIENTED_EDGE ( 'NONE', *, *, #23972, .T. ) ;
#35918 = CARTESIAN_POINT ( 'NONE',  ( 2.281351352603296689, -11.14238889600251703, -46.66131639318008695 ) ) ;
#35919 = VECTOR ( 'NONE', #34963, 1000.000000000000114 ) ;
#35920 = CARTESIAN_POINT ( 'NONE',  ( 5.974727161628369032, 17.76736931401846320, 10.27590650342043510 ) ) ;
#35921 = CARTESIAN_POINT ( 'NONE',  ( 4.549368137175248350, -2.596185425821630588, -42.84816078363929392 ) ) ;
#35922 = B_SPLINE_CURVE_WITH_KNOTS ( 'NONE', 3,
 ( #53978, #6349, #15799, #44027, #11103, #1661 ),
 .UNSPECIFIED., .F., .F.,
 ( 4, 2, 4 ),
 ( 1.267774990240505488E-17, 0.0002445244328975401671, 0.0004890488657950676490 ),
 .UNSPECIFIED. ) ;
#35923 = ORIENTED_EDGE ( 'NONE', *, *, #2917, .T. ) ;
#35924 = DIRECTION ( 'NONE',  ( 0.000000000000000000, 8.881784197001252323E-16, 1.000000000000000000 ) ) ;
#35925 = CARTESIAN_POINT ( 'NONE',  ( 0.5839880159502346402, -47.49213420504720773, 6.206687493267523337 ) ) ;
#35926 = CARTESIAN_POINT ( 'NONE',  ( 0.1100053167205930910, 41.60823192620008371, -11.33468317718512530 ) ) ;
#35927 = VERTEX_POINT ( 'NONE', #18230 ) ;
#35928 = ORIENTED_EDGE ( 'NONE', *, *, #25423, .F. ) ;
#35929 = CARTESIAN_POINT ( 'NONE',  ( 0.8760168074886965917, -17.58183840866369252, -44.77533136581875084 ) ) ;
#35930 = AXIS2_PLACEMENT_3D ( 'NONE', #15477, #14872, #29250 ) ;
#35931 = DIRECTION ( 'NONE',  ( -1.000000000000000000, -0.000000000000000000, -0.000000000000000000 ) ) ;
#35932 = LINE ( 'NONE', #16501, #19957 ) ;
#35933 = ORIENTED_EDGE ( 'NONE', *, *, #34113, .F. ) ;
#35934 = EDGE_CURVE ( 'NONE', #40399, #50810, #18649, .T. ) ;
#35935 = B_SPLINE_CURVE_WITH_KNOTS ( 'NONE', 3,
 ( #33573, #20391, #33884, #10065, #43601, #53267, #24778, #10379, #43921, #20093, #39211, #58263, #16008, #26315, #26622, #54809, #31021, #21007, #35122 ),
 .UNSPECIFIED., .F., .F.,
 ( 4, 3, 3, 3, 3, 3, 4 ),
 ( 8.674294979774126656E-18, 0.0002732106629380573362, 0.0004098138914053730468, 0.0005464171197651428950, 0.0006830203481512527302, 0.0008196235766963571277, 0.001011968216111138342 ),
 .UNSPECIFIED. ) ;
#35936 = EDGE_LOOP ( 'NONE', ( #28291, #41360, #5068, #10292 ) ) ;
#35937 = ADVANCED_FACE ( 'NONE', ( #22614 ), #36420, .T. ) ;
#35938 = CARTESIAN_POINT ( 'NONE',  ( -6.078075953587585900, 9.977648803906024710, -16.46941706901153779 ) ) ;
#35939 = CARTESIAN_POINT ( 'NONE',  ( 0.5998501479064699549, -28.86886762351154090, 38.48283596221978797 ) ) ;
#35940 = ORIENTED_EDGE ( 'NONE', *, *, #5279, .F. ) ;
#35941 =( BOUNDED_SURFACE ( )  B_SPLINE_SURFACE ( 3, 1, ( 
 ( #46420, #8476 ),
 ( #10, #19151 ),
 ( #27917, #32938 ),
 ( #37644, #23833 ) ),
 .UNSPECIFIED., .F., .F., .F. ) 
 B_SPLINE_SURFACE_WITH_KNOTS ( ( 4, 4 ),
 ( 2, 2 ),
 ( 0.000000000000000000, 1.000000000000000000 ),
 ( 0.000000000000000000, 1.000000000000000000 ),
 .UNSPECIFIED. ) 
 GEOMETRIC_REPRESENTATION_ITEM ( )  RATIONAL_B_SPLINE_SURFACE ( (
 ( 1.000000000000000000, 1.000000000000000000),
 ( 0.7282232189291693025, 0.9929344683865674037),
 ( 0.7282232189291693025, 0.9929344683865674037),
 ( 1.000000000000000000, 1.000000000000000000) ) ) 
 REPRESENTATION_ITEM ( '' )  SURFACE ( )  );
#35942 = B_SPLINE_CURVE_WITH_KNOTS ( 'NONE', 3,
 ( #54898, #31107, #50822, #45535, #21710, #51427 ),
 .UNSPECIFIED., .F., .F.,
 ( 4, 2, 4 ),
 ( 0.000000000000000000, 0.0002291966416970797290, 0.0004583932833941594580 ),
 .UNSPECIFIED. ) ;
#35943 = CARTESIAN_POINT ( 'NONE',  ( 0.1129192098497447394, 29.30421273086510681, -32.98810246148386227 ) ) ;
#35944 = CARTESIAN_POINT ( 'NONE',  ( 0.9757402383260946888, 41.46830379850868553, -11.02350435907860948 ) ) ;
#35945 = ORIENTED_EDGE ( 'NONE', *, *, #16758, .F. ) ;
#35946 = EDGE_CURVE ( 'NONE', #21513, #43532, #61219, .T. ) ;
#35947 = ADVANCED_FACE ( 'NONE', ( #5017 ), #34314, .F. ) ;
#35948 = CARTESIAN_POINT ( 'NONE',  ( 2.500000000000000000, 2.357898499370431722, -2.818925648462311528E-15 ) ) ;
#35949 = CARTESIAN_POINT ( 'NONE',  ( 0.1129192098497447394, -6.563350895509266536, 43.63340707310824484 ) ) ;
#35950 = EDGE_LOOP ( 'NONE', ( #43521, #32428 ) ) ;
#35951 = CARTESIAN_POINT ( 'NONE',  ( 0.6017667736363750963, -47.64919355032684223, -6.625250263233462888 ) ) ;
#35952 = ADVANCED_FACE ( 'NONE', ( #56414 ), #21127, .F. ) ;
#35953 = CARTESIAN_POINT ( 'NONE',  ( 0.5806925824938499181, -20.23436166722466467, 42.30594485723624132 ) ) ;
#35954 = CARTESIAN_POINT ( 'NONE',  ( 0.9968887458511649369, 42.62316256128691805, -4.948372828380340316 ) ) ;
#35955 = PRESENTATION_STYLE_ASSIGNMENT (( #60327 ) ) ;
#35956 = ORIENTED_EDGE ( 'NONE', *, *, #20697, .T. ) ;
#35957 = LINE ( 'NONE', #60038, #61715 ) ;
#35958 = CARTESIAN_POINT ( 'NONE',  ( 0.1135584504625008762, 39.94012421351568776, -18.75469354439548653 ) ) ;
#35959 = ORIENTED_EDGE ( 'NONE', *, *, #33245, .T. ) ;
#35960 = CARTESIAN_POINT ( 'NONE',  ( 1.154321485836935279, -15.65787964449893011, 39.95809831208273266 ) ) ;
#35961 = EDGE_CURVE ( 'NONE', #13656, #6553, #42356, .T. ) ;
#35962 = VERTEX_POINT ( 'NONE', #42974 ) ;
#35963 = CARTESIAN_POINT ( 'NONE',  ( 0.5839254288179560604, -18.41284501069709023, 44.21529885210824062 ) ) ;
#35964 = ORIENTED_EDGE ( 'NONE', *, *, #52308, .F. ) ;
#35965 = CARTESIAN_POINT ( 'NONE',  ( 0.6846871229502899947, -0.8641397935256196483, -47.90045233486065968 ) ) ;
#35966 = CARTESIAN_POINT ( 'NONE',  ( 0.9784957157296372277, 25.04636459167678098, 33.60078388569483820 ) ) ;
#35967 = CARTESIAN_POINT ( 'NONE',  ( 4.691466044806103852, 36.88741755356070229, -25.04870410140750181 ) ) ;
#35968 = VERTEX_POINT ( 'NONE', #29155 ) ;
#35969 = CARTESIAN_POINT ( 'NONE',  ( 5.838029081930955932, -32.85120734338305226, 33.93911068715524237 ) ) ;
#35970 = LINE ( 'NONE', #55339, #45808 ) ;
#35971 = CARTESIAN_POINT ( 'NONE',  ( 4.975610109902397937, 45.11887670192763267, -18.88746601040027784 ) ) ;
#35972 = VERTEX_POINT ( 'NONE', #33566 ) ;
#35973 = B_SPLINE_CURVE_WITH_KNOTS ( 'NONE', 3,
 ( #44159, #39442, #18087, #45676 ),
 .UNSPECIFIED., .F., .F.,
 ( 4, 4 ),
 ( 0.000000000000000000, 0.005004741218457424944 ),
 .UNSPECIFIED. ) ;
#35974 =( BOUNDED_SURFACE ( )  B_SPLINE_SURFACE ( 3, 1, ( 
 ( #36750, #23544 ),
 ( #32652, #42673 ),
 ( #51735, #46450 ),
 ( #42371, #27948 ) ),
 .UNSPECIFIED., .F., .F., .F. ) 
 B_SPLINE_SURFACE_WITH_KNOTS ( ( 4, 4 ),
 ( 2, 2 ),
 ( 0.000000000000000000, 1.000000000000000000 ),
 ( 0.000000000000000000, 1.000000000000000000 ),
 .UNSPECIFIED. ) 
 GEOMETRIC_REPRESENTATION_ITEM ( )  RATIONAL_B_SPLINE_SURFACE ( (
 ( 1.000000000000000000, 1.000000000000000000),
 ( 0.9953390228620291325, 0.8624445117760984880),
 ( 0.9953390228620291325, 0.8624445117760984880),
 ( 1.000000000000000000, 1.000000000000000000) ) ) 
 REPRESENTATION_ITEM ( '' )  SURFACE ( )  );
#35975 = ORIENTED_EDGE ( 'NONE', *, *, #41331, .T. ) ;
#35976 = CARTESIAN_POINT ( 'NONE',  ( 2.500000000000000000, -1.178949249685214307, 2.042000000000001592 ) ) ;
#35977 = CARTESIAN_POINT ( 'NONE',  ( 0.6846871229502932144, -46.49193983736599023, 11.56285438919616126 ) ) ;
#35978 = CARTESIAN_POINT ( 'NONE',  ( 0.6029442701453591180, 33.07943709324084836, 36.29457351660987285 ) ) ;
#35979 = CARTESIAN_POINT ( 'NONE',  ( 1.227938101723756947, -0.8460948827222184443, -42.91134962331487657 ) ) ;
#35980 = DIRECTION ( 'NONE',  ( 0.8191520442889896891, 1.003171929053522158E-16, -0.5735764363510490460 ) ) ;
#35981 = LINE ( 'NONE', #46297, #23805 ) ;
#35982 = ORIENTED_EDGE ( 'NONE', *, *, #55697, .F. ) ;
#35983 = CARTESIAN_POINT ( 'NONE',  ( 0.1102144999581333024, 37.40973521037463456, -21.45299314243954925 ) ) ;
#35984 = CARTESIAN_POINT ( 'NONE',  ( 0.8560838555295158248, -46.14148336882297485, 8.446084690930096173 ) ) ;
#35985 = CONICAL_SURFACE ( 'NONE', #43996, 42.92674063221959813, 1.485477209440487556 ) ;
#35986 = ORIENTED_EDGE ( 'NONE', *, *, #1330, .F. ) ;
#35987 = FACE_OUTER_BOUND ( 'NONE', #54994, .T. ) ;
#35988 = CARTESIAN_POINT ( 'NONE',  ( 0.5834584762367743815, 36.69082382167502487, 29.20649647424346185 ) ) ;
#35989 = CARTESIAN_POINT ( 'NONE',  ( 0.6024113833632039894, 44.14939292512354285, 21.50285965735530169 ) ) ;
#35990 = CARTESIAN_POINT ( 'NONE',  ( 0.5830081025819929819, 45.30112779307347637, 12.12599913647833105 ) ) ;
#35991 = EDGE_CURVE ( 'NONE', #16981, #35341, #38274, .T. ) ;
#35992 = LINE ( 'NONE', #60073, #10709 ) ;
#35993 = LINE ( 'NONE', #7753, #60088 ) ;
#35994 = CARTESIAN_POINT ( 'NONE',  ( 0.6008122571543325074, 5.148691493768951410, 48.83692789649354182 ) ) ;
#35995 = CARTESIAN_POINT ( 'NONE',  ( 0.1145239942831223490, -12.24112153461662444, -42.39222127088197567 ) ) ;
#35996 =( BOUNDED_SURFACE ( )  B_SPLINE_SURFACE ( 3, 1, ( 
 ( #54289, #30494 ),
 ( #12892, #11731 ),
 ( #30809, #49929 ),
 ( #25194, #53987 ) ),
 .UNSPECIFIED., .F., .F., .F. ) 
 B_SPLINE_SURFACE_WITH_KNOTS ( ( 4, 4 ),
 ( 2, 2 ),
 ( 0.000000000000000000, 1.000000000000000000 ),
 ( 0.000000000000000000, 1.000000000000000000 ),
 .UNSPECIFIED. ) 
 GEOMETRIC_REPRESENTATION_ITEM ( )  RATIONAL_B_SPLINE_SURFACE ( (
 ( 1.000000000000000000, 1.000000000000000000),
 ( 0.9953040768229005630, 0.8617119497784937465),
 ( 0.9953040768229005630, 0.8617119497784937465),
 ( 1.000000000000000000, 1.000000000000000000) ) ) 
 REPRESENTATION_ITEM ( '' )  SURFACE ( )  );
#35997 = ADVANCED_FACE ( 'NONE', ( #42654 ), #26779, .T. ) ;
#35998 = CARTESIAN_POINT ( 'NONE',  ( 3.782542959838393948, -33.65309862801750285, -25.19338814311196018 ) ) ;
#35999 = CARTESIAN_POINT ( 'NONE',  ( 0.5850706913938533704, 6.071602062250609499, 47.50996714391784792 ) ) ;
#36000 = CARTESIAN_POINT ( 'NONE',  ( 4.975610109902397937, -36.86873347511144772, 32.14258700041067840 ) ) ;
#36001 = CARTESIAN_POINT ( 'NONE',  ( 4.303969348037258058, -20.38638383586087954, -43.57722561725979915 ) ) ;
#36002 = DIRECTION ( 'NONE',  ( 0.000000000000000000, 0.000000000000000000, 1.000000000000000000 ) ) ;
#36003 = CARTESIAN_POINT ( 'NONE',  ( 2.528190830796657185, -28.01583037401040244, 31.26287550126642145 ) ) ;
#36004 = CARTESIAN_POINT ( 'NONE',  ( 5.895881250540457863, -19.93280900245019183, 2.685294561150000092 ) ) ;
#36005 = PRODUCT_DEFINITION ( 'UNKNOWN', '', #48888, #39874 ) ;
#36006 = CARTESIAN_POINT ( 'NONE',  ( 1.092182651088184020, -7.740215841539130004, -41.19284213511701864 ) ) ;
#36007 = DIRECTION ( 'NONE',  ( -1.000000000000000000, -0.000000000000000000, -0.000000000000000000 ) ) ;
#36008 = APPLICATION_CONTEXT ( 'automotive_design' ) ;
#36009 = ORIENTED_EDGE ( 'NONE', *, *, #16131, .T. ) ;
#36010 = DIRECTION ( 'NONE',  ( 0.07439287786467664587, -0.2453289374370136722, -0.9665813013808186582 ) ) ;
#36011 = AXIS2_PLACEMENT_3D ( 'NONE', #20440, #35175, #21370 ) ;
#36012 = CARTESIAN_POINT ( 'NONE',  ( 0.5817216825391126056, -20.15223717566626860, -42.34527469533232846 ) ) ;
#36013 = CARTESIAN_POINT ( 'NONE',  ( 5.974727161628369032, 20.35137732084676188, -2.663664384318572331 ) ) ;
#36014 = CARTESIAN_POINT ( 'NONE',  ( 0.6067099128993250767, 28.59222530349279268, -38.42667919752372541 ) ) ;
#36015 = CARTESIAN_POINT ( 'NONE',  ( 0.9752132459055878888, 39.55248938404437098, -16.63533515462534851 ) ) ;
#36016 = EDGE_LOOP ( 'NONE', ( #31000, #31452, #40625, #8888 ) ) ;
#36017 = CARTESIAN_POINT ( 'NONE',  ( 4.962356264823609031, -33.29728444345293781, 25.73958909062332268 ) ) ;
#36018 = CARTESIAN_POINT ( 'NONE',  ( 0.5997462898726536595, -47.63132954987522538, -11.95023328037962251 ) ) ;
#36019 = EDGE_CURVE ( 'NONE', #36850, #10364, #39628, .T. ) ;
#36020 = B_SPLINE_CURVE_WITH_KNOTS ( 'NONE', 3,
 ( #47102, #12668, #31767, #3229, #41487, #4148 ),
 .UNSPECIFIED., .F., .F.,
 ( 4, 2, 4 ),
 ( 2.235140038340936352E-18, 0.0002447193893791689491, 0.0004894387787583368140 ),
 .UNSPECIFIED. ) ;
#36021 = DIRECTION ( 'NONE',  ( 0.000000000000000000, 0.000000000000000000, -1.000000000000000000 ) ) ;
#36022 = ORIENTED_EDGE ( 'NONE', *, *, #20584, .T. ) ;
#36023 = ADVANCED_FACE ( 'NONE', ( #13531 ), #38351, .F. ) ;
#36024 = CARTESIAN_POINT ( 'NONE',  ( 3.238931869106853600, 41.96286875554255147, 9.350562014686273571 ) ) ;
#36025 = ORIENTED_EDGE ( 'NONE', *, *, #25464, .T. ) ;
#36026 = ADVANCED_FACE ( 'NONE', ( #43913 ), #18767, .F. ) ;
#36027 = CARTESIAN_POINT ( 'NONE',  ( -6.010958268070873523, 4.863021950010902650, -18.20513189769803120 ) ) ;
#36028 = AXIS2_PLACEMENT_3D ( 'NONE', #56053, #23474, #47002 ) ;
#36029 = CARTESIAN_POINT ( 'NONE',  ( 0.1073791018717483448, 25.86618856530710531, -34.50606437925521419 ) ) ;
#36030 = ORIENTED_EDGE ( 'NONE', *, *, #61021, .T. ) ;
#36031 = CARTESIAN_POINT ( 'NONE',  ( 0.7246131072078574320, -46.66866179549023741, 11.65529928397556780 ) ) ;
#36032 = EDGE_CURVE ( 'NONE', #59028, #43795, #2753, .T. ) ;
#36033 = VERTEX_POINT ( 'NONE', #6238 ) ;
#36034 = CARTESIAN_POINT ( 'NONE',  ( 5.910764540655178756, -18.52235246776667310, -7.837327192926230701 ) ) ;
#36035 = CARTESIAN_POINT ( 'NONE',  ( 0.1081432562775998113, -25.91533557232866869, -34.46918062033742558 ) ) ;
#36036 = ORIENTED_EDGE ( 'NONE', *, *, #42077, .F. ) ;
#36037 = CARTESIAN_POINT ( 'NONE',  ( 2.528190830796658517, 40.79054845818019004, -9.918936063603915443 ) ) ;
#36038 = VERTEX_POINT ( 'NONE', #53260 ) ;
#36039 = CARTESIAN_POINT ( 'NONE',  ( -6.015611763856276717, -0.006214430185273883862, 18.84324252354755203 ) ) ;
#36040 = VERTEX_POINT ( 'NONE', #11290 ) ;
#36041 = EDGE_LOOP ( 'NONE', ( #30676, #46432 ) ) ;
#36042 = CARTESIAN_POINT ( 'NONE',  ( -6.016761891674565099, 13.32172022638591713, 13.32657647165359904 ) ) ;
#36043 = CARTESIAN_POINT ( 'NONE',  ( -2.739355103387247858, -6.282164585817087143, 13.54186010368304593 ) ) ;
#36044 = CARTESIAN_POINT ( 'NONE',  ( -0.2111111111111110827, -9.497654031326126400, -1.199999999999999956 ) ) ;
#36045 = CARTESIAN_POINT ( 'NONE',  ( 5.959547316686252039, -19.82530672674358385, -5.315863417546260905 ) ) ;
#36046 = DIRECTION ( 'NONE',  ( 0.000000000000000000, 0.000000000000000000, -1.000000000000000000 ) ) ;
#36047 = ORIENTED_EDGE ( 'NONE', *, *, #36899, .T. ) ;
#36048 = CARTESIAN_POINT ( 'NONE',  ( 3.221118495291109163, 6.099796721976346703, 43.56092170297041122 ) ) ;
#36049 = CARTESIAN_POINT ( 'NONE',  ( 5.960721111146673579, 19.82454228767745974, -5.318514366754729217 ) ) ;
#36050 = CARTESIAN_POINT ( 'NONE',  ( 0.000000000000000000, 0.000000000000000000, 0.000000000000000000 ) ) ;
#36051 = ORIENTED_EDGE ( 'NONE', *, *, #39033, .F. ) ;
#36052 = ORIENTED_EDGE ( 'NONE', *, *, #4404, .F. ) ;
#36053 = CARTESIAN_POINT ( 'NONE',  ( 0.9758171775293912331, 34.03798695362348781, -26.12572690811879284 ) ) ;
#36054 = DIRECTION ( 'NONE',  ( 0.07439287786467665975, -0.2708295585865200805, 0.9597484305373162883 ) ) ;
#36055 = CARTESIAN_POINT ( 'NONE',  ( 4.691466044806103852, -2.583163953528794021, 44.51344083442434396 ) ) ;
#36056 = VERTEX_POINT ( 'NONE', #15385 ) ;
#36057 = CARTESIAN_POINT ( 'NONE',  ( 0.1103744047535531458, -42.75042227379824311, -5.667281528142243729 ) ) ;
#36058 = CARTESIAN_POINT ( 'NONE',  ( 1.834102595619085507, -34.50568523712564684, 27.37800999295042814 ) ) ;
#36059 = B_SPLINE_CURVE_WITH_KNOTS ( 'NONE', 3,
 ( #31740, #59299, #41159, #22035, #54905, #50525 ),
 .UNSPECIFIED., .F., .F.,
 ( 4, 2, 4 ),
 ( 0.000000000000000000, 0.0002447195606305744208, 0.0004894391212611488417 ),
 .UNSPECIFIED. ) ;
#36060 = ORIENTED_EDGE ( 'NONE', *, *, #12102, .F. ) ;
#36061 = CARTESIAN_POINT ( 'NONE',  ( -6.016489644550737204, -14.94663725562907963, -11.47450955518503335 ) ) ;
#36062 = ORIENTED_EDGE ( 'NONE', *, *, #56434, .F. ) ;
#36063 = CARTESIAN_POINT ( 'NONE',  ( -4.000000000000000000, 2.309401076758496263, -0.3572655899081631503 ) ) ;
#36064 = CARTESIAN_POINT ( 'NONE',  ( 0.9752132459055842251, -33.89922943039196923, 26.30543738863332948 ) ) ;
#36065 = CARTESIAN_POINT ( 'NONE',  ( 5.860006189529246790, 47.30964106197871644, -9.393028332204265141 ) ) ;
#36066 = B_SPLINE_CURVE_WITH_KNOTS ( 'NONE', 3,
 ( #21275, #40113, #20969, #1842 ),
 .UNSPECIFIED., .F., .F.,
 ( 4, 4 ),
 ( 0.000000000000000000, 0.005013413432710138971 ),
 .UNSPECIFIED. ) ;
#36067 =( NAMED_UNIT ( * ) PLANE_ANGLE_UNIT ( ) SI_UNIT ( $, .RADIAN. ) );
#36068 = CARTESIAN_POINT ( 'NONE',  ( 7.000000000000021316, -80.00000000000001421, -2.649999999999999467 ) ) ;
#36069 = CLOSED_SHELL ( 'NONE', ( #3718, #36467, #16422, #61639, #60637, #18725, #276, #38210, #59742, #61306, #31020, #1033, #16578, #27016, #28801, #56631, #30988, #9182, #40826, #46307, #50832, #40090, #45262, #4261, #45165, #45914, #20749, #5065, #15367, #31909, #17905, #10633, #27160, #27554, #25837, #50435, #11381, #22558, #51888, #27065, #19896, #8520, #13035, #25959 ) ) ;
#36070 = EDGE_CURVE ( 'NONE', #59493, #30942, #44526, .T. ) ;
#36071 = ORIENTED_EDGE ( 'NONE', *, *, #49227, .F. ) ;
#36072 = CARTESIAN_POINT ( 'NONE',  ( 0.1119899015040013712, 20.90518409856474946, -38.85787675616901993 ) ) ;
#36073 = CARTESIAN_POINT ( 'NONE',  ( 0.9268187852002115479, -8.013537751244687257, -43.35363359186865040 ) ) ;
#36074 = DIRECTION ( 'NONE',  ( -1.000000000000000000, -0.000000000000000000, -0.000000000000000000 ) ) ;
#36075 = CONICAL_SURFACE ( 'NONE', #5032, 4.000000000000000000, 1.047197551196595855 ) ;
#36076 = CARTESIAN_POINT ( 'NONE',  ( 0.1084644655670282121, -16.86976209534753224, -39.68806829486941012 ) ) ;
#36077 = CARTESIAN_POINT ( 'NONE',  ( 0.6846871229502899947, -47.37786444808398301, 7.109010606687220957 ) ) ;
#36078 = CARTESIAN_POINT ( 'NONE',  ( 4.834790513006555379, 24.88720127704534235, 40.16486715427070209 ) ) ;
#36079 = CARTESIAN_POINT ( 'NONE',  ( 0.3676999524040366896, 43.13409918076302318, -9.241215893319285613 ) ) ;
#36080 = CARTESIAN_POINT ( 'NONE',  ( 0.5804410086790514622, -14.41595396256474615, 44.62846763227044988 ) ) ;
#36081 = DIRECTION ( 'NONE',  ( -1.000000000000000000, -0.000000000000000000, -0.000000000000000000 ) ) ;
#36082 = CARTESIAN_POINT ( 'NONE',  ( 1.399999999999998579, 0.000000000000000000, 0.000000000000000000 ) ) ;
#36083 = CARTESIAN_POINT ( 'NONE',  ( -6.079354080745853928, -11.01762705387090868, 15.79255677051609830 ) ) ;
#36084 = ORIENTED_EDGE ( 'NONE', *, *, #45813, .T. ) ;
#36085 = CARTESIAN_POINT ( 'NONE',  ( 1.112077966505211624, -2.461812912967866307, -44.01101910101717607 ) ) ;
#36086 = CARTESIAN_POINT ( 'NONE',  ( 3.376099380956842921, 0.01224625995926260230, 13.40552996569639710 ) ) ;
#36087 = CARTESIAN_POINT ( 'NONE',  ( 0.6067375320500690838, 44.51755737952380798, -17.67235760802216404 ) ) ;
#36088 = ORIENTED_EDGE ( 'NONE', *, *, #14479, .F. ) ;
#36089 = CARTESIAN_POINT ( 'NONE',  ( 1.227938101723756947, -42.65467462194914816, -4.762198645644879491 ) ) ;
#36090 = CARTESIAN_POINT ( 'NONE',  ( 0.6029443199889047422, 44.24423630359484605, -21.30692835126788509 ) ) ;
#36091 = ADVANCED_FACE ( 'NONE', ( #1556 ), #39680, .F. ) ;
#36092 =( NAMED_UNIT ( * ) PLANE_ANGLE_UNIT ( ) SI_UNIT ( $, .RADIAN. ) );
#36093 = ORIENTED_EDGE ( 'NONE', *, *, #54001, .F. ) ;
#36094 = CARTESIAN_POINT ( 'NONE',  ( 1.830465331921979022, 40.20755377393447105, -17.99246162687467532 ) ) ;
#36095 =( BOUNDED_SURFACE ( )  B_SPLINE_SURFACE ( 3, 1, ( 
 ( #37255, #46966 ),
 ( #28139, #27836 ),
 ( #13138, #41345 ),
 ( #9031, #55704 ) ),
 .UNSPECIFIED., .F., .F., .F. ) 
 B_SPLINE_SURFACE_WITH_KNOTS ( ( 4, 4 ),
 ( 2, 2 ),
 ( 0.000000000000000000, 1.000000000000000000 ),
 ( 0.000000000000000000, 1.000000000000000000 ),
 .UNSPECIFIED. ) 
 GEOMETRIC_REPRESENTATION_ITEM ( )  RATIONAL_B_SPLINE_SURFACE ( (
 ( 1.000000000000000000, 1.000000000000000000),
 ( 0.7211978278499968642, 0.9934217856018975334),
 ( 0.7211978278499968642, 0.9934217856018975334),
 ( 1.000000000000000000, 1.000000000000000000) ) ) 
 REPRESENTATION_ITEM ( '' )  SURFACE ( )  );
#36096 = CARTESIAN_POINT ( 'NONE',  ( 0.9757402383260943557, -41.42435672089860788, -11.18751708556354352 ) ) ;
#36097 = ADVANCED_FACE ( 'NONE', ( #49188 ), #25142, .F. ) ;
#36098 = ORIENTED_EDGE ( 'NONE', *, *, #51654, .F. ) ;
#36099 = CIRCLE ( 'NONE', #13059, 43.08621763946400307 ) ;
#36100 = CARTESIAN_POINT ( 'NONE',  ( 5.960721111146673579, 12.49016043756449434, 16.28787783074231399 ) ) ;
#36101 = ORIENTED_EDGE ( 'NONE', *, *, #32303, .F. ) ;
#36102 = EDGE_CURVE ( 'NONE', #20981, #23782, #34654, .T. ) ;
#36103 = ORIENTED_EDGE ( 'NONE', *, *, #59584, .F. ) ;
#36104 = CARTESIAN_POINT ( 'NONE',  ( 0.9736507210033064075, -6.046964561328232790, 42.48017254354721217 ) ) ;
#36105 = EDGE_LOOP ( 'NONE', ( #39175, #2315, #23900, #38335 ) ) ;
#36106 = CARTESIAN_POINT ( 'NONE',  ( 0.1365634738349418842, -13.16346314626551539, 42.11396273945445046 ) ) ;
#36107 = ORIENTED_EDGE ( 'NONE', *, *, #12697, .F. ) ;
#36108 = LINE ( 'NONE', #42045, #59720 ) ;
#36109 = CIRCLE ( 'NONE', #52073, 42.92674063221959813 ) ;
#36110 = CARTESIAN_POINT ( 'NONE',  ( 0.9749527285493309048, 16.15611883305644980, 39.75066842359289154 ) ) ;
#36111 = ORIENTED_EDGE ( 'NONE', *, *, #61228, .T. ) ;
#36112 = LINE ( 'NONE', #46737, #61445 ) ;
#36113 = EDGE_CURVE ( 'NONE', #26582, #6528, #15788, .T. ) ;
#36114 = B_SPLINE_CURVE_WITH_KNOTS ( 'NONE', 3,
 ( #52977, #8840, #13552, #32662, #27954, #47993 ),
 .UNSPECIFIED., .F., .F.,
 ( 4, 2, 4 ),
 ( 2.528804606065167438E-17, 0.0002293755540694318877, 0.0004587511081388384593 ),
 .UNSPECIFIED. ) ;
#36115 = CARTESIAN_POINT ( 'NONE',  ( 49.80929115161121956, 12.23419022400559442, -2.564334511966932517 ) ) ;
#36116 = CARTESIAN_POINT ( 'NONE',  ( 0.8557997880470690211, -46.50333260518550560, -11.51622788066506686 ) ) ;
#36117 = ORIENTED_EDGE ( 'NONE', *, *, #59880, .T. ) ;
#36118 = CARTESIAN_POINT ( 'NONE',  ( 9.999999999999994671, 58.44237546506807490, 54.69470952477956871 ) ) ;
#36119 = ADVANCED_FACE ( 'NONE', ( #20085 ), #36341, .F. ) ;
#36120 = ORIENTED_EDGE ( 'NONE', *, *, #50773, .F. ) ;
#36121 = CARTESIAN_POINT ( 'NONE',  ( 0.08486401232817714080, 12.80000000000000071, -3.000000000000000000 ) ) ;
#36122 = B_SPLINE_CURVE_WITH_KNOTS ( 'NONE', 3,
 ( #44559, #31053, #6907, #36393 ),
 .UNSPECIFIED., .F., .F.,
 ( 4, 4 ),
 ( 2.256078575551061230E-17, 0.004564976165746191181 ),
 .UNSPECIFIED. ) ;
#36123 = CARTESIAN_POINT ( 'NONE',  ( 4.958415959904820092, 1.012370948441083440, 45.41122172861450679 ) ) ;
#36124 = CARTESIAN_POINT ( 'NONE',  ( 0.5549461598389365813, 14.40543502832328926, -41.68574261197179709 ) ) ;
#36125 = ORIENTED_EDGE ( 'NONE', *, *, #26293, .F. ) ;
#36126 = CARTESIAN_POINT ( 'NONE',  ( 0.8557997880470690211, 33.22501220301949587, -34.51495345639514767 ) ) ;
#36127 = CARTESIAN_POINT ( 'NONE',  ( 4.967162193818130511, -32.68434214048149045, -28.07411493385329138 ) ) ;
#36128 = CARTESIAN_POINT ( 'NONE',  ( 4.553261556744875094, 7.233533384971297941, -43.32684572631779218 ) ) ;
#36129 = SURFACE_STYLE_USAGE ( .BOTH. , #22011 ) ;
#36130 = EDGE_LOOP ( 'NONE', ( #36036, #58021, #21286 ) ) ;
#36131 = ORIENTED_EDGE ( 'NONE', *, *, #39922, .F. ) ;
#36132 = CARTESIAN_POINT ( 'NONE',  ( 5.974727161628369032, -19.82156119440441699, -5.327229920347356540 ) ) ;
#36133 = CARTESIAN_POINT ( 'NONE',  ( 0.1101816497532063371, 34.29544870207477913, 26.14462713083307221 ) ) ;
#36134 = CARTESIAN_POINT ( 'NONE',  ( 0.9730545539215892381, -16.88610103448586131, 39.44597740938055352 ) ) ;
#36135 = CARTESIAN_POINT ( 'NONE',  ( 5.896782393890504181, -19.39988559968493576, 5.307591317834223332 ) ) ;
#36136 = EDGE_CURVE ( 'NONE', #19642, #57673, #59192, .T. ) ;
#36137 = CARTESIAN_POINT ( 'NONE',  ( 1.296416391601052487, -13.60092540267492467, -41.92042702868174331 ) ) ;
#36138 = CARTESIAN_POINT ( 'NONE',  ( 0.6845945791218034371, -30.94166671083587516, 35.25648567100093800 ) ) ;
#36139 = CARTESIAN_POINT ( 'NONE',  ( 0.6017667736363749853, 12.78803812527888262, -46.37677940471285609 ) ) ;
#36140 = CARTESIAN_POINT ( 'NONE',  ( 0.3676999524040323597, 43.44964275340426951, -7.620966337964178550 ) ) ;
#36141 = CARTESIAN_POINT ( 'NONE',  ( 0.1073791018717483448, 34.50606437925512182, 25.86618856530722610 ) ) ;
#36142 = CARTESIAN_POINT ( 'NONE',  ( 5.000000000000012434, -80.00000000000001421, -1.569632904675596344E-31 ) ) ;
#36143 = CARTESIAN_POINT ( 'NONE',  ( -6.057079549204054558, 5.487289185789611778, -18.45862639773758573 ) ) ;
#36144 = CARTESIAN_POINT ( 'NONE',  ( 1.112077966505211402, 41.49149550466378855, -14.88240994983740251 ) ) ;
#36145 = CARTESIAN_POINT ( 'NONE',  ( 0.7948884756798504370, 17.76850134148177318, -45.77094061386453916 ) ) ;
#36146 = DIRECTION ( 'NONE',  ( -1.000000000000000000, -0.000000000000000000, -0.000000000000000000 ) ) ;
#36147 = CARTESIAN_POINT ( 'NONE',  ( 0.9762797500689124330, -22.97506929404208975, 35.04955029839425151 ) ) ;
#36148 = CIRCLE ( 'NONE', #38171, 16.00000000000000000 ) ;
#36149 = CARTESIAN_POINT ( 'NONE',  ( 0.1097557419366048670, -0.2231007852156707827, -43.12388302211984126 ) ) ;
#36150 = CARTESIAN_POINT ( 'NONE',  ( 0.5997462898726536595, 16.46871699354475993, 46.26373299606117229 ) ) ;
#36152 = ORIENTED_EDGE ( 'NONE', *, *, #4289, .T. ) ;
#36151 = CARTESIAN_POINT ( 'NONE',  ( -6.001507490154111224, -18.68469198366098283, 2.444174634178074790 ) ) ;
#36153 = ORIENTED_EDGE ( 'NONE', *, *, #6897, .F. ) ;
#36154 = CARTESIAN_POINT ( 'NONE',  ( 0.8557997880470606944, -46.50333260518566902, 11.51622788066442027 ) ) ;
#36155 = CARTESIAN_POINT ( 'NONE',  ( 2.706805983486679779, 2.574964235114478583, -43.93342318221557719 ) ) ;
#36156 = CARTESIAN_POINT ( 'NONE',  ( 1.227938101723756947, 30.94118573761312874, 29.74462687941236538 ) ) ;
#36157 = ORIENTED_EDGE ( 'NONE', *, *, #46922, .F. ) ;
#36158 = ORIENTED_EDGE ( 'NONE', *, *, #23975, .T. ) ;
#36159 = CARTESIAN_POINT ( 'NONE',  ( 0.6039202388192952409, -30.75412344224365313, 38.28508331123533992 ) ) ;
#36160 = CARTESIAN_POINT ( 'NONE',  ( 0.1103744047535531458, -37.36621271144552026, 21.52865142340072424 ) ) ;
#36161 =( BOUNDED_SURFACE ( )  B_SPLINE_SURFACE ( 3, 1, ( 
 ( #26326, #36065 ),
 ( #21632, #6026 ),
 ( #1040, #39601 ),
 ( #48977, #12559 ) ),
 .UNSPECIFIED., .F., .F., .F. ) 
 B_SPLINE_SURFACE_WITH_KNOTS ( ( 4, 4 ),
 ( 2, 2 ),
 ( 0.000000000000000000, 1.000000000000000000 ),
 ( 0.000000000000000000, 1.000000000000000000 ),
 .UNSPECIFIED. ) 
 GEOMETRIC_REPRESENTATION_ITEM ( )  RATIONAL_B_SPLINE_SURFACE ( (
 ( 1.000000000000000000, 1.000000000000000000),
 ( 0.7269869731126817891, 0.9931720237060910339),
 ( 0.7269869731126817891, 0.9931720237060910339),
 ( 1.000000000000000000, 1.000000000000000000) ) ) 
 REPRESENTATION_ITEM ( '' )  SURFACE ( )  );
#36162 = VERTEX_POINT ( 'NONE', #10370 ) ;
#36163 = EDGE_LOOP ( 'NONE', ( #54018, #48021, #1326, #28187 ) ) ;
#36164 = B_SPLINE_CURVE_WITH_KNOTS ( 'NONE', 3,
 ( #54447, #21270, #49773, #6833, #25974, #18122, #14052, #36941, #17504, #47553, #51000, #56929, #46953, #9321, #41629, #61616 ),
 .UNSPECIFIED., .F., .F.,
 ( 4, 3, 3, 3, 3, 4 ),
 ( 1.868480190406682863E-17, 0.0002612764279487719702, 0.0003919131003184807630, 0.0005225497727000651474, 0.0007837925190632448122, 0.001045051706266717602 ),
 .UNSPECIFIED. ) ;
#36165 = CARTESIAN_POINT ( 'NONE',  ( 0.5839879327111910934, 47.89596760851024015, -0.09083573661728495952 ) ) ;
#36166 = EDGE_CURVE ( 'NONE', #18232, #23007, #34488, .T. ) ;
#36167 = CARTESIAN_POINT ( 'NONE',  ( 0.8760168074887076939, -33.37827814204148780, 34.63873394077430135 ) ) ;
#36168 = EDGE_CURVE ( 'NONE', #55625, #32395, #56010, .T. ) ;
#36169 = ORIENTED_EDGE ( 'NONE', *, *, #51977, .T. ) ;
#36170 = CARTESIAN_POINT ( 'NONE',  ( 4.553261556744875094, 17.98701270972463817, -40.07501640179128799 ) ) ;
#36171 = B_SPLINE_CURVE_WITH_KNOTS ( 'NONE', 3,
 ( #28319, #38365, #19555, #99 ),
 .UNSPECIFIED., .F., .F.,
 ( 4, 4 ),
 ( 0.000000000000000000, 0.005013413432710145910 ),
 .UNSPECIFIED. ) ;
#36172 = CARTESIAN_POINT ( 'NONE',  ( -6.078457390727109555, 16.78028475769486505, -9.445451523785473924 ) ) ;
#36173 = EDGE_CURVE ( 'NONE', #47659, #45115, #5182, .T. ) ;
#36174 = CARTESIAN_POINT ( 'NONE',  ( 0.1087620492084205720, 21.24797679669908135, 37.52665900408526056 ) ) ;
#36175 = ORIENTED_EDGE ( 'NONE', *, *, #35510, .T. ) ;
#36176 = EDGE_LOOP ( 'NONE', ( #11693, #13503, #44150, #55404 ) ) ;
#36177 = CARTESIAN_POINT ( 'NONE',  ( -6.078457390727109555, 0.6215653986403898434, -19.24599094597939342 ) ) ;
#36178 = VERTEX_POINT ( 'NONE', #21615 ) ;
#36179 = CARTESIAN_POINT ( 'NONE',  ( 5.896782393890504181, 14.91246379622031526, -13.49609241241443947 ) ) ;
#36180 = CARTESIAN_POINT ( 'NONE',  ( -6.078726893082806448, 9.985094725776210822, 16.46486940689163703 ) ) ;
#36181 = CARTESIAN_POINT ( 'NONE',  ( 0.5806925824938502512, -46.82446035038566379, -2.586943222941716858 ) ) ;
#36182 = CARTESIAN_POINT ( 'NONE',  ( -6.078457390727109555, 15.43466132010190961, -11.51371968441379856 ) ) ;
#36183 = DIRECTION ( 'NONE',  ( 1.000000000000000000, 1.836909530733573776E-16, 0.000000000000000000 ) ) ;
#36184 = EDGE_CURVE ( 'NONE', #17426, #10554, #17851, .T. ) ;
#36185 = ORIENTED_EDGE ( 'NONE', *, *, #46483, .F. ) ;
#36186 = CARTESIAN_POINT ( 'NONE',  ( 4.975610109902397937, -22.11219452748616021, 43.62912170003406942 ) ) ;
#36187 = VECTOR ( 'NONE', #48004, 1000.000000000000114 ) ;
#36188 = DIRECTION ( 'NONE',  ( -1.000000000000000000, -1.836909530733580185E-16, 1.836909530733574022E-16 ) ) ;
#36189 = CIRCLE ( 'NONE', #45189, 48.91267123290010943 ) ;
#36190 = CARTESIAN_POINT ( 'NONE',  ( 0.1135584504625007096, -31.39461082923043023, -31.00532959051426829 ) ) ;
#36191 = CARTESIAN_POINT ( 'NONE',  ( 0.5980894510889457338, 47.60453381548693130, -6.974827154143607544 ) ) ;
#36192 = ORIENTED_EDGE ( 'NONE', *, *, #48810, .T. ) ;
#36193 = CARTESIAN_POINT ( 'NONE',  ( 0.1100053167205930632, 42.73174076921944220, -5.806749312984677225 ) ) ;
#36194 = CARTESIAN_POINT ( 'NONE',  ( -4.915099999999998914, 0.000000000000000000, 0.000000000000000000 ) ) ;
#36195 = CARTESIAN_POINT ( 'NONE',  ( 4.549368137175248350, 24.02461520945223228, 35.57418903283122802 ) ) ;
#36196 = CARTESIAN_POINT ( 'NONE',  ( 4.291220156522059348, 46.92833126662976184, -4.137719400244163737 ) ) ;
#36197 = ORIENTED_EDGE ( 'NONE', *, *, #25423, .T. ) ;
#36198 = CARTESIAN_POINT ( 'NONE',  ( 4.834790513006555379, 38.14091330549777581, 27.89014293880336481 ) ) ;
#36199 = CARTESIAN_POINT ( 'NONE',  ( 1.827119703190779765, -20.44859290426063936, 37.88337895042260328 ) ) ;
#36200 = CARTESIAN_POINT ( 'NONE',  ( 2.528100132419517365, -13.58805440665008923, -39.71924667052476110 ) ) ;
#36201 = CARTESIAN_POINT ( 'NONE',  ( 5.960221823109900008, -19.82761049839345446, 5.307149561567740648 ) ) ;
#36202 = CARTESIAN_POINT ( 'NONE',  ( 0.1064266379913943739, -34.55203636557793345, -25.80493164505191217 ) ) ;
#36203 = B_SPLINE_CURVE_WITH_KNOTS ( 'NONE', 3,
 ( #35953, #25914, #15905, #11839, #21833, #40656, #26522, #59722, #1774, #55016, #25289, #50324, #12146, #7084, #16515, #25598 ),
 .UNSPECIFIED., .F., .F.,
 ( 4, 3, 3, 3, 3, 4 ),
 ( 9.813676791237319219E-18, 0.0002732102107931888070, 0.0004098135523333875513, 0.0005464168938825055390, 0.0008195847345945404079, 0.001092771384553103747 ),
 .UNSPECIFIED. ) ;
#36204 = CARTESIAN_POINT ( 'NONE',  ( 0.6064515330803633697, 40.70784744179291437, 23.28530636888421057 ) ) ;
#36205 = CARTESIAN_POINT ( 'NONE',  ( 5.901764892641307547, 47.35677775444503368, 12.46302804922537177 ) ) ;
#36206 = CARTESIAN_POINT ( 'NONE',  ( 1.657374760986086493, -32.49590154289041521, -29.74738358523344672 ) ) ;
#36207 = CARTESIAN_POINT ( 'NONE',  ( 0.5839879327111926477, 38.05372318152053168, 29.08515285004899198 ) ) ;
#36208 = CARTESIAN_POINT ( 'NONE',  ( 3.660176727303408484, -47.34518114598553495, -8.130955556894974734 ) ) ;
#36209 = EDGE_LOOP ( 'NONE', ( #33161, #17437, #50307, #10297 ) ) ;
#36210 = ADVANCED_FACE ( 'NONE', ( #22239 ), #47128, .F. ) ;
#36211 = CARTESIAN_POINT ( 'NONE',  ( -17.69715666991890046, -12.32470354188516737, -2.086247415145098483 ) ) ;
#36212 = CARTESIAN_POINT ( 'NONE',  ( 0.8744876279028306332, 32.34273794994798834, -36.93639603806098393 ) ) ;
#36213 = CARTESIAN_POINT ( 'NONE',  ( 50.50000000000000000, 0.000000000000000000, 0.000000000000000000 ) ) ;
#36214 = CARTESIAN_POINT ( 'NONE',  ( 0.1145239942831223490, 44.05326557292652723, -2.501054390828159502 ) ) ;
#36215 = CARTESIAN_POINT ( 'NONE',  ( 0.5807400328401574052, 41.75144119563918821, -23.47602859900671035 ) ) ;
#36216 = DIRECTION ( 'NONE',  ( 0.000000000000000000, 1.224646799147331020E-16, 1.000000000000000000 ) ) ;
#36217 = EDGE_CURVE ( 'NONE', #16197, #22082, #12809, .T. ) ;
#36218 = APPLICATION_PROTOCOL_DEFINITION ( 'draft international standard', 'automotive_design', 1998, #54333 ) ;
#36219 = CARTESIAN_POINT ( 'NONE',  ( 0.6009453534118439633, -44.61081284455544704, 18.00606795643196989 ) ) ;
#36220 = CARTESIAN_POINT ( 'NONE',  ( 3.559346040607745287, 35.69064246342631463, -25.68284100503404588 ) ) ;
#36221 = B_SPLINE_CURVE_WITH_KNOTS ( 'NONE', 3,
 ( #61956, #34418, #43520, #4953, #19391, #53489 ),
 .UNSPECIFIED., .F., .F.,
 ( 4, 2, 4 ),
 ( 2.223916437056137064E-17, 0.0002293755540694324298, 0.0004587511081388426335 ),
 .UNSPECIFIED. ) ;
#36222 = EDGE_CURVE ( 'NONE', #22677, #21167, #58765, .T. ) ;
#36223 = CARTESIAN_POINT ( 'NONE',  ( 0.6000166863083106206, -42.53190469623940118, 24.55321902762372588 ) ) ;
#36225 = ORIENTED_EDGE ( 'NONE', *, *, #36924, .T. ) ;
#36224 = CARTESIAN_POINT ( 'NONE',  ( 4.967162193818130511, 38.44485641567099776, -19.45289607368781759 ) ) ;
#36226 = ORIENTED_EDGE ( 'NONE', *, *, #29476, .F. ) ;
#36227 = CARTESIAN_POINT ( 'NONE',  ( 2.009741617377216460, -19.07132956818588809, -39.69620216248254252 ) ) ;
#36228 = FACE_OUTER_BOUND ( 'NONE', #28399, .T. ) ;
#36229 = CARTESIAN_POINT ( 'NONE',  ( 4.975610109902397937, 38.85236532789286201, -29.71435874397630528 ) ) ;
#36230 = ORIENTED_EDGE ( 'NONE', *, *, #35781, .T. ) ;
#36231 = CARTESIAN_POINT ( 'NONE',  ( 5.958863334805807099, 5.313608583996244583, 19.82594244347354717 ) ) ;
#36232 = PLANE ( 'NONE',  #59182 ) ;
#36233 = DIRECTION ( 'NONE',  ( 1.000000000000000000, 1.836909530733573776E-16, 0.000000000000000000 ) ) ;
#36234 = AXIS2_PLACEMENT_3D ( 'NONE', #15651, #34755, #53821 ) ;
#36235 = ORIENTED_EDGE ( 'NONE', *, *, #60765, .T. ) ;
#36236 = ORIENTED_EDGE ( 'NONE', *, *, #8600, .F. ) ;
#36237 = DIRECTION ( 'NONE',  ( 1.000000000000000000, 0.000000000000000000, 0.000000000000000000 ) ) ;
#36238 = EDGE_CURVE ( 'NONE', #48578, #34855, #7397, .T. ) ;
#36239 = CARTESIAN_POINT ( 'NONE',  ( 0.1092355843206037486, -39.72582785521905890, -16.78033551728650608 ) ) ;
#36240 = CARTESIAN_POINT ( 'NONE',  ( 0.9787464366903569912, 32.99929854755155390, -25.83370450129101314 ) ) ;
#36241 = ORIENTED_EDGE ( 'NONE', *, *, #6561, .F. ) ;
#36242 = EDGE_CURVE ( 'NONE', #49531, #3017, #55724, .T. ) ;
#36243 = DIRECTION ( 'NONE',  ( 0.000000000000000000, 0.000000000000000000, 1.000000000000000000 ) ) ;
#36244 = ADVANCED_FACE ( 'NONE', ( #31013 ), #46765, .F. ) ;
#36245 = DIRECTION ( 'NONE',  ( -1.807003620809173399E-16, 1.000000000000000000, 0.000000000000000000 ) ) ;
#36246 = B_SPLINE_CURVE_WITH_KNOTS ( 'NONE', 3,
 ( #39519, #11000, #58569, #15699 ),
 .UNSPECIFIED., .F., .F.,
 ( 4, 4 ),
 ( 0.000000000000000000, 0.004042984057420972825 ),
 .UNSPECIFIED. ) ;
#36247 = ORIENTED_EDGE ( 'NONE', *, *, #48085, .T. ) ;
#36248 = CARTESIAN_POINT ( 'NONE',  ( 4.956653778116975495, -39.67974989265057673, 27.17045123668458828 ) ) ;
#36249 = DIRECTION ( 'NONE',  ( 0.000000000000000000, 0.000000000000000000, 1.000000000000000000 ) ) ;
#36250 = EDGE_LOOP ( 'NONE', ( #3167, #4712 ) ) ;
#36251 = CARTESIAN_POINT ( 'NONE',  ( 1.154321485836933503, 15.65787964449918235, -39.95809831208263319 ) ) ;
#36252 = LINE ( 'NONE', #12437, #43565 ) ;
#36253 = VERTEX_POINT ( 'NONE', #40437 ) ;
#36254 = CARTESIAN_POINT ( 'NONE',  ( 2.648799415243708655, -44.91402171431691670, 19.67862080369118161 ) ) ;
#36255 = CARTESIAN_POINT ( 'NONE',  ( 4.967162193818130511, -13.42934394584192148, 40.93989340068605998 ) ) ;
#36256 = CARTESIAN_POINT ( 'NONE',  ( 1.227938101723756947, 25.45152231597106507, -34.55893248994479450 ) ) ;
#36257 = CARTESIAN_POINT ( 'NONE',  ( 5.965394784446460541, -18.96850062921640401, 7.841344330024606180 ) ) ;
#36258 = ADVANCED_FACE ( 'NONE', ( #16613 ), #31556, .F. ) ;
#36259 = VERTEX_POINT ( 'NONE', #57560 ) ;
#36260 = FACE_OUTER_BOUND ( 'NONE', #52272, .T. ) ;
#36261 = CARTESIAN_POINT ( 'NONE',  ( 4.553261556744873317, -20.51767157960462384, -38.84024612145397981 ) ) ;
#36262 = ORIENTED_EDGE ( 'NONE', *, *, #38380, .F. ) ;
#36263 = CARTESIAN_POINT ( 'NONE',  ( 0.5804410086790514622, -19.24447200597919405, -42.76879877979365574 ) ) ;
#36264 = VERTEX_POINT ( 'NONE', #38206 ) ;
#36265 = DIRECTION ( 'NONE',  ( 0.000000000000000000, 0.000000000000000000, -1.000000000000000000 ) ) ;
#36266 = ORIENTED_EDGE ( 'NONE', *, *, #19067, .T. ) ;
#36267 = CARTESIAN_POINT ( 'NONE',  ( 1.088908134280554219, 26.73890361625913314, 33.56490895818176767 ) ) ;
#36268 = CARTESIAN_POINT ( 'NONE',  ( 0.6008122571543327295, -48.75817579134915292, -5.847635758595932209 ) ) ;
#36269 = CARTESIAN_POINT ( 'NONE',  ( 0.1098349054025746507, -26.42143025180014604, 34.08267426123914134 ) ) ;
#36270 = ORIENTED_EDGE ( 'NONE', *, *, #12959, .T. ) ;
#36271 = CARTESIAN_POINT ( 'NONE',  ( 0.1158403557922069033, -27.48134092720074051, -34.52124285171061047 ) ) ;
#36272 = CARTESIAN_POINT ( 'NONE',  ( 0.9754292589017204973, -0.8180784385973481898, 41.90057534883716528 ) ) ;
#36273 = CARTESIAN_POINT ( 'NONE',  ( 1.231276596079881047, 33.41651732065586344, -25.31033664684003170 ) ) ;
#36274 = VERTEX_POINT ( 'NONE', #57253 ) ;
#36275 = CIRCLE ( 'NONE', #15297, 13.50000000000000178 ) ;
#36276 = VERTEX_POINT ( 'NONE', #13778 ) ;
#36277 = VECTOR ( 'NONE', #36972, 1000.000000000000000 ) ;
#36278 = CARTESIAN_POINT ( 'NONE',  ( -2.601141883200662974, -14.91960803315171269, 0.4480218817239753903 ) ) ;
#36279 = CARTESIAN_POINT ( 'NONE',  ( 3.376099380956842921, -13.33697911751164256, 1.354020550481185969 ) ) ;
#36280 = CARTESIAN_POINT ( 'NONE',  ( 0.8751705887134553219, -44.08562551107095828, 19.22545746485582185 ) ) ;
#36281 = CARTESIAN_POINT ( 'NONE',  ( 0.1064266418746776799, 41.79703894102872397, -10.61815661559954904 ) ) ;
#36282 = CARTESIAN_POINT ( 'NONE',  ( 0.5807400328401574052, 46.40483864045162221, -11.87003418057194715 ) ) ;
#36283 = ORIENTED_EDGE ( 'NONE', *, *, #33760, .F. ) ;
#36284 = CARTESIAN_POINT ( 'NONE',  ( 0.1084644655670282398, 37.14658555883732305, -21.90577137312953582 ) ) ;
#36285 = DIRECTION ( 'NONE',  ( 1.000000000000000000, 0.000000000000000000, 0.000000000000000000 ) ) ;
#36286 = VERTEX_POINT ( 'NONE', #28774 ) ;
#36287 = B_SPLINE_CURVE_WITH_KNOTS ( 'NONE', 3,
 ( #55973, #41002, #12789, #12471, #8058, #22471 ),
 .UNSPECIFIED., .F., .F.,
 ( 4, 2, 4 ),
 ( 1.266823315017301927E-16, 0.0002450741128632358116, 0.0004901482257263448800 ),
 .UNSPECIFIED. ) ;
#36288 = ADVANCED_FACE ( 'NONE', ( #42906 ), #55783, .F. ) ;
#36289 = CARTESIAN_POINT ( 'NONE',  ( 0.9747592971366223491, -30.11108831501858418, 30.56898208368264136 ) ) ;
#36290 = DIRECTION ( 'NONE',  ( 0.000000000000000000, 0.000000000000000000, -1.000000000000000000 ) ) ;
#36291 = CARTESIAN_POINT ( 'NONE',  ( 4.956653778116970166, 45.35992544608529187, 15.97476558431900884 ) ) ;
#36292 = CARTESIAN_POINT ( 'NONE',  ( 0.5806925824938499181, 45.08220210717423271, 12.91578164539256335 ) ) ;
#36293 = CARTESIAN_POINT ( 'NONE',  ( 0.5980894510889448457, -47.78766676462080909, 5.583794302584446534 ) ) ;
#36294 = CARTESIAN_POINT ( 'NONE',  ( 4.999999999999982236, 85.00000000000001421, 1.040949779275250495E-14 ) ) ;
#36295 = FACE_OUTER_BOUND ( 'NONE', #19401, .T. ) ;
#36296 = EDGE_CURVE ( 'NONE', #2066, #8473, #13458, .T. ) ;
#36297 =( NAMED_UNIT ( * ) SI_UNIT ( $, .STERADIAN. ) SOLID_ANGLE_UNIT ( ) );
#36298 = CARTESIAN_POINT ( 'NONE',  ( 0.6009453534118439633, 37.89911869481691298, 29.63106322864197750 ) ) ;
#36299 = CARTESIAN_POINT ( 'NONE',  ( 5.901764892641307547, -10.85461099010599106, -47.75111399426351255 ) ) ;
#36300 = DIRECTION ( 'NONE',  ( 1.000000000000000000, 1.836909530733573776E-16, 0.000000000000000000 ) ) ;
#36301 = B_SPLINE_CURVE_WITH_KNOTS ( 'NONE', 3,
 ( #32838, #47234, #24032, #14041 ),
 .UNSPECIFIED., .F., .F.,
 ( 4, 4 ),
 ( 0.000000000000000000, 0.005013413432710142441 ),
 .UNSPECIFIED. ) ;
#36302 = EDGE_CURVE ( 'NONE', #29142, #40875, #15657, .T. ) ;
#36303 = CARTESIAN_POINT ( 'NONE',  ( 5.959547316686252039, 7.851524054666414010, -18.96456592444092593 ) ) ;
#36304 = ADVANCED_FACE ( 'NONE', ( #51646 ), #55509, .F. ) ;
#36305 = CARTESIAN_POINT ( 'NONE',  ( 10.00000000000002132, -85.00000000000001421, -1.925929944387237167E-31 ) ) ;
#36306 = EDGE_CURVE ( 'NONE', #40743, #42423, #35737, .T. ) ;
#36307 = CARTESIAN_POINT ( 'NONE',  ( 2.624215991343608501, 22.77108897942136423, 42.26352390376104751 ) ) ;
#36308 = SURFACE_SIDE_STYLE ('',( #16253 ) ) ;
#36309 = FACE_OUTER_BOUND ( 'NONE', #27857, .T. ) ;
#36310 = PRODUCT_DEFINITION_SHAPE ( 'NONE', 'NONE',  #61982 ) ;
#36311 = CARTESIAN_POINT ( 'NONE',  ( 0.7057020205115011047, 37.48480537461333739, 29.82342581815218807 ) ) ;
#36312 = LINE ( 'NONE', #25345, #57653 ) ;
#36313 = ADVANCED_FACE ( 'NONE', ( #4323 ), #44402, .F. ) ;
#36314 = VERTEX_POINT ( 'NONE', #46986 ) ;
#36315 = CARTESIAN_POINT ( 'NONE',  ( 0.1095718737110177865, 11.40943879390648696, -41.58781525899398446 ) ) ;
#36316 = EDGE_CURVE ( 'NONE', #22472, #45586, #11092, .T. ) ;
#36317 = CARTESIAN_POINT ( 'NONE',  ( -6.001507490154110336, 18.68469198366097217, 2.444174634178205796 ) ) ;
#36318 = CARTESIAN_POINT ( 'NONE',  ( 0.9747592971366239034, -26.37717450293403587, -33.84353661172428929 ) ) ;
#36319 = CARTESIAN_POINT ( 'NONE',  ( 4.958415959904818315, 40.30989464198789562, -20.93600601295462837 ) ) ;
#36320 = VERTEX_POINT ( 'NONE', #23160 ) ;
#36321 = CARTESIAN_POINT ( 'NONE',  ( 1.091591847532194182, -0.6204316382185598444, -41.90911661605549909 ) ) ;
#36322 = CARTESIAN_POINT ( 'NONE',  ( 0.8753041380234530822, -35.88662119133316963, -33.51550010581278372 ) ) ;
#36323 = B_SPLINE_CURVE_WITH_KNOTS ( 'NONE', 3,
 ( #12433, #7703, #53756, #10889 ),
 .UNSPECIFIED., .F., .F.,
 ( 4, 4 ),
 ( 7.152448122690996019E-18, 0.005014147105413695182 ),
 .UNSPECIFIED. ) ;
#36324 = CIRCLE ( 'NONE', #6254, 15.71999999999999709 ) ;
#36325 = B_SPLINE_CURVE_WITH_KNOTS ( 'NONE', 3,
 ( #50418, #7483, #26610, #45742, #161, #48720 ),
 .UNSPECIFIED., .F., .F.,
 ( 4, 2, 4 ),
 ( 7.372574772901430151E-18, 0.0002291472222819941824, 0.0004582944445639809922 ),
 .UNSPECIFIED. ) ;
#36326 = CARTESIAN_POINT ( 'NONE',  ( 4.956653778116981712, -42.88673967249145846, 21.75875759808692322 ) ) ;
#36327 = ORIENTED_EDGE ( 'NONE', *, *, #32212, .T. ) ;
#36328 = B_SPLINE_CURVE_WITH_KNOTS ( 'NONE', 3,
 ( #44646, #49624, #29593, #44962, #48706, #1999 ),
 .UNSPECIFIED., .F., .F.,
 ( 4, 2, 4 ),
 ( 1.223195814675714468E-16, 0.0002448718616795907653, 0.0004897437233590592326 ),
 .UNSPECIFIED. ) ;
#36329 = CARTESIAN_POINT ( 'NONE',  ( 4.549368137175248350, 42.06008734272383975, 8.582197505784577629 ) ) ;
#36330 = ORIENTED_EDGE ( 'NONE', *, *, #57282, .T. ) ;
#36331 = CARTESIAN_POINT ( 'NONE',  ( 14.84250595937556483, 5.000000000000012434, -2.300655493813809945E-30 ) ) ;
#36332 = CARTESIAN_POINT ( 'NONE',  ( 1.830465331921977912, -44.03239073142495386, -1.234755989461712389 ) ) ;
#36333 = ORIENTED_EDGE ( 'NONE', *, *, #53158, .F. ) ;
#36334 = CARTESIAN_POINT ( 'NONE',  ( 5.959547316686252039, -12.49803383497762255, 16.28190225198596863 ) ) ;
#36335 = ORIENTED_EDGE ( 'NONE', *, *, #35674, .T. ) ;
#36336 = CARTESIAN_POINT ( 'NONE',  ( 0.5806925824938499181, 42.95845041307745760, 18.80940989108190209 ) ) ;
#36337 = CARTESIAN_POINT ( 'NONE',  ( 0.1135584504625009039, 20.02520167614220981, 39.31848610978152436 ) ) ;
#36338 = ADVANCED_FACE ( 'NONE', ( #46670 ), #13107, .F. ) ;
#36339 = VERTEX_POINT ( 'NONE', #9050 ) ;
#36340 = DIRECTION ( 'NONE',  ( -0.07906939808003035641, -0.8264033190538698781, -0.5574994031781644876 ) ) ;
#36342 = ORIENTED_EDGE ( 'NONE', *, *, #17990, .T. ) ;
#36341 =( BOUNDED_SURFACE ( )  B_SPLINE_SURFACE ( 3, 1, ( 
 ( #58255, #44833 ),
 ( #35113, #48569 ),
 ( #6548, #15074 ),
 ( #16297, #25692 ) ),
 .UNSPECIFIED., .F., .F., .F. ) 
 B_SPLINE_SURFACE_WITH_KNOTS ( ( 4, 4 ),
 ( 2, 2 ),
 ( 0.000000000000000000, 1.000000000000000000 ),
 ( 0.000000000000000000, 1.000000000000000000 ),
 .UNSPECIFIED. ) 
 GEOMETRIC_REPRESENTATION_ITEM ( )  RATIONAL_B_SPLINE_SURFACE ( (
 ( 1.000000000000000000, 1.000000000000000000),
 ( 0.9953485035131437453, 0.8621029689291515030),
 ( 0.9953485035131437453, 0.8621029689291515030),
 ( 1.000000000000000000, 1.000000000000000000) ) ) 
 REPRESENTATION_ITEM ( '' )  SURFACE ( )  );
#36343 = FACE_OUTER_BOUND ( 'NONE', #8655, .T. ) ;
#36344 = EDGE_CURVE ( 'NONE', #478, #56169, #28156, .T. ) ;
#36345 = VECTOR ( 'NONE', #17652, 1000.000000000000114 ) ;
#36346 = ORIENTED_EDGE ( 'NONE', *, *, #21657, .T. ) ;
#36347 = ORIENTED_EDGE ( 'NONE', *, *, #43607, .F. ) ;
#36348 = DIRECTION ( 'NONE',  ( -1.000000000000000000, -0.000000000000000000, -0.000000000000000000 ) ) ;
#36349 = CARTESIAN_POINT ( 'NONE',  ( -6.077587904424778920, -16.13490349385135758, 10.51003856501172606 ) ) ;
#36350 = CARTESIAN_POINT ( 'NONE',  ( 2.281351352603296245, 44.80774876812585461, -17.13758816714702249 ) ) ;
#36351 = CARTESIAN_POINT ( 'NONE',  ( 0.5850706913938534814, 46.31100969101487408, 12.22095376872053230 ) ) ;
#36352 = DIRECTION ( 'NONE',  ( 1.000000000000000000, 0.000000000000000000, 0.000000000000000000 ) ) ;
#36353 = VERTEX_POINT ( 'NONE', #59117 ) ;
#36354 = CARTESIAN_POINT ( 'NONE',  ( 0.9741495583595177754, 10.72301204857656565, 41.54695848110000611 ) ) ;
#36355 = CARTESIAN_POINT ( 'NONE',  ( 0.6254087463353916743, 6.960754339421171721, 47.60024110474255110 ) ) ;
#36356 = CARTESIAN_POINT ( 'NONE',  ( 0.6016117650947688800, 46.49485840376616608, -15.80440433101590969 ) ) ;
#36357 = ORIENTED_EDGE ( 'NONE', *, *, #55929, .T. ) ;
#36358 = ORIENTED_EDGE ( 'NONE', *, *, #29175, .F. ) ;
#36359 =( BOUNDED_SURFACE ( )  B_SPLINE_SURFACE ( 3, 1, ( 
 ( #45467, #2513 ),
 ( #50448, #44854 ),
 ( #59213, #30400 ),
 ( #31346, #40778 ) ),
 .UNSPECIFIED., .F., .F., .F. ) 
 B_SPLINE_SURFACE_WITH_KNOTS ( ( 4, 4 ),
 ( 2, 2 ),
 ( 0.000000000000000000, 1.000000000000000000 ),
 ( 0.000000000000000000, 1.000000000000000000 ),
 .UNSPECIFIED. ) 
 GEOMETRIC_REPRESENTATION_ITEM ( )  RATIONAL_B_SPLINE_SURFACE ( (
 ( 1.000000000000000000, 1.000000000000000000),
 ( 0.7211978278499970862, 0.9934217856018976445),
 ( 0.7211978278499970862, 0.9934217856018976445),
 ( 1.000000000000000000, 1.000000000000000000) ) ) 
 REPRESENTATION_ITEM ( '' )  SURFACE ( )  );
#36360 = CARTESIAN_POINT ( 'NONE',  ( 0.1097557419366048670, -21.75515245866099079, -37.23482781437637357 ) ) ;
#36361 = CARTESIAN_POINT ( 'NONE',  ( -6.063463321072278589, -8.893131869789531407, -17.08018319650008010 ) ) ;
#36362 = CARTESIAN_POINT ( 'NONE',  ( 0.5806925824938494740, 36.46274162637944016, -29.49052111156159128 ) ) ;
#36363 = ORIENTED_EDGE ( 'NONE', *, *, #9784, .T. ) ;
#36364 = CARTESIAN_POINT ( 'NONE',  ( 0.1084644655670283508, -42.80575641816244570, -5.234391617063844926 ) ) ;
#36365 = CARTESIAN_POINT ( 'NONE',  ( 0.9754292589017233839, 9.147692918817449836, -40.89800950117612643 ) ) ;
#36366 = ORIENTED_EDGE ( 'NONE', *, *, #56390, .T. ) ;
#36367 = EDGE_LOOP ( 'NONE', ( #238, #12528, #24757, #53069, #59107, #58611 ) ) ;
#36368 = DIRECTION ( 'NONE',  ( 0.07836865515943411409, 0.007886984708664454904, -0.9968932487286223942 ) ) ;
#36369 = CARTESIAN_POINT ( 'NONE',  ( 0.9757787079277446818, -34.06559579809986360, 26.08967489699748299 ) ) ;
#36370 = CARTESIAN_POINT ( 'NONE',  ( 0.8751705887134553219, -5.393078191593054349, 47.79200036674269825 ) ) ;
#36371 = AXIS2_PLACEMENT_3D ( 'NONE', #13403, #3051, #41303 ) ;
#36372 = ADVANCED_FACE ( 'NONE', ( #29389 ), #53136, .F. ) ;
#36373 = CARTESIAN_POINT ( 'NONE',  ( 0.2230388203127633140, 39.54016926433973111, -17.20066002792375670 ) ) ;
#36374 = APPLICATION_CONTEXT ( 'automotive_design' ) ;
#36375 = ORIENTED_EDGE ( 'NONE', *, *, #867, .T. ) ;
#36376 = CARTESIAN_POINT ( 'NONE',  ( 0.5782707292762423457, -44.06349990951380846, 16.06687055502393946 ) ) ;
#36377 = CARTESIAN_POINT ( 'NONE',  ( 2.528190830796658517, 16.21068873809912958, -38.72296097652494495 ) ) ;
#36378 = EDGE_CURVE ( 'NONE', #54442, #56211, #42503, .T. ) ;
#36379 = CARTESIAN_POINT ( 'NONE',  ( 1.227938101723748288, 36.73927144310511750, 22.18841447410732215 ) ) ;
#36380 = EDGE_CURVE ( 'NONE', #51524, #4311, #53654, .T. ) ;
#36381 = CARTESIAN_POINT ( 'NONE',  ( 4.549368137175248350, -19.17571786012351254, 38.40568845698243194 ) ) ;
#36382 = EDGE_CURVE ( 'NONE', #27771, #4535, #14102, .T. ) ;
#36383 = CARTESIAN_POINT ( 'NONE',  ( -2.708315649062916552, -14.47261168455371028, 2.171184472130447851 ) ) ;
#36384 = CARTESIAN_POINT ( 'NONE',  ( 0.5835226383429286123, 32.73248470276266175, 33.58313445361189764 ) ) ;
#36385 = CARTESIAN_POINT ( 'NONE',  ( 0.1129192098497447394, 43.21532672376840623, -8.909956450123800664 ) ) ;
#36386 = CARTESIAN_POINT ( 'NONE',  ( 0.6008123274975392114, -49.10565096348182124, -0.4354246331507586332 ) ) ;
#36387 = AXIS2_PLACEMENT_3D ( 'NONE', #57136, #32754, #32133 ) ;
#36388 = CARTESIAN_POINT ( 'NONE',  ( 0.2224561200757615154, -0.7594684977688249683, 43.11279565427788185 ) ) ;
#36389 = EDGE_CURVE ( 'NONE', #1853, #57497, #28789, .T. ) ;
#36390 = CARTESIAN_POINT ( 'NONE',  ( 5.896782393890504181, -19.39652907507971236, -5.319844614046497000 ) ) ;
#36391 = CARTESIAN_POINT ( 'NONE',  ( 0.5837374860065649429, -29.30115996485969276, -37.88763545422905565 ) ) ;
#36392 = VERTEX_POINT ( 'NONE', #6475 ) ;
#36393 = CARTESIAN_POINT ( 'NONE',  ( 4.549368137175248350, -40.71620287708334018, -13.59764261105737404 ) ) ;
#36394 = CARTESIAN_POINT ( 'NONE',  ( 0.8554163680231720024, 9.985124899324969050, -45.84215040611314862 ) ) ;
#36395 = DIRECTION ( 'NONE',  ( -0.07439287786467650709, -0.9903339163990665384, -0.1170659376278938568 ) ) ;
#36396 = ORIENTED_EDGE ( 'NONE', *, *, #55140, .F. ) ;
#36397 = CARTESIAN_POINT ( 'NONE',  ( 1.227938101723748288, -15.63977281655813023, -39.96870412324352628 ) ) ;
#36398 = CARTESIAN_POINT ( 'NONE',  ( 0.6016117650947688800, 44.09211389101648138, -21.62028091552307174 ) ) ;
#36399 = CARTESIAN_POINT ( 'NONE',  ( 0.7056313189692702270, -14.69870890607749025, -44.53870901195897858 ) ) ;
#36400 = ORIENTED_EDGE ( 'NONE', *, *, #12914, .F. ) ;
#36401 = DIRECTION ( 'NONE',  ( 0.000000000000000000, 0.000000000000000000, 1.000000000000000000 ) ) ;
#36402 = CARTESIAN_POINT ( 'NONE',  ( 0.9758171775293917882, -41.44794628856068641, -11.09981579996850520 ) ) ;
#36403 = CARTESIAN_POINT ( 'NONE',  ( 3.390910168358336918, -10.61186345626784977, 42.67886468170355840 ) ) ;
#36404 = EDGE_LOOP ( 'NONE', ( #13441, #16214, #8129, #21503 ) ) ;
#36405 = CARTESIAN_POINT ( 'NONE',  ( 0.6023143664670691511, 29.07782746490703474, 38.32505149877522399 ) ) ;
#36406 = EDGE_LOOP ( 'NONE', ( #58179, #42271, #52876, #11734 ) ) ;
#36407 = ORIENTED_EDGE ( 'NONE', *, *, #17192, .F. ) ;
#36408 = CARTESIAN_POINT ( 'NONE',  ( 0.1158816050234198897, 44.03387193347052886, 2.821376233662789001 ) ) ;
#36409 = VERTEX_POINT ( 'NONE', #1794 ) ;
#36410 = VECTOR ( 'NONE', #19049, 999.9999999999998863 ) ;
#36411 = VERTEX_POINT ( 'NONE', #35042 ) ;
#36412 = CARTESIAN_POINT ( 'NONE',  ( 1.231276596079887264, -37.02495017545888345, 19.65781868679367150 ) ) ;
#36413 = EDGE_CURVE ( 'NONE', #20940, #42745, #34118, .T. ) ;
#36414 = CARTESIAN_POINT ( 'NONE',  ( 2.528190830796654076, 8.550381731088631199, 41.09921055696414527 ) ) ;
#36415 = VERTEX_POINT ( 'NONE', #20923 ) ;
#36416 = CARTESIAN_POINT ( 'NONE',  ( 4.291220156522059348, 45.95810865397728406, -10.35573494518448356 ) ) ;
#36417 = CARTESIAN_POINT ( 'NONE',  ( 4.291220156522059348, -46.81214323738918637, -5.292659334196264886 ) ) ;
#36418 = CARTESIAN_POINT ( 'NONE',  ( 4.553261556744875094, -36.93702150832111641, 23.77385134801386712 ) ) ;
#36419 = ORIENTED_EDGE ( 'NONE', *, *, #7189, .T. ) ;
#36420 = PLANE ( 'NONE',  #42807 ) ;
#36421 = CIRCLE ( 'NONE', #37403, 2.649999999999992806 ) ;
#36422 = ORIENTED_EDGE ( 'NONE', *, *, #57953, .F. ) ;
#36423 = CARTESIAN_POINT ( 'NONE',  ( 0.9747592971366245695, -42.90728926179867386, 0.3237797888853479189 ) ) ;
#36424 = LINE ( 'NONE', #12930, #8466 ) ;
#36425 = CARTESIAN_POINT ( 'NONE',  ( 3.050102900204245682, 13.48218373028109340, -41.87667574009432769 ) ) ;
#36426 = EDGE_LOOP ( 'NONE', ( #54593, #54455, #59929, #54397 ) ) ;
#36427 = CARTESIAN_POINT ( 'NONE',  ( 0.5807400328401637335, -6.791881299635922353, 47.41494605191441281 ) ) ;
#36428 = LINE ( 'NONE', #961, #15304 ) ;
#36429 = CARTESIAN_POINT ( 'NONE',  ( 0.6000166863083106206, 48.30184070260992968, 8.874438937090559421 ) ) ;
#36430 = DIRECTION ( 'NONE',  ( -1.000000000000000000, -0.000000000000000000, -0.000000000000000000 ) ) ;
#36431 =( BOUNDED_SURFACE ( )  B_SPLINE_SURFACE ( 3, 1, ( 
 ( #36478, #55235 ),
 ( #31771, #36791 ),
 ( #12062, #31448 ),
 ( #32081, #49942 ) ),
 .UNSPECIFIED., .F., .F., .F. ) 
 B_SPLINE_SURFACE_WITH_KNOTS ( ( 4, 4 ),
 ( 2, 2 ),
 ( 0.000000000000000000, 1.000000000000000000 ),
 ( 0.000000000000000000, 1.000000000000000000 ),
 .UNSPECIFIED. ) 
 GEOMETRIC_REPRESENTATION_ITEM ( )  RATIONAL_B_SPLINE_SURFACE ( (
 ( 1.000000000000000000, 1.000000000000000000),
 ( 0.7269869731126817891, 0.9931720237060910339),
 ( 0.7269869731126817891, 0.9931720237060910339),
 ( 1.000000000000000000, 1.000000000000000000) ) ) 
 REPRESENTATION_ITEM ( '' )  SURFACE ( )  );
#36432 = EDGE_LOOP ( 'NONE', ( #30123, #16440, #11274, #37831 ) ) ;
#36433 = ORIENTED_EDGE ( 'NONE', *, *, #46996, .T. ) ;
#36434 = CARTESIAN_POINT ( 'NONE',  ( 4.956653778116966613, 0.000000000000000000, 0.000000000000000000 ) ) ;
#36435 = CARTESIAN_POINT ( 'NONE',  ( 0.5998501479064708430, 23.59887241503295741, 41.92175333043627461 ) ) ;
#36436 = CARTESIAN_POINT ( 'NONE',  ( 4.956445790444001354, -33.12351118015997997, 33.47194433010209025 ) ) ;
#36437 = FACE_OUTER_BOUND ( 'NONE', #13598, .T. ) ;
#36438 = B_SPLINE_CURVE_WITH_KNOTS ( 'NONE', 3,
 ( #23159, #29085, #239, #19389, #51957, #28773 ),
 .UNSPECIFIED., .F., .F.,
 ( 4, 2, 4 ),
 ( 1.512800854419661994E-16, 0.0002445252820015211956, 0.0004890505640028910365 ),
 .UNSPECIFIED. ) ;
#36439 = EDGE_CURVE ( 'NONE', #27464, #61276, #5060, .T. ) ;
#36440 = CARTESIAN_POINT ( 'NONE',  ( 4.390527457369402420, 12.19251145444202855, 42.20815088418253680 ) ) ;
#36441 = DIRECTION ( 'NONE',  ( -0.07836865515943411409, 0.7956898808744471419, 0.6006129930017412022 ) ) ;
#36442 = EDGE_CURVE ( 'NONE', #45486, #5687, #44152, .T. ) ;
#36443 = CARTESIAN_POINT ( 'NONE',  ( 0.5980271706414711508, 48.96187791475873752, 3.844964746512286258 ) ) ;
#36444 = EDGE_CURVE ( 'NONE', #37898, #24638, #44455, .T. ) ;
#36445 = EDGE_CURVE ( 'NONE', #38091, #6280, #39827, .T. ) ;
#36446 = LINE ( 'NONE', #55206, #37259 ) ;
#36447 = CARTESIAN_POINT ( 'NONE',  ( 0.9775691876210961251, 32.65442599162690840, 26.26827310934911353 ) ) ;
#36448 = CARTESIAN_POINT ( 'NONE',  ( -6.078726893082806448, 7.791390017580341443, -17.60932374802251132 ) ) ;
#36449 = CARTESIAN_POINT ( 'NONE',  ( 0.9972139404380304661, 29.87264297738568075, -30.80335716430286652 ) ) ;
#36450 = CIRCLE ( 'NONE', #33406, 2.649999999999985700 ) ;
#36451 = CARTESIAN_POINT ( 'NONE',  ( 0.6023142530420679819, -34.20176999054685041, -33.83147280953675562 ) ) ;
#36452 = FACE_OUTER_BOUND ( 'NONE', #50406, .T. ) ;
#36453 = CARTESIAN_POINT ( 'NONE',  ( 2.526464513654345545, 9.948146339971810193, -41.81190200959790104 ) ) ;
#36454 =( BOUNDED_SURFACE ( )  B_SPLINE_SURFACE ( 3, 1, ( 
 ( #20151, #16067 ),
 ( #39268, #58318 ),
 ( #29839, #6003 ),
 ( #58632, #11063 ) ),
 .UNSPECIFIED., .F., .F., .F. ) 
 B_SPLINE_SURFACE_WITH_KNOTS ( ( 4, 4 ),
 ( 2, 2 ),
 ( 0.000000000000000000, 1.000000000000000000 ),
 ( 0.000000000000000000, 1.000000000000000000 ),
 .UNSPECIFIED. ) 
 GEOMETRIC_REPRESENTATION_ITEM ( )  RATIONAL_B_SPLINE_SURFACE ( (
 ( 1.000000000000000000, 1.000000000000000000),
 ( 0.7269869731126821222, 0.9931720237060910339),
 ( 0.7269869731126821222, 0.9931720237060910339),
 ( 1.000000000000000000, 1.000000000000000000) ) ) 
 REPRESENTATION_ITEM ( '' )  SURFACE ( )  );
#36455 = CARTESIAN_POINT ( 'NONE',  ( 0.2885700199627512785, 43.10898996868493072, -0.8047882683534313131 ) ) ;
#36456 = CARTESIAN_POINT ( 'NONE',  ( 0.5800708057587382616, -44.00606528161371500, -18.90714313908705435 ) ) ;
#36457 = CARTESIAN_POINT ( 'NONE',  ( 4.553261556744875094, 0.000000000000000000, 0.000000000000000000 ) ) ;
#36459 = ORIENTED_EDGE ( 'NONE', *, *, #52982, .T. ) ;
#36458 = CARTESIAN_POINT ( 'NONE',  ( 0.5809828226811553087, -37.66417181417572380, 29.58751527316164953 ) ) ;
#36460 = EDGE_LOOP ( 'NONE', ( #55699, #58681, #33724, #4886 ) ) ;
#36461 = EDGE_CURVE ( 'NONE', #23179, #22826, #16225, .T. ) ;
#36462 = B_SPLINE_CURVE_WITH_KNOTS ( 'NONE', 3,
 ( #47915, #18173, #47001, #52587, #51662, #9680, #52902, #57574, #51973, #32583, #14710, #47599, #42604, #4642, #14101, #56977, #61666, #13476, #56358, #52274, #8756, #23174, #37288, #41996, #4964 ),
 .UNSPECIFIED., .F., .F.,
 ( 4, 3, 3, 3, 3, 3, 3, 3, 4 ),
 ( 4.670885906470169154E-18, 0.0005656085177311383390, 0.001131215744874499622, 0.001696821861372764832, 0.002262427090022497284, 0.002828031679238744624, 0.003393635864401603995, 0.003977030878808131623, 0.004561030005651157265 ),
 .UNSPECIFIED. ) ;
#36463 = FACE_OUTER_BOUND ( 'NONE', #42263, .T. ) ;
#36464 = CARTESIAN_POINT ( 'NONE',  ( 0.7954190325252782356, -48.09103420665682194, 0.8690070772087629125 ) ) ;
#36465 = DIRECTION ( 'NONE',  ( -1.000000000000000000, -0.000000000000000000, -0.000000000000000000 ) ) ;
#36466 = VERTEX_POINT ( 'NONE', #41284 ) ;
#36467 = ADVANCED_FACE ( 'NONE', ( #45992 ), #21773, .T. ) ;
#36468 = ORIENTED_EDGE ( 'NONE', *, *, #49696, .T. ) ;
#36469 = DIRECTION ( 'NONE',  ( 0.000000000000000000, 0.000000000000000000, -1.000000000000000000 ) ) ;
#36470 = AXIS2_PLACEMENT_3D ( 'NONE', #16770, #55569, #21457 ) ;
#36471 = CARTESIAN_POINT ( 'NONE',  ( 1.157644175074339588, -39.31880106288546273, -14.52701478131064938 ) ) ;
#36472 = ORIENTED_EDGE ( 'NONE', *, *, #16994, .F. ) ;
#36473 = ORIENTED_EDGE ( 'NONE', *, *, #27271, .T. ) ;
#36474 = CARTESIAN_POINT ( 'NONE',  ( 4.962356264823608143, 27.50309822711080443, -31.85616401533997077 ) ) ;
#36475 = CARTESIAN_POINT ( 'NONE',  ( 4.962356264823602814, -25.31392337492848554, -33.62202970123303203 ) ) ;
#36476 = CARTESIAN_POINT ( 'NONE',  ( 0.9740398440564311811, -41.33716823241940119, 11.50548031350427181 ) ) ;
#36477 = ORIENTED_EDGE ( 'NONE', *, *, #33831, .T. ) ;
#36478 = CARTESIAN_POINT ( 'NONE',  ( 5.981074661064941900, -20.34795181394747132, -2.687517936919926687 ) ) ;
#36479 = CARTESIAN_POINT ( 'NONE',  ( 0.3676999524040323597, 25.91024933382809436, -35.70167450949183774 ) ) ;
#36480 = VECTOR ( 'NONE', #31280, 999.9999999999998863 ) ;
#36481 = ADVANCED_FACE ( 'NONE', ( #31243 ), #10340, .F. ) ;
#36482 = CARTESIAN_POINT ( 'NONE',  ( 4.962356264823608143, 0.000000000000000000, 0.000000000000000000 ) ) ;
#36483 = ORIENTED_EDGE ( 'NONE', *, *, #53235, .F. ) ;
#36484 = B_SPLINE_CURVE_WITH_KNOTS ( 'NONE', 3,
 ( #13652, #18042, #18656, #28347 ),
 .UNSPECIFIED., .F., .F.,
 ( 4, 4 ),
 ( 0.000000000000000000, 0.004446090762761349506 ),
 .UNSPECIFIED. ) ;
#36485 = ORIENTED_EDGE ( 'NONE', *, *, #33850, .F. ) ;
#36486 = ORIENTED_EDGE ( 'NONE', *, *, #48667, .T. ) ;
#36487 = CARTESIAN_POINT ( 'NONE',  ( 0.6028777368367059797, -48.71531753957629007, 6.193356628624226978 ) ) ;
#36488 = CARTESIAN_POINT ( 'NONE',  ( 2.891212509700765487, 5.349982771599759140E-15, 41.99381090189422139 ) ) ;
#36489 = CARTESIAN_POINT ( 'NONE',  ( 0.5997462898726536595, -25.00873172704263325, 42.26245340191598387 ) ) ;
#36490 = CARTESIAN_POINT ( 'NONE',  ( 0.5848930533535030563, 4.512869149484262543, -46.67876491968475250 ) ) ;
#36491 = CARTESIAN_POINT ( 'NONE',  ( 0.5819845079324649229, 11.95724301473572204, -46.37938935563219189 ) ) ;
#36492 = ORIENTED_EDGE ( 'NONE', *, *, #50107, .F. ) ;
#36493 = DIRECTION ( 'NONE',  ( 0.000000000000000000, -1.287488025362403787E-15, -1.000000000000000000 ) ) ;
#36494 = CARTESIAN_POINT ( 'NONE',  ( 1.091591847532197734, 32.40455690483145190, 26.58389893821784256 ) ) ;
#36495 = CARTESIAN_POINT ( 'NONE',  ( 0.1084644655670281427, 39.68806829486948118, -16.86976209534739723 ) ) ;
#36496 = VECTOR ( 'NONE', #7243, 1000.000000000000000 ) ;
#36497 = ORIENTED_EDGE ( 'NONE', *, *, #52915, .F. ) ;
#36498 = PLANE ( 'NONE',  #19508 ) ;
#36499 = CARTESIAN_POINT ( 'NONE',  ( 0.1129192098497447394, 30.02178898772887550, 32.33641869102754640 ) ) ;
#36500 = CARTESIAN_POINT ( 'NONE',  ( 0.8560838555295158248, 9.983184696770717181, 45.83349056521764453 ) ) ;
#36501 = CARTESIAN_POINT ( 'NONE',  ( 0.5980894510889457338, 11.77356634613317787, -46.65000524237075297 ) ) ;
#36503 = VERTEX_POINT ( 'NONE', #17458 ) ;
#36502 = AXIS2_PLACEMENT_3D ( 'NONE', #18730, #38779, #14967 ) ;
#36504 = CARTESIAN_POINT ( 'NONE',  ( 1.092182651088187351, -13.16162218539093764, -39.79362870977350042 ) ) ;
#36505 = LINE ( 'NONE', #17386, #9689 ) ;
#36506 = CARTESIAN_POINT ( 'NONE',  ( -6.016104459813374383, -0.005335450885198452994, 18.84322058118302223 ) ) ;
#36507 = AXIS2_PLACEMENT_3D ( 'NONE', #61581, #43449, #23395 ) ;
#36508 = B_SPLINE_CURVE_WITH_KNOTS ( 'NONE', 3,
 ( #2025, #21156, #11773, #30852, #7027, #59659, #26158, #35887, #56506, #9514, #47137, #57112, #4481, #27708, #9211, #37130, #61504, #13941, #3879 ),
 .UNSPECIFIED., .F., .F.,
 ( 4, 3, 3, 3, 3, 3, 4 ),
 ( 1.153344816771540786E-16, 0.0002618519381806248326, 0.0003927759815485966800, 0.0005237000248299420206, 0.0006546240681324977167, 0.0007855481115631320586, 0.0009699050456655102914 ),
 .UNSPECIFIED. ) ;
#36509 = CARTESIAN_POINT ( 'NONE',  ( 0.7242003506639994592, -14.75411309231543022, -46.83297792138777993 ) ) ;
#36510 = FACE_OUTER_BOUND ( 'NONE', #40083, .T. ) ;
#36511 = CARTESIAN_POINT ( 'NONE',  ( 0.9757787079277449038, 42.90844198810271592, 0.03949005143916181626 ) ) ;
#36512 = DIRECTION ( 'NONE',  ( 0.000000000000000000, 0.000000000000000000, 1.000000000000000000 ) ) ;
#36513 = CARTESIAN_POINT ( 'NONE',  ( 4.291220156522060236, -5.703517857940846092, 46.76386298574836786 ) ) ;
#36514 = EDGE_CURVE ( 'NONE', #33861, #17001, #45069, .T. ) ;
#36515 = CARTESIAN_POINT ( 'NONE',  ( 5.910764540655177868, -18.52235246776677968, 7.837327192925977570 ) ) ;
#36516 = CARTESIAN_POINT ( 'NONE',  ( 4.833616638992208614, -38.70560126501845843, -25.31740731790884524 ) ) ;
#36517 = ORIENTED_EDGE ( 'NONE', *, *, #7132, .T. ) ;
#36518 = EDGE_CURVE ( 'NONE', #817, #12427, #45369, .T. ) ;
#36519 = CARTESIAN_POINT ( 'NONE',  ( 0.6041374136657476912, -6.106202762793827787, 47.71861871402578714 ) ) ;
#36520 = CARTESIAN_POINT ( 'NONE',  ( 0.7764139734771270396, -25.98546517425588931, 39.04863724362736122 ) ) ;
#36521 = CARTESIAN_POINT ( 'NONE',  ( 0.7762783648524380631, -0.8897020150994838783, -47.89627393592492410 ) ) ;
#36522 = CARTESIAN_POINT ( 'NONE',  ( 1.830465331921977246, 11.00192678874612895, -42.65364770817919293 ) ) ;
#36523 = B_SPLINE_CURVE_WITH_KNOTS ( 'NONE', 3,
 ( #49857, #17280, #3157, #6593, #45487, #26664 ),
 .UNSPECIFIED., .F., .F.,
 ( 4, 2, 4 ),
 ( 5.553824967135426632E-18, 0.0002447193893791698707, 0.0004894387787583342119 ),
 .UNSPECIFIED. ) ;
#36524 = CARTESIAN_POINT ( 'NONE',  ( -6.015611763856276717, 0.006214430185405465240, -18.84324252354755203 ) ) ;
#36525 = CARTESIAN_POINT ( 'NONE',  ( 5.959828726073459926, 20.34941966491239285, -2.683617577144171928 ) ) ;
#36526 = PRODUCT_CONTEXT ( 'NONE', #39569, 'mechanical' ) ;
#36527 = CARTESIAN_POINT ( 'NONE',  ( 0.6252788684277219566, -2.260168747266527500, -49.05441843919412293 ) ) ;
#36528 =( BOUNDED_SURFACE ( )  B_SPLINE_SURFACE ( 3, 1, ( 
 ( #16554, #59135 ),
 ( #16245, #30328 ),
 ( #49748, #45691 ),
 ( #41305, #25950 ) ),
 .UNSPECIFIED., .F., .F., .F. ) 
 B_SPLINE_SURFACE_WITH_KNOTS ( ( 4, 4 ),
 ( 2, 2 ),
 ( 0.000000000000000000, 1.000000000000000000 ),
 ( 0.000000000000000000, 1.000000000000000000 ),
 .UNSPECIFIED. ) 
 GEOMETRIC_REPRESENTATION_ITEM ( )  RATIONAL_B_SPLINE_SURFACE ( (
 ( 1.000000000000000000, 1.000000000000000000),
 ( 0.9953390228620291325, 0.8624445117761032620),
 ( 0.9953390228620291325, 0.8624445117761032620),
 ( 1.000000000000000000, 1.000000000000000000) ) ) 
 REPRESENTATION_ITEM ( '' )  SURFACE ( )  );
#36529 = AXIS2_PLACEMENT_3D ( 'NONE', #36540, #55298, #12121 ) ;
#36530 = CARTESIAN_POINT ( 'NONE',  ( 1.112077966505211624, 36.35951895807152567, -24.92018672213736963 ) ) ;
#36531 = CARTESIAN_POINT ( 'NONE',  ( 0.6016117650947689910, -1.225764908963027366, 49.09224536148712303 ) ) ;
#36533 = ORIENTED_EDGE ( 'NONE', *, *, #56564, .F. ) ;
#36532 = CARTESIAN_POINT ( 'NONE',  ( 0.5809828226811617480, -46.11980934799329646, -12.92184523170252497 ) ) ;
#36534 = VERTEX_POINT ( 'NONE', #31552 ) ;
#36535 = CARTESIAN_POINT ( 'NONE',  ( 0.7948884756798489937, 27.37439991543159223, 40.75954948070661743 ) ) ;
#36536 = CARTESIAN_POINT ( 'NONE',  ( -6.010958268070873523, 7.224487401384299012, 17.40352239307059534 ) ) ;
#36537 = CARTESIAN_POINT ( 'NONE',  ( 3.783198216974389627, 41.09147814699341694, 12.79806054635149160 ) ) ;
#36538 = EDGE_CURVE ( 'NONE', #49383, #61119, #2857, .T. ) ;
#36539 = EDGE_LOOP ( 'NONE', ( #48652, #2550, #37029, #51317 ) ) ;
#36540 = CARTESIAN_POINT ( 'NONE',  ( -4.473699999999999122, 0.000000000000000000, 0.000000000000000000 ) ) ;
#36541 = CARTESIAN_POINT ( 'NONE',  ( 0.7044674535453004927, -8.668117436800327980, -48.33907801057799247 ) ) ;
#36542 = CARTESIAN_POINT ( 'NONE',  ( 0.7246131072078538793, -29.92944207473678375, 37.65685186358339109 ) ) ;
#36543 = VERTEX_POINT ( 'NONE', #59741 ) ;
#36544 = ORIENTED_EDGE ( 'NONE', *, *, #51002, .F. ) ;
#36545 =( GEOMETRIC_REPRESENTATION_CONTEXT ( 3 ) GLOBAL_UNCERTAINTY_ASSIGNED_CONTEXT ( ( #46178 ) ) GLOBAL_UNIT_ASSIGNED_CONTEXT ( ( #18785, #57567, #13783 ) ) REPRESENTATION_CONTEXT ( 'NONE', 'WORKASPACE' ) );
#36546 = CARTESIAN_POINT ( 'NONE',  ( 0.9756354156337477823, 41.41248945940456849, 11.23134828980288624 ) ) ;
#36548 = CARTESIAN_POINT ( 'NONE',  ( 21.00000000000000355, 0.000000000000000000, 2.055000000000000160 ) ) ;
#36547 = CIRCLE ( 'NONE', #15571, 2.649999999999992806 ) ;
#36549 = CARTESIAN_POINT ( 'NONE',  ( 0.9762797500689124330, 33.20096159360354449, -25.57383300261748360 ) ) ;
#36550 = ORIENTED_EDGE ( 'NONE', *, *, #37941, .T. ) ;
#36552 = FACE_OUTER_BOUND ( 'NONE', #43737, .T. ) ;
#36551 = CIRCLE ( 'NONE', #38569, 2.649999999999999467 ) ;
#36553 = CARTESIAN_POINT ( 'NONE',  ( 0.5987334308729319599, 48.08272117021891034, -9.980722991683057543 ) ) ;
#36554 = EDGE_CURVE ( 'NONE', #25968, #17303, #39515, .T. ) ;
#36555 = CARTESIAN_POINT ( 'NONE',  ( 0.1368894036331295694, 33.18070637688693836, -29.08439530494225167 ) ) ;
#36556 = CARTESIAN_POINT ( 'NONE',  ( 0.1310142868023682905, 11.77532653407838836, -41.48473022063170390 ) ) ;
#36557 = ORIENTED_EDGE ( 'NONE', *, *, #7051, .T. ) ;
#36558 = CARTESIAN_POINT ( 'NONE',  ( -6.078457390727109555, -4.289140445936591384, 18.77226105914092713 ) ) ;
#36559 = LINE ( 'NONE', #3011, #12576 ) ;
#36560 = VERTEX_POINT ( 'NONE', #54722 ) ;
#36561 = CARTESIAN_POINT ( 'NONE',  ( 4.335381028904216727, -44.56680861641540048, 20.33608658056285279 ) ) ;
#36562 = CARTESIAN_POINT ( 'NONE',  ( -6.078075953587585900, -17.34679059108030685, -8.359666885489142274 ) ) ;
#36563 = CARTESIAN_POINT ( 'NONE',  ( 0.9787464366903567692, 4.370983831000746278, -41.68007309542044680 ) ) ;
#36564 = ORIENTED_EDGE ( 'NONE', *, *, #33329, .T. ) ;
#36566 = EDGE_CURVE ( 'NONE', #5033, #44660, #35970, .T. ) ;
#36565 = ORIENTED_EDGE ( 'NONE', *, *, #6086, .T. ) ;
#36567 = CYLINDRICAL_SURFACE ( 'NONE', #14763, 2.500000000000000444 ) ;
#36568 = CARTESIAN_POINT ( 'NONE',  ( 0.5819845079324652559, 41.70428776698897622, 23.55367910461011505 ) ) ;
#36569 = ORIENTED_EDGE ( 'NONE', *, *, #38914, .T. ) ;
#36570 = CARTESIAN_POINT ( 'NONE',  ( 0.9722240750034599754, -15.88116978453009409, 39.86121765932393401 ) ) ;
#36571 = ORIENTED_EDGE ( 'NONE', *, *, #43299, .F. ) ;
#36572 = EDGE_CURVE ( 'NONE', #36573, #3024, #45662, .T. ) ;
#36573 = VERTEX_POINT ( 'NONE', #11858 ) ;
#36574 = CARTESIAN_POINT ( 'NONE',  ( 0.6254087463353902310, 44.17672642933501237, -19.04342133627998379 ) ) ;
#36575 = CARTESIAN_POINT ( 'NONE',  ( 4.975801465491695552, 0.000000000000000000, 0.000000000000000000 ) ) ;
#36576 = ORIENTED_EDGE ( 'NONE', *, *, #35083, .T. ) ;
#36577 = CARTESIAN_POINT ( 'NONE',  ( 0.1129192098497447394, -27.88830454350447852, -34.19348267541494124 ) ) ;
#36578 = CARTESIAN_POINT ( 'NONE',  ( 5.960721111146673579, -20.52557019979492026, 0.006321279846751705171 ) ) ;
#36579 = CARTESIAN_POINT ( 'NONE',  ( 0.5835871038041849923, -41.91697779741947016, 21.02858590662108895 ) ) ;
#36580 = ORIENTED_EDGE ( 'NONE', *, *, #32433, .F. ) ;
#36581 = DIRECTION ( 'NONE',  ( -1.000000000000000000, -0.000000000000000000, -0.000000000000000000 ) ) ;
#36582 = FACE_OUTER_BOUND ( 'NONE', #18529, .T. ) ;
#36583 = CARTESIAN_POINT ( 'NONE',  ( 0.5997462898726536595, 32.62638226927682439, 36.70246327105753892 ) ) ;
#36584 = CARTESIAN_POINT ( 'NONE',  ( 0.5998501479064708430, 47.76154736470757456, -5.759754759340284913 ) ) ;
#36586 = CONICAL_SURFACE ( 'NONE', #44594, 43.92652462719577500, 1.486293639869522343 ) ;
#36585 = CARTESIAN_POINT ( 'NONE',  ( 4.549368137175248350, -42.84816078363928682, -2.596185425821792236 ) ) ;
#36587 = ORIENTED_EDGE ( 'NONE', *, *, #12252, .F. ) ;
#36588 = EDGE_CURVE ( 'NONE', #29999, #58167, #20651, .T. ) ;
#36589 = CARTESIAN_POINT ( 'NONE',  ( 1.827119703190779765, 12.32825544177779165, 41.24693285842933221 ) ) ;
#36590 = CYLINDRICAL_SURFACE ( 'NONE', #7823, 9.500000000000005329 ) ;
#36591 = ORIENTED_EDGE ( 'NONE', *, *, #44294, .T. ) ;
#36592 = AXIS2_PLACEMENT_3D ( 'NONE', #33004, #52077, #47395 ) ;
#36593 = EDGE_CURVE ( 'NONE', #45511, #13813, #22464, .T. ) ;
#36594 = DIRECTION ( 'NONE',  ( 1.000000000000000000, 0.000000000000000000, 0.000000000000000000 ) ) ;
#36595 = CARTESIAN_POINT ( 'NONE',  ( 1.227938101723748288, -29.74462687941204209, -30.94118573761343782 ) ) ;
#36596 = CARTESIAN_POINT ( 'NONE',  ( 5.896782393890504181, 16.57826022845101122, -11.38803647148056797 ) ) ;
#36597 = AXIS2_PLACEMENT_3D ( 'NONE', #12623, #13230, #51410 ) ;
#36598 = CARTESIAN_POINT ( 'NONE',  ( 0.9752570700956786354, 5.829291291129283792, -42.51066151201238341 ) ) ;
#36599 = B_SPLINE_CURVE_WITH_KNOTS ( 'NONE', 3,
 ( #37840, #56891, #41595, #41913 ),
 .UNSPECIFIED., .F., .F.,
 ( 4, 4 ),
 ( 2.091695478256946045E-17, 0.004444306975806114161 ),
 .UNSPECIFIED. ) ;
#36600 = CARTESIAN_POINT ( 'NONE',  ( 5.960721111146673579, -12.50019045452750355, 16.28018152803671370 ) ) ;
#36601 = CARTESIAN_POINT ( 'NONE',  ( 5.901463166500146684, 17.95741941801098207, 9.058087998373544281 ) ) ;
#36602 = CARTESIAN_POINT ( 'NONE',  ( 2.282816707992308736, 6.007215363275087761, 46.58766285173788191 ) ) ;
#36603 = ADVANCED_FACE ( 'NONE', ( #16533 ), #40742, .F. ) ;
#36604 =( NAMED_UNIT ( * ) PLANE_ANGLE_UNIT ( ) SI_UNIT ( $, .RADIAN. ) );
#36605 = CARTESIAN_POINT ( 'NONE',  ( 0.1158403557922069033, -12.51823201008644659, -42.31115898348171811 ) ) ;
#36606 = CARTESIAN_POINT ( 'NONE',  ( 5.958863334805807099, 14.51469124124459675, 14.51296551801808121 ) ) ;
#36607 = DIRECTION ( 'NONE',  ( 0.000000000000000000, 0.000000000000000000, 1.000000000000000000 ) ) ;
#36608 =( BOUNDED_SURFACE ( )  B_SPLINE_SURFACE ( 3, 1, ( 
 ( #2617, #26127 ),
 ( #49939, #35238 ),
 ( #1996, #26428 ),
 ( #6994, #44641 ) ),
 .UNSPECIFIED., .F., .F., .F. ) 
 B_SPLINE_SURFACE_WITH_KNOTS ( ( 4, 4 ),
 ( 2, 2 ),
 ( 0.000000000000000000, 1.000000000000000000 ),
 ( 0.000000000000000000, 1.000000000000000000 ),
 .UNSPECIFIED. ) 
 GEOMETRIC_REPRESENTATION_ITEM ( )  RATIONAL_B_SPLINE_SURFACE ( (
 ( 1.000000000000000000, 1.000000000000000000),
 ( 0.9953040768229005630, 0.8617119497784937465),
 ( 0.9953040768229005630, 0.8617119497784937465),
 ( 1.000000000000000000, 1.000000000000000000) ) ) 
 REPRESENTATION_ITEM ( '' )  SURFACE ( )  );
#36609 = CARTESIAN_POINT ( 'NONE',  ( 0.1073791018717483448, -40.02496097243048467, -16.05399293000801819 ) ) ;
#36610 = CARTESIAN_POINT ( 'NONE',  ( -6.063463321072276813, -18.28058862190277267, -6.053142334046738071 ) ) ;
#36611 = CARTESIAN_POINT ( 'NONE',  ( 0.6845945791218034371, -41.46895371680775355, -21.92561055813956372 ) ) ;
#36612 = CARTESIAN_POINT ( 'NONE',  ( 2.281448460670310929, 1.314143534315831419, 47.95523685111403012 ) ) ;
#36613 = CARTESIAN_POINT ( 'NONE',  ( 3.894904216938897878, 17.24901631294985904, 40.43013441372400507 ) ) ;
#36614 = ADVANCED_FACE ( 'NONE', ( #35659 ), #1905, .F. ) ;
#36615 = DIRECTION ( 'NONE',  ( -1.000000000000000000, -0.000000000000000000, -0.000000000000000000 ) ) ;
#36616 = CARTESIAN_POINT ( 'NONE',  ( 4.962356264823597485, -9.332162870646813602, 41.03835198954837438 ) ) ;
#36617 = ORIENTED_EDGE ( 'NONE', *, *, #29983, .F. ) ;
#36618 = CARTESIAN_POINT ( 'NONE',  ( 0.8560838555295223751, 33.26091945577352504, 33.07694168205818386 ) ) ;
#36619 = DIRECTION ( 'NONE',  ( 0.07836865515943411409, -0.6006129930017385377, -0.7956898808744492513 ) ) ;
#36620 = CARTESIAN_POINT ( 'NONE',  ( 0.9754642270333685472, -39.57465882553916003, -16.58255499746116968 ) ) ;
#36621 = CARTESIAN_POINT ( 'NONE',  ( 0.5782707292762423457, -25.84399470232749252, -39.13852694639499674 ) ) ;
#36622 = EDGE_LOOP ( 'NONE', ( #10750, #59955, #17173, #27993 ) ) ;
#36623 = LINE ( 'NONE', #18125, #2922 ) ;
#36624 = CARTESIAN_POINT ( 'NONE',  ( 0.6009453534118439633, 24.43073772334918203, -41.44251633523867184 ) ) ;
#36625 = ORIENTED_EDGE ( 'NONE', *, *, #37883, .F. ) ;
#36626 = CARTESIAN_POINT ( 'NONE',  ( 4.975610109902397937, 35.53430708602585497, -33.61193875773584949 ) ) ;
#36627 = ORIENTED_EDGE ( 'NONE', *, *, #45845, .T. ) ;
#36628 = EDGE_CURVE ( 'NONE', #37468, #12657, #32728, .T. ) ;
#36629 = CARTESIAN_POINT ( 'NONE',  ( -6.015611763856276717, -11.46610900684713030, -14.95313250337441424 ) ) ;
#36630 = CARTESIAN_POINT ( 'NONE',  ( 4.960156602257182357, 38.88108289790896066, -25.36362146861343803 ) ) ;
#36631 = VECTOR ( 'NONE', #44722, 1000.000000000000114 ) ;
#36632 = ORIENTED_EDGE ( 'NONE', *, *, #27235, .T. ) ;
#36633 = CARTESIAN_POINT ( 'NONE',  ( -6.057079549204054558, -1.857573237467230909, 19.16717644221975547 ) ) ;
#36634 = CARTESIAN_POINT ( 'NONE',  ( 0.1073791018717483448, 26.63563652260123149, 33.91564619577815165 ) ) ;
#36635 = VERTEX_POINT ( 'NONE', #13699 ) ;
#36636 = CARTESIAN_POINT ( 'NONE',  ( 0.9757402383260949108, 21.38067434779580012, 37.20221273948016005 ) ) ;
#36637 = CARTESIAN_POINT ( 'NONE',  ( 0.1157991065609915576, 20.33690428145512286, 39.15804757370611355 ) ) ;
#36638 = ADVANCED_FACE ( 'NONE', ( #42516 ), #44756, .F. ) ;
#36639 = AXIS2_PLACEMENT_3D ( 'NONE', #12334, #6647, #21713 ) ;
#36640 = EDGE_LOOP ( 'NONE', ( #42813, #25578, #36587, #54449 ) ) ;
#36641 = EDGE_CURVE ( 'NONE', #39264, #12159, #47828, .T. ) ;
#36642 = DIRECTION ( 'NONE',  ( 0.09722883295013595717, -0.2904161885395372678, -0.9519479983052239191 ) ) ;
#36643 = VERTEX_POINT ( 'NONE', #51564 ) ;
#36644 = CARTESIAN_POINT ( 'NONE',  ( 0.9762797500689124330, 28.76866969767982951, 30.47438972336447804 ) ) ;
#36645 = ORIENTED_EDGE ( 'NONE', *, *, #43706, .F. ) ;
#36646 = ADVANCED_FACE ( 'NONE', ( #19315 ), #16744, .F. ) ;
#36647 = ORIENTED_EDGE ( 'NONE', *, *, #2746, .F. ) ;
#36648 = CARTESIAN_POINT ( 'NONE',  ( 0.9756008150404597012, -0.1421465479999864390, -42.90824081423206593 ) ) ;
#36650 = AXIS2_PLACEMENT_3D ( 'NONE', #25717, #30717, #6257 ) ;
#36649 = CARTESIAN_POINT ( 'NONE',  ( 4.956653778116966613, 0.000000000000000000, 0.000000000000000000 ) ) ;
#36651 = CARTESIAN_POINT ( 'NONE',  ( 0.6029443449137436017, -25.41969901341494875, -42.01640679604484774 ) ) ;
#36652 = CARTESIAN_POINT ( 'NONE',  ( 0.5850706913938533704, 46.21698775168644602, 12.57184842332033980 ) ) ;
#36653 = CARTESIAN_POINT ( 'NONE',  ( 4.691466044806102076, -44.51344083442437238, 2.583163953528321066 ) ) ;
#36654 = VERTEX_POINT ( 'NONE', #51262 ) ;
#36655 = CARTESIAN_POINT ( 'NONE',  ( 4.549368137175248350, 0.000000000000000000, 0.000000000000000000 ) ) ;
#36656 = CARTESIAN_POINT ( 'NONE',  ( 0.9769922540276041456, -18.04061514536692812, 37.82681271615258822 ) ) ;
#36657 = CARTESIAN_POINT ( 'NONE',  ( 4.060580049360325461, 0.9058177295226151893, 43.93913049435652596 ) ) ;
#36658 = ORIENTED_EDGE ( 'NONE', *, *, #54295, .F. ) ;
#36659 = VERTEX_POINT ( 'NONE', #33115 ) ;
#36660 = CARTESIAN_POINT ( 'NONE',  ( 0.5987334308729320709, 11.51672212534787576, 47.73811912986572281 ) ) ;
#36661 = CARTESIAN_POINT ( 'NONE',  ( 4.549368137175248350, 19.17571786012269541, 38.40568845698284406 ) ) ;
#36662 = CARTESIAN_POINT ( 'NONE',  ( 0.1313383488274128541, -42.66669366003527841, 6.260443365526650261 ) ) ;
#36663 = ORIENTED_EDGE ( 'NONE', *, *, #33478, .T. ) ;
#36664 = DIRECTION ( 'NONE',  ( 0.000000000000000000, 0.000000000000000000, 1.000000000000000000 ) ) ;
#36665 = CARTESIAN_POINT ( 'NONE',  ( 4.060580049360325461, -33.78822741605884517, 28.10379658408981740 ) ) ;
#36666 = EDGE_CURVE ( 'NONE', #37717, #12846, #10311, .T. ) ;
#36667 = EDGE_LOOP ( 'NONE', ( #4735, #57572, #10062, #22823 ) ) ;
#36668 = CARTESIAN_POINT ( 'NONE',  ( 4.956653778116949738, 45.71126949320249366, 14.93973939759898606 ) ) ;
#36669 = VERTEX_POINT ( 'NONE', #4556 ) ;
#36670 = EDGE_CURVE ( 'NONE', #60330, #33022, #7276, .T. ) ;
#36671 = CARTESIAN_POINT ( 'NONE',  ( 2.648799415243696664, -21.10807549816198403, 44.26021477640490787 ) ) ;
#36672 = CARTESIAN_POINT ( 'NONE',  ( 0.7764146366350267447, -44.00885459193158766, 16.22532561076629065 ) ) ;
#36673 = DIRECTION ( 'NONE',  ( 1.000000000000000000, 0.000000000000000000, 0.000000000000000000 ) ) ;
#36674 = CARTESIAN_POINT ( 'NONE',  ( 2.533389852662419894, -43.42454841681725952, 7.194381594627227372 ) ) ;
#36675 = EDGE_CURVE ( 'NONE', #53786, #14355, #17658, .T. ) ;
#36676 = CARTESIAN_POINT ( 'NONE',  ( 3.270143674763207553, -13.14781761974166585, -3.806843787666058798 ) ) ;
#36677 = EDGE_LOOP ( 'NONE', ( #25185, #40673, #35123, #9495 ) ) ;
#36678 = LINE ( 'NONE', #55749, #2685 ) ;
#36679 = CARTESIAN_POINT ( 'NONE',  ( 5.960221823109900008, -16.28072933292556357, 12.49951306783062144 ) ) ;
#36680 = AXIS2_PLACEMENT_3D ( 'NONE', #43519, #58802, #15925 ) ;
#36681 = CARTESIAN_POINT ( 'NONE',  ( 5.959828726073459926, -2.674641840416323912, 20.35060134307029855 ) ) ;
#36682 = CARTESIAN_POINT ( 'NONE',  ( 0.1103878639767399278, 21.52017980327898528, -37.37111717125851840 ) ) ;
#36683 = CIRCLE ( 'NONE', #33632, 0.05882000000000109363 ) ;
#36684 = AXIS2_PLACEMENT_3D ( 'NONE', #7646, #58719, #40292 ) ;
#36685 = CARTESIAN_POINT ( 'NONE',  ( 0.5807400328401637335, -47.41494605191447675, 6.791881299635417868 ) ) ;
#36686 = CARTESIAN_POINT ( 'NONE',  ( 0.5830081025819924267, 32.79755092742119160, 33.51943745866657309 ) ) ;
#36687 = CARTESIAN_POINT ( 'NONE',  ( 2.528190830796654076, 32.18156550548854966, 26.95553705213378493 ) ) ;
#36688 = EDGE_CURVE ( 'NONE', #37892, #7602, #59661, .T. ) ;
#36689 = CARTESIAN_POINT ( 'NONE',  ( 0.7056313189692720034, -8.631130581270838320, -46.10045801124549314 ) ) ;
#36690 = B_SPLINE_CURVE_WITH_KNOTS ( 'NONE', 3,
 ( #59382, #16491, #12736, #35620 ),
 .UNSPECIFIED., .F., .F.,
 ( 4, 4 ),
 ( 2.175771182130668512E-17, 0.004559932413162188537 ),
 .UNSPECIFIED. ) ;
#36691 = CARTESIAN_POINT ( 'NONE',  ( 0.5804410086790514622, 17.36461428077188884, -43.56592731407664587 ) ) ;
#36692 = EDGE_CURVE ( 'NONE', #41039, #11235, #40809, .T. ) ;
#36693 = DIRECTION ( 'NONE',  ( 1.000000000000000000, 0.000000000000000000, 0.000000000000000000 ) ) ;
#36694 = CARTESIAN_POINT ( 'NONE',  ( 0.5839254288179548391, -29.08514953649795487, -38.05364096126348272 ) ) ;
#36695 = VECTOR ( 'NONE', #20959, 1000.000000000000000 ) ;
#36696 = ORIENTED_EDGE ( 'NONE', *, *, #30029, .F. ) ;
#36697 = DIRECTION ( 'NONE',  ( 1.000000000000000000, 0.000000000000000000, 0.000000000000000000 ) ) ;
#36698 = CARTESIAN_POINT ( 'NONE',  ( 0.5850706913938533704, -41.38834827854191190, -24.10530971368332231 ) ) ;
#36699 = CARTESIAN_POINT ( 'NONE',  ( -6.016489644550737204, 11.47450955518509552, -14.94663725562903878 ) ) ;
#36700 = CARTESIAN_POINT ( 'NONE',  ( 3.559346040607745287, -41.96528360729811169, 13.12803310862003769 ) ) ;
#36701 = ORIENTED_EDGE ( 'NONE', *, *, #14039, .F. ) ;
#36702 = B_SPLINE_CURVE_WITH_KNOTS ( 'NONE', 3,
 ( #8932, #37783, #28043, #47163 ),
 .UNSPECIFIED., .F., .F.,
 ( 4, 4 ),
 ( 0.000000000000000000, 0.004446090762761125727 ),
 .UNSPECIFIED. ) ;
#36703 = FACE_OUTER_BOUND ( 'NONE', #57340, .T. ) ;
#36704 = CARTESIAN_POINT ( 'NONE',  ( 0.9790320750461911636, -41.80925896709178602, -2.884960513567975227 ) ) ;
#36705 =( BOUNDED_SURFACE ( )  B_SPLINE_SURFACE ( 3, 1, ( 
 ( #24712, #61969 ),
 ( #48825, #28474 ),
 ( #48513, #38839 ),
 ( #33510, #10006 ) ),
 .UNSPECIFIED., .F., .F., .F. ) 
 B_SPLINE_SURFACE_WITH_KNOTS ( ( 4, 4 ),
 ( 2, 2 ),
 ( 0.000000000000000000, 1.000000000000000000 ),
 ( 0.000000000000000000, 1.000000000000000000 ),
 .UNSPECIFIED. ) 
 GEOMETRIC_REPRESENTATION_ITEM ( )  RATIONAL_B_SPLINE_SURFACE ( (
 ( 1.000000000000000000, 1.000000000000000000),
 ( 0.7211978278499968642, 0.9934217856018975334),
 ( 0.7211978278499968642, 0.9934217856018975334),
 ( 1.000000000000000000, 1.000000000000000000) ) ) 
 REPRESENTATION_ITEM ( '' )  SURFACE ( )  );
#36706 = ORIENTED_EDGE ( 'NONE', *, *, #37427, .T. ) ;
#36707 = CARTESIAN_POINT ( 'NONE',  ( 0.6000166863083106206, -49.10753961887881758, 0.5225268306041193078 ) ) ;
#36708 = CARTESIAN_POINT ( 'NONE',  ( 2.618530812446111078, 43.80811722902110716, -17.04627977144998141 ) ) ;
#36709 = CARTESIAN_POINT ( 'NONE',  ( 3.782542959838395280, 2.488391571546694436, 41.96481574823395988 ) ) ;
#36710 = ORIENTED_EDGE ( 'NONE', *, *, #44374, .T. ) ;
#36711 = CARTESIAN_POINT ( 'NONE',  ( 0.5998501479064708430, 46.33007877220720871, 12.95623334615518374 ) ) ;
#36712 = ORIENTED_EDGE ( 'NONE', *, *, #31804, .F. ) ;
#36713 = ORIENTED_EDGE ( 'NONE', *, *, #29709, .F. ) ;
#36714 = CARTESIAN_POINT ( 'NONE',  ( 2.528190830796658517, -16.56543340168992628, -38.57253624493965560 ) ) ;
#36715 = EDGE_CURVE ( 'NONE', #10852, #55528, #29015, .T. ) ;
#36716 = ORIENTED_EDGE ( 'NONE', *, *, #2527, .T. ) ;
#36717 = DIRECTION ( 'NONE',  ( -1.000000000000000000, -0.000000000000000000, -0.000000000000000000 ) ) ;
#36718 = VERTEX_POINT ( 'NONE', #19945 ) ;
#36719 = EDGE_CURVE ( 'NONE', #21910, #29055, #6096, .T. ) ;
#36720 = CARTESIAN_POINT ( 'NONE',  ( 2.643462169533613793, -42.27470921730922981, -22.81120928486480892 ) ) ;
#36721 =( BOUNDED_SURFACE ( )  B_SPLINE_SURFACE ( 3, 1, ( 
 ( #11559, #15643 ),
 ( #1504, #30636 ),
 ( #34440, #10627 ),
 ( #39153, #29716 ) ),
 .UNSPECIFIED., .F., .F., .F. ) 
 B_SPLINE_SURFACE_WITH_KNOTS ( ( 4, 4 ),
 ( 2, 2 ),
 ( 0.000000000000000000, 1.000000000000000000 ),
 ( 0.000000000000000000, 1.000000000000000000 ),
 .UNSPECIFIED. ) 
 GEOMETRIC_REPRESENTATION_ITEM ( )  RATIONAL_B_SPLINE_SURFACE ( (
 ( 1.000000000000000000, 1.000000000000000000),
 ( 0.9952954269826590483, 0.8620686068821339365),
 ( 0.9952954269826590483, 0.8620686068821339365),
 ( 1.000000000000000000, 1.000000000000000000) ) ) 
 REPRESENTATION_ITEM ( '' )  SURFACE ( )  );
#36722 = CARTESIAN_POINT ( 'NONE',  ( 0.9758171775293918992, 16.42583507057867465, 39.64000636436365710 ) ) ;
#36723 = CIRCLE ( 'NONE', #44727, 2.500000000000000444 ) ;
#36724 = ADVANCED_FACE ( 'NONE', ( #58416 ), #6270, .F. ) ;
#36725 = ORIENTED_EDGE ( 'NONE', *, *, #50413, .T. ) ;
#36726 = EDGE_CURVE ( 'NONE', #16730, #7010, #34342, .T. ) ;
#36727 = CARTESIAN_POINT ( 'NONE',  ( 3.782542959838401497, -35.60516656857437567, 22.34971961838993693 ) ) ;
#36728 = AXIS2_PLACEMENT_3D ( 'NONE', #4949, #58410, #42903 ) ;
#36729 = CARTESIAN_POINT ( 'NONE',  ( 2.648799415243708655, 36.42501529472047395, -32.82888551365973484 ) ) ;
#36730 = DIRECTION ( 'NONE',  ( -0.07500201931887529039, -0.3083113411842438034, -0.9483242135447474963 ) ) ;
#36731 = CIRCLE ( 'NONE', #44733, 2.099999999999999645 ) ;
#36732 = CYLINDRICAL_SURFACE ( 'NONE', #34658, 2.649999999999992806 ) ;
#36734 = ADVANCED_FACE ( 'NONE', ( #24627 ), #25890, .F. ) ;
#36733 = ORIENTED_EDGE ( 'NONE', *, *, #11057, .F. ) ;
#36735 = DIRECTION ( 'NONE',  ( -1.000000000000000000, -0.000000000000000000, -0.000000000000000000 ) ) ;
#36736 = ORIENTED_EDGE ( 'NONE', *, *, #33394, .F. ) ;
#36737 = VERTEX_POINT ( 'NONE', #29619 ) ;
#36738 = CARTESIAN_POINT ( 'NONE',  ( 0.1158516988532803244, -12.50734325492080501, 42.31440090012363697 ) ) ;
#36739 = ADVANCED_FACE ( 'NONE', ( #5790 ), #15105, .F. ) ;
#36740 = CARTESIAN_POINT ( 'NONE',  ( 4.834790513006555379, -26.65333699373609733, 39.01524020203795828 ) ) ;
#36741 = ORIENTED_EDGE ( 'NONE', *, *, #26090, .F. ) ;
#36742 = DIRECTION ( 'NONE',  ( -1.000000000000000000, -0.000000000000000000, -0.000000000000000000 ) ) ;
#36743 = CARTESIAN_POINT ( 'NONE',  ( 3.680882792899938138, 47.94008871805919370, -1.849662971457720850 ) ) ;
#36744 = CARTESIAN_POINT ( 'NONE',  ( 0.6026112563231247332, 27.95217006345316690, 40.37594808358065279 ) ) ;
#36745 = CARTESIAN_POINT ( 'NONE',  ( 0.5837800304671215690, -1.521551379193686770, -46.87133680171679373 ) ) ;
#36746 = CONICAL_SURFACE ( 'NONE', #29731, 42.08604991992415023, 1.569615340895231137 ) ;
#36747 = ORIENTED_EDGE ( 'NONE', *, *, #36688, .T. ) ;
#36748 = ORIENTED_EDGE ( 'NONE', *, *, #4062, .T. ) ;
#36749 = DIRECTION ( 'NONE',  ( -1.000000000000000000, -0.000000000000000000, -0.000000000000000000 ) ) ;
#36750 = CARTESIAN_POINT ( 'NONE',  ( 5.960721111146673579, 17.77882586010667154, -10.25731071096564051 ) ) ;
#36751 = CARTESIAN_POINT ( 'NONE',  ( 0.6041374136657475802, 41.57494627055111636, 24.20487816031535289 ) ) ;
#36752 = FACE_OUTER_BOUND ( 'NONE', #9278, .T. ) ;
#36753 = CARTESIAN_POINT ( 'NONE',  ( 0.5800708057587390387, 6.873290064482054262, -47.40012370174857637 ) ) ;
#36754 = CARTESIAN_POINT ( 'NONE',  ( 1.231276596079881047, -13.22565419922034557, 39.77887431816932917 ) ) ;
#36755 = DIRECTION ( 'NONE',  ( 0.000000000000000000, 0.000000000000000000, 1.000000000000000000 ) ) ;
#36756 = DIRECTION ( 'NONE',  ( 0.07500201931887538753, 0.9957672615368112767, -0.05312492776061850802 ) ) ;
#36757 = CARTESIAN_POINT ( 'NONE',  ( 0.9783242366443536397, 32.72304825568722464, 26.18275392433902837 ) ) ;
#36758 = LINE ( 'NONE', #46461, #59054 ) ;
#36759 = EDGE_CURVE ( 'NONE', #42953, #52918, #51449, .T. ) ;
#36760 = CARTESIAN_POINT ( 'NONE',  ( 5.999999999999998224, 6.934333478519240412E-15, 0.000000000000000000 ) ) ;
#36761 = CARTESIAN_POINT ( 'NONE',  ( 5.895596859100789899, -19.93390588528923857, 2.677233529021818104 ) ) ;
#36762 = CARTESIAN_POINT ( 'NONE',  ( 0.8760168074887076939, -38.69913431881803945, -28.57146030081966259 ) ) ;
#36763 = CARTESIAN_POINT ( 'NONE',  ( 5.895596859100789899, -7.232071727010249695, 18.76766692340490295 ) ) ;
#36764 = EDGE_CURVE ( 'NONE', #50490, #42276, #22085, .T. ) ;
#36765 = CARTESIAN_POINT ( 'NONE',  ( -6.015611763856276717, 16.32183393015596451, 9.416239407363361735 ) ) ;
#36766 = VECTOR ( 'NONE', #19518, 1000.000000000000000 ) ;
#36767 = CARTESIAN_POINT ( 'NONE',  ( 0.6026777506516367566, 17.12337608662687671, 46.02538845064920991 ) ) ;
#36768 = DIRECTION ( 'NONE',  ( 0.000000000000000000, 0.000000000000000000, 1.000000000000000000 ) ) ;
#36770 = ORIENTED_EDGE ( 'NONE', *, *, #16275, .T. ) ;
#36769 = CARTESIAN_POINT ( 'NONE',  ( 3.680974057930773924, 25.57193971028160107, -40.59247216052828122 ) ) ;
#36771 = ORIENTED_EDGE ( 'NONE', *, *, #56434, .T. ) ;
#36772 = B_SPLINE_CURVE_WITH_KNOTS ( 'NONE', 3,
 ( #26571, #31900, #6815, #25958 ),
 .UNSPECIFIED., .F., .F.,
 ( 4, 4 ),
 ( 8.673617379884035472E-19, 0.004042984057420972825 ),
 .UNSPECIFIED. ) ;
#36773 = VECTOR ( 'NONE', #21002, 1000.000000000000000 ) ;
#36774 = CARTESIAN_POINT ( 'NONE',  ( 4.956653778116966613, 0.000000000000000000, 0.000000000000000000 ) ) ;
#36775 = CARTESIAN_POINT ( 'NONE',  ( 1.296416391601052487, 3.124427423165220485, -43.96072482743581844 ) ) ;
#36776 = VECTOR ( 'NONE', #2083, 1000.000000000000227 ) ;
#36777 = DIRECTION ( 'NONE',  ( 0.09835009131224552170, -0.8656670924898581809, -0.4908642831975333354 ) ) ;
#36778 = ORIENTED_EDGE ( 'NONE', *, *, #22208, .T. ) ;
#36779 = ORIENTED_EDGE ( 'NONE', *, *, #11776, .T. ) ;
#36780 = CARTESIAN_POINT ( 'NONE',  ( 1.231276596079887264, -23.26513148155214594, -34.87134107206314582 ) ) ;
#36781 = CARTESIAN_POINT ( 'NONE',  ( 0.6023142530420679819, 6.538792732869218582, 47.66103033449100934 ) ) ;
#36782 = B_SPLINE_CURVE_WITH_KNOTS ( 'NONE', 3,
 ( #2533, #41104, #11647, #36087, #11974, #22277 ),
 .UNSPECIFIED., .F., .F.,
 ( 4, 2, 4 ),
 ( 1.516581828351926341E-16, 0.0002445252820015211413, 0.0004890505640028906028 ),
 .UNSPECIFIED. ) ;
#36783 = B_SPLINE_CURVE_WITH_KNOTS ( 'NONE', 3,
 ( #59312, #49303, #44634, #45556, #6361, #2610, #21115, #16117, #21733, #36160, #40873, #53988, #16419, #16732, #44336, #45259, #40559, #44950, #7294 ),
 .UNSPECIFIED., .F., .F.,
 ( 4, 3, 3, 3, 3, 3, 4 ),
 ( 1.149162571898268292E-16, 0.0002618519381806262963, 0.0003927759815485967884, 0.0005237000248299434300, 0.0006546240681324954399, 0.0007855481115631328176, 0.0009699050456655098577 ),
 .UNSPECIFIED. ) ;
#36784 = UNCERTAINTY_MEASURE_WITH_UNIT (LENGTH_MEASURE( 1.000000000000000082E-05 ), #43873, 'distance_accuracy_value', 'NONE');
#36785 = ORIENTED_EDGE ( 'NONE', *, *, #48647, .F. ) ;
#36786 = ORIENTED_EDGE ( 'NONE', *, *, #851, .T. ) ;
#36787 = CARTESIAN_POINT ( 'NONE',  ( 5.896278296736517710, -19.39678151694237229, -5.319008027667046612 ) ) ;
#36788 = LINE ( 'NONE', #32078, #55932 ) ;
#36789 = CARTESIAN_POINT ( 'NONE',  ( 0.1073791018717483448, -0.4849339620930353534, -43.12183934961191056 ) ) ;
#36790 = EDGE_LOOP ( 'NONE', ( #59316, #16360, #57124, #42653 ) ) ;
#36791 = CARTESIAN_POINT ( 'NONE',  ( 4.303969348037258058, 47.93217632892348234, 4.133486515473467016 ) ) ;
#36792 = CARTESIAN_POINT ( 'NONE',  ( 2.301529144917015657, -47.77346141661147527, -4.990866136406468812 ) ) ;
#36793 = EDGE_CURVE ( 'NONE', #50931, #34042, #17703, .T. ) ;
#36794 = B_SPLINE_CURVE_WITH_KNOTS ( 'NONE', 3,
 ( #27910, #47032, #51383, #23209, #3460, #36711 ),
 .UNSPECIFIED., .F., .F.,
 ( 4, 2, 4 ),
 ( 1.266794085606387986E-16, 0.0002450741128632358658, 0.0004901482257263449884 ),
 .UNSPECIFIED. ) ;
#36795 = CARTESIAN_POINT ( 'NONE',  ( 0.1104177457020372732, 21.56646482560080003, 37.34442418285510001 ) ) ;
#36796 = EDGE_CURVE ( 'NONE', #9480, #49434, #11451, .T. ) ;
#36797 = ORIENTED_EDGE ( 'NONE', *, *, #3371, .T. ) ;
#36798 = ORIENTED_EDGE ( 'NONE', *, *, #36799, .F. ) ;
#36799 = EDGE_CURVE ( 'NONE', #53953, #37569, #40599, .T. ) ;
#36800 = CARTESIAN_POINT ( 'NONE',  ( 0.1129192098497447394, 3.754263797494919341, -43.96427289429421137 ) ) ;
#36801 = ORIENTED_EDGE ( 'NONE', *, *, #34964, .F. ) ;
#36802 = CARTESIAN_POINT ( 'NONE',  ( 0.6041374136657475802, -12.61972904329631540, 46.42299778158134416 ) ) ;
#36803 = CARTESIAN_POINT ( 'NONE',  ( -6.010958268070873523, -0.01451635840150067996, -18.84344976839986785 ) ) ;
#36804 = CARTESIAN_POINT ( 'NONE',  ( 0.6017666602106490625, 33.76944145963975075, -34.26316403931524235 ) ) ;
#36805 = EDGE_CURVE ( 'NONE', #6137, #26843, #55113, .T. ) ;
#36806 = CARTESIAN_POINT ( 'NONE',  ( 0.6000166863083090663, -31.02657807334512086, -38.06803035050636197 ) ) ;
#36807 = CARTESIAN_POINT ( 'NONE',  ( 0.5809828226811565299, -23.47450554821739743, 41.74875432577639600 ) ) ;
#36808 = ORIENTED_EDGE ( 'NONE', *, *, #50234, .T. ) ;
#36809 = CARTESIAN_POINT ( 'NONE',  ( -6.072942160501519915, 11.99473239968607885, -15.06421444845171287 ) ) ;
#36810 = PLANE ( 'NONE',  #43805 ) ;
#36811 = FACE_OUTER_BOUND ( 'NONE', #44054, .T. ) ;
#36812 = ORIENTED_EDGE ( 'NONE', *, *, #55343, .F. ) ;
#36813 = CARTESIAN_POINT ( 'NONE',  ( 2.500000000000000000, 2.357898499370431722, -2.818925648462311528E-15 ) ) ;
#36814 = CARTESIAN_POINT ( 'NONE',  ( -6.015611763856276717, 13.31979030221799398, 13.32857883366838081 ) ) ;
#36815 = CARTESIAN_POINT ( 'NONE',  ( 0.9749527285493310158, 30.13822974582813430, 30.54214995146782741 ) ) ;
#36816 = CARTESIAN_POINT ( 'NONE',  ( 2.359973842542475886, -5.532421374462768604, 43.67525853807723735 ) ) ;
#36817 = EDGE_CURVE ( 'NONE', #30066, #54983, #37709, .T. ) ;
#36818 = VECTOR ( 'NONE', #30463, 1000.000000000000114 ) ;
#36819 = ORIENTED_EDGE ( 'NONE', *, *, #27547, .F. ) ;
#36820 = B_SPLINE_CURVE_WITH_KNOTS ( 'NONE', 3,
 ( #15529, #61869, #4861, #48414 ),
 .UNSPECIFIED., .F., .F.,
 ( 4, 4 ),
 ( 0.000000000000000000, 0.005004948556313810505 ),
 .UNSPECIFIED. ) ;
#36821 = CARTESIAN_POINT ( 'NONE',  ( 0.3676999524040366896, -11.75791688508890331, 42.51707861373098041 ) ) ;
#36822 = FACE_OUTER_BOUND ( 'NONE', #13143, .T. ) ;
#36823 = EDGE_CURVE ( 'NONE', #46958, #51774, #36505, .T. ) ;
#36824 = CARTESIAN_POINT ( 'NONE',  ( 4.691466044806103852, -43.79545162262303393, -8.371234562541701507 ) ) ;
#36825 = PRODUCT ( 'instrument roller bearing_iso_ISO 1224 - 171015 - R,24,SI,NC,24', 'instrument roller bearing_iso_ISO 1224 - 171015 - R,24,SI,NC,24', '', ( #56220 ) ) ;
#36826 = CARTESIAN_POINT ( 'NONE',  ( 1.000110580585055420, -23.10262754908167793, 34.96692841958402198 ) ) ;
#36827 = CARTESIAN_POINT ( 'NONE',  ( -6.001507490154110336, -16.32705935667500796, -9.408444979392495355 ) ) ;
#36828 = CARTESIAN_POINT ( 'NONE',  ( 2.299746137290199055, 21.52978567797254428, -44.05394041793203996 ) ) ;
#36829 =( BOUNDED_SURFACE ( )  B_SPLINE_SURFACE ( 3, 1, ( 
 ( #31506, #60930 ),
 ( #35920, #31828 ),
 ( #26184, #41546 ),
 ( #2368, #50300 ) ),
 .UNSPECIFIED., .F., .F., .F. ) 
 B_SPLINE_SURFACE_WITH_KNOTS ( ( 4, 4 ),
 ( 2, 2 ),
 ( 0.000000000000000000, 1.000000000000000000 ),
 ( 0.000000000000000000, 1.000000000000000000 ),
 .UNSPECIFIED. ) 
 GEOMETRIC_REPRESENTATION_ITEM ( )  RATIONAL_B_SPLINE_SURFACE ( (
 ( 1.000000000000000000, 1.000000000000000000),
 ( 0.7269869731126817891, 0.9931720237060910339),
 ( 0.7269869731126817891, 0.9931720237060910339),
 ( 1.000000000000000000, 1.000000000000000000) ) ) 
 REPRESENTATION_ITEM ( '' )  SURFACE ( )  );
#36830 = DIRECTION ( 'NONE',  ( -1.000000000000000000, -0.000000000000000000, -0.000000000000000000 ) ) ;
#36831 = FACE_OUTER_BOUND ( 'NONE', #21590, .T. ) ;
#36832 = CARTESIAN_POINT ( 'NONE',  ( 5.283180000000047727, 0.000000000000000000, 0.000000000000000000 ) ) ;
#36833 = CARTESIAN_POINT ( 'NONE',  ( 4.956445790444018229, -10.39006634428234577, -45.93021414603951058 ) ) ;
#36834 = ORIENTED_EDGE ( 'NONE', *, *, #2892, .F. ) ;
#36835 = CIRCLE ( 'NONE', #26833, 0.2800000000000024691 ) ;
#36836 = B_SPLINE_CURVE_WITH_KNOTS ( 'NONE', 3,
 ( #903, #53513, #40092, #30332 ),
 .UNSPECIFIED., .F., .F.,
 ( 4, 4 ),
 ( 5.818439421673297140E-18, 0.004566006591234648103 ),
 .UNSPECIFIED. ) ;
#36837 = CARTESIAN_POINT ( 'NONE',  ( 2.648799415243708655, -40.11112523584274925, -28.20664984722818502 ) ) ;
#36838 = CARTESIAN_POINT ( 'NONE',  ( 4.967162193818130511, 0.000000000000000000, 0.000000000000000000 ) ) ;
#36839 = CARTESIAN_POINT ( 'NONE',  ( 0.5987334363312689645, -13.39119798739007905, -47.24657366343718934 ) ) ;
#36840 = CARTESIAN_POINT ( 'NONE',  ( 0.5806925824938502512, 17.36345040154772690, 43.56297685531322372 ) ) ;
#36841 = CARTESIAN_POINT ( 'NONE',  ( 2.706805983486679779, -24.21343163196654658, -36.74895701817722937 ) ) ;
#36842 = VECTOR ( 'NONE', #6484, 1000.000000000000114 ) ;
#36843 = CARTESIAN_POINT ( 'NONE',  ( 0.9780106845699478857, -31.29111759374672630, 27.87825687143571685 ) ) ;
#36844 = SHAPE_DEFINITION_REPRESENTATION ( #29395, #8803 ) ;
#36845 = CARTESIAN_POINT ( 'NONE',  ( 2.526552050251863690, 4.405466163647298039, 42.75269566045968617 ) ) ;
#36846 = ADVANCED_FACE ( 'NONE', ( #45913 ), #27902, .F. ) ;
#36847 = CARTESIAN_POINT ( 'NONE',  ( 4.956445790444004018, -45.27177431812791042, 12.96165499572219737 ) ) ;
#36848 = CARTESIAN_POINT ( 'NONE',  ( 1.827326673878742813, 33.38933471001438846, 27.17438009792344289 ) ) ;
#36850 = VERTEX_POINT ( 'NONE', #55573 ) ;
#36849 = CARTESIAN_POINT ( 'NONE',  ( 5.981074661064941900, -5.320466518160800184, -19.82308078259089612 ) ) ;
#36851 = VERTEX_POINT ( 'NONE', #7335 ) ;
#36852 = LINE ( 'NONE', #8007, #53151 ) ;
#36853 = CARTESIAN_POINT ( 'NONE',  ( 3.407937589446174087, -13.63405474014709462, 1.331713209622455985 ) ) ;
#36854 = CARTESIAN_POINT ( 'NONE',  ( 2.299652685299200972, -9.094837095626216339, 48.18262822908455689 ) ) ;
#36855 = ORIENTED_EDGE ( 'NONE', *, *, #5865, .F. ) ;
#36856 = LINE ( 'NONE', #3291, #55492 ) ;
#36857 = CARTESIAN_POINT ( 'NONE',  ( -3.319141568766058814, -12.31039395171775830, -1.199999999999999956 ) ) ;
#36858 = CARTESIAN_POINT ( 'NONE',  ( 0.9730545539215883499, 39.44597740938085195, -16.88610103448514721 ) ) ;
#36859 = EDGE_LOOP ( 'NONE', ( #50550, #28815, #43164, #50650 ) ) ;
#36860 = VERTEX_POINT ( 'NONE', #16157 ) ;
#36861 = CARTESIAN_POINT ( 'NONE',  ( 0.9780303403264759554, 24.59793831445992041, -33.93053262289160443 ) ) ;
#36862 = AXIS2_PLACEMENT_3D ( 'NONE', #37638, #8174, #8792 ) ;
#36863 = VECTOR ( 'NONE', #55981, 1000.000000000000114 ) ;
#36864 = CARTESIAN_POINT ( 'NONE',  ( 4.962356264823598373, -24.61258717641114657, 34.13877780978559429 ) ) ;
#36865 = DIRECTION ( 'NONE',  ( 1.000000000000000000, 0.000000000000000000, 0.000000000000000000 ) ) ;
#36866 = CARTESIAN_POINT ( 'NONE',  ( 4.958415959904818315, 40.76596448693018715, 20.03347431857450545 ) ) ;
#36867 = CARTESIAN_POINT ( 'NONE',  ( 5.894904586330512508, -18.51647496758831579, 7.852997315440658710 ) ) ;
#36868 = B_SPLINE_CURVE_WITH_KNOTS ( 'NONE', 3,
 ( #58018, #42730, #19847, #4775 ),
 .UNSPECIFIED., .F., .F.,
 ( 4, 4 ),
 ( 0.000000000000000000, 0.005013413432710147645 ),
 .UNSPECIFIED. ) ;
#36869 = CARTESIAN_POINT ( 'NONE',  ( 2.618530812446111078, -12.57566640959636217, -45.29436392701359182 ) ) ;
#36870 = EDGE_CURVE ( 'NONE', #5016, #44428, #12700, .T. ) ;
#36871 = ORIENTED_EDGE ( 'NONE', *, *, #55087, .F. ) ;
#36872 = CARTESIAN_POINT ( 'NONE',  ( -6.077587904424778920, -4.290907484552348272, 18.77189746277512583 ) ) ;
#36873 = CARTESIAN_POINT ( 'NONE',  ( 5.960721111146673579, 20.35079619394242201, 2.672857320903374578 ) ) ;
#36874 = VECTOR ( 'NONE', #22262, 1000.000000000000114 ) ;
#36875 = ORIENTED_EDGE ( 'NONE', *, *, #14240, .T. ) ;
#36876 = CARTESIAN_POINT ( 'NONE',  ( 1.231276596079887264, -31.65135013586864332, -27.48579279545554144 ) ) ;
#36877 = CARTESIAN_POINT ( 'NONE',  ( -6.078457390727109555, 16.77598442640661958, -9.453087197443521106 ) ) ;
#36878 = ADVANCED_FACE ( 'NONE', ( #7976 ), #46216, .T. ) ;
#36879 = CARTESIAN_POINT ( 'NONE',  ( 0.5797568599927116484, 46.38942897415957844, 6.873586263546419772 ) ) ;
#36880 = CARTESIAN_POINT ( 'NONE',  ( 4.967162193818130511, 0.000000000000000000, 0.000000000000000000 ) ) ;
#36881 = VERTEX_POINT ( 'NONE', #7650 ) ;
#36882 = ORIENTED_EDGE ( 'NONE', *, *, #5242, .T. ) ;
#36883 = CARTESIAN_POINT ( 'NONE',  ( 5.981074661064941900, -7.846517100474943440, 18.96560215432003815 ) ) ;
#36884 = CARTESIAN_POINT ( 'NONE',  ( 0.5839254288179568375, 41.43367229384582373, 24.02657516616520539 ) ) ;
#36885 = VERTEX_POINT ( 'NONE', #45593 ) ;
#36886 = CARTESIAN_POINT ( 'NONE',  ( 4.962356264823608143, 0.000000000000000000, 0.000000000000000000 ) ) ;
#36887 = ORIENTED_EDGE ( 'NONE', *, *, #5361, .F. ) ;
#36888 = FACE_OUTER_BOUND ( 'NONE', #21192, .T. ) ;
#36889 = ORIENTED_EDGE ( 'NONE', *, *, #50407, .T. ) ;
#36890 = DIRECTION ( 'NONE',  ( 0.000000000000000000, 0.7071067811865382469, 0.7071067811865566766 ) ) ;
#36891 = CARTESIAN_POINT ( 'NONE',  ( -6.016489644550737204, 7.215050741358277619, -17.40716454747921915 ) ) ;
#36892 = EDGE_CURVE ( 'NONE', #19313, #49122, #49911, .T. ) ;
#36893 = B_SPLINE_CURVE_WITH_KNOTS ( 'NONE', 3,
 ( #15295, #20297, #49102, #38189, #38490, #6153 ),
 .UNSPECIFIED., .F., .F.,
 ( 4, 2, 4 ),
 ( 2.538052214298621590E-18, 0.0002447193893791693828, 0.0004894387787583361635 ),
 .UNSPECIFIED. ) ;
#36894 = CARTESIAN_POINT ( 'NONE',  ( 0.1092355843206037486, -26.49036028133807363, 34.02913268098544819 ) ) ;
#36895 = VERTEX_POINT ( 'NONE', #44990 ) ;
#36897 = AXIS2_PLACEMENT_3D ( 'NONE', #37854, #19340, #28729 ) ;
#36896 = CARTESIAN_POINT ( 'NONE',  ( 5.910764540655177868, 14.92665574186510113, -13.47947279506912466 ) ) ;
#36898 = DIRECTION ( 'NONE',  ( 0.000000000000000000, 0.000000000000000000, 1.000000000000000000 ) ) ;
#36899 = EDGE_CURVE ( 'NONE', #60202, #51250, #36508, .T. ) ;
#36900 = FACE_OUTER_BOUND ( 'NONE', #25628, .T. ) ;
#36901 = B_SPLINE_CURVE_WITH_KNOTS ( 'NONE', 3,
 ( #17405, #22409, #36527, #50592, #59371, #59996 ),
 .UNSPECIFIED., .F., .F.,
 ( 4, 2, 4 ),
 ( 0.000000000000000000, 0.0002447195606305751798, 0.0004894391212611503596 ),
 .UNSPECIFIED. ) ;
#36902 = ORIENTED_EDGE ( 'NONE', *, *, #6764, .F. ) ;
#36903 = CARTESIAN_POINT ( 'NONE',  ( -19.96574511507958150, -12.48220789061827496, -0.6787824490278846490 ) ) ;
#36904 =( BOUNDED_SURFACE ( )  B_SPLINE_SURFACE ( 3, 1, ( 
 ( #27057, #28280 ),
 ( #33311, #61167 ),
 ( #57076, #14208 ),
 ( #33007, #13275 ) ),
 .UNSPECIFIED., .F., .F., .F. ) 
 B_SPLINE_SURFACE_WITH_KNOTS ( ( 4, 4 ),
 ( 2, 2 ),
 ( 0.000000000000000000, 1.000000000000000000 ),
 ( 0.000000000000000000, 1.000000000000000000 ),
 .UNSPECIFIED. ) 
 GEOMETRIC_REPRESENTATION_ITEM ( )  RATIONAL_B_SPLINE_SURFACE ( (
 ( 1.000000000000000000, 1.000000000000000000),
 ( 0.9732289882329797637, 0.9999525324661233672),
 ( 0.9732289882329797637, 0.9999525324661233672),
 ( 1.000000000000000000, 1.000000000000000000) ) ) 
 REPRESENTATION_ITEM ( '' )  SURFACE ( )  );
#36905 = FACE_OUTER_BOUND ( 'NONE', #61083, .T. ) ;
#36906 = CARTESIAN_POINT ( 'NONE',  ( 1.157643937452368599, -26.42675007435921586, 32.53658179806398465 ) ) ;
#36907 = CARTESIAN_POINT ( 'NONE',  ( 0.1102144999581333024, 26.35238362727840311, -34.13606714958023503 ) ) ;
#36908 = CARTESIAN_POINT ( 'NONE',  ( 0.1129192098497455998, 33.28205046155587610, 28.96993104685618547 ) ) ;
#36909 = ORIENTED_EDGE ( 'NONE', *, *, #28940, .F. ) ;
#36910 = CARTESIAN_POINT ( 'NONE',  ( 0.1100247026804066219, 37.43141430507372291, -21.41511734445759529 ) ) ;
#36911 = CARTESIAN_POINT ( 'NONE',  ( 0.6252788684277225117, -48.78635097398380793, -5.597882619074505683 ) ) ;
#36912 = EDGE_LOOP ( 'NONE', ( #2, #7469, #28169, #23139 ) ) ;
#36913 = CIRCLE ( 'NONE', #22890, 42.92674063221959813 ) ;
#36914 = CARTESIAN_POINT ( 'NONE',  ( 0.8751705887134553219, -41.19904111682524928, 24.81530984069135570 ) ) ;
#36915 = CARTESIAN_POINT ( 'NONE',  ( 0.9789889208857696090, -26.98387854568887079, 32.06563887830525061 ) ) ;
#36916 = DIRECTION ( 'NONE',  ( 0.000000000000000000, 0.000000000000000000, 1.000000000000000000 ) ) ;
#36917 = CARTESIAN_POINT ( 'NONE',  ( 1.154321713695928286, 41.66001467525155277, -10.30834583266686977 ) ) ;
#36918 = CARTESIAN_POINT ( 'NONE',  ( 0.6846871229502932144, 23.20185915381556185, 41.91507847151805777 ) ) ;
#36919 = CARTESIAN_POINT ( 'NONE',  ( -6.001507490154110336, -18.84387066167321478, 0.01557731607546725128 ) ) ;
#36920 = CARTESIAN_POINT ( 'NONE',  ( 0.6029443199889047422, 4.715466349721216588, 48.88048709821794091 ) ) ;
#36921 = PRESENTATION_STYLE_ASSIGNMENT (( #41015 ) ) ;
#36922 = CARTESIAN_POINT ( 'NONE',  ( 0.6009452777970412107, 38.43042656245034294, 28.93864923253911314 ) ) ;
#36923 = B_SPLINE_CURVE_WITH_KNOTS ( 'NONE', 3,
 ( #59431, #21543, #40371, #60059 ),
 .UNSPECIFIED., .F., .F.,
 ( 4, 4 ),
 ( 0.000000000000000000, 0.004446090762761356445 ),
 .UNSPECIFIED. ) ;
#36924 = EDGE_CURVE ( 'NONE', #45586, #15076, #28693, .T. ) ;
#36925 = CARTESIAN_POINT ( 'NONE',  ( 0.9741495583595167762, -39.79188455996729346, 16.05424148287313102 ) ) ;
#36926 = CARTESIAN_POINT ( 'NONE',  ( 0.8751705887134423323, -44.08562551107069538, -19.22545746485646490 ) ) ;
#36927 = CARTESIAN_POINT ( 'NONE',  ( 0.1119898979215348395, -27.94769354442891895, -34.14509823969635960 ) ) ;
#36928 = DIRECTION ( 'NONE',  ( 0.000000000000000000, 0.000000000000000000, 1.000000000000000000 ) ) ;
#36929 = AXIS2_PLACEMENT_3D ( 'NONE', #51579, #36594, #46011 ) ;
#36930 = CARTESIAN_POINT ( 'NONE',  ( 0.2885700199627522777, 31.05173037893199606, 29.91358789498793058 ) ) ;
#36931 = CARTESIAN_POINT ( 'NONE',  ( 0.6029443449137434907, -1.530470916618504429, -49.08357359399087017 ) ) ;
#36932 = DIRECTION ( 'NONE',  ( 1.836970198721027962E-16, -1.000000000000000000, 1.069580750882383731E-61 ) ) ;
#36933 = CARTESIAN_POINT ( 'NONE',  ( 3.270143674763207553, -11.98875605389974908, -6.605065939546945764 ) ) ;
#36934 = CARTESIAN_POINT ( 'NONE',  ( 0.8560838555295223751, -26.00596412780120303, -39.03924517540328765 ) ) ;
#36935 = DIRECTION ( 'NONE',  ( -1.000000000000000000, -0.000000000000000000, -0.000000000000000000 ) ) ;
#36936 = AXIS2_PLACEMENT_3D ( 'NONE', #28728, #43158, #192 ) ;
#36937 = ORIENTED_EDGE ( 'NONE', *, *, #29828, .T. ) ;
#36938 = CARTESIAN_POINT ( 'NONE',  ( 2.281448460670576939, 47.37344300043622525, -7.562315317391275826 ) ) ;
#36939 = CARTESIAN_POINT ( 'NONE',  ( -5.995132425357893702, -18.68405145320022243, -2.451215106828539714 ) ) ;
#36940 = DIRECTION ( 'NONE',  ( -1.807003620809173399E-16, 1.000000000000000000, 0.000000000000000000 ) ) ;
#36941 = CARTESIAN_POINT ( 'NONE',  ( 0.6028777368367060907, -45.48575615302912922, -18.50907389628789090 ) ) ;
#36942 = ORIENTED_EDGE ( 'NONE', *, *, #53350, .F. ) ;
#36943 = FACE_OUTER_BOUND ( 'NONE', #59260, .T. ) ;
#36944 = CARTESIAN_POINT ( 'NONE',  ( 0.6028618097248863439, 23.90242650600276519, -41.74935807801021781 ) ) ;
#36945 = ORIENTED_EDGE ( 'NONE', *, *, #18279, .F. ) ;
#36946 = CARTESIAN_POINT ( 'NONE',  ( 2.009741617377216460, -26.37340513181155544, 35.26964104405346490 ) ) ;
#36947 = ADVANCED_FACE ( 'NONE', ( #36822 ), #23149, .F. ) ;
#36948 = ORIENTED_EDGE ( 'NONE', *, *, #18601, .F. ) ;
#36949 = CARTESIAN_POINT ( 'NONE',  ( 0.5832366564991497970, -0.2724446024274073119, -47.89515933308369000 ) ) ;
#36951 = CARTESIAN_POINT ( 'NONE',  ( 0.2885700199627497242, 22.25146206940414118, 36.93108631019301669 ) ) ;
#36950 = CIRCLE ( 'NONE', #9931, 42.08604991992415023 ) ;
#36952 = ORIENTED_EDGE ( 'NONE', *, *, #15447, .T. ) ;
#36953 = CARTESIAN_POINT ( 'NONE',  ( 0.5998501479064708430, -28.86886762351098312, -38.48283596222019298 ) ) ;
#36954 = CARTESIAN_POINT ( 'NONE',  ( 0.5827357941260201679, -28.86820951701459492, 38.21849163199665611 ) ) ;
#36956 = ORIENTED_EDGE ( 'NONE', *, *, #5129, .T. ) ;
#36955 = EDGE_CURVE ( 'NONE', #37400, #37022, #29057, .T. ) ;
#36957 = CARTESIAN_POINT ( 'NONE',  ( 4.694002226626920127, -41.22189368134345244, -19.46895612944235765 ) ) ;
#36958 = CARTESIAN_POINT ( 'NONE',  ( 0.1073791018717483448, -26.63563652260144821, -33.91564619577798823 ) ) ;
#36959 = ORIENTED_EDGE ( 'NONE', *, *, #24836, .F. ) ;
#36960 = B_SPLINE_CURVE_WITH_KNOTS ( 'NONE', 3,
 ( #18945, #14856, #9515, #16383, #6021, #19866, #29857, #48972, #48657, #35508, #44604, #10770, #20465, #54566, #11697, #1642, #49269, #6956, #11077 ),
 .UNSPECIFIED., .F., .F.,
 ( 4, 3, 3, 3, 3, 3, 4 ),
 ( 1.153344816771540786E-16, 0.0002618519381806232063, 0.0003927759815485975473, 0.0005237000248299442974, 0.0006546240681324945725, 0.0007855481115631333597, 0.0009699050456655120261 ),
 .UNSPECIFIED. ) ;
#36961 = CARTESIAN_POINT ( 'NONE',  ( 5.901764892641307547, -32.95403503760685737, 36.22185862403885892 ) ) ;
#36962 = EDGE_CURVE ( 'NONE', #3984, #47332, #13621, .T. ) ;
#36963 = VERTEX_POINT ( 'NONE', #18322 ) ;
#36964 = CARTESIAN_POINT ( 'NONE',  ( 0.5806925824938506953, -38.96949031362410665, -26.08833430941730924 ) ) ;
#36965 = ORIENTED_EDGE ( 'NONE', *, *, #3602, .T. ) ;
#36966 = B_SPLINE_CURVE_WITH_KNOTS ( 'NONE', 3,
 ( #3795, #31711, #22935, #26382 ),
 .UNSPECIFIED., .F., .F.,
 ( 4, 4 ),
 ( 6.992893892674702526E-18, 0.004566006591234645501 ),
 .UNSPECIFIED. ) ;
#36967 = ORIENTED_EDGE ( 'NONE', *, *, #18167, .F. ) ;
#36968 = CARTESIAN_POINT ( 'NONE',  ( 0.6008123274975391004, -42.57300165257447588, -24.47639845745999310 ) ) ;
#36969 = CARTESIAN_POINT ( 'NONE',  ( 4.956653778116971942, 35.79382859084115864, 32.11725092155054995 ) ) ;
#36970 = CARTESIAN_POINT ( 'NONE',  ( 4.975801465491695552, -26.14269827151708370, 40.15204426031488794 ) ) ;
#36971 = CIRCLE ( 'NONE', #20939, 41.88877248453276536 ) ;
#36972 = DIRECTION ( 'NONE',  ( 1.000000000000000000, 1.836909530733573776E-16, 0.000000000000000000 ) ) ;
#36973 = CARTESIAN_POINT ( 'NONE',  ( 0.1129192098497455998, -7.520259262076605999, 43.47870154933683295 ) ) ;
#36974 = VERTEX_POINT ( 'NONE', #42747 ) ;
#36975 = CARTESIAN_POINT ( 'NONE',  ( 1.479689385636123067, 5.399678476185347797, 43.73130820843933719 ) ) ;
#36976 = CARTESIAN_POINT ( 'NONE',  ( 4.303969348037246512, -46.98258166031697414, 10.35452842635826975 ) ) ;
#36977 = EDGE_CURVE ( 'NONE', #55224, #20551, #26715, .T. ) ;
#36978 = CARTESIAN_POINT ( 'NONE',  ( 5.894904586330512508, 20.06808393774119281, -1.342169560605708467 ) ) ;
#36979 = ORIENTED_EDGE ( 'NONE', *, *, #47122, .T. ) ;
#36980 = VERTEX_POINT ( 'NONE', #28618 ) ;
#36981 = CYLINDRICAL_SURFACE ( 'NONE', #41288, 6.728125000000022560 ) ;
#36982 = CARTESIAN_POINT ( 'NONE',  ( 0.3676999524040323597, -26.85386693986589890, -34.99743438737782242 ) ) ;
#36983 = CARTESIAN_POINT ( 'NONE',  ( 4.553261556744873317, 22.57774691820481294, -37.68003330573274923 ) ) ;
#36984 = CARTESIAN_POINT ( 'NONE',  ( 0.8557997880470606944, 43.90420959842181503, 19.17299735372024827 ) ) ;
#36985 = CARTESIAN_POINT ( 'NONE',  ( 0.1073791018717578927, -42.68962945260949482, -6.109314776652552403 ) ) ;
#36986 = CARTESIAN_POINT ( 'NONE',  ( 3.376099380956838925, 11.76186387009564349, -6.431713763329790723 ) ) ;
#36987 =( BOUNDED_SURFACE ( )  B_SPLINE_SURFACE ( 3, 1, ( 
 ( #6688, #59640 ),
 ( #10820, #26137 ),
 ( #29911, #20222 ),
 ( #49631, #2005 ) ),
 .UNSPECIFIED., .F., .F., .F. ) 
 B_SPLINE_SURFACE_WITH_KNOTS ( ( 4, 4 ),
 ( 2, 2 ),
 ( 0.000000000000000000, 1.000000000000000000 ),
 ( 0.000000000000000000, 1.000000000000000000 ),
 .UNSPECIFIED. ) 
 GEOMETRIC_REPRESENTATION_ITEM ( )  RATIONAL_B_SPLINE_SURFACE ( (
 ( 1.000000000000000000, 1.000000000000000000),
 ( 0.7223157951917476005, 0.9931996967497186413),
 ( 0.7223157951917476005, 0.9931996967497186413),
 ( 1.000000000000000000, 1.000000000000000000) ) ) 
 REPRESENTATION_ITEM ( '' )  SURFACE ( )  );
#36988 = EDGE_LOOP ( 'NONE', ( #10133, #2657, #10424, #55949 ) ) ;
#36989 = CARTESIAN_POINT ( 'NONE',  ( 1.793499172322287949, -0.3976920648075739639, -41.94333330318345077 ) ) ;
#36990 = CARTESIAN_POINT ( 'NONE',  ( -6.077587904424778920, 7.788877841491995468, -17.61049128685073129 ) ) ;
#36991 = CARTESIAN_POINT ( 'NONE',  ( 4.963659409799330291, -19.36487359954670140, -40.34793212403990736 ) ) ;
#36992 = B_SPLINE_CURVE_WITH_KNOTS ( 'NONE', 3,
 ( #33087, #42487, #28360, #48396, #52159, #5456 ),
 .UNSPECIFIED., .F., .F.,
 ( 4, 2, 4 ),
 ( 7.757919228897728493E-18, 0.0002291978881530151843, 0.0004583957763060226166 ),
 .UNSPECIFIED. ) ;
#36993 = CARTESIAN_POINT ( 'NONE',  ( 0.5837800304671242335, -41.83504527563591324, -21.19118493536846870 ) ) ;
#36994 = CARTESIAN_POINT ( 'NONE',  ( 3.559346040607745287, -43.29952482140919301, 7.653850781283672688 ) ) ;
#36995 = B_SPLINE_CURVE_WITH_KNOTS ( 'NONE', 3,
 ( #221, #57862, #9338, #47569 ),
 .UNSPECIFIED., .F., .F.,
 ( 4, 4 ),
 ( 6.992893892674702526E-18, 0.005013413432710137237 ),
 .UNSPECIFIED. ) ;
#36996 = VECTOR ( 'NONE', #53002, 1000.000000000000000 ) ;
#36997 = VERTEX_POINT ( 'NONE', #18944 ) ;
#36998 = CARTESIAN_POINT ( 'NONE',  ( 0.5988103622719984642, 37.79415722405556721, 29.76496569135174752 ) ) ;
#36999 = CARTESIAN_POINT ( 'NONE',  ( -5.272380000000000067, 0.000000000000000000, 12.49999999999999822 ) ) ;
#37000 = CARTESIAN_POINT ( 'NONE',  ( 0.8551540677456715978, 7.157691013575044892, -47.37911285756612756 ) ) ;
#37001 =( BOUNDED_SURFACE ( )  B_SPLINE_SURFACE ( 3, 1, ( 
 ( #9033, #56642 ),
 ( #18446, #4937 ),
 ( #52244, #46969 ),
 ( #9341, #23145 ) ),
 .UNSPECIFIED., .F., .F., .F. ) 
 B_SPLINE_SURFACE_WITH_KNOTS ( ( 4, 4 ),
 ( 2, 2 ),
 ( 0.000000000000000000, 1.000000000000000000 ),
 ( 0.000000000000000000, 1.000000000000000000 ),
 .UNSPECIFIED. ) 
 GEOMETRIC_REPRESENTATION_ITEM ( )  RATIONAL_B_SPLINE_SURFACE ( (
 ( 1.000000000000000000, 1.000000000000000000),
 ( 0.9953485035131437453, 0.8621029689291523912),
 ( 0.9953485035131437453, 0.8621029689291523912),
 ( 1.000000000000000000, 1.000000000000000000) ) ) 
 REPRESENTATION_ITEM ( '' )  SURFACE ( )  );
#37002 = CARTESIAN_POINT ( 'NONE',  ( 0.5850706913938533704, 29.30134895053109645, -37.88789093229775062 ) ) ;
#37003 = CARTESIAN_POINT ( 'NONE',  ( 4.956653778116990594, -26.26162724282345096, -40.28700667097706400 ) ) ;
#37004 = ADVANCED_FACE ( 'NONE', ( #8582 ), #8306, .F. ) ;
#37005 = CARTESIAN_POINT ( 'NONE',  ( 4.962356264823593932, 31.50371261889118557, 27.90612278853270922 ) ) ;
#37006 = B_SPLINE_CURVE_WITH_KNOTS ( 'NONE', 3,
 ( #496, #51573, #32815, #42836, #61282, #8987 ),
 .UNSPECIFIED., .F., .F.,
 ( 4, 2, 4 ),
 ( 2.504320737601683728E-17, 0.0002293755540694346795, 0.0004587511081388443140 ),
 .UNSPECIFIED. ) ;
#37007 = CARTESIAN_POINT ( 'NONE',  ( 1.231276596079881047, 19.39962232756238691, 37.16088568059176112 ) ) ;
#37008 = CARTESIAN_POINT ( 'NONE',  ( 0.5837800304671207918, 22.57726808510225425, -41.10358011162680469 ) ) ;
#37009 = EDGE_CURVE ( 'NONE', #54002, #31835, #40182, .T. ) ;
#37010 = EDGE_CURVE ( 'NONE', #45271, #50728, #28318, .T. ) ;
#37011 = DIRECTION ( 'NONE',  ( -1.000000000000000000, -0.000000000000000000, -0.000000000000000000 ) ) ;
#37012 = CARTESIAN_POINT ( 'NONE',  ( 4.335381028904216727, 39.85754067141783707, -28.48040202122537679 ) ) ;
#37013 = VERTEX_POINT ( 'NONE', #46517 ) ;
#37014 = CARTESIAN_POINT ( 'NONE',  ( -6.077587904424778920, 19.25606354205735116, -0.006185319731011218458 ) ) ;
#37015 = B_SPLINE_CURVE_WITH_KNOTS ( 'NONE', 3,
 ( #22910, #27914, #9407, #23511, #42040, #22600, #4073, #52315, #46727, #28512, #42961, #9102, #23212, #8796, #57016, #18516 ),
 .UNSPECIFIED., .F., .F.,
 ( 4, 3, 3, 3, 3, 4 ),
 ( 1.127622383284612036E-17, 0.0002724568934985555470, 0.0004086836638483797675, 0.0005449104342063609829, 0.0008173270854453709017, 0.001089761613562690743 ),
 .UNSPECIFIED. ) ;
#37016 = CARTESIAN_POINT ( 'NONE',  ( 0.9787284016396619046, 20.30453793353213854, 36.66144757418319955 ) ) ;
#37017 = CARTESIAN_POINT ( 'NONE',  ( 0.5998501479064708430, -38.48283596222049141, 28.86886762351059588 ) ) ;
#37018 = CARTESIAN_POINT ( 'NONE',  ( 0.7056313189692740018, -45.78630481351672188, 10.16675638939457649 ) ) ;
#37019 = ORIENTED_EDGE ( 'NONE', *, *, #5959, .T. ) ;
#37020 = CARTESIAN_POINT ( 'NONE',  ( 0.5809828226811553087, 46.11980934799357357, -12.92184523170154620 ) ) ;
#37021 = CARTESIAN_POINT ( 'NONE',  ( 0.9789233960466698914, -41.80609487568101201, -2.930385312190553648 ) ) ;
#37022 = VERTEX_POINT ( 'NONE', #22698 ) ;
#37023 = CARTESIAN_POINT ( 'NONE',  ( 1.199999999999992628, 0.000000000000000000, -6.728125000000023448 ) ) ;
#37024 = FACE_OUTER_BOUND ( 'NONE', #30081, .T. ) ;
#37025 = CARTESIAN_POINT ( 'NONE',  ( 0.7044674535453004927, -45.83030039157684854, -17.64614090470599805 ) ) ;
#37026 = EDGE_CURVE ( 'NONE', #54760, #43185, #51339, .T. ) ;
#37027 = ORIENTED_EDGE ( 'NONE', *, *, #32121, .F. ) ;
#37028 = LINE ( 'NONE', #52007, #5814 ) ;
#37029 = ORIENTED_EDGE ( 'NONE', *, *, #34731, .F. ) ;
#37030 = ORIENTED_EDGE ( 'NONE', *, *, #18837, .T. ) ;
#37031 = FACE_OUTER_BOUND ( 'NONE', #40474, .T. ) ;
#37032 = ORIENTED_EDGE ( 'NONE', *, *, #30276, .F. ) ;
#37033 = CARTESIAN_POINT ( 'NONE',  ( 1.157643937452369487, 24.19453194249153327, -34.22903590051158318 ) ) ;
#37034 = ORIENTED_EDGE ( 'NONE', *, *, #7416, .F. ) ;
#37035 = CARTESIAN_POINT ( 'NONE',  ( 0.6000166863083106206, -42.53190469623904590, -24.55321902762431918 ) ) ;
#37036 = ADVANCED_FACE ( 'NONE', ( #41832 ), #51491, .T. ) ;
#37037 = B_SPLINE_CURVE_WITH_KNOTS ( 'NONE', 3,
 ( #30383, #20390, #49814, #59198 ),
 .UNSPECIFIED., .F., .F.,
 ( 4, 4 ),
 ( 0.000000000000000000, 0.005004741218457418872 ),
 .UNSPECIFIED. ) ;
#37038 = FACE_OUTER_BOUND ( 'NONE', #54636, .T. ) ;
#37039 = CARTESIAN_POINT ( 'NONE',  ( 3.238018933889920792, 11.38191749426270150, 7.061122185704597598 ) ) ;
#37040 = ORIENTED_EDGE ( 'NONE', *, *, #21155, .F. ) ;
#37041 = CARTESIAN_POINT ( 'NONE',  ( 0.1140933569871964981, 14.88246909729719825, 41.53868153482846992 ) ) ;
#37042 = VECTOR ( 'NONE', #49247, 1000.000000000000000 ) ;
#37043 = CARTESIAN_POINT ( 'NONE',  ( 0.5834584762367766020, -44.24114406392340726, -15.55497222525211143 ) ) ;
#37044 = CARTESIAN_POINT ( 'NONE',  ( 0.3622758884714730732, -11.95365414648468594, -41.42293301073622303 ) ) ;
#37045 = ORIENTED_EDGE ( 'NONE', *, *, #5508, .T. ) ;
#37046 = CARTESIAN_POINT ( 'NONE',  ( 0.6064515330803581517, 43.44825878165435995, 17.65171790165140919 ) ) ;
#37047 = EDGE_CURVE ( 'NONE', #52648, #38360, #40958, .T. ) ;
#37048 = ORIENTED_EDGE ( 'NONE', *, *, #3170, .F. ) ;
#37049 = CARTESIAN_POINT ( 'NONE',  ( 5.860006189529246790, -31.78942168514539546, -36.27483683749468923 ) ) ;
#37050 = VERTEX_POINT ( 'NONE', #43368 ) ;
#37051 = CARTESIAN_POINT ( 'NONE',  ( 0.6064515330803604831, -25.83061180769639620, -39.14222566075134324 ) ) ;
#37052 = CARTESIAN_POINT ( 'NONE',  ( 0.1313383488274123267, 11.77600546273712290, 41.48452234694100582 ) ) ;
#37053 = EDGE_LOOP ( 'NONE', ( #36778, #25678, #57378, #46339 ) ) ;
#37054 = CARTESIAN_POINT ( 'NONE',  ( 30.00000000000000711, 16.00000000000000000, -1.386669559958810165E-30 ) ) ;
#37055 = CARTESIAN_POINT ( 'NONE',  ( 0.8560838555295158248, -35.39593983670192756, 30.78149244527153883 ) ) ;
#37056 = EDGE_LOOP ( 'NONE', ( #21484, #37096, #42160, #60952 ) ) ;
#37057 = CARTESIAN_POINT ( 'NONE',  ( 1.088908134280555107, 41.64642044161488599, 10.35121946298427709 ) ) ;
#37058 = CARTESIAN_POINT ( 'NONE',  ( 0.9769922540276045897, -41.84221118692512675, 2.358159891712742429 ) ) ;
#37059 = CARTESIAN_POINT ( 'NONE',  ( 2.281448460670572054, -13.68109378871678139, -45.98107640562109566 ) ) ;
#37060 = CARTESIAN_POINT ( 'NONE',  ( -6.016761891674565099, 18.68243340030205957, -2.456125503350522710 ) ) ;
#37061 = DIRECTION ( 'NONE',  ( 0.000000000000000000, 0.000000000000000000, 1.000000000000000000 ) ) ;
#37062 = CARTESIAN_POINT ( 'NONE',  ( -6.077587904424778920, -19.21689618909968544, 1.227567615773810239 ) ) ;
#37063 = CARTESIAN_POINT ( 'NONE',  ( 4.956653778116966613, 0.000000000000000000, 0.000000000000000000 ) ) ;
#37064 = CARTESIAN_POINT ( 'NONE',  ( 0.5834872094924168362, -46.32218741137608475, 12.17696997821507132 ) ) ;
#37065 = CARTESIAN_POINT ( 'NONE',  ( 5.901463166500145796, -15.79333916981814134, 12.45344563595652509 ) ) ;
#37066 = LINE ( 'NONE', #33286, #33230 ) ;
#37067 = CARTESIAN_POINT ( 'NONE',  ( -17.97369999999976642, -12.32233744059949210, -2.099999999999997424 ) ) ;
#37068 = EDGE_CURVE ( 'NONE', #29664, #40762, #5711, .T. ) ;
#37069 = CARTESIAN_POINT ( 'NONE',  ( 1.154321485836935057, 33.53917069757689973, -26.77578840293002216 ) ) ;
#37070 = CARTESIAN_POINT ( 'NONE',  ( -6.001507490154111224, -7.225628667346702727, 17.40350523682693051 ) ) ;
#37071 = CARTESIAN_POINT ( 'NONE',  ( 0.6253024248130465423, 17.60252607561340099, -45.84315982973894421 ) ) ;
#37072 = CARTESIAN_POINT ( 'NONE',  ( 0.9747592971366230152, 37.32069240268771892, 21.17324310849245705 ) ) ;
#37074 = EDGE_CURVE ( 'NONE', #56714, #52535, #14754, .T. ) ;
#37073 = CARTESIAN_POINT ( 'NONE',  ( 5.894904586330512508, -7.227592724925899326, 18.76942501687893738 ) ) ;
#37075 =( BOUNDED_SURFACE ( )  B_SPLINE_SURFACE ( 3, 1, ( 
 ( #38235, #47298 ),
 ( #13487, #51057 ),
 ( #46700, #17880 ),
 ( #27267, #23483 ) ),
 .UNSPECIFIED., .F., .F., .F. ) 
 B_SPLINE_SURFACE_WITH_KNOTS ( ( 4, 4 ),
 ( 2, 2 ),
 ( 0.000000000000000000, 1.000000000000000000 ),
 ( 0.000000000000000000, 1.000000000000000000 ),
 .UNSPECIFIED. ) 
 GEOMETRIC_REPRESENTATION_ITEM ( )  RATIONAL_B_SPLINE_SURFACE ( (
 ( 1.000000000000000000, 1.000000000000000000),
 ( 0.7269869731126817891, 0.9931720237060910339),
 ( 0.7269869731126817891, 0.9931720237060910339),
 ( 1.000000000000000000, 1.000000000000000000) ) ) 
 REPRESENTATION_ITEM ( '' )  SURFACE ( )  );
#37076 = CARTESIAN_POINT ( 'NONE',  ( 0.6846871229502899947, 34.48177377577836467, 33.25969555998755567 ) ) ;
#37077 = EDGE_CURVE ( 'NONE', #56211, #60, #29545, .T. ) ;
#37078 = CARTESIAN_POINT ( 'NONE',  ( 0.6001305935487422083, -47.62765676940938420, -6.798494447612039693 ) ) ;
#37079 = CARTESIAN_POINT ( 'NONE',  ( 1.088908134280559326, 11.85879120571506284, 41.24246781061821565 ) ) ;
#37080 = ADVANCED_FACE ( 'NONE', ( #38364 ), #29856, .T. ) ;
#37082 = ORIENTED_EDGE ( 'NONE', *, *, #24309, .T. ) ;
#37081 = CARTESIAN_POINT ( 'NONE',  ( 0.9756008150404611445, 39.69644259322205926, 16.28894658522346361 ) ) ;
#37084 = ORIENTED_EDGE ( 'NONE', *, *, #49698, .T. ) ;
#37083 = B_SPLINE_CURVE_WITH_KNOTS ( 'NONE', 3,
 ( #57416, #9518, #51496, #60902, #13626, #18016, #37134, #47750, #14555, #51812, #52120, #42151, #28323, #56202, #3570, #33656, #27395, #61509, #23626 ),
 .UNSPECIFIED., .F., .F.,
 ( 4, 3, 3, 3, 3, 3, 4 ),
 ( 3.469552829456483146E-18, 0.0002612768053151680227, 0.0003919133833142895160, 0.0005225499612322576093, 0.0006531865391693353080, 0.0008112755173415210500, 0.0009693688056799712720 ),
 .UNSPECIFIED. ) ;
#37085 = CARTESIAN_POINT ( 'NONE',  ( 0.6000166863083090663, -34.91285637184702040, 34.53861522509602366 ) ) ;
#37086 = CARTESIAN_POINT ( 'NONE',  ( -6.072942160501519915, -17.34299816270055317, 8.368068894170592742 ) ) ;
#37087 = ADVANCED_FACE ( 'NONE', ( #20169 ), #4650, .F. ) ;
#37088 = CARTESIAN_POINT ( 'NONE',  ( 5.959547316686252039, 19.82530672674354832, 5.315863417546399461 ) ) ;
#37089 = VERTEX_POINT ( 'NONE', #48354 ) ;
#37090 = EDGE_LOOP ( 'NONE', ( #7726, #9038 ) ) ;
#37091 = CARTESIAN_POINT ( 'NONE',  ( 0.9268187852002115479, -30.97276895400849384, 31.37581737947608218 ) ) ;
#37092 = CARTESIAN_POINT ( 'NONE',  ( 0.9972139404380295780, 4.947665363829381491, -42.62325912566426211 ) ) ;
#37093 =( BOUNDED_SURFACE ( )  B_SPLINE_SURFACE ( 3, 1, ( 
 ( #47779, #9239 ),
 ( #28348, #23049 ),
 ( #56230, #19277 ),
 ( #14275, #5138 ) ),
 .UNSPECIFIED., .F., .F., .F. ) 
 B_SPLINE_SURFACE_WITH_KNOTS ( ( 4, 4 ),
 ( 2, 2 ),
 ( 0.000000000000000000, 1.000000000000000000 ),
 ( 0.000000000000000000, 1.000000000000000000 ),
 .UNSPECIFIED. ) 
 GEOMETRIC_REPRESENTATION_ITEM ( )  RATIONAL_B_SPLINE_SURFACE ( (
 ( 1.000000000000000000, 1.000000000000000000),
 ( 0.7269869731126821222, 0.9931720237060910339),
 ( 0.7269869731126821222, 0.9931720237060910339),
 ( 1.000000000000000000, 1.000000000000000000) ) ) 
 REPRESENTATION_ITEM ( '' )  SURFACE ( )  );
#37095 = ORIENTED_EDGE ( 'NONE', *, *, #61142, .F. ) ;
#37094 = AXIS2_PLACEMENT_3D ( 'NONE', #16053, #24509, #33933 ) ;
#37096 = ORIENTED_EDGE ( 'NONE', *, *, #17771, .T. ) ;
#37097 = ADVANCED_FACE ( 'NONE', ( #47745 ), #18692, .F. ) ;
#37098 = CARTESIAN_POINT ( 'NONE',  ( 3.238018933889920792, 5.069615556373336496, -12.39784217024198121 ) ) ;
#37099 = EDGE_CURVE ( 'NONE', #25364, #45115, #10141, .T. ) ;
#37100 = FACE_OUTER_BOUND ( 'NONE', #17364, .T. ) ;
#37101 = CARTESIAN_POINT ( 'NONE',  ( 1.157643937452369265, -2.225587402986053398, -41.85748481820694877 ) ) ;
#37102 = ORIENTED_EDGE ( 'NONE', *, *, #15211, .F. ) ;
#37103 = VERTEX_POINT ( 'NONE', #52730 ) ;
#37104 = CARTESIAN_POINT ( 'NONE',  ( 4.694002226626921015, 36.32786722402816793, -27.54216466437439337 ) ) ;
#37105 = B_SPLINE_CURVE_WITH_KNOTS ( 'NONE', 3,
 ( #54618, #44653, #21133, #59330, #45274, #11751 ),
 .UNSPECIFIED., .F., .F.,
 ( 4, 2, 4 ),
 ( 0.000000000000000000, 0.0002447195606305739330, 0.0004894391212611478659 ),
 .UNSPECIFIED. ) ;
#37106 = CARTESIAN_POINT ( 'NONE',  ( 0.8751705887134553219, -47.79200036674276220, -5.393078191592532988 ) ) ;
#37107 = B_SPLINE_CURVE_WITH_KNOTS ( 'NONE', 3,
 ( #41412, #16344, #16662, #2847, #59865, #31373, #11655, #35782, #36402, #50172, #36096, #41111, #45803, #22284, #60170, #50469, #55775, #26665, #7229 ),
 .UNSPECIFIED., .F., .F.,
 ( 4, 3, 3, 3, 3, 3, 4 ),
 ( 1.040890552917501732E-17, 0.0002724573126191767855, 0.0004086839781548530308, 0.0005449106435901854978, 0.0006811373090491518916, 0.0008459866663933626523, 0.001010840725717205343 ),
 .UNSPECIFIED. ) ;
#37108 = CARTESIAN_POINT ( 'NONE',  ( 0.6025881611877910160, -48.10699274197334319, -0.2181813582436762100 ) ) ;
#37109 = ORIENTED_EDGE ( 'NONE', *, *, #42718, .F. ) ;
#37110 = EDGE_LOOP ( 'NONE', ( #5482, #34550, #39012, #26813 ) ) ;
#37111 = CARTESIAN_POINT ( 'NONE',  ( 5.960221823109900008, 17.77840967225706592, 10.25807604135628104 ) ) ;
#37112 = ORIENTED_EDGE ( 'NONE', *, *, #51297, .T. ) ;
#37113 = CARTESIAN_POINT ( 'NONE',  ( 0.9722240750034555345, 20.94823713380391439, -37.44729079646473480 ) ) ;
#37114 = CARTESIAN_POINT ( 'NONE',  ( 0.5998501479064699549, 33.64490850298844293, -34.38546660123262200 ) ) ;
#37115 = CARTESIAN_POINT ( 'NONE',  ( 0.5804410086790514622, 4.150428748652404742, -46.71502748642835456 ) ) ;
#37116 = CARTESIAN_POINT ( 'NONE',  ( 16.60577576646022635, -4.999999999999987566, 6.123233995736738672E-16 ) ) ;
#37117 = B_SPLINE_CURVE_WITH_KNOTS ( 'NONE', 3,
 ( #27236, #41659, #13153, #32253, #46666, #3709, #22845, #54798, #31009, #50118, #26305, #2487, #21611, #40751, #236, #33183, #32565, #14080, #13453 ),
 .UNSPECIFIED., .F., .F.,
 ( 4, 3, 3, 3, 3, 3, 4 ),
 ( 1.185767046459373819E-16, 0.0002618519381806248868, 0.0003927759815485954331, 0.0005237000248299434300, 0.0006546240681324973915, 0.0007855481115631293481, 0.0009699050456655103998 ),
 .UNSPECIFIED. ) ;
#37118 = EDGE_CURVE ( 'NONE', #27417, #23299, #15526, .T. ) ;
#37119 = ORIENTED_EDGE ( 'NONE', *, *, #40023, .T. ) ;
#37120 = CARTESIAN_POINT ( 'NONE',  ( 0.9730545539215883499, -29.98130006528840141, -30.69604515769682251 ) ) ;
#37121 = CARTESIAN_POINT ( 'NONE',  ( -6.063463321072276813, 18.62294427965544585, -4.899632520538490965 ) ) ;
#37122 = ADVANCED_FACE ( 'NONE', ( #14854 ), #42737, .F. ) ;
#37123 = CARTESIAN_POINT ( 'NONE',  ( 0.1097557419366048670, 39.75589591229785924, -16.70891382096329281 ) ) ;
#37124 = ORIENTED_EDGE ( 'NONE', *, *, #49370, .T. ) ;
#37125 = CARTESIAN_POINT ( 'NONE',  ( 0.1073791018717578927, 42.81622261970994003, -5.147744207006430983 ) ) ;
#37126 = CARTESIAN_POINT ( 'NONE',  ( -6.890143360408123030, -11.60930335864404306, -1.199999999999999956 ) ) ;
#37127 = CARTESIAN_POINT ( 'NONE',  ( 2.526552050251864134, 33.34585601411865952, 27.11558601691277204 ) ) ;
#37128 = VERTEX_POINT ( 'NONE', #6020 ) ;
#37129 = CARTESIAN_POINT ( 'NONE',  ( 0.3676999524040323597, 19.66859742988730986, 39.48540057367873857 ) ) ;
#37130 = CARTESIAN_POINT ( 'NONE',  ( 0.1092355843206037486, -42.79374386763049642, 5.330717085612596939 ) ) ;
#37131 = PRODUCT_RELATED_PRODUCT_CATEGORY ( 'part', '', ( #13314 ) ) ;
#37132 = CARTESIAN_POINT ( 'NONE',  ( 0.5997462898726536595, -30.20781297212619165, 38.71743361310707598 ) ) ;
#37133 = CARTESIAN_POINT ( 'NONE',  ( 0.8744876279028306332, -13.11369837310865805, 47.31153099782990523 ) ) ;
#37134 = CARTESIAN_POINT ( 'NONE',  ( 0.1157506346131639274, -17.94551365393233411, -40.31003844576883921 ) ) ;
#37135 = CARTESIAN_POINT ( 'NONE',  ( 0.2230388203127650903, -34.66629317821153222, -25.64246103889284356 ) ) ;
#37136 = AXIS2_PLACEMENT_3D ( 'NONE', #9149, #8847, #23559 ) ;
#37137 = CARTESIAN_POINT ( 'NONE',  ( 0.1064266379913941934, 42.67882137217590355, -6.185137063632576648 ) ) ;
#37138 = CARTESIAN_POINT ( 'NONE',  ( 4.962356264823608143, -14.71877352713578269, -39.42833123173278409 ) ) ;
#37139 = CARTESIAN_POINT ( 'NONE',  ( 4.960386119450139297, 1.932332837766398859, 43.71158375621307357 ) ) ;
#37140 = CARTESIAN_POINT ( 'NONE',  ( 0.9780303403264763995, 41.90745447159759607, -0.3238411741276359668 ) ) ;
#37141 = CARTESIAN_POINT ( 'NONE',  ( 0.1129192098497455998, 36.71339784380029414, 24.47607416535571545 ) ) ;
#37142 = EDGE_LOOP ( 'NONE', ( #44849, #20349, #33801, #25993 ) ) ;
#37143 = CARTESIAN_POINT ( 'NONE',  ( -16.69237839429539605, -12.38826022272751359, -1.669401441924114993 ) ) ;
#37144 = CARTESIAN_POINT ( 'NONE',  ( 4.956653778116999476, 43.37017594958085454, -20.77844580450516077 ) ) ;
#37145 = CARTESIAN_POINT ( 'NONE',  ( 0.1156495703730067437, -35.44308041932243469, -26.28176180587048449 ) ) ;
#37146 = CARTESIAN_POINT ( 'NONE',  ( 7.000000000000016875, -56.56854249492331377, -56.56854249492430142 ) ) ;
#37147 = DIRECTION ( 'NONE',  ( -0.1024043820194934229, 0.6159418278945659742, -0.7811075516170014055 ) ) ;
#37148 = CARTESIAN_POINT ( 'NONE',  ( 0.1104177457020373287, 42.75615561261993491, 5.624018123398786706 ) ) ;
#37149 = SHAPE_DEFINITION_REPRESENTATION ( #17805, #10831 ) ;
#37151 = EDGE_CURVE ( 'NONE', #21383, #31710, #37172, .T. ) ;
#37150 = CARTESIAN_POINT ( 'NONE',  ( 0.5837800304671211249, -25.27226667711949304, 39.50379563004109684 ) ) ;
#37152 = CARTESIAN_POINT ( 'NONE',  ( 4.975801465491695552, -35.64402118370979622, 32.01766832630250548 ) ) ;
#37153 = CARTESIAN_POINT ( 'NONE',  ( 0.5997462898726536595, -1.051648045107538954, 49.09628974305014992 ) ) ;
#37154 = EDGE_CURVE ( 'NONE', #59171, #49382, #34169, .T. ) ;
#37156 = ORIENTED_EDGE ( 'NONE', *, *, #36692, .F. ) ;
#37155 = LINE ( 'NONE', #23650, #39381 ) ;
#37157 = ORIENTED_EDGE ( 'NONE', *, *, #52462, .F. ) ;
#37158 = CARTESIAN_POINT ( 'NONE',  ( 0.1158516988532803244, -6.993612654201856849, 43.56640380930912215 ) ) ;
#37159 = CARTESIAN_POINT ( 'NONE',  ( 0.8554163680231738898, -14.77070554666880753, 44.53124443315532233 ) ) ;
#37160 = EDGE_CURVE ( 'NONE', #19013, #3214, #11757, .T. ) ;
#37161 = FACE_OUTER_BOUND ( 'NONE', #1441, .T. ) ;
#37162 = VERTEX_POINT ( 'NONE', #35196 ) ;
#37163 = CARTESIAN_POINT ( 'NONE',  ( 0.5834584762367753807, 22.37749980484480972, 41.21266178612297182 ) ) ;
#37164 = CARTESIAN_POINT ( 'NONE',  ( -6.057079549204054558, -6.658663215492206078, 18.06912934489068334 ) ) ;
#37165 = CARTESIAN_POINT ( 'NONE',  ( 4.975801465491695552, 42.71626295676264817, -21.70134120755155394 ) ) ;
#37166 = ORIENTED_EDGE ( 'NONE', *, *, #17908, .T. ) ;
#37167 = ORIENTED_EDGE ( 'NONE', *, *, #48749, .F. ) ;
#37168 = CARTESIAN_POINT ( 'NONE',  ( 0.9787284016396597952, 24.70838012762134284, -33.85013959199871181 ) ) ;
#37169 = FACE_OUTER_BOUND ( 'NONE', #10659, .T. ) ;
#37170 = CARTESIAN_POINT ( 'NONE',  ( -2.569797478183790229, 12.89088113963436122, -6.924386868080713242 ) ) ;
#37171 = CARTESIAN_POINT ( 'NONE',  ( 2.009741617377216460, -44.01846488356086695, 1.370703074251920173 ) ) ;
#37172 = B_SPLINE_CURVE_WITH_KNOTS ( 'NONE', 3,
 ( #25153, #43060, #98, #57411, #14549, #33652 ),
 .UNSPECIFIED., .F., .F.,
 ( 4, 2, 4 ),
 ( 1.870559545977334001E-17, 0.0002293319059085101167, 0.0004586638118170015309 ),
 .UNSPECIFIED. ) ;
#37173 = CARTESIAN_POINT ( 'NONE',  ( 0.1152339509894530906, -42.73720773065363687, -10.97605420186156344 ) ) ;
#37174 = VECTOR ( 'NONE', #18983, 1000.000000000000227 ) ;
#37175 = AXIS2_PLACEMENT_3D ( 'NONE', #9697, #47928, #4976 ) ;
#37176 = CARTESIAN_POINT ( 'NONE',  ( 0.1158403557922069033, 33.57359527808708322, 28.63134658529052956 ) ) ;
#37177 = VERTEX_POINT ( 'NONE', #58974 ) ;
#37178 = CARTESIAN_POINT ( 'NONE',  ( 0.5987334308729321819, 22.17584284255811156, -43.81546417410061167 ) ) ;
#37179 = CARTESIAN_POINT ( 'NONE',  ( -6.016489644550737204, -18.84320342686341121, -0.004404229197973906322 ) ) ;
#37180 = ORIENTED_EDGE ( 'NONE', *, *, #36518, .T. ) ;
#37181 = CARTESIAN_POINT ( 'NONE',  ( -6.079354080745853928, 3.074405391879146521, 19.00897121715287241 ) ) ;
#37182 = CARTESIAN_POINT ( 'NONE',  ( -5.272380000000000067, 0.000000000000000000, 0.000000000000000000 ) ) ;
#37183 = CARTESIAN_POINT ( 'NONE',  ( 0.9769922540276043676, 4.634276657682153910, -41.65159102538806479 ) ) ;
#37184 = CARTESIAN_POINT ( 'NONE',  ( 0.3676999524040323597, 37.41430475689418245, -23.36921870497780418 ) ) ;
#37185 = VERTEX_POINT ( 'NONE', #36435 ) ;
#37186 = EDGE_LOOP ( 'NONE', ( #50539, #15814, #44164, #29780 ) ) ;
#37187 = CARTESIAN_POINT ( 'NONE',  ( 4.549368137175248350, 35.57418903283115696, -24.02461520945233531 ) ) ;
#37188 = CARTESIAN_POINT ( 'NONE',  ( 0.5809828226811553087, 41.74875432577648837, 23.47450554821725532 ) ) ;
#37189 = CARTESIAN_POINT ( 'NONE',  ( 2.500000000000000000, -1.768423874527825568, -1.020999999999998575 ) ) ;
#37190 =( BOUNDED_SURFACE ( )  B_SPLINE_SURFACE ( 3, 1, ( 
 ( #48688, #38701 ),
 ( #57758, #34602 ),
 ( #15805, #10174 ),
 ( #29269, #43716 ) ),
 .UNSPECIFIED., .F., .F., .F. ) 
 B_SPLINE_SURFACE_WITH_KNOTS ( ( 4, 4 ),
 ( 2, 2 ),
 ( 0.000000000000000000, 1.000000000000000000 ),
 ( 0.000000000000000000, 1.000000000000000000 ),
 .UNSPECIFIED. ) 
 GEOMETRIC_REPRESENTATION_ITEM ( )  RATIONAL_B_SPLINE_SURFACE ( (
 ( 1.000000000000000000, 1.000000000000000000),
 ( 0.9952954269826590483, 0.8620686068821307169),
 ( 0.9952954269826590483, 0.8620686068821307169),
 ( 1.000000000000000000, 1.000000000000000000) ) ) 
 REPRESENTATION_ITEM ( '' )  SURFACE ( )  );
#37191 = EDGE_CURVE ( 'NONE', #51445, #29061, #48356, .T. ) ;
#37192 = EDGE_LOOP ( 'NONE', ( #53692, #41045, #36565, #48691 ) ) ;
#37193 = DIRECTION ( 'NONE',  ( 1.000000000000000000, 0.000000000000000000, 0.000000000000000000 ) ) ;
#37194 = ORIENTED_EDGE ( 'NONE', *, *, #6121, .F. ) ;
#37195 = CARTESIAN_POINT ( 'NONE',  ( 1.112077966505211624, 43.45537587376833955, 7.393282951305692130 ) ) ;
#37196 = CARTESIAN_POINT ( 'NONE',  ( 2.299652685299202748, -12.71149381474350371, -47.35714993383671612 ) ) ;
#37197 = B_SPLINE_CURVE_WITH_KNOTS ( 'NONE', 3,
 ( #60501, #9133, #3491, #51732 ),
 .UNSPECIFIED., .F., .F.,
 ( 4, 4 ),
 ( 0.000000000000000000, 0.004444103432399266161 ),
 .UNSPECIFIED. ) ;
#37198 = CARTESIAN_POINT ( 'NONE',  ( 0.6252788684277238440, 33.51946330543371744, 35.88718310050747107 ) ) ;
#37199 = ORIENTED_EDGE ( 'NONE', *, *, #54052, .T. ) ;
#37200 = CARTESIAN_POINT ( 'NONE',  ( 0.5998501479064699549, -33.64490850298868452, 34.38546660123239462 ) ) ;
#37201 = CARTESIAN_POINT ( 'NONE',  ( 0.1157506346131639274, -27.43836492290452256, 34.55541622033160820 ) ) ;
#37202 = CARTESIAN_POINT ( 'NONE',  ( 1.231276596079887931, -41.87427716283724521, -1.954912557623687652 ) ) ;
#37203 = B_SPLINE_CURVE_WITH_KNOTS ( 'NONE', 3,
 ( #30724, #54510, #50455, #36388, #59220, #7522 ),
 .UNSPECIFIED., .F., .F.,
 ( 4, 2, 4 ),
 ( 1.807478856737577690E-17, 0.0002293319059085094391, 0.0004586638118170007720 ),
 .UNSPECIFIED. ) ;
#37204 = ORIENTED_EDGE ( 'NONE', *, *, #29751, .F. ) ;
#37205 = CARTESIAN_POINT ( 'NONE',  ( 0.5839254288179558383, -18.24509008251443376, -44.28478521851638305 ) ) ;
#37206 = CARTESIAN_POINT ( 'NONE',  ( 5.000000000000012434, -80.00000000000001421, 2.649999999999999467 ) ) ;
#37207 = CARTESIAN_POINT ( 'NONE',  ( 4.956445790444005794, -40.23882117934059011, -24.46171131046819625 ) ) ;
#37208 = CARTESIAN_POINT ( 'NONE',  ( 5.896782393890504181, -19.93422257774826889, 2.674482585249640110 ) ) ;
#37209 = CARTESIAN_POINT ( 'NONE',  ( 0.5807400328401574052, 46.12278621143515522, -12.92266817605966445 ) ) ;
#37210 = VERTEX_POINT ( 'NONE', #16699 ) ;
#37211 = CARTESIAN_POINT ( 'NONE',  ( 0.5809828226811565299, -17.82437196699712700, 44.45562576850595349 ) ) ;
#37212 = CARTESIAN_POINT ( 'NONE',  ( 4.833616638992208614, 38.70560126501828080, 25.31740731790911880 ) ) ;
#37213 = ORIENTED_EDGE ( 'NONE', *, *, #8467, .F. ) ;
#37214 = CARTESIAN_POINT ( 'NONE',  ( 50.00005079999999680, 0.000000000000000000, 0.000000000000000000 ) ) ;
#37215 = CARTESIAN_POINT ( 'NONE',  ( 0.9790724872846771065, -27.08825771237176383, 31.97751560221001554 ) ) ;
#37216 = CARTESIAN_POINT ( 'NONE',  ( 4.833616638992208614, 43.93936707042080059, 14.43699082351728968 ) ) ;
#37217 = CARTESIAN_POINT ( 'NONE',  ( 0.5848930533535030563, 40.25661832390772332, -24.05572205340705594 ) ) ;
#37218 = DIRECTION ( 'NONE',  ( 0.09722883295013597105, 0.4670337431504756887, -0.8788777143619072030 ) ) ;
#37219 = DIRECTION ( 'NONE',  ( -1.558861125776144859E-16, 1.000000000000000000, 0.000000000000000000 ) ) ;
#37220 = CIRCLE ( 'NONE', #47181, 6.866799999999992465 ) ;
#37221 = CARTESIAN_POINT ( 'NONE',  ( 2.000000000000027089, 3.464101615137739731, -5.600000000000000533 ) ) ;
#37223 = EDGE_CURVE ( 'NONE', #29664, #26668, #23731, .T. ) ;
#37222 = CARTESIAN_POINT ( 'NONE',  ( 0.1119898979215351448, 39.50795620750168524, -19.64898736724001083 ) ) ;
#37224 = VECTOR ( 'NONE', #14353, 999.9999999999998863 ) ;
#37225 = B_SPLINE_CURVE_WITH_KNOTS ( 'NONE', 3,
 ( #46181, #60546, #51155, #12055 ),
 .UNSPECIFIED., .F., .F.,
 ( 4, 4 ),
 ( 0.000000000000000000, 0.005013413432710145910 ),
 .UNSPECIFIED. ) ;
#37226 = CARTESIAN_POINT ( 'NONE',  ( 2.648799415243708655, -9.190926635156966285, -48.16683849783750304 ) ) ;
#37227 = CARTESIAN_POINT ( 'NONE',  ( 4.694002226626920127, -4.720386398733717570, -45.34316622924322360 ) ) ;
#37228 = EDGE_CURVE ( 'NONE', #1703, #20061, #20735, .T. ) ;
#37229 = CARTESIAN_POINT ( 'NONE',  ( 0.1100247026804066219, -5.797046384220175597, 42.73303500775676866 ) ) ;
#37230 = ORIENTED_EDGE ( 'NONE', *, *, #25088, .F. ) ;
#37231 = DIRECTION ( 'NONE',  ( -0.07500201931887527651, -0.8838330717251269286, 0.4617507968840091626 ) ) ;
#37232 = CARTESIAN_POINT ( 'NONE',  ( 3.660087539126834599, 1.881558488211524383, 48.00143792263125420 ) ) ;
#37233 = ADVANCED_FACE ( 'NONE', ( #6955 ), #26087, .F. ) ;
#37234 = FACE_OUTER_BOUND ( 'NONE', #48262, .T. ) ;
#37235 = CARTESIAN_POINT ( 'NONE',  ( 0.7056313189692768884, 23.27565847123662124, 40.71845241027597240 ) ) ;
#37236 = CARTESIAN_POINT ( 'NONE',  ( 4.956445790443998689, -10.39006634428300835, 45.93021414603936847 ) ) ;
#37237 = CARTESIAN_POINT ( 'NONE',  ( 0.3676999524040366896, 33.04872056100262512, -29.21870381457057775 ) ) ;
#37238 = EDGE_LOOP ( 'NONE', ( #23664, #43819, #45440, #31140 ) ) ;
#37239 = CARTESIAN_POINT ( 'NONE',  ( 0.9756008150404608115, 10.96816689273754442, -41.48296819691537252 ) ) ;
#37240 = ADVANCED_FACE ( 'NONE', ( #8830 ), #45130, .F. ) ;
#37241 = FACE_OUTER_BOUND ( 'NONE', #22231, .T. ) ;
#37242 = CARTESIAN_POINT ( 'NONE',  ( 2.009741617377216460, 28.57895180276246805, -33.50742591543588844 ) ) ;
#37243 = CARTESIAN_POINT ( 'NONE',  ( -18.90529782703537975, -7.774448652089772871, -1.887028486091764101 ) ) ;
#37244 = ORIENTED_EDGE ( 'NONE', *, *, #51218, .F. ) ;
#37245 = ADVANCED_FACE ( 'NONE', ( #56739 ), #29532, .F. ) ;
#37246 = DIRECTION ( 'NONE',  ( -1.000000000000000000, -0.000000000000000000, -0.000000000000000000 ) ) ;
#37247 = CARTESIAN_POINT ( 'NONE',  ( 0.6017666602106489515, 23.75081624637622113, -41.83584962818292752 ) ) ;
#37248 = EDGE_LOOP ( 'NONE', ( #7498, #10674, #41885, #10182 ) ) ;
#37249 = CARTESIAN_POINT ( 'NONE',  ( 2.879087469061462734, -26.05926906996272763, 35.45442387520437677 ) ) ;
#37250 = VERTEX_POINT ( 'NONE', #18244 ) ;
#37251 = CARTESIAN_POINT ( 'NONE',  ( 0.5839879882104919151, -5.421203860810959572E-16, -47.89596766822081975 ) ) ;
#37252 = CARTESIAN_POINT ( 'NONE',  ( -0.3263565795980851170, 4.430380094434251959, -5.351519936624993257 ) ) ;
#37253 = VERTEX_POINT ( 'NONE', #56430 ) ;
#37254 = CARTESIAN_POINT ( 'NONE',  ( 5.959828726073459926, -12.49879082830580579, 16.28130559351243178 ) ) ;
#37255 = CARTESIAN_POINT ( 'NONE',  ( -6.057079549204054558, -14.65763772032089740, -12.48939100034763250 ) ) ;
#37256 = ORIENTED_EDGE ( 'NONE', *, *, #52275, .F. ) ;
#37257 = CARTESIAN_POINT ( 'NONE',  ( 0.6253024248130445439, -43.12021026963351034, 23.49663153986622177 ) ) ;
#37258 = B_SPLINE_CURVE_WITH_KNOTS ( 'NONE', 3,
 ( #35602, #44693, #6415, #39690 ),
 .UNSPECIFIED., .F., .F.,
 ( 4, 4 ),
 ( 6.254634441385501517E-18, 0.004566006591234648970 ),
 .UNSPECIFIED. ) ;
#37259 = VECTOR ( 'NONE', #36756, 999.9999999999998863 ) ;
#37260 = ORIENTED_EDGE ( 'NONE', *, *, #34873, .F. ) ;
#37261 = CARTESIAN_POINT ( 'NONE',  ( 0.6008123274975392114, -7.407413473420949579, -48.54569781960332620 ) ) ;
#37262 = ORIENTED_EDGE ( 'NONE', *, *, #38801, .F. ) ;
#37263 = FACE_OUTER_BOUND ( 'NONE', #32310, .T. ) ;
#37264 =( BOUNDED_SURFACE ( )  B_SPLINE_SURFACE ( 3, 1, ( 
 ( #19336, #29036 ),
 ( #28107, #23108 ),
 ( #57199, #52833 ),
 ( #47224, #4271 ) ),
 .UNSPECIFIED., .F., .F., .F. ) 
 B_SPLINE_SURFACE_WITH_KNOTS ( ( 4, 4 ),
 ( 2, 2 ),
 ( 0.000000000000000000, 1.000000000000000000 ),
 ( 0.000000000000000000, 1.000000000000000000 ),
 .UNSPECIFIED. ) 
 GEOMETRIC_REPRESENTATION_ITEM ( )  RATIONAL_B_SPLINE_SURFACE ( (
 ( 1.000000000000000000, 1.000000000000000000),
 ( 0.7211978278499970862, 0.9934217856018976445),
 ( 0.7211978278499970862, 0.9934217856018976445),
 ( 1.000000000000000000, 1.000000000000000000) ) ) 
 REPRESENTATION_ITEM ( '' )  SURFACE ( )  );
#37265 = AXIS2_PLACEMENT_3D ( 'NONE', #26611, #55411, #31943 ) ;
#37266 = ADVANCED_FACE ( 'NONE', ( #51114 ), #59910, .F. ) ;
#37267 = ORIENTED_EDGE ( 'NONE', *, *, #1450, .T. ) ;
#37268 = ORIENTED_EDGE ( 'NONE', *, *, #43607, .T. ) ;
#37269 = DIRECTION ( 'NONE',  ( 0.000000000000000000, 0.000000000000000000, 1.000000000000000000 ) ) ;
#37270 = CARTESIAN_POINT ( 'NONE',  ( 0.6023143664670691511, -34.20175727332151894, 33.83148565876871317 ) ) ;
#37271 = CARTESIAN_POINT ( 'NONE',  ( 0.5809828226811617480, 28.72298383114487663, 38.32755012159156394 ) ) ;
#37272 = FACE_OUTER_BOUND ( 'NONE', #25904, .T. ) ;
#37273 = CARTESIAN_POINT ( 'NONE',  ( 4.975610109902397937, 42.33317580307119954, 24.50207406657730047 ) ) ;
#37274 = ORIENTED_EDGE ( 'NONE', *, *, #37047, .T. ) ;
#37275 = CARTESIAN_POINT ( 'NONE',  ( 2.359973842542475886, 5.726946755930971911, 43.65017726753503524 ) ) ;
#37276 = CARTESIAN_POINT ( 'NONE',  ( 5.910764540655177868, 8.451874527002114945, 18.25012480639449564 ) ) ;
#37277 = CARTESIAN_POINT ( 'NONE',  ( 0.5263152470540364281, 0.000000000000000000, 0.000000000000000000 ) ) ;
#37278 = VERTEX_POINT ( 'NONE', #12940 ) ;
#37279 = ORIENTED_EDGE ( 'NONE', *, *, #47735, .F. ) ;
#37280 = CARTESIAN_POINT ( 'NONE',  ( 0.1103310638050662290, -21.49083802119874775, -37.38800124003704184 ) ) ;
#37281 = CARTESIAN_POINT ( 'NONE',  ( 1.231276596079887931, 8.892602616354244205, -40.96581977363174332 ) ) ;
#37282 = CARTESIAN_POINT ( 'NONE',  ( 0.8551540677456739292, 13.28067116677265957, -46.03951182599413983 ) ) ;
#37283 = CARTESIAN_POINT ( 'NONE',  ( 0.1104177457020373010, -34.20994892372227270, 26.25638621857933686 ) ) ;
#37284 = CARTESIAN_POINT ( 'NONE',  ( 3.727782113643637540, -33.91244348195018432, 27.97720416677674393 ) ) ;
#37285 = ORIENTED_EDGE ( 'NONE', *, *, #47477, .T. ) ;
#37286 = CARTESIAN_POINT ( 'NONE',  ( 4.960156602257184133, 44.12083041402459571, 14.43621227656543304 ) ) ;
#37287 = CARTESIAN_POINT ( 'NONE',  ( 3.678834586032790011, 31.53396450442054544, 37.47294293570093515 ) ) ;
#37288 = CARTESIAN_POINT ( 'NONE',  ( 0.7413678028165013867, 43.09507536412139217, -9.343477464570760560 ) ) ;
#37289 = CARTESIAN_POINT ( 'NONE',  ( 3.559346040607745287, -39.27867776338149497, -19.76400148508467325 ) ) ;
#37290 = CARTESIAN_POINT ( 'NONE',  ( 3.221118495291109163, -43.34303269931057656, 7.492859006296892943 ) ) ;
#37291 = CARTESIAN_POINT ( 'NONE',  ( 4.553261556744875094, 0.000000000000000000, 0.000000000000000000 ) ) ;
#37292 = ORIENTED_EDGE ( 'NONE', *, *, #25474, .F. ) ;
#37293 = CARTESIAN_POINT ( 'NONE',  ( 0.3622758884714600280, -15.73321244754826509, -40.13994584881776007 ) ) ;
#37294 = CARTESIAN_POINT ( 'NONE',  ( 0.5806925824938499181, 28.25565086187788921, -37.42780459384738379 ) ) ;
#37295 = ADVANCED_FACE ( 'NONE', ( #22946 ), #35974, .F. ) ;
#37296 = CARTESIAN_POINT ( 'NONE',  ( 5.959547316686252039, -12.49238070347988483, 16.28624005235077732 ) ) ;
#37297 = CARTESIAN_POINT ( 'NONE',  ( 5.959547316686252039, -7.858107265727872992, 18.96183906913529782 ) ) ;
#37298 = EDGE_CURVE ( 'NONE', #42435, #44157, #31949, .T. ) ;
#37299 = DIRECTION ( 'NONE',  ( -1.000000000000000000, -1.836909530733573776E-16, 2.465190328815655050E-32 ) ) ;
#37300 = CARTESIAN_POINT ( 'NONE',  ( 0.6064515330803589288, -8.500244729551798883, -46.12027943947015274 ) ) ;
#37301 = VECTOR ( 'NONE', #24731, 999.9999999999997726 ) ;
#37302 = CARTESIAN_POINT ( 'NONE',  ( 4.833616638992205949, 38.70560126501862896, -25.31740731790855747 ) ) ;
#37303 = VECTOR ( 'NONE', #4398, 1000.000000000000000 ) ;
#37304 = CARTESIAN_POINT ( 'NONE',  ( -90.00000000000000000, 0.000000000000000000, 0.000000000000000000 ) ) ;
#37305 = ORIENTED_EDGE ( 'NONE', *, *, #39231, .T. ) ;
#37306 = CARTESIAN_POINT ( 'NONE',  ( 1.231276596079887931, 5.037240371905710390, 41.61613846158375196 ) ) ;
#37307 = CARTESIAN_POINT ( 'NONE',  ( 0.9762797500689124330, 19.69530149098661909, 36.99215976885973589 ) ) ;
#37308 = LINE ( 'NONE', #22585, #27188 ) ;
#37309 = DIRECTION ( 'NONE',  ( -1.000000000000000000, -3.552713678800500929E-15, 0.000000000000000000 ) ) ;
#37310 = ORIENTED_EDGE ( 'NONE', *, *, #37571, .F. ) ;
#37311 = EDGE_CURVE ( 'NONE', #35778, #43148, #43168, .T. ) ;
#37312 = DIRECTION ( 'NONE',  ( -1.000000000000000000, -0.000000000000000000, -0.000000000000000000 ) ) ;
#37313 = CARTESIAN_POINT ( 'NONE',  ( -49.49999999999975842, 4.769696007084736067, -1.500000000000002220 ) ) ;
#37314 = B_SPLINE_CURVE_WITH_KNOTS ( 'NONE', 3,
 ( #3666, #22799, #41930, #56298 ),
 .UNSPECIFIED., .F., .F.,
 ( 4, 4 ),
 ( 0.000000000000000000, 0.005014147105413703856 ),
 .UNSPECIFIED. ) ;
#37315 = ORIENTED_EDGE ( 'NONE', *, *, #2639, .T. ) ;
#37316 = CARTESIAN_POINT ( 'NONE',  ( 4.960156602257182357, -2.524999074837246837, -46.35381625054459676 ) ) ;
#37317 = AXIS2_PLACEMENT_3D ( 'NONE', #34461, #29126, #52926 ) ;
#37318 = CARTESIAN_POINT ( 'NONE',  ( -6.016104459813374383, 18.68131780085931837, 2.464823636987509392 ) ) ;
#37319 = CARTESIAN_POINT ( 'NONE',  ( 1.231276596079881047, 25.54232633153377208, -33.23952972879584422 ) ) ;
#37320 = ORIENTED_EDGE ( 'NONE', *, *, #49016, .F. ) ;
#37321 = CARTESIAN_POINT ( 'NONE',  ( 0.6027935024548037868, 29.14731236071017051, 38.27223087442856553 ) ) ;
#37322 = EDGE_LOOP ( 'NONE', ( #25150, #37910, #22658, #13223 ) ) ;
#37323 = VERTEX_POINT ( 'NONE', #39764 ) ;
#37324 = CARTESIAN_POINT ( 'NONE',  ( 5.894904586330512508, 8.465111963867505196, -18.24476065890780418 ) ) ;
#37325 = CARTESIAN_POINT ( 'NONE',  ( 2.299652685299202748, 47.86636889862017341, 10.63449356195967432 ) ) ;
#37326 = VERTEX_POINT ( 'NONE', #58818 ) ;
#37327 = PRODUCT_DEFINITION_SHAPE ( 'NONE', 'NONE',  #36005 ) ;
#37328 = ORIENTED_EDGE ( 'NONE', *, *, #15447, .F. ) ;
#37329 = CARTESIAN_POINT ( 'NONE',  ( 0.5839879882104920261, 5.827794150371782279E-15, 47.89596766822081264 ) ) ;
#37330 = CARTESIAN_POINT ( 'NONE',  ( 0.5809828226811553087, 12.92184523170202937, 46.11980934799343856 ) ) ;
#37331 = CARTESIAN_POINT ( 'NONE',  ( 0.7948878604505656975, 40.66950417720534006, -27.50800024136056976 ) ) ;
#37332 =( BOUNDED_SURFACE ( )  B_SPLINE_SURFACE ( 3, 1, ( 
 ( #4428, #42695 ),
 ( #60536, #37382 ),
 ( #61757, #14195 ),
 ( #17647, #37085 ) ),
 .UNSPECIFIED., .F., .F., .F. ) 
 B_SPLINE_SURFACE_WITH_KNOTS ( ( 4, 4 ),
 ( 2, 2 ),
 ( 0.000000000000000000, 1.000000000000000000 ),
 ( 0.000000000000000000, 1.000000000000000000 ),
 .UNSPECIFIED. ) 
 GEOMETRIC_REPRESENTATION_ITEM ( )  RATIONAL_B_SPLINE_SURFACE ( (
 ( 1.000000000000000000, 1.000000000000000000),
 ( 0.9953485035131437453, 0.8621029689291515030),
 ( 0.9953485035131437453, 0.8621029689291515030),
 ( 1.000000000000000000, 1.000000000000000000) ) ) 
 REPRESENTATION_ITEM ( '' )  SURFACE ( )  );
#37333 = VERTEX_POINT ( 'NONE', #39448 ) ;
#37334 = CARTESIAN_POINT ( 'NONE',  ( 5.896782393890504181, 20.06834277495334362, -1.337050913387380691 ) ) ;
#37335 = FACE_OUTER_BOUND ( 'NONE', #50102, .T. ) ;
#37336 = CARTESIAN_POINT ( 'NONE',  ( 1.834102595619085285, -37.72341624877798694, 22.74074781925867939 ) ) ;
#37337 = CARTESIAN_POINT ( 'NONE',  ( 0.6252788684277205133, 27.52863421382489406, -40.66470987840802565 ) ) ;
#37338 = VERTEX_POINT ( 'NONE', #15633 ) ;
#37339 = CARTESIAN_POINT ( 'NONE',  ( 0.5834872094924158370, -33.70665904794267220, -34.02770606800797282 ) ) ;
#37340 = CARTESIAN_POINT ( 'NONE',  ( 0.5998501479064708430, 29.69975237324613460, -37.84527566984826308 ) ) ;
#37341 = ORIENTED_EDGE ( 'NONE', *, *, #21081, .F. ) ;
#37342 = AXIS2_PLACEMENT_3D ( 'NONE', #19356, #5828, #44116 ) ;
#37343 = CARTESIAN_POINT ( 'NONE',  ( 4.975801465491695552, -2.564218696447830403, 47.84403947906839250 ) ) ;
#37344 = EDGE_CURVE ( 'NONE', #37128, #37711, #13690, .T. ) ;
#37345 = ORIENTED_EDGE ( 'NONE', *, *, #20303, .T. ) ;
#37346 = CARTESIAN_POINT ( 'NONE',  ( 0.1149546198390367369, -12.81688777603463514, 42.22172370663890462 ) ) ;
#37347 = CARTESIAN_POINT ( 'NONE',  ( 0.5835226383429296115, 10.69419208715441272, -45.66045039362849423 ) ) ;
#37348 = EDGE_LOOP ( 'NONE', ( #32800, #51309, #2292, #43294, #36808, #53375 ) ) ;
#37349 = CARTESIAN_POINT ( 'NONE',  ( 5.896782393890504181, -17.30835043929350192, -10.24436879210333906 ) ) ;
#37350 = CARTESIAN_POINT ( 'NONE',  ( -6.063463321072278589, 7.809047921946556947, -17.60225051043791922 ) ) ;
#37351 = ADVANCED_FACE ( 'NONE', ( #53801, #54111 ), #10935, .T. ) ;
#37352 = CARTESIAN_POINT ( 'NONE',  ( 4.975610109902397937, 0.000000000000000000, 0.000000000000000000 ) ) ;
#37353 = CARTESIAN_POINT ( 'NONE',  ( 0.5837157313716041518, -1.476039657514138348, -46.87278923332241476 ) ) ;
#37354 =( BOUNDED_SURFACE ( )  B_SPLINE_SURFACE ( 3, 1, ( 
 ( #17037, #54908 ),
 ( #36151, #60223 ),
 ( #21104, #26109 ),
 ( #30798, #49920 ) ),
 .UNSPECIFIED., .F., .F., .F. ) 
 B_SPLINE_SURFACE_WITH_KNOTS ( ( 4, 4 ),
 ( 2, 2 ),
 ( 0.000000000000000000, 1.000000000000000000 ),
 ( 0.000000000000000000, 1.000000000000000000 ),
 .UNSPECIFIED. ) 
 GEOMETRIC_REPRESENTATION_ITEM ( )  RATIONAL_B_SPLINE_SURFACE ( (
 ( 1.000000000000000000, 1.000000000000000000),
 ( 0.7223157951917476005, 0.9931996967497186413),
 ( 0.7223157951917476005, 0.9931996967497186413),
 ( 1.000000000000000000, 1.000000000000000000) ) ) 
 REPRESENTATION_ITEM ( '' )  SURFACE ( )  );
#37355 = ORIENTED_EDGE ( 'NONE', *, *, #32777, .F. ) ;
#37356 = CARTESIAN_POINT ( 'NONE',  ( 0.7056759521544992975, 45.00498525904872338, 13.20227749101629477 ) ) ;
#37357 = CARTESIAN_POINT ( 'NONE',  ( 0.5782707292762442330, 46.89575936232449749, 0.7239527184646523672 ) ) ;
#37358 =( BOUNDED_SURFACE ( )  B_SPLINE_SURFACE ( 3, 1, ( 
 ( #59834, #45457 ),
 ( #16948, #50735 ),
 ( #36061, #35129 ),
 ( #55125, #2810 ) ),
 .UNSPECIFIED., .F., .F., .F. ) 
 B_SPLINE_SURFACE_WITH_KNOTS ( ( 4, 4 ),
 ( 2, 2 ),
 ( 0.000000000000000000, 1.000000000000000000 ),
 ( 0.000000000000000000, 1.000000000000000000 ),
 .UNSPECIFIED. ) 
 GEOMETRIC_REPRESENTATION_ITEM ( )  RATIONAL_B_SPLINE_SURFACE ( (
 ( 1.000000000000000000, 1.000000000000000000),
 ( 0.9953040768229005630, 0.8617119497784937465),
 ( 0.9953040768229005630, 0.8617119497784937465),
 ( 1.000000000000000000, 1.000000000000000000) ) ) 
 REPRESENTATION_ITEM ( '' )  SURFACE ( )  );
#37359 = FACE_OUTER_BOUND ( 'NONE', #52191, .T. ) ;
#37360 = CARTESIAN_POINT ( 'NONE',  ( 0.5839879882012674051, -44.25011577017258446, -18.32896541547120250 ) ) ;
#37361 = AXIS2_PLACEMENT_3D ( 'NONE', #20802, #436, #10479 ) ;
#37362 = CARTESIAN_POINT ( 'NONE',  ( 4.549368137175248350, 0.000000000000000000, 0.000000000000000000 ) ) ;
#37363 = CARTESIAN_POINT ( 'NONE',  ( 4.553261556744875094, 0.000000000000000000, 0.000000000000000000 ) ) ;
#37364 = CARTESIAN_POINT ( 'NONE',  ( 1.154321713695927176, 39.95809834491024759, -15.65787958845375449 ) ) ;
#37365 = EDGE_CURVE ( 'NONE', #59890, #22653, #28937, .T. ) ;
#37366 = CARTESIAN_POINT ( 'NONE',  ( 0.8557997880470606944, -24.73961900479280374, 41.02602466100771039 ) ) ;
#37367 = CARTESIAN_POINT ( 'NONE',  ( 0.9791128995231617171, -12.41164548084656083, 40.02859591222185998 ) ) ;
#37368 = EDGE_CURVE ( 'NONE', #13900, #29507, #46692, .T. ) ;
#37369 = CARTESIAN_POINT ( 'NONE',  ( 3.238018933889920792, 4.556392162264823575, -12.59550645394239865 ) ) ;
#37370 = CARTESIAN_POINT ( 'NONE',  ( -7.955290792335435235, 8.751533712787090025, -2.059410264200305690E-15 ) ) ;
#37371 = CARTESIAN_POINT ( 'NONE',  ( 0.7056759521544981872, 33.20631110585615176, -33.12234490277042909 ) ) ;
#37372 = DIRECTION ( 'NONE',  ( -1.000000000000000000, -0.000000000000000000, -0.000000000000000000 ) ) ;
#37373 = CARTESIAN_POINT ( 'NONE',  ( 0.5809828226811553087, 24.41822904836923058, 41.20389530892317254 ) ) ;
#37374 = CARTESIAN_POINT ( 'NONE',  ( 0.3676999524040323597, -31.10876963919482563, -31.27610965031216139 ) ) ;
#37375 = EDGE_CURVE ( 'NONE', #26144, #52281, #27332, .T. ) ;
#37376 = CARTESIAN_POINT ( 'NONE',  ( 0.8551540677456715978, 34.52115452272929730, 33.23105123575911790 ) ) ;
#37377 = CARTESIAN_POINT ( 'NONE',  ( 0.5817216825391118284, 45.10732437693867070, -12.82825942055636936 ) ) ;
#37378 = DIRECTION ( 'NONE',  ( 0.000000000000000000, 0.000000000000000000, -1.000000000000000000 ) ) ;
#37380 = VERTEX_POINT ( 'NONE', #48822 ) ;
#37379 = CARTESIAN_POINT ( 'NONE',  ( 0.9747592971366246806, 39.76507150545830171, 16.12077520819463672 ) ) ;
#37381 = VERTEX_POINT ( 'NONE', #30323 ) ;
#37382 = CARTESIAN_POINT ( 'NONE',  ( 0.7044674535453004927, -34.68719619958527289, 34.76494128604828404 ) ) ;
#37383 = CARTESIAN_POINT ( 'NONE',  ( 3.270143674763207553, 1.514386915940791445, -13.60381564321232695 ) ) ;
#37384 = DIRECTION ( 'NONE',  ( 1.000000000000000000, 0.000000000000000000, 0.000000000000000000 ) ) ;
#37385 = ORIENTED_EDGE ( 'NONE', *, *, #51249, .F. ) ;
#37386 = EDGE_CURVE ( 'NONE', #21039, #24195, #47542, .T. ) ;
#37387 = EDGE_LOOP ( 'NONE', ( #44431, #14461, #22318, #12771 ) ) ;
#37388 = CARTESIAN_POINT ( 'NONE',  ( 0.1368894036331306796, -23.41594797177933174, -37.39725533386449996 ) ) ;
#37389 = CARTESIAN_POINT ( 'NONE',  ( 0.5806925824938502512, 16.34374012233117313, -43.95571090492413191 ) ) ;
#37390 = CIRCLE ( 'NONE', #12390, 4.000000000000000000 ) ;
#37391 = UNCERTAINTY_MEASURE_WITH_UNIT (LENGTH_MEASURE( 1.000000000000000082E-05 ), #22795, 'distance_accuracy_value', 'NONE');
#37392 = ORIENTED_EDGE ( 'NONE', *, *, #16062, .T. ) ;
#37393 = ORIENTED_EDGE ( 'NONE', *, *, #20936, .T. ) ;
#37394 = CARTESIAN_POINT ( 'NONE',  ( 0.9741495583595169983, -10.72301204857627255, -41.54695848110009848 ) ) ;
#37395 = CARTESIAN_POINT ( 'NONE',  ( 0.5797568665920712627, 4.067664388277952625, -46.71915469083538142 ) ) ;
#37396 = CARTESIAN_POINT ( 'NONE',  ( 3.661933894777893439, 29.39589352174664683, -36.72209973585098908 ) ) ;
#37397 = ORIENTED_EDGE ( 'NONE', *, *, #14734, .T. ) ;
#37398 = VERTEX_POINT ( 'NONE', #10619 ) ;
#37399 = CARTESIAN_POINT ( 'NONE',  ( 0.5832366564991503521, -12.65934068133952195, -46.19265750221184419 ) ) ;
#37400 = VERTEX_POINT ( 'NONE', #49431 ) ;
#37401 = CARTESIAN_POINT ( 'NONE',  ( 2.526552050251863246, 31.23611603144905402, -29.52128340070568413 ) ) ;
#37402 = CARTESIAN_POINT ( 'NONE',  ( 4.834790513006553603, 18.70372717509320637, 43.39078163255486942 ) ) ;
#37403 = AXIS2_PLACEMENT_3D ( 'NONE', #40432, #15995, #49183 ) ;
#37404 = B_SPLINE_CURVE_WITH_KNOTS ( 'NONE', 3,
 ( #46599, #17778, #2728, #27472, #31253, #60060 ),
 .UNSPECIFIED., .F., .F.,
 ( 4, 2, 4 ),
 ( 1.518576772339270681E-16, 0.0002445252820015215208, 0.0004890505640028912533 ),
 .UNSPECIFIED. ) ;
#37405 = CARTESIAN_POINT ( 'NONE',  ( 0.1104177457020373149, -30.49705356371285347, -30.49013195371445306 ) ) ;
#37406 = ORIENTED_EDGE ( 'NONE', *, *, #52338, .T. ) ;
#37407 = CARTESIAN_POINT ( 'NONE',  ( 0.1081432562775998391, 0.4234896101211546027, -43.12249629849792854 ) ) ;
#37408 = VERTEX_POINT ( 'NONE', #58202 ) ;
#37409 = ORIENTED_EDGE ( 'NONE', *, *, #20822, .T. ) ;
#37410 = EDGE_CURVE ( 'NONE', #32248, #47641, #25897, .T. ) ;
#37411 = DIRECTION ( 'NONE',  ( -0.1011922191286467460, -0.2338987173090957550, 0.9669806227784399910 ) ) ;
#37412 = ORIENTED_EDGE ( 'NONE', *, *, #51566, .F. ) ;
#37413 = CARTESIAN_POINT ( 'NONE',  ( 4.390527457369402420, 35.01638428076268639, 26.53371757840531231 ) ) ;
#37414 = DIRECTION ( 'NONE',  ( -1.000000000000000000, -0.000000000000000000, -0.000000000000000000 ) ) ;
#37415 = CARTESIAN_POINT ( 'NONE',  ( 0.6023142530420679819, 33.83147280953687641, -34.20176999054672962 ) ) ;
#37416 = CARTESIAN_POINT ( 'NONE',  ( 0.5806925824938494740, -38.35106547415225009, 26.98922265165951018 ) ) ;
#37417 = LINE ( 'NONE', #46501, #20402 ) ;
#37418 = EDGE_CURVE ( 'NONE', #15516, #36162, #25629, .T. ) ;
#37419 = ORIENTED_EDGE ( 'NONE', *, *, #55351, .F. ) ;
#37420 = CARTESIAN_POINT ( 'NONE',  ( 4.956445790444004018, -43.56224489968113289, 17.88487823385560205 ) ) ;
#37421 = CARTESIAN_POINT ( 'NONE',  ( -2.569797478183783568, 14.44232325624826707, -2.353985772484601835 ) ) ;
#37422 = EDGE_CURVE ( 'NONE', #16278, #21005, #36723, .T. ) ;
#37423 = CARTESIAN_POINT ( 'NONE',  ( 0.1104177457020373287, 39.83992599038884919, -16.50753524010258033 ) ) ;
#37424 = ORIENTED_EDGE ( 'NONE', *, *, #58120, .T. ) ;
#37425 = CARTESIAN_POINT ( 'NONE',  ( 0.8751705887134423323, -7.160166390004656378, 47.55935879196458416 ) ) ;
#37426 = CARTESIAN_POINT ( 'NONE',  ( 0.1119898979215350893, 30.07795596614133160, 32.28432859996768656 ) ) ;
#37427 = EDGE_CURVE ( 'NONE', #13696, #6658, #45081, .T. ) ;
#37428 = DIRECTION ( 'NONE',  ( 1.000000000000000000, -0.000000000000000000, -0.000000000000000000 ) ) ;
#37429 = CARTESIAN_POINT ( 'NONE',  ( 0.5998501479064708430, 46.60114184914316837, -11.94461217097420658 ) ) ;
#37430 = EDGE_CURVE ( 'NONE', #39646, #13518, #25705, .T. ) ;
#37431 = ORIENTED_EDGE ( 'NONE', *, *, #13375, .F. ) ;
#37432 = ORIENTED_EDGE ( 'NONE', *, *, #21734, .T. ) ;
#37433 = CARTESIAN_POINT ( 'NONE',  ( -6.057079549204054558, 17.85280408805613561, 7.218629876453331207 ) ) ;
#37434 = CARTESIAN_POINT ( 'NONE',  ( 0.8760168074887076939, -37.61398439004553751, 29.98565522133283068 ) ) ;
#37435 = CYLINDRICAL_SURFACE ( 'NONE', #53820, 9.500000000000000000 ) ;
#37436 = B_SPLINE_CURVE_WITH_KNOTS ( 'NONE', 3,
 ( #58848, #21272, #11899, #40405 ),
 .UNSPECIFIED., .F., .F.,
 ( 4, 4 ),
 ( 1.843143693225357538E-18, 0.004444878191957690391 ),
 .UNSPECIFIED. ) ;
#37437 = VECTOR ( 'NONE', #15791, 1000.000000000000000 ) ;
#37438 = CARTESIAN_POINT ( 'NONE',  ( 0.5832655196449144652, -30.10317133800721834, -35.95878555190522263 ) ) ;
#37439 = CARTESIAN_POINT ( 'NONE',  ( 0.9730545539215883499, -42.60426903087357431, 5.099196237954729760 ) ) ;
#37440 =( BOUNDED_SURFACE ( )  B_SPLINE_SURFACE ( 3, 1, ( 
 ( #10860, #1420 ),
 ( #59057, #15866 ),
 ( #39688, #30247 ),
 ( #49984, #54044 ) ),
 .UNSPECIFIED., .F., .F., .F. ) 
 B_SPLINE_SURFACE_WITH_KNOTS ( ( 4, 4 ),
 ( 2, 2 ),
 ( 0.000000000000000000, 1.000000000000000000 ),
 ( 0.000000000000000000, 1.000000000000000000 ),
 .UNSPECIFIED. ) 
 GEOMETRIC_REPRESENTATION_ITEM ( )  RATIONAL_B_SPLINE_SURFACE ( (
 ( 1.000000000000000000, 1.000000000000000000),
 ( 0.9754377213608244057, 0.9999580625633939235),
 ( 0.9754377213608244057, 0.9999580625633939235),
 ( 1.000000000000000000, 1.000000000000000000) ) ) 
 REPRESENTATION_ITEM ( '' )  SURFACE ( )  );
#37441 = FILL_AREA_STYLE_COLOUR ( '', #7338 ) ;
#37442 = CARTESIAN_POINT ( 'NONE',  ( 0.9745511491811756910, 42.90705396078542577, 0.3405614984922070154 ) ) ;
#37443 = LINE ( 'NONE', #106, #59794 ) ;
#37444 = CARTESIAN_POINT ( 'NONE',  ( 0.8557997880470697982, -37.44587306708118035, 29.88293891557457371 ) ) ;
#37445 = ADVANCED_FACE ( 'NONE', ( #48510 ), #51480, .F. ) ;
#37446 =( BOUNDED_SURFACE ( )  B_SPLINE_SURFACE ( 3, 1, ( 
 ( #42641, #9103 ),
 ( #47952, #56704 ),
 ( #43269, #38566 ),
 ( #47329, #61701 ) ),
 .UNSPECIFIED., .F., .F., .F. ) 
 B_SPLINE_SURFACE_WITH_KNOTS ( ( 4, 4 ),
 ( 2, 2 ),
 ( 0.000000000000000000, 1.000000000000000000 ),
 ( 0.000000000000000000, 1.000000000000000000 ),
 .UNSPECIFIED. ) 
 GEOMETRIC_REPRESENTATION_ITEM ( )  RATIONAL_B_SPLINE_SURFACE ( (
 ( 1.000000000000000000, 1.000000000000000000),
 ( 0.9953485035131437453, 0.8621029689291515030),
 ( 0.9953485035131437453, 0.8621029689291515030),
 ( 1.000000000000000000, 1.000000000000000000) ) ) 
 REPRESENTATION_ITEM ( '' )  SURFACE ( )  );
#37447 = CARTESIAN_POINT ( 'NONE',  ( 0.1119899015040008994, 36.67093986234336001, 24.53983451054433118 ) ) ;
#37448 = ORIENTED_EDGE ( 'NONE', *, *, #10328, .F. ) ;
#37449 = ADVANCED_FACE ( 'NONE', ( #17171 ), #57883, .F. ) ;
#37450 = CARTESIAN_POINT ( 'NONE',  ( 4.694002226626921015, -44.68037479411228219, -9.052562051916137165 ) ) ;
#37451 = CARTESIAN_POINT ( 'NONE',  ( 4.967162193818130511, 38.83676580803792433, -18.65818244221215849 ) ) ;
#37452 = CARTESIAN_POINT ( 'NONE',  ( 0.6027444965799114707, -39.27709376116379048, -29.47623486071769960 ) ) ;
#37453 = COLOUR_RGB ( '', 0.08235294, 0.09019608, 0.10196078) ;
#37454 = CARTESIAN_POINT ( 'NONE',  ( 2.009741617377216460, -23.99099187825139978, -36.93150939672950983 ) ) ;
#37455 = CARTESIAN_POINT ( 'NONE',  ( 4.975801465491695552, 0.000000000000000000, 0.000000000000000000 ) ) ;
#37456 = ITEM_DEFINED_TRANSFORMATION ( 'NONE', 'NONE', #22918,  #14677 ) ;
#37457 = CARTESIAN_POINT ( 'NONE',  ( 0.8760168074886960365, -48.09529047980637273, -0.8912768426704541502 ) ) ;
#37458 = B_SPLINE_CURVE_WITH_KNOTS ( 'NONE', 3,
 ( #6450, #29985, #49096, #6148 ),
 .UNSPECIFIED., .F., .F.,
 ( 4, 4 ),
 ( 1.551583845779545699E-17, 0.005004948556313833924 ),
 .UNSPECIFIED. ) ;
#37459 = EDGE_CURVE ( 'NONE', #147, #22861, #6441, .T. ) ;
#37460 = DIRECTION ( 'NONE',  ( 0.000000000000000000, -0.5000000000000009992, -0.8660254037844380415 ) ) ;
#37461 = CARTESIAN_POINT ( 'NONE',  ( 4.214292481396495482, -11.25702090725073035, 0.000000000000000000 ) ) ;
#37463 = VERTEX_POINT ( 'NONE', #60665 ) ;
#37462 = CARTESIAN_POINT ( 'NONE',  ( 1.227938101723748288, -6.439911493064859549, 42.43379953535183802 ) ) ;
#37464 = ORIENTED_EDGE ( 'NONE', *, *, #33677, .T. ) ;
#37465 = CARTESIAN_POINT ( 'NONE',  ( 0.1155031312995260795, -7.208502386081764080, 43.53135796045952333 ) ) ;
#37466 = CARTESIAN_POINT ( 'NONE',  ( -6.078457390727109555, 3.077585051287140772, -19.00849760737554917 ) ) ;
#37467 = EDGE_CURVE ( 'NONE', #61214, #61173, #57266, .T. ) ;
#37468 = VERTEX_POINT ( 'NONE', #16869 ) ;
#37469 = CARTESIAN_POINT ( 'NONE',  ( 0.6029442701453590070, 10.84250512224628338, -47.89556668244295423 ) ) ;
#37470 = DIRECTION ( 'NONE',  ( 0.000000000000000000, 0.000000000000000000, 1.000000000000000000 ) ) ;
#37471 = CARTESIAN_POINT ( 'NONE',  ( 5.880360259849739535, 31.66572319753511877, 36.03610316515393919 ) ) ;
#37473 = EDGE_CURVE ( 'NONE', #24987, #37338, #60269, .T. ) ;
#37472 = ORIENTED_EDGE ( 'NONE', *, *, #37692, .T. ) ;
#37474 = VERTEX_POINT ( 'NONE', #11869 ) ;
#37475 = CARTESIAN_POINT ( 'NONE',  ( 0.9757892942422807803, 41.45966865212812280, 11.05594550521658981 ) ) ;
#37476 = CARTESIAN_POINT ( 'NONE',  ( 4.226256110419178924, -39.76716733621343991, 18.69223507344121771 ) ) ;
#37477 = CARTESIAN_POINT ( 'NONE',  ( 4.390527457369402420, 38.12195674272248169, 21.83808028959083103 ) ) ;
#37478 = CARTESIAN_POINT ( 'NONE',  ( 1.199999999999992628, 0.000000000000000000, 0.000000000000000000 ) ) ;
#37479 = DIRECTION ( 'NONE',  ( -1.000000000000000000, -1.836909530733573776E-16, 1.925929944387235853E-32 ) ) ;
#37480 = CARTESIAN_POINT ( 'NONE',  ( 0.5997462898726536595, 48.97040376101512749, 3.667585803694950464 ) ) ;
#37481 = VECTOR ( 'NONE', #17529, 999.9999999999998863 ) ;
#37482 = CARTESIAN_POINT ( 'NONE',  ( 0.9736507210033054083, 41.56063510425045848, -10.66979144439325644 ) ) ;
#37483 = ORIENTED_EDGE ( 'NONE', *, *, #2279, .T. ) ;
#37484 = CARTESIAN_POINT ( 'NONE',  ( 7.999999999999986677, 56.56854249492371878, 56.56854249492391062 ) ) ;
#37485 = DIRECTION ( 'NONE',  ( 1.000000000000000000, 0.000000000000000000, 0.000000000000000000 ) ) ;
#37486 = VERTEX_POINT ( 'NONE', #7425 ) ;
#37487 = CARTESIAN_POINT ( 'NONE',  ( 0.9780303403264775097, -37.54924812539149315, -18.61165168954299887 ) ) ;
#37488 = LINE ( 'NONE', #51547, #45666 ) ;
#37489 = CARTESIAN_POINT ( 'NONE',  ( 0.7764139734771238199, 46.35884964711795675, 7.134250507430955679 ) ) ;
#37490 = CARTESIAN_POINT ( 'NONE',  ( 4.691466044806103852, 43.79545162262296998, 8.371234562542003488 ) ) ;
#37491 = EDGE_CURVE ( 'NONE', #50490, #21383, #17693, .T. ) ;
#37492 = VECTOR ( 'NONE', #6713, 1000.000000000000000 ) ;
#37493 = VERTEX_POINT ( 'NONE', #46605 ) ;
#37494 = ORIENTED_EDGE ( 'NONE', *, *, #5497, .T. ) ;
#37495 = CARTESIAN_POINT ( 'NONE',  ( 4.553261556744873317, -39.67390170502044100, -18.85526688551536623 ) ) ;
#37496 = CARTESIAN_POINT ( 'NONE',  ( 0.5980271706414711508, 37.84660806146532508, -31.29989618327016743 ) ) ;
#37497 = EDGE_CURVE ( 'NONE', #37701, #6142, #52727, .T. ) ;
#37498 = LINE ( 'NONE', #56572, #6134 ) ;
#37499 = B_SPLINE_CURVE_WITH_KNOTS ( 'NONE', 3,
 ( #7666, #51201, #8283, #60911, #50284, #35902 ),
 .UNSPECIFIED., .F., .F.,
 ( 4, 2, 4 ),
 ( 7.040638946443416885E-18, 0.0002445244328975375650, 0.0004890488657950680827 ),
 .UNSPECIFIED. ) ;
#37500 = ORIENTED_EDGE ( 'NONE', *, *, #10926, .F. ) ;
#37501 = CARTESIAN_POINT ( 'NONE',  ( 4.956445790443988031, 0.000000000000000000, 0.000000000000000000 ) ) ;
#37503 = ORIENTED_EDGE ( 'NONE', *, *, #59435, .T. ) ;
#37502 = ADVANCED_FACE ( 'NONE', ( #55048 ), #12740, .F. ) ;
#37504 = CARTESIAN_POINT ( 'NONE',  ( 0.9730545539215883499, -5.099196237954599198, -42.60426903087358852 ) ) ;
#37505 = CARTESIAN_POINT ( 'NONE',  ( 0.3676999524040323597, -23.56959980820351674, 37.28839696479283106 ) ) ;
#37507 = ADVANCED_FACE ( 'NONE', ( #13710 ), #8683, .F. ) ;
#37506 = B_SPLINE_CURVE_WITH_KNOTS ( 'NONE', 3,
 ( #21624, #40763, #59828, #51656, #56351, #253 ),
 .UNSPECIFIED., .F., .F.,
 ( 4, 2, 4 ),
 ( 0.000000000000000000, 0.0002450742804987317367, 0.0004901485609974634734 ),
 .UNSPECIFIED. ) ;
#37508 = CARTESIAN_POINT ( 'NONE',  ( 4.956653778116990594, -26.26162724282345096, -40.28700667097706400 ) ) ;
#37509 = ORIENTED_EDGE ( 'NONE', *, *, #4988, .F. ) ;
#37510 = CARTESIAN_POINT ( 'NONE',  ( 0.7954190325252786797, -33.39101560460825624, 34.61997719899426329 ) ) ;
#37511 = EDGE_CURVE ( 'NONE', #21617, #56576, #28099, .T. ) ;
#37512 = CARTESIAN_POINT ( 'NONE',  ( 5.838029081930957709, -4.708022006888409550, 46.99893176377070603 ) ) ;
#37513 = CARTESIAN_POINT ( 'NONE',  ( 0.5830081025819928708, -41.73161187439133357, 21.39403198902457248 ) ) ;
#37514 = ORIENTED_EDGE ( 'NONE', *, *, #38598, .F. ) ;
#37515 = CARTESIAN_POINT ( 'NONE',  ( 0.8744876279028263033, -0.6840263623742536270, -49.09055060105834656 ) ) ;
#37516 = CARTESIAN_POINT ( 'NONE',  ( 4.967162193818130511, 8.839793687085803597, -42.16965968614184135 ) ) ;
#37517 = DIRECTION ( 'NONE',  ( -1.000000000000000000, -0.000000000000000000, -0.000000000000000000 ) ) ;
#37518 = AXIS2_PLACEMENT_3D ( 'NONE', #18648, #33374, #61527 ) ;
#37519 = EDGE_CURVE ( 'NONE', #20804, #55162, #31106, .T. ) ;
#37520 = CARTESIAN_POINT ( 'NONE',  ( 1.399999999999998579, 6.123233995736767268E-16, 5.000000000000000888 ) ) ;
#37521 = CARTESIAN_POINT ( 'NONE',  ( 0.8751705887134553219, 44.08562551107081617, -19.22545746485614870 ) ) ;
#37522 = VERTEX_POINT ( 'NONE', #4569 ) ;
#37523 = CARTESIAN_POINT ( 'NONE',  ( -6.010958268070873523, 14.95835081545473955, 11.45964880703832023 ) ) ;
#37524 = DIRECTION ( 'NONE',  ( 0.1736481776669314414, -0.9848077530122079093, 5.551115123125779621E-17 ) ) ;
#37525 = ORIENTED_EDGE ( 'NONE', *, *, #43030, .F. ) ;
#37526 = CARTESIAN_POINT ( 'NONE',  ( 0.5806925824938499181, 43.38503874128572591, -17.80339225430652306 ) ) ;
#37527 = CARTESIAN_POINT ( 'NONE',  ( 0.9789233960466703355, -27.15769414545705729, 31.91858981117664484 ) ) ;
#37528 = CARTESIAN_POINT ( 'NONE',  ( 5.960721111146673579, -2.685391721745896909, -20.34914600876574298 ) ) ;
#37529 = CARTESIAN_POINT ( 'NONE',  ( 0.9752132459055862235, 5.369621847648212487, -42.57112816680945855 ) ) ;
#37530 = CARTESIAN_POINT ( 'NONE',  ( 0.7954196712028475114, 37.62416450255248179, 29.96539649507097991 ) ) ;
#37531 = CARTESIAN_POINT ( 'NONE',  ( 0.8751705887134553219, -41.19904111682524928, 24.81530984069135570 ) ) ;
#37532 = CARTESIAN_POINT ( 'NONE',  ( 52.88134325800242408, 15.45619532895059045, 1.175551374349551370 ) ) ;
#37533 = DIRECTION ( 'NONE',  ( 1.000000000000000000, 5.849908684041128993E-17, -9.909413611503008370E-17 ) ) ;
#37534 = CARTESIAN_POINT ( 'NONE',  ( 0.6031356219577719280, 47.70727206974377310, 6.192730535896314059 ) ) ;
#37535 = CARTESIAN_POINT ( 'NONE',  ( 5.959547316686252039, -17.77749189599224877, 10.25972575517499052 ) ) ;
#37536 = FACE_OUTER_BOUND ( 'NONE', #12596, .T. ) ;
#37537 = AXIS2_PLACEMENT_3D ( 'NONE', #1253, #20092, #6873 ) ;
#37538 = CARTESIAN_POINT ( 'NONE',  ( 0.1102847568649952675, -5.537466591275985728, 42.76743495471819756 ) ) ;
#37539 = VERTEX_POINT ( 'NONE', #37211 ) ;
#37540 = CIRCLE ( 'NONE', #54475, 48.09070567114147110 ) ;
#37541 = CARTESIAN_POINT ( 'NONE',  ( -31.75000000000000000, 0.000000000000000000, 0.000000000000000000 ) ) ;
#37542 = CARTESIAN_POINT ( 'NONE',  ( 0.5807400328401637335, -44.45848844984429604, -17.82553128098455275 ) ) ;
#37543 = CARTESIAN_POINT ( 'NONE',  ( 0.8551540677456715978, 47.90804413217340851, -0.9122407826477486603 ) ) ;
#37544 = AXIS2_PLACEMENT_3D ( 'NONE', #34628, #11753, #34323 ) ;
#37545 = CARTESIAN_POINT ( 'NONE',  ( 1.157644175074336923, -16.89177048331274378, -38.36235609837159899 ) ) ;
#37546 = CARTESIAN_POINT ( 'NONE',  ( 4.962356264823608143, 0.000000000000000000, 0.000000000000000000 ) ) ;
#37548 = B_SPLINE_CURVE_WITH_KNOTS ( 'NONE', 3,
 ( #35551, #48398, #44645, #19919 ),
 .UNSPECIFIED., .F., .F.,
 ( 4, 4 ),
 ( 5.485677294651094893E-18, 0.004566006591234647236 ),
 .UNSPECIFIED. ) ;
#37547 = CARTESIAN_POINT ( 'NONE',  ( 1.479689385636123067, 32.77795963426115122, -29.44807646489730146 ) ) ;
#37549 = ADVANCED_FACE ( 'NONE', ( #42227 ), #53491, .F. ) ;
#37550 = EDGE_LOOP ( 'NONE', ( #21008, #41109, #28896, #43748 ) ) ;
#37551 = CARTESIAN_POINT ( 'NONE',  ( 3.660087539127338641, 47.34518630204121337, -8.130906407639580280 ) ) ;
#37552 = FACE_OUTER_BOUND ( 'NONE', #17573, .T. ) ;
#37553 = CARTESIAN_POINT ( 'NONE',  ( 4.956653778116960396, -3.690426056930336429, 47.94889704119049867 ) ) ;
#37554 = VERTEX_POINT ( 'NONE', #48139 ) ;
#37555 = DIRECTION ( 'NONE',  ( 0.000000000000000000, 0.000000000000000000, 1.000000000000000000 ) ) ;
#37556 = B_SPLINE_CURVE_WITH_KNOTS ( 'NONE', 3,
 ( #50301, #50914, #55920, #35921 ),
 .UNSPECIFIED., .F., .F.,
 ( 4, 4 ),
 ( 0.000000000000000000, 0.005014147105413698652 ),
 .UNSPECIFIED. ) ;
#37557 = CARTESIAN_POINT ( 'NONE',  ( 5.896782393890504181, 16.58545041924856278, 11.37756218478545911 ) ) ;
#37558 = ORIENTED_EDGE ( 'NONE', *, *, #35859, .T. ) ;
#37559 =( BOUNDED_SURFACE ( )  B_SPLINE_SURFACE ( 3, 1, ( 
 ( #51594, #22803 ),
 ( #40705, #36307 ),
 ( #17802, #56302 ),
 ( #55993, #22495 ) ),
 .UNSPECIFIED., .F., .F., .F. ) 
 B_SPLINE_SURFACE_WITH_KNOTS ( ( 4, 4 ),
 ( 2, 2 ),
 ( 0.000000000000000000, 1.000000000000000000 ),
 ( 0.000000000000000000, 1.000000000000000000 ),
 .UNSPECIFIED. ) 
 GEOMETRIC_REPRESENTATION_ITEM ( )  RATIONAL_B_SPLINE_SURFACE ( (
 ( 1.000000000000000000, 1.000000000000000000),
 ( 0.7269869731126821222, 0.9931720237060910339),
 ( 0.7269869731126821222, 0.9931720237060910339),
 ( 1.000000000000000000, 1.000000000000000000) ) ) 
 REPRESENTATION_ITEM ( '' )  SURFACE ( )  );
#37560 = FACE_OUTER_BOUND ( 'NONE', #14087, .T. ) ;
#37561 = ORIENTED_EDGE ( 'NONE', *, *, #31204, .F. ) ;
#37562 = CARTESIAN_POINT ( 'NONE',  ( 50.67548179587118540, 15.27178771460630813, -2.649999999999993694 ) ) ;
#37563 = CARTESIAN_POINT ( 'NONE',  ( -2.739355103387247858, -4.498893467419792458, 14.23402699589348686 ) ) ;
#37564 = ORIENTED_EDGE ( 'NONE', *, *, #58973, .T. ) ;
#37565 = CARTESIAN_POINT ( 'NONE',  ( 0.5827359174754824789, -29.44457394064646749, 37.77623182210385977 ) ) ;
#37566 = CARTESIAN_POINT ( 'NONE',  ( 0.9741495583595165542, 21.11077839432136827, 37.35596046161874995 ) ) ;
#37567 = CARTESIAN_POINT ( 'NONE',  ( 0.7242486021783788308, -43.17951146175377630, 23.37822175226863664 ) ) ;
#37568 = EDGE_CURVE ( 'NONE', #44145, #60939, #14326, .T. ) ;
#37569 = VERTEX_POINT ( 'NONE', #47216 ) ;
#37570 = CARTESIAN_POINT ( 'NONE',  ( 0.9780303403264759554, -7.289770003306762725, -41.26982998140380232 ) ) ;
#37571 = EDGE_CURVE ( 'NONE', #26859, #26613, #51670, .T. ) ;
#37572 = B_SPLINE_CURVE_WITH_KNOTS ( 'NONE', 3,
 ( #54499, #34824, #2192, #11628, #10698, #6568 ),
 .UNSPECIFIED., .F., .F.,
 ( 4, 2, 4 ),
 ( 1.187272666737178580E-16, 0.0002448718616795955358, 0.0004897437233590723514 ),
 .UNSPECIFIED. ) ;
#37573 = ORIENTED_EDGE ( 'NONE', *, *, #24836, .T. ) ;
#37574 = CARTESIAN_POINT ( 'NONE',  ( 0.7764146366350235251, -39.16768488414486171, -25.80567640046461975 ) ) ;
#37576 = ADVANCED_FACE ( 'NONE', ( #19327 ), #19138, .F. ) ;
#37575 = ORIENTED_EDGE ( 'NONE', *, *, #53744, .F. ) ;
#37577 = VERTEX_POINT ( 'NONE', #8668 ) ;
#37578 = CARTESIAN_POINT ( 'NONE',  ( 4.960386119450146403, -4.847629508246811270, -43.48490488460468839 ) ) ;
#37579 = CARTESIAN_POINT ( 'NONE',  ( -2.500000000000002220, 0.000000000000000000, -5.574599999999999334 ) ) ;
#37580 = ADVANCED_FACE ( 'NONE', ( #43145 ), #4276, .F. ) ;
#37581 = AXIS2_PLACEMENT_3D ( 'NONE', #17576, #11328, #30415 ) ;
#37582 = CARTESIAN_POINT ( 'NONE',  ( 0.9756354156337461170, 33.96210048825376049, 26.22428641656263437 ) ) ;
#37583 = CARTESIAN_POINT ( 'NONE',  ( 0.5807400328401637335, -37.66660715020845629, -29.58941477093055639 ) ) ;
#37584 = ORIENTED_EDGE ( 'NONE', *, *, #53365, .T. ) ;
#37585 = CARTESIAN_POINT ( 'NONE',  ( 3.238018933889920792, -2.498552698661791638, -13.15920692061884090 ) ) ;
#37586 = EDGE_CURVE ( 'NONE', #46003, #53253, #31902, .T. ) ;
#37587 = CARTESIAN_POINT ( 'NONE',  ( 0.5848930533535030563, 45.27791896734284194, -12.21405487028341241 ) ) ;
#37588 = CARTESIAN_POINT ( 'NONE',  ( 1.139999999999998570, 8.422079734756228398E-16, 6.866799999999992465 ) ) ;
#37589 = AXIS2_PLACEMENT_3D ( 'NONE', #33046, #9517, #24552 ) ;
#37590 = ORIENTED_EDGE ( 'NONE', *, *, #51197, .T. ) ;
#37591 = ORIENTED_EDGE ( 'NONE', *, *, #56212, .T. ) ;
#37592 = CARTESIAN_POINT ( 'NONE',  ( 0.1104177457020372732, -21.56646482560105937, -37.34442418285495791 ) ) ;
#37593 = CARTESIAN_POINT ( 'NONE',  ( 2.528190830796651412, 23.91659899089207642, 34.50000621538883649 ) ) ;
#37594 = CARTESIAN_POINT ( 'NONE',  ( 4.256456730324547522, 0.6428818333149034503, -47.05679108708081770 ) ) ;
#37595 = CARTESIAN_POINT ( 'NONE',  ( 4.956653778116975495, -36.51451553856441024, 31.29546495791839078 ) ) ;
#37596 = LINE ( 'NONE', #42598, #47830 ) ;
#37597 = EDGE_CURVE ( 'NONE', #3834, #2066, #22666, .T. ) ;
#37598 = VERTEX_POINT ( 'NONE', #1117 ) ;
#37599 = EDGE_CURVE ( 'NONE', #11949, #15688, #3629, .T. ) ;
#37600 = CARTESIAN_POINT ( 'NONE',  ( 4.834790513006553603, -44.98626621068908094, 14.45078521553053008 ) ) ;
#37601 = CARTESIAN_POINT ( 'NONE',  ( 50.50000000000000000, 15.27178771460631168, 2.649999999999992806 ) ) ;
#37602 = CARTESIAN_POINT ( 'NONE',  ( 4.390527457369402420, -39.44280170213821890, -19.35072945690735580 ) ) ;
#37603 = LINE ( 'NONE', #41686, #60807 ) ;
#37604 = SURFACE_STYLE_FILL_AREA ( #23177 ) ;
#37605 = CARTESIAN_POINT ( 'NONE',  ( 0.7762783648524402835, -34.49689442177322718, -33.23866576554873831 ) ) ;
#37606 = ORIENTED_EDGE ( 'NONE', *, *, #44810, .F. ) ;
#37607 = FACE_OUTER_BOUND ( 'NONE', #37056, .T. ) ;
#37608 = CARTESIAN_POINT ( 'NONE',  ( 0.6064782688330886407, 28.38738766212763309, -37.32948791691164558 ) ) ;
#37609 = LINE ( 'NONE', #46694, #14870 ) ;
#37610 = DIRECTION ( 'NONE',  ( 1.000000000000000000, 1.836909530733573776E-16, 0.000000000000000000 ) ) ;
#37611 = CARTESIAN_POINT ( 'NONE',  ( 0.9783242366443554161, 28.94125691613812634, 30.31069346485841365 ) ) ;
#37612 = CARTESIAN_POINT ( 'NONE',  ( 0.8751705887134553219, -34.63284514348562482, -33.37254303619542384 ) ) ;
#37613 = CARTESIAN_POINT ( 'NONE',  ( 0.7764146366350260786, -8.679346565860239338, -46.09457036201614955 ) ) ;
#37614 = CARTESIAN_POINT ( 'NONE',  ( 0.6064515330803591509, 37.24100359994584153, 28.50336799232513840 ) ) ;
#37615 = B_SPLINE_CURVE_WITH_KNOTS ( 'NONE', 3,
 ( #40924, #55274, #60909, #56210 ),
 .UNSPECIFIED., .F., .F.,
 ( 4, 4 ),
 ( 0.000000000000000000, 0.004442905043737217438 ),
 .UNSPECIFIED. ) ;
#37616 =( BOUNDED_SURFACE ( )  B_SPLINE_SURFACE ( 3, 1, ( 
 ( #15125, #34236 ),
 ( #49239, #44573 ),
 ( #10422, #1002 ),
 ( #29513, #48621 ) ),
 .UNSPECIFIED., .F., .F., .F. ) 
 B_SPLINE_SURFACE_WITH_KNOTS ( ( 4, 4 ),
 ( 2, 2 ),
 ( 0.000000000000000000, 1.000000000000000000 ),
 ( 0.000000000000000000, 1.000000000000000000 ),
 .UNSPECIFIED. ) 
 GEOMETRIC_REPRESENTATION_ITEM ( )  RATIONAL_B_SPLINE_SURFACE ( (
 ( 1.000000000000000000, 1.000000000000000000),
 ( 0.9953485035131437453, 0.8621029689291515030),
 ( 0.9953485035131437453, 0.8621029689291515030),
 ( 1.000000000000000000, 1.000000000000000000) ) ) 
 REPRESENTATION_ITEM ( '' )  SURFACE ( )  );
#37617 = EDGE_CURVE ( 'NONE', #35664, #43133, #53721, .T. ) ;
#37618 = DIRECTION ( 'NONE',  ( 0.000000000000000000, 0.000000000000000000, -1.000000000000000000 ) ) ;
#37619 = ORIENTED_EDGE ( 'NONE', *, *, #32067, .T. ) ;
#37620 = B_SPLINE_CURVE_WITH_KNOTS ( 'NONE', 3,
 ( #5334, #43603, #19786, #41076 ),
 .UNSPECIFIED., .F., .F.,
 ( 4, 4 ),
 ( 0.000000000000000000, 0.004446090762761369455 ),
 .UNSPECIFIED. ) ;
#37621 = CARTESIAN_POINT ( 'NONE',  ( 0.5809828226811553087, 47.89273459658653564, -0.5448590168534052092 ) ) ;
#37622 = CIRCLE ( 'NONE', #14593, 9.500000000000000000 ) ;
#37623 = CARTESIAN_POINT ( 'NONE',  ( 0.9785694773339250752, 19.94506828457740610, 36.85823729966229934 ) ) ;
#37624 = CARTESIAN_POINT ( 'NONE',  ( 0.7056555295713312637, 34.46100226633736696, 33.27140645154206311 ) ) ;
#37625 = DIRECTION ( 'NONE',  ( 0.9990097760809872884, 0.000000000000000000, -0.04449120468829269315 ) ) ;
#37626 = ORIENTED_EDGE ( 'NONE', *, *, #52913, .T. ) ;
#37627 = CARTESIAN_POINT ( 'NONE',  ( 4.975801465491695552, 9.906103548667566372, 46.87746200127460128 ) ) ;
#37628 = VECTOR ( 'NONE', #22485, 1000.000000000000114 ) ;
#37629 = CARTESIAN_POINT ( 'NONE',  ( 2.526464513654346433, 17.56107808841309037, 39.22765990515326706 ) ) ;
#37630 =( LENGTH_UNIT ( ) NAMED_UNIT ( * ) SI_UNIT ( .MILLI., .METRE. ) );
#37631 =( BOUNDED_SURFACE ( )  B_SPLINE_SURFACE ( 3, 1, ( 
 ( #4125, #47375 ),
 ( #3825, #42090 ),
 ( #4423, #27037 ),
 ( #36765, #32988 ) ),
 .UNSPECIFIED., .F., .F., .F. ) 
 B_SPLINE_SURFACE_WITH_KNOTS ( ( 4, 4 ),
 ( 2, 2 ),
 ( 0.000000000000000000, 1.000000000000000000 ),
 ( 0.000000000000000000, 1.000000000000000000 ),
 .UNSPECIFIED. ) 
 GEOMETRIC_REPRESENTATION_ITEM ( )  RATIONAL_B_SPLINE_SURFACE ( (
 ( 1.000000000000000000, 1.000000000000000000),
 ( 0.9953040768229013402, 0.8617119497784988535),
 ( 0.9953040768229013402, 0.8617119497784988535),
 ( 1.000000000000000000, 1.000000000000000000) ) ) 
 REPRESENTATION_ITEM ( '' )  SURFACE ( )  );
#37632 = ORIENTED_EDGE ( 'NONE', *, *, #46999, .F. ) ;
#37633 = DIRECTION ( 'NONE',  ( -0.07906939808003034253, 0.6987975377710859970, 0.7109360248941737348 ) ) ;
#37634 = CARTESIAN_POINT ( 'NONE',  ( 0.5835871038041873238, -45.92888218877342865, -9.474821042704075325 ) ) ;
#37635 = CARTESIAN_POINT ( 'NONE',  ( 5.901764892641288895, 48.96927204603445460, -0.04315925332753958038 ) ) ;
#37636 = ORIENTED_EDGE ( 'NONE', *, *, #23113, .F. ) ;
#37637 = CIRCLE ( 'NONE', #33648, 43.92652462719577500 ) ;
#37638 = CARTESIAN_POINT ( 'NONE',  ( 4.975610109902397937, 0.000000000000000000, 0.000000000000000000 ) ) ;
#37639 = ORIENTED_EDGE ( 'NONE', *, *, #35453, .T. ) ;
#37640 = ORIENTED_EDGE ( 'NONE', *, *, #40858, .T. ) ;
#37641 = CARTESIAN_POINT ( 'NONE',  ( 4.975610109902397937, -11.44439439467527642, -47.55497076097196185 ) ) ;
#37642 = LINE ( 'NONE', #3772, #40497 ) ;
#37643 = EDGE_LOOP ( 'NONE', ( #51082, #52319 ) ) ;
#37644 = CARTESIAN_POINT ( 'NONE',  ( 5.896782393890504181, -13.98685533979025131, 14.45316451791071266 ) ) ;
#37645 = ORIENTED_EDGE ( 'NONE', *, *, #58031, .T. ) ;
#37646 = CARTESIAN_POINT ( 'NONE',  ( 0.5806925824938502512, 11.40214825760292250, 45.48860711711456872 ) ) ;
#37647 = CARTESIAN_POINT ( 'NONE',  ( 0.6039202388192952409, 4.888815891286901305, -48.86372061182091642 ) ) ;
#37648 = CARTESIAN_POINT ( 'NONE',  ( 5.838029081930957709, 14.01343897760509805, 45.10752250095163873 ) ) ;
#37649 = EDGE_CURVE ( 'NONE', #41654, #30011, #34902, .T. ) ;
#37650 = VERTEX_POINT ( 'NONE', #49356 ) ;
#37651 = CARTESIAN_POINT ( 'NONE',  ( 0.9740398440564311811, -16.80263250099859462, -39.48175649279251331 ) ) ;
#37652 = CARTESIAN_POINT ( 'NONE',  ( 0.6039202388192952409, 37.27969488251749652, 31.96541978944418361 ) ) ;
#37653 = FACE_OUTER_BOUND ( 'NONE', #61264, .T. ) ;
#37654 = CARTESIAN_POINT ( 'NONE',  ( 0.8753041380234465318, -6.957149426673734816, -48.60798699522449340 ) ) ;
#37655 = ORIENTED_EDGE ( 'NONE', *, *, #3367, .F. ) ;
#37656 = ADVANCED_FACE ( 'NONE', ( #39999, #29324 ), #11161, .F. ) ;
#37657 = CARTESIAN_POINT ( 'NONE',  ( -6.017396004339686577, 9.422598049764623340, 16.31807101179373731 ) ) ;
#37658 = CARTESIAN_POINT ( 'NONE',  ( 4.975801465491695552, -35.64402118370979622, 32.01766832630250548 ) ) ;
#37659 = VERTEX_POINT ( 'NONE', #15247 ) ;
#37660 = CARTESIAN_POINT ( 'NONE',  ( 0.5806925824938499181, 43.38503874128572591, -17.80339225430652306 ) ) ;
#37661 = ORIENTED_EDGE ( 'NONE', *, *, #57668, .F. ) ;
#37662 = FACE_OUTER_BOUND ( 'NONE', #17214, .T. ) ;
#37663 = CARTESIAN_POINT ( 'NONE',  ( 0.6028777368367060907, 46.63305245651208253, -15.39149920895511059 ) ) ;
#37664 = ORIENTED_EDGE ( 'NONE', *, *, #16298, .F. ) ;
#37665 = CARTESIAN_POINT ( 'NONE',  ( 2.301430502907646947, 13.67112791032043084, -46.04685681264152208 ) ) ;
#37666 = CARTESIAN_POINT ( 'NONE',  ( 1.231276596079887931, 36.49189576017872128, 20.63051901543724043 ) ) ;
#37667 = CARTESIAN_POINT ( 'NONE',  ( 1.479689385636123067, 8.655498711569247661, -43.20493244204549654 ) ) ;
#37668 = CARTESIAN_POINT ( 'NONE',  ( 0.5830081025819895402, -1.840045895287395261, -46.85985771943282430 ) ) ;
#37669 = CIRCLE ( 'NONE', #35655, 75.00000000000001421 ) ;
#37670 = ORIENTED_EDGE ( 'NONE', *, *, #31857, .T. ) ;
#37671 = DIRECTION ( 'NONE',  ( 0.000000000000000000, 0.000000000000000000, -1.000000000000000000 ) ) ;
#37672 = CIRCLE ( 'NONE', #8657, 42.92674063221959813 ) ;
#37673 = CARTESIAN_POINT ( 'NONE',  ( 0.9790320750461900534, -41.82074296194507923, 2.713409414944875309 ) ) ;
#37674 = CARTESIAN_POINT ( 'NONE',  ( 2.643462169533600914, -19.65219740572217688, 43.83256147628700461 ) ) ;
#37675 = EDGE_CURVE ( 'NONE', #26391, #47393, #53660, .T. ) ;
#37676 = CARTESIAN_POINT ( 'NONE',  ( 0.5832367798473389042, -44.14510605973666202, -18.58036934788121997 ) ) ;
#37677 =( REPRESENTATION_RELATIONSHIP ('NONE','NONE', #44881, #19619 ) REPRESENTATION_RELATIONSHIP_WITH_TRANSFORMATION ( #14879 )SHAPE_REPRESENTATION_RELATIONSHIP( ) );
#37678 = B_SPLINE_CURVE_WITH_KNOTS ( 'NONE', 3,
 ( #18724, #23412, #43159, #52838 ),
 .UNSPECIFIED., .F., .F.,
 ( 4, 4 ),
 ( 0.000000000000000000, 0.005004948556313805301 ),
 .UNSPECIFIED. ) ;
#37679 = CARTESIAN_POINT ( 'NONE',  ( 0.5804410086790514622, -46.82762660194602233, 2.587129429331431751 ) ) ;
#37680 = CARTESIAN_POINT ( 'NONE',  ( 4.975610109902397937, 24.86209007719020647, -42.12274782266053563 ) ) ;
#37681 = CARTESIAN_POINT ( 'NONE',  ( 0.5832367798473385712, -46.33367954572892700, 12.13303976268045048 ) ) ;
#37682 = VECTOR ( 'NONE', #6267, 1000.000000000000000 ) ;
#37683 = CARTESIAN_POINT ( 'NONE',  ( 4.956653778116975495, -26.26162724282400518, 40.28700667097671584 ) ) ;
#37684 = CARTESIAN_POINT ( 'NONE',  ( 0.9785694773339259633, -12.62891347609833126, 39.96055492767703043 ) ) ;
#37685 = CARTESIAN_POINT ( 'NONE',  ( 0.1310142868023688179, -22.11113027429312083, 37.02349354742202792 ) ) ;
#37686 = DIRECTION ( 'NONE',  ( 0.9990097760809872884, 0.000000000000000000, -0.04449120468829285274 ) ) ;
#37687 = CARTESIAN_POINT ( 'NONE',  ( 0.6041374136657475802, 29.14743607025033967, 38.27243465845350556 ) ) ;
#37688 = CARTESIAN_POINT ( 'NONE',  ( 0.9756354156337465611, 37.09450626018210073, 21.56699035436949430 ) ) ;
#37689 = CARTESIAN_POINT ( 'NONE',  ( 4.553261556744875094, 0.000000000000000000, 0.000000000000000000 ) ) ;
#37690 = B_SPLINE_CURVE_WITH_KNOTS ( 'NONE', 3,
 ( #29318, #10224, #48737, #5490, #58421, #60825 ),
 .UNSPECIFIED., .F., .F.,
 ( 4, 2, 4 ),
 ( 0.002336974151641520864, 0.003500975885716454961, 0.004664977619791389057 ),
 .UNSPECIFIED. ) ;
#37691 = CARTESIAN_POINT ( 'NONE',  ( 0.5807400328401637335, -23.47602859900744221, 41.75144119563879030 ) ) ;
#37692 = EDGE_CURVE ( 'NONE', #30308, #2370, #10689, .T. ) ;
#37693 = CARTESIAN_POINT ( 'NONE',  ( 0.5834584762367753807, 45.27752917664024324, -12.21398136037885784 ) ) ;
#37694 = CARTESIAN_POINT ( 'NONE',  ( 0.9730545539215883499, 15.95224156741883270, -39.83279466599022811 ) ) ;
#37696 = ORIENTED_EDGE ( 'NONE', *, *, #5917, .T. ) ;
#37695 = CARTESIAN_POINT ( 'NONE',  ( 0.9736507210033062965, 39.46762617149634167, 16.83559693395279311 ) ) ;
#37697 = DIRECTION ( 'NONE',  ( -1.000000000000000000, -1.836909530733573776E-16, 1.925929944387235853E-32 ) ) ;
#37698 = CARTESIAN_POINT ( 'NONE',  ( 0.5834872094924163921, 23.75111410077710161, 41.59216540884673208 ) ) ;
#37699 = LINE ( 'NONE', #27659, #41754 ) ;
#37700 = ORIENTED_EDGE ( 'NONE', *, *, #11032, .F. ) ;
#37701 = VERTEX_POINT ( 'NONE', #19640 ) ;
#37702 = CARTESIAN_POINT ( 'NONE',  ( 4.975610109902397937, -41.30423662854469313, 26.19941685746003301 ) ) ;
#37703 = DIRECTION ( 'NONE',  ( -1.000000000000000000, -0.000000000000000000, -0.000000000000000000 ) ) ;
#37704 = EDGE_CURVE ( 'NONE', #56788, #10029, #14947, .T. ) ;
#37705 = VERTEX_POINT ( 'NONE', #30242 ) ;
#37706 = ORIENTED_EDGE ( 'NONE', *, *, #25209, .F. ) ;
#37707 = DIRECTION ( 'NONE',  ( -1.000000000000000000, -0.000000000000000000, -0.000000000000000000 ) ) ;
#37708 = EDGE_CURVE ( 'NONE', #44643, #20535, #22122, .T. ) ;
#37709 = CIRCLE ( 'NONE', #14718, 47.09074272231896430 ) ;
#37711 = VERTEX_POINT ( 'NONE', #44391 ) ;
#37710 =( BOUNDED_SURFACE ( )  B_SPLINE_SURFACE ( 3, 1, ( 
 ( #61073, #13185 ),
 ( #31663, #9081 ),
 ( #27887, #3745 ),
 ( #4047, #32912 ) ),
 .UNSPECIFIED., .F., .F., .F. ) 
 B_SPLINE_SURFACE_WITH_KNOTS ( ( 4, 4 ),
 ( 2, 2 ),
 ( 0.000000000000000000, 1.000000000000000000 ),
 ( 0.000000000000000000, 1.000000000000000000 ),
 .UNSPECIFIED. ) 
 GEOMETRIC_REPRESENTATION_ITEM ( )  RATIONAL_B_SPLINE_SURFACE ( (
 ( 1.000000000000000000, 1.000000000000000000),
 ( 0.9953390228620291325, 0.8624445117761032620),
 ( 0.9953390228620291325, 0.8624445117761032620),
 ( 1.000000000000000000, 1.000000000000000000) ) ) 
 REPRESENTATION_ITEM ( '' )  SURFACE ( )  );
#37712 = DIRECTION ( 'NONE',  ( -1.000000000000000000, -0.000000000000000000, -0.000000000000000000 ) ) ;
#37713 = AXIS2_PLACEMENT_3D ( 'NONE', #7225, #26051, #26352 ) ;
#37714 = CARTESIAN_POINT ( 'NONE',  ( 4.956445790444029775, 29.98832127573299289, -36.30755619981957949 ) ) ;
#37715 = VECTOR ( 'NONE', #47717, 999.9999999999998863 ) ;
#37716 = ORIENTED_EDGE ( 'NONE', *, *, #21522, .F. ) ;
#37717 = VERTEX_POINT ( 'NONE', #20553 ) ;
#37718 = DIRECTION ( 'NONE',  ( 1.000000000000000000, 0.000000000000000000, 0.000000000000000000 ) ) ;
#37719 = EDGE_LOOP ( 'NONE', ( #6291, #55330, #21078, #8860 ) ) ;
#37720 = DIRECTION ( 'NONE',  ( -0.1011922191286467460, 0.9269080304895044309, -0.3613884859841106634 ) ) ;
#37721 = CYLINDRICAL_SURFACE ( 'NONE', #22583, 10.00000000000000711 ) ;
#37722 = EDGE_LOOP ( 'NONE', ( #12840, #3726, #53778, #57855 ) ) ;
#37723 = DIRECTION ( 'NONE',  ( -1.000000000000000000, -0.000000000000000000, -0.000000000000000000 ) ) ;
#37724 = B_SPLINE_CURVE_WITH_KNOTS ( 'NONE', 3,
 ( #20501, #49608, #34608, #17577 ),
 .UNSPECIFIED., .F., .F.,
 ( 4, 4 ),
 ( 2.294131830766625192E-17, 0.004564976165746188579 ),
 .UNSPECIFIED. ) ;
#37725 = CARTESIAN_POINT ( 'NONE',  ( 5.917102823773431552, -9.657882276496826179, 17.64128759430757754 ) ) ;
#37726 = VERTEX_POINT ( 'NONE', #20258 ) ;
#37727 = EDGE_CURVE ( 'NONE', #23289, #33299, #11464, .T. ) ;
#37728 = AXIS2_PLACEMENT_3D ( 'NONE', #33535, #282, #20354 ) ;
#37729 = ORIENTED_EDGE ( 'NONE', *, *, #24565, .F. ) ;
#37730 =( BOUNDED_SURFACE ( )  B_SPLINE_SURFACE ( 3, 1, ( 
 ( #17441, #21213 ),
 ( #59410, #40350 ),
 ( #16517, #54390 ),
 ( #12764, #16213 ) ),
 .UNSPECIFIED., .F., .F., .F. ) 
 B_SPLINE_SURFACE_WITH_KNOTS ( ( 4, 4 ),
 ( 2, 2 ),
 ( 0.000000000000000000, 1.000000000000000000 ),
 ( 0.000000000000000000, 1.000000000000000000 ),
 .UNSPECIFIED. ) 
 GEOMETRIC_REPRESENTATION_ITEM ( )  RATIONAL_B_SPLINE_SURFACE ( (
 ( 1.000000000000000000, 1.000000000000000000),
 ( 0.7211978278499970862, 0.9934217856018976445),
 ( 0.7211978278499970862, 0.9934217856018976445),
 ( 1.000000000000000000, 1.000000000000000000) ) ) 
 REPRESENTATION_ITEM ( '' )  SURFACE ( )  );
#37731 = CARTESIAN_POINT ( 'NONE',  ( 4.553261556744875094, 43.92594400279101308, 0.2258523573163287723 ) ) ;
#37732 = EDGE_LOOP ( 'NONE', ( #15307, #55050, #7565, #33328 ) ) ;
#37733 = CARTESIAN_POINT ( 'NONE',  ( 0.3622758884714730732, 41.42293301073625855, -11.95365414648454205 ) ) ;
#37734 = CARTESIAN_POINT ( 'NONE',  ( 0.7044674535452954967, -24.73445998053410833, -42.42651543884158372 ) ) ;
#37735 = CARTESIAN_POINT ( 'NONE',  ( 5.960721111146673579, 2.672857320903031741, 20.35079619394246819 ) ) ;
#37736 = CARTESIAN_POINT ( 'NONE',  ( 0.1101816497532062678, 5.763501205266542193, 42.73758747687831772 ) ) ;
#37737 = CARTESIAN_POINT ( 'NONE',  ( 0.6253024248130498730, -2.260222131445328131, 49.05441492194326969 ) ) ;
#37738 = ADVANCED_FACE ( 'NONE', ( #34055 ), #10712, .F. ) ;
#37739 =( BOUNDED_SURFACE ( )  B_SPLINE_SURFACE ( 3, 1, ( 
 ( #7069, #26196 ),
 ( #59703, #44720 ),
 ( #11496, #34691 ),
 ( #16821, #49087 ) ),
 .UNSPECIFIED., .F., .F., .F. ) 
 B_SPLINE_SURFACE_WITH_KNOTS ( ( 4, 4 ),
 ( 2, 2 ),
 ( 0.000000000000000000, 1.000000000000000000 ),
 ( 0.000000000000000000, 1.000000000000000000 ),
 .UNSPECIFIED. ) 
 GEOMETRIC_REPRESENTATION_ITEM ( )  RATIONAL_B_SPLINE_SURFACE ( (
 ( 1.000000000000000000, 1.000000000000000000),
 ( 0.7269869731126817891, 0.9931720237060910339),
 ( 0.7269869731126817891, 0.9931720237060910339),
 ( 1.000000000000000000, 1.000000000000000000) ) ) 
 REPRESENTATION_ITEM ( '' )  SURFACE ( )  );
#37740 = VERTEX_POINT ( 'NONE', #13023 ) ;
#37741 = CARTESIAN_POINT ( 'NONE',  ( -6.001507490154110336, -4.862106078788054120, 18.20581304543296142 ) ) ;
#37742 = VECTOR ( 'NONE', #5581, 1000.000000000000227 ) ;
#37743 = CARTESIAN_POINT ( 'NONE',  ( 0.6254311100348639574, 24.64676532715794011, -41.31309618784389670 ) ) ;
#37744 = EDGE_CURVE ( 'NONE', #56250, #44331, #35563, .T. ) ;
#37745 = CARTESIAN_POINT ( 'NONE',  ( 5.910764540655177868, 18.99430111539255961, 6.611940986348878724 ) ) ;
#37746 = B_SPLINE_CURVE_WITH_KNOTS ( 'NONE', 3,
 ( #45942, #26490, #45616, #40938 ),
 .UNSPECIFIED., .F., .F.,
 ( 4, 4 ),
 ( 0.000000000000000000, 0.005013413432710147645 ),
 .UNSPECIFIED. ) ;
#37747 = VERTEX_POINT ( 'NONE', #50581 ) ;
#37748 = CARTESIAN_POINT ( 'NONE',  ( 7.000000000000019540, -72.00000000000002842, 8.817456953860944867E-15 ) ) ;
#37749 = CARTESIAN_POINT ( 'NONE',  ( 0.5804410086790514622, -7.261380058784692615, 46.33348909263450821 ) ) ;
#37750 = CARTESIAN_POINT ( 'NONE',  ( 3.390910168358336918, -5.067088124568913443, 43.68548677159830618 ) ) ;
#37751 = ORIENTED_EDGE ( 'NONE', *, *, #18964, .T. ) ;
#37752 = ORIENTED_EDGE ( 'NONE', *, *, #5312, .T. ) ;
#37753 = DIRECTION ( 'NONE',  ( 0.8660254037844354880, -0.5000000000000055511, 0.000000000000000000 ) ) ;
#37754 = CARTESIAN_POINT ( 'NONE',  ( 0.7048096507298635682, -37.64898672361973553, 29.95256433478663283 ) ) ;
#37755 = CARTESIAN_POINT ( 'NONE',  ( -6.203732170862584994, -1.182048853166489222, 5.744326400484686099E-14 ) ) ;
#37756 = EDGE_CURVE ( 'NONE', #38361, #36415, #10938, .T. ) ;
#37757 = CARTESIAN_POINT ( 'NONE',  ( -2.739355103387247858, 3.577672767447764635, -14.49302675496321768 ) ) ;
#37758 = CARTESIAN_POINT ( 'NONE',  ( 0.5806925824938502512, -20.23436166722406426, -42.30594485723652554 ) ) ;
#37759 = CARTESIAN_POINT ( 'NONE',  ( 4.322998006666179727, 10.36018990813312968, -46.85697641700698313 ) ) ;
#37760 = CARTESIAN_POINT ( 'NONE',  ( 0.3622758884714600280, 40.13994584881781691, -15.73321244754812298 ) ) ;
#37761 = CARTESIAN_POINT ( 'NONE',  ( 2.648799415243696664, 38.22150636651035427, -30.71862487749745441 ) ) ;
#37762 = CYLINDRICAL_SURFACE ( 'NONE', #24788, 12.50000000000000000 ) ;
#37763 = CARTESIAN_POINT ( 'NONE',  ( 0.7954190325252777916, 29.96539637359164843, 37.62416463577120140 ) ) ;
#37764 = CIRCLE ( 'NONE', #24761, 15.43999999999999417 ) ;
#37765 = CARTESIAN_POINT ( 'NONE',  ( 0.9785694773339252972, -1.177911127880463260, -41.89209867134238863 ) ) ;
#37766 = CARTESIAN_POINT ( 'NONE',  ( 1.231276596079887264, 3.353048872156665805, -41.78556968953512296 ) ) ;
#37767 = ORIENTED_EDGE ( 'NONE', *, *, #51466, .F. ) ;
#37768 = VECTOR ( 'NONE', #48042, 1000.000000000000114 ) ;
#37769 = AXIS2_PLACEMENT_3D ( 'NONE', #42574, #27841, #29076 ) ;
#37770 = DIRECTION ( 'NONE',  ( 3.273063162220399693E-16, -1.000000000000000000, -5.236901059552639509E-15 ) ) ;
#37771 = CARTESIAN_POINT ( 'NONE',  ( 0.6039202388192953519, -1.748061966038592097, -49.07655236680628974 ) ) ;
#37772 = CARTESIAN_POINT ( 'NONE',  ( 0.7246131072078569879, -33.42811616637893479, -34.58859703353066806 ) ) ;
#37773 = CARTESIAN_POINT ( 'NONE',  ( 0.5824935313925944103, -35.02383213588255728, -31.18604430785284265 ) ) ;
#37774 = CARTESIAN_POINT ( 'NONE',  ( 2.301430502907645614, 44.85388302506905234, -17.18551536142205194 ) ) ;
#37775 = CARTESIAN_POINT ( 'NONE',  ( 0.1092355843206037486, 42.71527351115371829, 5.926758618548121582 ) ) ;
#37776 = B_SPLINE_CURVE_WITH_KNOTS ( 'NONE', 3,
 ( #48876, #16293, #40140, #34792 ),
 .UNSPECIFIED., .F., .F.,
 ( 4, 4 ),
 ( 8.673617379884035472E-19, 0.004050076154992999014 ),
 .UNSPECIFIED. ) ;
#37777 = CONTEXT_DEPENDENT_SHAPE_REPRESENTATION ( #57172, #59782 ) ;
#37778 = CARTESIAN_POINT ( 'NONE',  ( -6.001507490154110336, 18.84387066167321478, -0.01557731607559883699 ) ) ;
#37779 = B_SPLINE_CURVE_WITH_KNOTS ( 'NONE', 3,
 ( #17430, #36553, #24285, #33089, #28672, #23670 ),
 .UNSPECIFIED., .F., .F.,
 ( 4, 2, 4 ),
 ( 0.000000000000000000, 0.0002447195606305750714, 0.0004894391212611501427 ),
 .UNSPECIFIED. ) ;
#37780 = CARTESIAN_POINT ( 'NONE',  ( 3.680974057930773036, -35.20670187740681456, 32.59081219553969078 ) ) ;
#37781 = AXIS2_PLACEMENT_3D ( 'NONE', #53225, #48534, #29735 ) ;
#37782 = CARTESIAN_POINT ( 'NONE',  ( 5.974727161628367256, 0.01551142186621108643, 20.52494643607030156 ) ) ;
#37784 = VERTEX_POINT ( 'NONE', #45924 ) ;
#37783 = CARTESIAN_POINT ( 'NONE',  ( 3.660176727303303679, 32.61164548483971259, 35.27264088192871583 ) ) ;
#37785 = ORIENTED_EDGE ( 'NONE', *, *, #41719, .T. ) ;
#37786 = FACE_OUTER_BOUND ( 'NONE', #49399, .T. ) ;
#37787 = CARTESIAN_POINT ( 'NONE',  ( -6.077587904424778920, 3.079371755031687474, -19.00824797261030241 ) ) ;
#37788 = CARTESIAN_POINT ( 'NONE',  ( 5.860006189529246790, 9.426589201136151175, -47.30296539008815415 ) ) ;
#37789 = EDGE_CURVE ( 'NONE', #39188, #27783, #59669, .T. ) ;
#37790 = ORIENTED_EDGE ( 'NONE', *, *, #8641, .F. ) ;
#37791 = DIRECTION ( 'NONE',  ( -1.000000000000000000, -0.000000000000000000, -0.000000000000000000 ) ) ;
#37792 = CARTESIAN_POINT ( 'NONE',  ( 3.173036816750036238, 10.71375812043179643, -2.686686273116197949E-15 ) ) ;
#37793 = CARTESIAN_POINT ( 'NONE',  ( 4.975801465491694664, -45.18341283946446651, -15.94009207553035523 ) ) ;
#37794 = ADVANCED_FACE ( 'NONE', ( #60280 ), #17121, .F. ) ;
#37795 = VERTEX_POINT ( 'NONE', #31808 ) ;
#37796 = EDGE_LOOP ( 'NONE', ( #10288, #17596, #61169, #34029 ) ) ;
#37797 = CARTESIAN_POINT ( 'NONE',  ( 0.9762797500689124330, 24.45014227843030596, -34.03697001423921620 ) ) ;
#37798 = EDGE_CURVE ( 'NONE', #22653, #28122, #51290, .T. ) ;
#37799 = VECTOR ( 'NONE', #59456, 1000.000000000000000 ) ;
#37800 = CARTESIAN_POINT ( 'NONE',  ( 0.8751705887134423323, 48.08707113907594533, 0.8911681664090089772 ) ) ;
#37801 = B_SPLINE_CURVE_WITH_KNOTS ( 'NONE', 3,
 ( #58303, #36714, #55167, #44889 ),
 .UNSPECIFIED., .F., .F.,
 ( 4, 4 ),
 ( 0.000000000000000000, 0.004041751736740997747 ),
 .UNSPECIFIED. ) ;
#37802 = CARTESIAN_POINT ( 'NONE',  ( 1.231276596079887264, 25.54232633153331733, 33.23952972879620660 ) ) ;
#37803 = CARTESIAN_POINT ( 'NONE',  ( 0.6001305935487315502, -34.38748867424691014, -33.64689939321930012 ) ) ;
#37804 = CARTESIAN_POINT ( 'NONE',  ( 4.975610109902397937, -41.30423662854430944, -26.19941685746064053 ) ) ;
#37805 = CARTESIAN_POINT ( 'NONE',  ( 0.1156495703730067576, 33.68638054895946254, 28.49860906679054295 ) ) ;
#37806 = ORIENTED_EDGE ( 'NONE', *, *, #21576, .T. ) ;
#37807 = ADVANCED_FACE ( 'NONE', ( #22395 ), #23500, .F. ) ;
#37808 = CARTESIAN_POINT ( 'NONE',  ( 0.8557997880470697982, -17.48760788519248521, 44.60232077416680596 ) ) ;
#37809 = CARTESIAN_POINT ( 'NONE',  ( -6.057079549204054558, 19.09996424292739192, 2.454098005099527580 ) ) ;
#37810 = VECTOR ( 'NONE', #28425, 1000.000000000000114 ) ;
#37811 = ORIENTED_EDGE ( 'NONE', *, *, #4494, .F. ) ;
#37812 = AXIS2_PLACEMENT_3D ( 'NONE', #20998, #39830, #57949 ) ;
#37813 = CARTESIAN_POINT ( 'NONE',  ( 0.9784957157296372277, -37.50864571392711611, -18.69316863721794419 ) ) ;
#37814 = EDGE_CURVE ( 'NONE', #24133, #11002, #5638, .T. ) ;
#37815 = CARTESIAN_POINT ( 'NONE',  ( 5.896278296736517710, 0.6665948613552165058, 20.10180665774095132 ) ) ;
#37816 = CARTESIAN_POINT ( 'NONE',  ( 0.9784957157296363395, 3.963203712989006533, -41.72081103384405054 ) ) ;
#37817 = CARTESIAN_POINT ( 'NONE',  ( 0.6254311100348652896, -6.960804577577174967, 47.60023274471267740 ) ) ;
#37818 = B_SPLINE_CURVE_WITH_KNOTS ( 'NONE', 3,
 ( #7570, #26694, #2874, #22006 ),
 .UNSPECIFIED., .F., .F.,
 ( 4, 4 ),
 ( 2.142911263092167033E-17, 0.004564976165746191181 ),
 .UNSPECIFIED. ) ;
#37819 = EDGE_LOOP ( 'NONE', ( #3038, #23153, #61253, #46179 ) ) ;
#37820 = ORIENTED_EDGE ( 'NONE', *, *, #42224, .T. ) ;
#37821 = DIRECTION ( 'NONE',  ( 0.000000000000000000, 0.000000000000000000, 1.000000000000000000 ) ) ;
#37822 = FACE_BOUND ( 'NONE', #39987, .T. ) ;
#37823 = ADVANCED_FACE ( 'NONE', ( #56208 ), #29903, .F. ) ;
#37824 = DIRECTION ( 'NONE',  ( 0.09722883295013592941, -0.9646010353641026880, -0.2451354658503246409 ) ) ;
#37825 =( BOUNDED_SURFACE ( )  B_SPLINE_SURFACE ( 3, 1, ( 
 ( #1340, #39294 ),
 ( #20476, #35517 ),
 ( #6332, #25469 ),
 ( #54575, #10463 ) ),
 .UNSPECIFIED., .F., .F., .F. ) 
 B_SPLINE_SURFACE_WITH_KNOTS ( ( 4, 4 ),
 ( 2, 2 ),
 ( 0.000000000000000000, 1.000000000000000000 ),
 ( 0.000000000000000000, 1.000000000000000000 ),
 .UNSPECIFIED. ) 
 GEOMETRIC_REPRESENTATION_ITEM ( )  RATIONAL_B_SPLINE_SURFACE ( (
 ( 1.000000000000000000, 1.000000000000000000),
 ( 0.9732289882329797637, 0.9999525324661233672),
 ( 0.9732289882329797637, 0.9999525324661233672),
 ( 1.000000000000000000, 1.000000000000000000) ) ) 
 REPRESENTATION_ITEM ( '' )  SURFACE ( )  );
#37826 = EDGE_LOOP ( 'NONE', ( #57788, #49486, #24994, #33711 ) ) ;
#37827 = CARTESIAN_POINT ( 'NONE',  ( 4.553261556744875094, 43.59419396814060832, -5.393126930804686303 ) ) ;
#37828 = EDGE_LOOP ( 'NONE', ( #45548, #1762, #6592, #38476 ) ) ;
#37829 = CARTESIAN_POINT ( 'NONE',  ( 2.185380717157383135, 43.47195670229825026, 7.000627367651174993 ) ) ;
#37830 = DIRECTION ( 'NONE',  ( 0.000000000000000000, 0.000000000000000000, 1.000000000000000000 ) ) ;
#37831 = ORIENTED_EDGE ( 'NONE', *, *, #56123, .F. ) ;
#37832 = CARTESIAN_POINT ( 'NONE',  ( 0.6254087463353915632, -33.52637152047104507, 34.49952850220913803 ) ) ;
#37833 = CARTESIAN_POINT ( 'NONE',  ( 1.231276596079881047, 14.27346765619277846, 39.41503383336979027 ) ) ;
#37834 = EDGE_CURVE ( 'NONE', #35413, #13688, #2654, .T. ) ;
#37835 = VECTOR ( 'NONE', #39292, 1000.000000000000114 ) ;
#37836 = EDGE_LOOP ( 'NONE', ( #49320, #20979, #20281, #33786 ) ) ;
#37837 = CARTESIAN_POINT ( 'NONE',  ( 0.6023142530420679819, -29.49327578399161354, -38.00626667377512291 ) ) ;
#37838 = CARTESIAN_POINT ( 'NONE',  ( 4.956653778116970166, 47.94889704119054130, 3.690426056930153464 ) ) ;
#37839 = CARTESIAN_POINT ( 'NONE',  ( 5.896782393890504181, -19.39988559968486115, -5.307591317834501332 ) ) ;
#37840 = CARTESIAN_POINT ( 'NONE',  ( 0.8751705887134553219, 42.09020928323342758, 23.27176129838440488 ) ) ;
#37841 = CARTESIAN_POINT ( 'NONE',  ( 0.1097557419366048670, 16.29667732266752722, -39.92664986079716982 ) ) ;
#37842 = ORIENTED_EDGE ( 'NONE', *, *, #21394, .F. ) ;
#37843 = CARTESIAN_POINT ( 'NONE',  ( 0.6845945791218023269, -46.13320409389241661, -8.493173773402611815 ) ) ;
#37844 = CARTESIAN_POINT ( 'NONE',  ( 0.5809828226811617480, -24.41822904836953612, 41.20389530892298779 ) ) ;
#37845 = VERTEX_POINT ( 'NONE', #51198 ) ;
#37846 = CARTESIAN_POINT ( 'NONE',  ( -2.569797478183783568, 6.924386868080847357, -12.89088113963429194 ) ) ;
#37847 = CARTESIAN_POINT ( 'NONE',  ( 0.5838002273316430513, 0.1361971433784746333, -47.89576566046785899 ) ) ;
#37848 = CARTESIAN_POINT ( 'NONE',  ( 4.303969348037258058, -14.52400616872337302, -45.86537346639072865 ) ) ;
#37849 = CARTESIAN_POINT ( 'NONE',  ( 0.9740398440564312921, 5.189371650077472253, -42.59352035928881719 ) ) ;
#37850 = CARTESIAN_POINT ( 'NONE',  ( 4.967162193818130511, 42.96271701169385437, 3.259922920617894793 ) ) ;
#37851 = CARTESIAN_POINT ( 'NONE',  ( 0.6000166863083106206, 11.43688157230898383, 47.76003791465657144 ) ) ;
#37852 = CARTESIAN_POINT ( 'NONE',  ( 50.50000000000000000, 15.27178771460631168, 2.649999999999992806 ) ) ;
#37853 = DIRECTION ( 'NONE',  ( 1.000000000000000000, 6.938893907776594816E-17, -1.110223024625156540E-16 ) ) ;
#37854 = CARTESIAN_POINT ( 'NONE',  ( 1.500000000000001332, 0.000000000000000000, 0.000000000000000000 ) ) ;
#37855 = CARTESIAN_POINT ( 'NONE',  ( 4.335381028904216727, -9.909170555160370597, -47.97463065593197484 ) ) ;
#37856 = CARTESIAN_POINT ( 'NONE',  ( 0.8554163680231720024, 43.54276151446858734, 17.47092993535067151 ) ) ;
#37857 = CARTESIAN_POINT ( 'NONE',  ( 0.1100053167205930771, -5.450899213259822851, 42.77858932361494482 ) ) ;
#37858 = ORIENTED_EDGE ( 'NONE', *, *, #40400, .F. ) ;
#37859 = CARTESIAN_POINT ( 'NONE',  ( 0.1119899015040012047, 39.99500458464175523, -18.63762099805095929 ) ) ;
#37860 = CARTESIAN_POINT ( 'NONE',  ( 47.86716078833156729, 15.49703963710948784, -0.3472037173684915934 ) ) ;
#37861 = EDGE_CURVE ( 'NONE', #56788, #40746, #59497, .T. ) ;
#37862 = DIRECTION ( 'NONE',  ( -1.000000000000000000, -1.836909530733573776E-16, 1.925929944387235853E-32 ) ) ;
#37863 = CARTESIAN_POINT ( 'NONE',  ( 0.5837800005270554760, 46.47757879888824561, 6.250594182549330746 ) ) ;
#37864 = CARTESIAN_POINT ( 'NONE',  ( 0.5809828226811617480, 34.25055090842200656, -33.48000389720580472 ) ) ;
#37865 = EDGE_CURVE ( 'NONE', #61953, #58463, #16929, .T. ) ;
#37866 = ORIENTED_EDGE ( 'NONE', *, *, #52677, .F. ) ;
#37867 = CARTESIAN_POINT ( 'NONE',  ( 0.9752132459055858904, 10.88033124649678740, -41.50604997043402022 ) ) ;
#37868 = EDGE_CURVE ( 'NONE', #12199, #56380, #39338, .T. ) ;
#37869 = EDGE_CURVE ( 'NONE', #24828, #41141, #7915, .T. ) ;
#37870 = VECTOR ( 'NONE', #38915, 1000.000000000000114 ) ;
#37871 = CARTESIAN_POINT ( 'NONE',  ( -19.64296139440948252, -7.897528540900530025, -1.281472113053201856 ) ) ;
#37872 = ADVANCED_FACE ( 'NONE', ( #39923 ), #14866, .F. ) ;
#37873 = DIRECTION ( 'NONE',  ( -1.000000000000000000, -0.000000000000000000, -0.000000000000000000 ) ) ;
#37874 = VERTEX_POINT ( 'NONE', #38680 ) ;
#37875 = CARTESIAN_POINT ( 'NONE',  ( 1.154321713695931839, -25.46626713715435741, -34.54400171733326630 ) ) ;
#37876 = B_SPLINE_CURVE_WITH_KNOTS ( 'NONE', 3,
 ( #41621, #3365, #46947, #51923, #60689, #8694, #17807, #9012, #23424, #37863, #32526, #27814, #55680, #42249, #13118, #3981 ),
 .UNSPECIFIED., .F., .F.,
 ( 4, 3, 3, 3, 3, 4 ),
 ( 1.214354834101861570E-17, 0.0002732102107931890780, 0.0004098135523333805040, 0.0005464168938824999011, 0.0008195847345945434436, 0.001092771384553108301 ),
 .UNSPECIFIED. ) ;
#37877 = CARTESIAN_POINT ( 'NONE',  ( 0.5837800304671211249, 43.15703759574290643, 18.34958959048216443 ) ) ;
#37878 = ORIENTED_EDGE ( 'NONE', *, *, #19840, .F. ) ;
#37879 = EDGE_CURVE ( 'NONE', #38025, #58675, #50515, .T. ) ;
#37880 = CARTESIAN_POINT ( 'NONE',  ( 0.7764139734771222656, 37.35658946184352658, -28.36416215378391570 ) ) ;
#37881 = AXIS2_PLACEMENT_3D ( 'NONE', #56057, #31342, #3428 ) ;
#37882 = ORIENTED_EDGE ( 'NONE', *, *, #42111, .T. ) ;
#37883 = EDGE_CURVE ( 'NONE', #37650, #42525, #61696, .T. ) ;
#37884 = CARTESIAN_POINT ( 'NONE',  ( -6.017396004339687465, 17.40926186480789539, -7.209881890566363971 ) ) ;
#37885 = CARTESIAN_POINT ( 'NONE',  ( 4.549368137175248350, 0.000000000000000000, 0.000000000000000000 ) ) ;
#37886 = ORIENTED_EDGE ( 'NONE', *, *, #56024, .T. ) ;
#37887 = CARTESIAN_POINT ( 'NONE',  ( 2.643462169533613793, 40.89244134039111600, -25.20536747735737038 ) ) ;
#37888 = CARTESIAN_POINT ( 'NONE',  ( 0.8751705887134423323, 37.60752970653787486, 29.98056538504974000 ) ) ;
#37889 = CARTESIAN_POINT ( 'NONE',  ( 4.834790513006555379, -42.76900418948076776, -20.08486050647493570 ) ) ;
#37890 = CARTESIAN_POINT ( 'NONE',  ( 0.8744876279028263033, 17.78802839418742110, -45.75954650373051891 ) ) ;
#37891 = B_SPLINE_CURVE_WITH_KNOTS ( 'NONE', 3,
 ( #18011, #18321, #4180, #13620 ),
 .UNSPECIFIED., .F., .F.,
 ( 4, 4 ),
 ( 0.000000000000000000, 0.005004741218457419739 ),
 .UNSPECIFIED. ) ;
#37892 = VERTEX_POINT ( 'NONE', #19563 ) ;
#37893 = CARTESIAN_POINT ( 'NONE',  ( 0.5997462898726536595, -7.321308210775074876, -48.55872811583048332 ) ) ;
#37894 = ORIENTED_EDGE ( 'NONE', *, *, #45283, .F. ) ;
#37895 = CARTESIAN_POINT ( 'NONE',  ( 4.335381028904201628, -46.16199858719154747, 16.39593651184559064 ) ) ;
#37896 = B_SPLINE_CURVE_WITH_KNOTS ( 'NONE', 3,
 ( #4748, #61165, #24194, #48015, #57372, #365 ),
 .UNSPECIFIED., .F., .F.,
 ( 4, 2, 4 ),
 ( 2.602085213965210642E-18, 0.0002447193893791707381, 0.0004894387787583388740 ),
 .UNSPECIFIED. ) ;
#37897 = ORIENTED_EDGE ( 'NONE', *, *, #24258, .T. ) ;
#37898 = VERTEX_POINT ( 'NONE', #49278 ) ;
#37899 = CARTESIAN_POINT ( 'NONE',  ( 0.6008122571543325074, -43.00034544187082730, -23.71760616810003697 ) ) ;
#37900 = CARTESIAN_POINT ( 'NONE',  ( 0.6031356219577718170, -33.95537057546208359, 34.07882816221562905 ) ) ;
#37901 = CIRCLE ( 'NONE', #10918, 48.91267123290010943 ) ;
#37902 = CARTESIAN_POINT ( 'NONE',  ( 0.8554163680231720024, -24.47000373826209341, 40.03029340588522444 ) ) ;
#37903 = CARTESIAN_POINT ( 'NONE',  ( 2.706805983486679779, -28.71399201132674861, -33.35090367731014283 ) ) ;
#37904 = ORIENTED_EDGE ( 'NONE', *, *, #55865, .F. ) ;
#37905 = CARTESIAN_POINT ( 'NONE',  ( 0.6000166863083090663, 4.195342255947408283, -48.93079383234974244 ) ) ;
#37906 = CARTESIAN_POINT ( 'NONE',  ( 4.291220156522059348, -32.02897670715592682, 34.54755633034208984 ) ) ;
#37907 = CARTESIAN_POINT ( 'NONE',  ( 0.1156867017252034141, -38.50738325018485853, 21.54354294211074716 ) ) ;
#37909 = VERTEX_POINT ( 'NONE', #28947 ) ;
#37908 = ADVANCED_FACE ( 'NONE', ( #6331 ), #50731, .F. ) ;
#37910 = ORIENTED_EDGE ( 'NONE', *, *, #41124, .T. ) ;
#37911 = CARTESIAN_POINT ( 'NONE',  ( 0.9968887458511670463, 17.02616470386932690, -39.38692798189845945 ) ) ;
#37913 = ADVANCED_FACE ( 'NONE', ( #20787 ), #25508, .F. ) ;
#37912 = CARTESIAN_POINT ( 'NONE',  ( 4.303969348037246512, 45.86537346639057944, 14.52400616872384909 ) ) ;
#37914 = CARTESIAN_POINT ( 'NONE',  ( -6.057079549204054558, -11.01026639367717763, -15.79890075416645701 ) ) ;
#37915 = FACE_OUTER_BOUND ( 'NONE', #7872, .T. ) ;
#37916 = DIRECTION ( 'NONE',  ( -0.1011922191286467321, 0.6302926308031447933, -0.7697345869473909419 ) ) ;
#37917 = EDGE_LOOP ( 'NONE', ( #515, #45079, #51462, #23197 ) ) ;
#37918 = VECTOR ( 'NONE', #4722, 1000.000000000000114 ) ;
#37919 = ORIENTED_EDGE ( 'NONE', *, *, #45708, .F. ) ;
#37920 = CARTESIAN_POINT ( 'NONE',  ( 0.5326698147273822848, 0.000000000000000000, 8.000000000000000000 ) ) ;
#37921 = CARTESIAN_POINT ( 'NONE',  ( 48.11924514954072407, 15.45610412777417686, 1.176765604160352252 ) ) ;
#37922 = CARTESIAN_POINT ( 'NONE',  ( 1.834102595619085729, -39.00212455761993624, -20.47027173365282593 ) ) ;
#37923 = CARTESIAN_POINT ( 'NONE',  ( 0.1073791018717483448, -10.69234304550083081, 41.77800844988496465 ) ) ;
#37924 = CARTESIAN_POINT ( 'NONE',  ( -2.601141883200665639, -13.66110686928766249, -6.014115610402755330 ) ) ;
#37925 = EDGE_CURVE ( 'NONE', #2051, #44917, #11639, .T. ) ;
#37926 = ORIENTED_EDGE ( 'NONE', *, *, #44754, .T. ) ;
#37927 = CARTESIAN_POINT ( 'NONE',  ( 5.960721111146673579, 0.006321279846820317821, -20.52557019979492026 ) ) ;
#37928 = CARTESIAN_POINT ( 'NONE',  ( 5.901463166500145796, 8.479222689262201129, -18.23789058324832268 ) ) ;
#37929 = CARTESIAN_POINT ( 'NONE',  ( 5.880360259849739535, 26.61251048557248922, -39.91356965504121490 ) ) ;
#37930 = DIRECTION ( 'NONE',  ( 0.000000000000000000, 0.000000000000000000, 1.000000000000000000 ) ) ;
#37931 = CARTESIAN_POINT ( 'NONE',  ( 0.9784957157296378938, 29.30143428922444926, 29.96262681385981708 ) ) ;
#37932 = DIRECTION ( 'NONE',  ( 0.07439287786467664587, 0.3937848822959431616, -0.9161872986448684753 ) ) ;
#37933 = CARTESIAN_POINT ( 'NONE',  ( 1.231276596079881047, 19.39962232756238691, 37.16088568059176112 ) ) ;
#37934 = EDGE_CURVE ( 'NONE', #47555, #24092, #58703, .T. ) ;
#37935 =( BOUNDED_SURFACE ( )  B_SPLINE_SURFACE ( 3, 1, ( 
 ( #27863, #61056 ),
 ( #14397, #19398 ),
 ( #42914, #46994 ),
 ( #52582, #38215 ) ),
 .UNSPECIFIED., .F., .F., .F. ) 
 B_SPLINE_SURFACE_WITH_KNOTS ( ( 4, 4 ),
 ( 2, 2 ),
 ( 0.000000000000000000, 1.000000000000000000 ),
 ( 0.000000000000000000, 1.000000000000000000 ),
 .UNSPECIFIED. ) 
 GEOMETRIC_REPRESENTATION_ITEM ( )  RATIONAL_B_SPLINE_SURFACE ( (
 ( 1.000000000000000000, 1.000000000000000000),
 ( 0.7211978278499970862, 0.9934217856018976445),
 ( 0.7211978278499970862, 0.9934217856018976445),
 ( 1.000000000000000000, 1.000000000000000000) ) ) 
 REPRESENTATION_ITEM ( '' )  SURFACE ( )  );
#37936 = B_SPLINE_CURVE_WITH_KNOTS ( 'NONE', 3,
 ( #21499, #54996, #26503, #45633, #41250, #35008 ),
 .UNSPECIFIED., .F., .F.,
 ( 4, 2, 4 ),
 ( 3.529906531158615134E-18, 0.0002445244328975384866, 0.0004890488657950735037 ),
 .UNSPECIFIED. ) ;
#37937 = EDGE_CURVE ( 'NONE', #48800, #52075, #7589, .T. ) ;
#37938 = CARTESIAN_POINT ( 'NONE',  ( 4.322998006666179727, -36.74401119231429647, 30.86725474310297557 ) ) ;
#37939 = VECTOR ( 'NONE', #29808, 1000.000000000000000 ) ;
#37940 = ORIENTED_EDGE ( 'NONE', *, *, #31072, .F. ) ;
#37941 = EDGE_CURVE ( 'NONE', #50136, #36718, #40020, .T. ) ;
#37942 = AXIS2_PLACEMENT_3D ( 'NONE', #38822, #47898, #9991 ) ;
#37943 = CARTESIAN_POINT ( 'NONE',  ( 0.9722240750034584211, -39.86121765932388428, -15.88116978453023620 ) ) ;
#37944 = CARTESIAN_POINT ( 'NONE',  ( 5.958863334805807099, 17.77512673691304812, 10.26388325355093833 ) ) ;
#37945 = CARTESIAN_POINT ( 'NONE',  ( 4.956445790443998689, -16.41925925744477510, 44.13554095710679093 ) ) ;
#37946 = CARTESIAN_POINT ( 'NONE',  ( 0.3676999524040366896, -40.57213187173863389, 17.31625533148228513 ) ) ;
#37947 = EDGE_CURVE ( 'NONE', #7184, #940, #25776, .T. ) ;
#37948 = ORIENTED_EDGE ( 'NONE', *, *, #44978, .T. ) ;
#37949 = CARTESIAN_POINT ( 'NONE',  ( 43.00000000000000000, 9.184850993605153466E-15, -75.00000000000001421 ) ) ;
#37950 = CARTESIAN_POINT ( 'NONE',  ( 4.549368137175248350, 42.14271863032822552, 8.166781970325878603 ) ) ;
#37951 = ORIENTED_EDGE ( 'NONE', *, *, #28353, .F. ) ;
#37952 = CARTESIAN_POINT ( 'NONE',  ( 4.303969348037258058, 45.86537346639077839, -14.52400616872321493 ) ) ;
#37954 = AXIS2_PLACEMENT_3D ( 'NONE', #40677, #15926, #40070 ) ;
#37953 = CARTESIAN_POINT ( 'NONE',  ( 0.5832655196449136881, -45.91040371394484509, -9.563995702421170364 ) ) ;
#37955 = CARTESIAN_POINT ( 'NONE',  ( -6.078726893082806448, 17.84743921491351415, 7.229312189875837014 ) ) ;
#37956 = ORIENTED_EDGE ( 'NONE', *, *, #51612, .F. ) ;
#37957 = CARTESIAN_POINT ( 'NONE',  ( 0.6001305935487422083, -38.48510059944028683, -28.87057754790923525 ) ) ;
#37958 = VECTOR ( 'NONE', #48902, 1000.000000000000114 ) ;
#37959 = VERTEX_POINT ( 'NONE', #44925 ) ;
#37960 = FACE_BOUND ( 'NONE', #5062, .T. ) ;
#37961 = ORIENTED_EDGE ( 'NONE', *, *, #46191, .F. ) ;
#37962 = CARTESIAN_POINT ( 'NONE',  ( 0.2885700199627515561, -42.84523253167937895, -4.828949117911622402 ) ) ;
#37963 = CARTESIAN_POINT ( 'NONE',  ( 0.8760168074886960365, -44.09317760313739853, -19.22870327415288827 ) ) ;
#37964 = VERTEX_POINT ( 'NONE', #2268 ) ;
#37965 = CARTESIAN_POINT ( 'NONE',  ( 0.5807400328401637335, -47.89582301953904420, 0.5448834511088314070 ) ) ;
#37966 = EDGE_LOOP ( 'NONE', ( #43410, #8010, #52089, #5978 ) ) ;
#37967 = CARTESIAN_POINT ( 'NONE',  ( 5.895596859100789899, -19.39920506799825262, -5.310275505304632659 ) ) ;
#37968 = CARTESIAN_POINT ( 'NONE',  ( 5.896782393890504181, 8.460428369634295009, 18.24684188237239724 ) ) ;
#37969 = CARTESIAN_POINT ( 'NONE',  ( 5.917102823773431552, -7.236410236533870943, -18.76496962268603852 ) ) ;
#37970 = ORIENTED_EDGE ( 'NONE', *, *, #4294, .F. ) ;
#37971 = DIRECTION ( 'NONE',  ( 1.000000000000000000, 0.000000000000000000, 0.000000000000000000 ) ) ;
#37972 = CARTESIAN_POINT ( 'NONE',  ( 0.5997462898726536595, -39.66574928371219499, -28.95133786038212875 ) ) ;
#37973 = CARTESIAN_POINT ( 'NONE',  ( 5.960221823109900008, -7.849768660536430076, -18.96526051813977531 ) ) ;
#37974 = CARTESIAN_POINT ( 'NONE',  ( 0.1135584504625008206, -22.50320180596501984, -37.95468298662583351 ) ) ;
#37975 = VERTEX_POINT ( 'NONE', #58981 ) ;
#37976 = CARTESIAN_POINT ( 'NONE',  ( 0.5809828226811617480, -33.48000389720591841, -34.25055090842189287 ) ) ;
#37977 = CARTESIAN_POINT ( 'NONE',  ( 0.1152809850208376535, -31.54231067941225319, -30.85494967575203873 ) ) ;
#37978 = ORIENTED_EDGE ( 'NONE', *, *, #6777, .F. ) ;
#37979 = CARTESIAN_POINT ( 'NONE',  ( 0.6067099128993237445, 47.57459301987705658, 5.548253864790559930 ) ) ;
#37980 = VERTEX_POINT ( 'NONE', #22025 ) ;
#37981 = AXIS2_PLACEMENT_3D ( 'NONE', #32535, #45720, #51614 ) ;
#37982 = CARTESIAN_POINT ( 'NONE',  ( -6.016761891674564211, 18.20201388312095503, 4.873659902332430960 ) ) ;
#37983 = ADVANCED_FACE ( 'NONE', ( #26095 ), #35232, .F. ) ;
#37984 = CARTESIAN_POINT ( 'NONE',  ( 0.1064266418746774301, -41.50637583369812944, -11.70292610004310419 ) ) ;
#37985 = ORIENTED_EDGE ( 'NONE', *, *, #41327, .F. ) ;
#37986 = CARTESIAN_POINT ( 'NONE',  ( 0.5782707292762442330, 39.98024706216819624, 24.52174950030299527 ) ) ;
#37987 = CARTESIAN_POINT ( 'NONE',  ( 0.6000166863083106206, 48.97316450298212942, -3.667784109282603122 ) ) ;
#37988 = CARTESIAN_POINT ( 'NONE',  ( 4.975801465491695552, -45.18341283946470099, 15.94009207552969620 ) ) ;
#37989 = CARTESIAN_POINT ( 'NONE',  ( 0.3676999524040323597, -31.10876963919482563, -31.27610965031216139 ) ) ;
#37990 = AXIS2_PLACEMENT_3D ( 'NONE', #36434, #12630, #3193 ) ;
#37991 = VERTEX_POINT ( 'NONE', #21090 ) ;
#37992 = CARTESIAN_POINT ( 'NONE',  ( 3.407937589446178528, -2.242416846335508307, -13.51415833181190429 ) ) ;
#37993 = CARTESIAN_POINT ( 'NONE',  ( 5.894904586330512508, -15.78384355525776428, -12.46594138782911010 ) ) ;
#37994 = CARTESIAN_POINT ( 'NONE',  ( 0.6001305935487315502, 48.10757715638247589, 0.5236757026891092348 ) ) ;
#37996 = DIRECTION ( 'NONE',  ( -1.000000000000000000, -0.000000000000000000, -0.000000000000000000 ) ) ;
#37995 =( BOUNDED_SURFACE ( )  B_SPLINE_SURFACE ( 3, 1, ( 
 ( #18650, #4819 ),
 ( #56837, #33375 ),
 ( #37782, #14887 ),
 ( #23959, #13967 ) ),
 .UNSPECIFIED., .F., .F., .F. ) 
 B_SPLINE_SURFACE_WITH_KNOTS ( ( 4, 4 ),
 ( 2, 2 ),
 ( 0.000000000000000000, 1.000000000000000000 ),
 ( 0.000000000000000000, 1.000000000000000000 ),
 .UNSPECIFIED. ) 
 GEOMETRIC_REPRESENTATION_ITEM ( )  RATIONAL_B_SPLINE_SURFACE ( (
 ( 1.000000000000000000, 1.000000000000000000),
 ( 0.7269869731126821222, 0.9931720237060910339),
 ( 0.7269869731126821222, 0.9931720237060910339),
 ( 1.000000000000000000, 1.000000000000000000) ) ) 
 REPRESENTATION_ITEM ( '' )  SURFACE ( )  );
#37997 = B_SPLINE_CURVE_WITH_KNOTS ( 'NONE', 3,
 ( #15190, #34293, #53371, #10482, #29577, #35222 ),
 .UNSPECIFIED., .F., .F.,
 ( 4, 2, 4 ),
 ( 1.266058488688919593E-17, 0.0002448709889506549340, 0.0004897419779012971829 ),
 .UNSPECIFIED. ) ;
#37998 = FACE_OUTER_BOUND ( 'NONE', #28435, .T. ) ;
#37999 = CARTESIAN_POINT ( 'NONE',  ( 3.661933894777871679, -26.87748316552291783, 38.60352397953695913 ) ) ;
#38000 = CARTESIAN_POINT ( 'NONE',  ( 0.8751705887134553219, 29.98056538504910051, 37.60752970653838645 ) ) ;
#38001 = CIRCLE ( 'NONE', #59958, 0.05882000000000109363 ) ;
#38002 = CARTESIAN_POINT ( 'NONE',  ( 5.959828726073459926, 19.82738831247213440, -5.308046411395043407 ) ) ;
#38003 = CARTESIAN_POINT ( 'NONE',  ( 5.896782393890504181, -4.656380635072583374, -19.56640504178867346 ) ) ;
#38004 = CARTESIAN_POINT ( 'NONE',  ( 0.1087620492084204610, -21.87505161834442902, 37.16461718700628580 ) ) ;
#38005 = DIRECTION ( 'NONE',  ( -1.000000000000000000, -0.000000000000000000, -0.000000000000000000 ) ) ;
#38006 = CARTESIAN_POINT ( 'NONE',  ( 3.407937589446178528, 12.08659953757608818, 6.447869442558206821 ) ) ;
#38007 = B_SPLINE_CURVE_WITH_KNOTS ( 'NONE', 3,
 ( #33013, #71, #13910, #24203, #52085, #61174 ),
 .UNSPECIFIED., .F., .F.,
 ( 4, 2, 4 ),
 ( 0.000000000000000000, 0.0002291966416970780756, 0.0004583932833941561512 ),
 .UNSPECIFIED. ) ;
#38008 = EDGE_CURVE ( 'NONE', #53492, #8960, #26399, .T. ) ;
#38009 =( BOUNDED_SURFACE ( )  B_SPLINE_SURFACE ( 3, 1, ( 
 ( #1206, #4649 ),
 ( #9377, #19416 ),
 ( #23799, #29110 ),
 ( #43542, #587 ) ),
 .UNSPECIFIED., .F., .F., .F. ) 
 B_SPLINE_SURFACE_WITH_KNOTS ( ( 4, 4 ),
 ( 2, 2 ),
 ( 0.000000000000000000, 1.000000000000000000 ),
 ( 0.000000000000000000, 1.000000000000000000 ),
 .UNSPECIFIED. ) 
 GEOMETRIC_REPRESENTATION_ITEM ( )  RATIONAL_B_SPLINE_SURFACE ( (
 ( 1.000000000000000000, 1.000000000000000000),
 ( 0.7211978278499970862, 0.9934217856018976445),
 ( 0.7211978278499970862, 0.9934217856018976445),
 ( 1.000000000000000000, 1.000000000000000000) ) ) 
 REPRESENTATION_ITEM ( '' )  SURFACE ( )  );
#38010 = CARTESIAN_POINT ( 'NONE',  ( 0.9757402383260936896, -37.11731350497343840, -21.52772413548522223 ) ) ;
#38011 = EDGE_CURVE ( 'NONE', #4544, #15054, #31778, .T. ) ;
#38012 = CARTESIAN_POINT ( 'NONE',  ( 2.301430502907644726, 11.18388433759652578, 46.71331171933237414 ) ) ;
#38013 = CARTESIAN_POINT ( 'NONE',  ( 0.1119898979215348395, 20.90518435893999083, 38.85787661685284888 ) ) ;
#38014 = ORIENTED_EDGE ( 'NONE', *, *, #47110, .F. ) ;
#38015 = DIRECTION ( 'NONE',  ( 0.000000000000000000, 0.000000000000000000, 1.000000000000000000 ) ) ;
#38016 = CARTESIAN_POINT ( 'NONE',  ( 0.5987334363312692975, 5.317554374040649456, -48.81891561629772980 ) ) ;
#38017 = CARTESIAN_POINT ( 'NONE',  ( 45.00000000000001421, 2.163354392537210416E-30, 75.00000000000001421 ) ) ;
#38018 = EDGE_CURVE ( 'NONE', #759, #19623, #21344, .T. ) ;
#38019 = ORIENTED_EDGE ( 'NONE', *, *, #25784, .T. ) ;
#38020 = CARTESIAN_POINT ( 'NONE',  ( 4.963659409799332067, 25.25989740981550113, -36.94443854030191687 ) ) ;
#38021 = DIRECTION ( 'NONE',  ( 1.000000000000000000, 1.836909530733573776E-16, 0.000000000000000000 ) ) ;
#38022 = B_SPLINE_CURVE_WITH_KNOTS ( 'NONE', 3,
 ( #25138, #26684, #16999, #60189 ),
 .UNSPECIFIED., .F., .F.,
 ( 4, 4 ),
 ( 0.000000000000000000, 0.004442905043737212234 ),
 .UNSPECIFIED. ) ;
#38023 = VERTEX_POINT ( 'NONE', #55203 ) ;
#38024 =( REPRESENTATION_RELATIONSHIP ('NONE','NONE', #44881, #13 ) REPRESENTATION_RELATIONSHIP_WITH_TRANSFORMATION ( #23643 )SHAPE_REPRESENTATION_RELATIONSHIP( ) );
#38025 = VERTEX_POINT ( 'NONE', #48559 ) ;
#38026 = DIRECTION ( 'NONE',  ( 1.836909530733573776E-16, -1.000000000000000000, 0.000000000000000000 ) ) ;
#38027 = VERTEX_POINT ( 'NONE', #16287 ) ;
#38028 = EDGE_CURVE ( 'NONE', #29080, #32390, #51167, .T. ) ;
#38029 = AXIS2_PLACEMENT_3D ( 'NONE', #53465, #57225, #43184 ) ;
#38030 = CARTESIAN_POINT ( 'NONE',  ( 4.834790513006553603, -22.26269597880833473, 41.67687258755787383 ) ) ;
#38032 = CARTESIAN_POINT ( 'NONE',  ( 0.6001305935487315502, 24.50730504006458332, -41.40054608060268038 ) ) ;
#38031 = B_SPLINE_CURVE_WITH_KNOTS ( 'NONE', 3,
 ( #48900, #30092, #10389, #5950, #25712, #34201 ),
 .UNSPECIFIED., .F., .F.,
 ( 4, 2, 4 ),
 ( 1.506204625983992411E-16, 0.0002445252820015209245, 0.0004890505640028912533 ),
 .UNSPECIFIED. ) ;
#38033 = EDGE_LOOP ( 'NONE', ( #26424, #11490, #14633, #17123 ) ) ;
#38034 = ORIENTED_EDGE ( 'NONE', *, *, #50693, .T. ) ;
#38035 = CARTESIAN_POINT ( 'NONE',  ( -6.078726893082806448, -17.34758611460008382, 8.357948149232223400 ) ) ;
#38037 = EDGE_LOOP ( 'NONE', ( #12163, #29024, #22523, #8387 ) ) ;
#38036 = ADVANCED_FACE ( 'NONE', ( #10668 ), #44039, .F. ) ;
#38038 = CARTESIAN_POINT ( 'NONE',  ( 0.1119899015040013435, -23.35186486751172552, 37.43863933694675694 ) ) ;
#38039 = CARTESIAN_POINT ( 'NONE',  ( 4.553261556744873317, 35.06776520399894537, -26.45357082552063233 ) ) ;
#38040 = CARTESIAN_POINT ( 'NONE',  ( -6.001507490154110336, 18.20581304543297918, 4.862106078787989283 ) ) ;
#38041 = ORIENTED_EDGE ( 'NONE', *, *, #53130, .T. ) ;
#38042 = CARTESIAN_POINT ( 'NONE',  ( 0.5998501479064699549, -44.64337787626236320, -17.92509395669093308 ) ) ;
#38043 = CARTESIAN_POINT ( 'NONE',  ( 0.9769922540276041456, -39.73250790563689350, 13.32889232511943511 ) ) ;
#38044 = EDGE_LOOP ( 'NONE', ( #8894, #33507, #4912, #956 ) ) ;
#38045 = ORIENTED_EDGE ( 'NONE', *, *, #7265, .F. ) ;
#38046 = CARTESIAN_POINT ( 'NONE',  ( 0.6000166863083106206, 41.44150143800037966, 26.35195325346237283 ) ) ;
#38047 = AXIS2_PLACEMENT_3D ( 'NONE', #2042, #21172, #21475 ) ;
#38048 = VERTEX_POINT ( 'NONE', #1860 ) ;
#38049 = CARTESIAN_POINT ( 'NONE',  ( 2.009741617377216460, 34.40621083346663767, 27.49030253936991741 ) ) ;
#38050 = CARTESIAN_POINT ( 'NONE',  ( 0.9730545539215883499, 36.90443313492330901, 21.89037132892449478 ) ) ;
#38051 = DIRECTION ( 'NONE',  ( -0.1736481776669312471, 0.9848077530122077983, -5.551115123125779621E-17 ) ) ;
#38052 = CARTESIAN_POINT ( 'NONE',  ( 0.1092355843206037486, 5.330717085612747042, 42.79374386763048221 ) ) ;
#38053 = ORIENTED_EDGE ( 'NONE', *, *, #11377, .F. ) ;
#38054 = CARTESIAN_POINT ( 'NONE',  ( -6.015611763856276717, -4.870987357968304288, 18.20278301740935234 ) ) ;
#38055 = DIRECTION ( 'NONE',  ( 0.000000000000000000, 0.000000000000000000, 1.000000000000000000 ) ) ;
#38056 = CARTESIAN_POINT ( 'NONE',  ( 0.5830081025819940921, 36.63399018927692907, -29.27768428674311352 ) ) ;
#38057 = EDGE_CURVE ( 'NONE', #45571, #29832, #41780, .T. ) ;
#38058 = VERTEX_POINT ( 'NONE', #24445 ) ;
#38059 = CARTESIAN_POINT ( 'NONE',  ( 4.962356264823597485, -9.332162870646813602, 41.03835198954837438 ) ) ;
#38060 = DIRECTION ( 'NONE',  ( 0.000000000000000000, 0.000000000000000000, 1.000000000000000000 ) ) ;
#38061 = CARTESIAN_POINT ( 'NONE',  ( 0.6254311100348658448, 46.64066536338342672, -11.78487556908959988 ) ) ;
#38062 = ORIENTED_EDGE ( 'NONE', *, *, #11055, .F. ) ;
#38063 = ORIENTED_EDGE ( 'NONE', *, *, #52505, .T. ) ;
#38064 = CARTESIAN_POINT ( 'NONE',  ( 4.553261556744875094, 0.000000000000000000, 0.000000000000000000 ) ) ;
#38065 = CARTESIAN_POINT ( 'NONE',  ( 0.7048096507298579061, -48.10291524268441066, -0.8437160066905596834 ) ) ;
#38066 = CARTESIAN_POINT ( 'NONE',  ( 4.956445790443993360, 20.31112743693043399, 42.48524629068788983 ) ) ;
#38067 = FACE_OUTER_BOUND ( 'NONE', #44758, .T. ) ;
#38068 = CARTESIAN_POINT ( 'NONE',  ( -6.016761891674565099, -11.47373234755513671, 14.94721834528410831 ) ) ;
#38069 = CARTESIAN_POINT ( 'NONE',  ( 0.9752570700956801897, -42.57087745267993739, 5.371905812151998028 ) ) ;
#38070 = CARTESIAN_POINT ( 'NONE',  ( 2.624215991343620935, -22.77108897942165910, 42.26352390376089829 ) ) ;
#38071 = CARTESIAN_POINT ( 'NONE',  ( 0.1073791018717578927, -30.83464511437158961, 30.14884492832337060 ) ) ;
#38072 = FACE_OUTER_BOUND ( 'NONE', #44227, .T. ) ;
#38073 = CARTESIAN_POINT ( 'NONE',  ( 2.648799415243708655, -48.43667485455544863, 7.642381325455785301 ) ) ;
#38074 = CARTESIAN_POINT ( 'NONE',  ( 0.1129192098497447394, -22.45785791439742241, 37.98152716363431125 ) ) ;
#38075 = CARTESIAN_POINT ( 'NONE',  ( 0.5850706913938533704, 12.22095376872036532, 46.31100969101492382 ) ) ;
#38076 = EDGE_LOOP ( 'NONE', ( #16170, #309, #54174, #27623 ) ) ;
#38077 = CARTESIAN_POINT ( 'NONE',  ( 2.299652685299201860, -38.51197436690490150, -30.34978674094784523 ) ) ;
#38078 = CARTESIAN_POINT ( 'NONE',  ( -6.078726893082806448, 0.6205993875982012131, 19.24600991553399254 ) ) ;
#38079 = CARTESIAN_POINT ( 'NONE',  ( 0.1157991065609915576, -35.31295772492552487, -26.45632972003714656 ) ) ;
#38080 = CARTESIAN_POINT ( 'NONE',  ( 3.783198216974383854, 24.80909581868442615, 35.16829104054179567 ) ) ;
#38081 = B_SPLINE_CURVE_WITH_KNOTS ( 'NONE', 3,
 ( #17302, #7564, #26688, #41132 ),
 .UNSPECIFIED., .F., .F.,
 ( 4, 4 ),
 ( 0.000000000000000000, 0.004444103432399267896 ),
 .UNSPECIFIED. ) ;
#38082 = CARTESIAN_POINT ( 'NONE',  ( 4.967162193818130511, 2.375726030843182457, -43.02067033766016380 ) ) ;
#38083 = CARTESIAN_POINT ( 'NONE',  ( 0.9972139404380321315, -39.38665787682673880, 17.02682566833171052 ) ) ;
#38084 = FACE_OUTER_BOUND ( 'NONE', #12238, .T. ) ;
#38085 = VECTOR ( 'NONE', #46109, 1000.000000000000114 ) ;
#38086 = CARTESIAN_POINT ( 'NONE',  ( 0.8744876279028263033, 48.35212675551510841, -8.510105087370661181 ) ) ;
#38087 = CARTESIAN_POINT ( 'NONE',  ( 0.5839880159502324197, 12.35255585954184276, 46.27569712847341066 ) ) ;
#38088 = EDGE_CURVE ( 'NONE', #21206, #60545, #43582, .T. ) ;
#38089 = LINE ( 'NONE', #52760, #33456 ) ;
#38091 = VERTEX_POINT ( 'NONE', #10984 ) ;
#38090 = CARTESIAN_POINT ( 'NONE',  ( 0.6031356755773454870, -46.46822857981034360, -12.45109777649093274 ) ) ;
#38092 = ORIENTED_EDGE ( 'NONE', *, *, #28269, .F. ) ;
#38093 = AXIS2_PLACEMENT_3D ( 'NONE', #16807, #50299, #14843 ) ;
#38094 = DIRECTION ( 'NONE',  ( 0.000000000000000000, 0.000000000000000000, 1.000000000000000000 ) ) ;
#38095 = CARTESIAN_POINT ( 'NONE',  ( 2.282816707992308736, -43.92595909538881926, 16.64352979263095733 ) ) ;
#38096 = FACE_OUTER_BOUND ( 'NONE', #29271, .T. ) ;
#38097 = EDGE_CURVE ( 'NONE', #25828, #18062, #43001, .T. ) ;
#38098 = VERTEX_POINT ( 'NONE', #57940 ) ;
#38099 = CARTESIAN_POINT ( 'NONE',  ( -6.072942160501519915, -18.89839206595250687, 3.695259072184732929 ) ) ;
#38100 = CARTESIAN_POINT ( 'NONE',  ( 0.5809828226811553087, 37.66417181417592275, -29.58751527316140795 ) ) ;
#38101 = CARTESIAN_POINT ( 'NONE',  ( 2.281448460670575606, 28.15071835136453515, -38.84544723616112805 ) ) ;
#38102 = EDGE_CURVE ( 'NONE', #10248, #41488, #20375, .T. ) ;
#38103 = ORIENTED_EDGE ( 'NONE', *, *, #2749, .F. ) ;
#38104 = VERTEX_POINT ( 'NONE', #39818 ) ;
#38105 = CARTESIAN_POINT ( 'NONE',  ( 3.407937589446178528, -8.699069120706699465, -10.58239600294647609 ) ) ;
#38106 = CARTESIAN_POINT ( 'NONE',  ( 5.959828726073459926, 7.858992891709871031, 18.96145866559674786 ) ) ;
#38107 = CARTESIAN_POINT ( 'NONE',  ( 0.5832655196449118007, 17.06701948983755557, -43.68011021857475384 ) ) ;
#38108 =( BOUNDED_SURFACE ( )  B_SPLINE_SURFACE ( 3, 1, ( 
 ( #8177, #21986 ),
 ( #45811, #41419 ),
 ( #16351, #59244 ),
 ( #17593, #35476 ) ),
 .UNSPECIFIED., .F., .F., .F. ) 
 B_SPLINE_SURFACE_WITH_KNOTS ( ( 4, 4 ),
 ( 2, 2 ),
 ( 0.000000000000000000, 1.000000000000000000 ),
 ( 0.000000000000000000, 1.000000000000000000 ),
 .UNSPECIFIED. ) 
 GEOMETRIC_REPRESENTATION_ITEM ( )  RATIONAL_B_SPLINE_SURFACE ( (
 ( 1.000000000000000000, 1.000000000000000000),
 ( 0.7211978278499968642, 0.9934217856018975334),
 ( 0.7211978278499968642, 0.9934217856018975334),
 ( 1.000000000000000000, 1.000000000000000000) ) ) 
 REPRESENTATION_ITEM ( '' )  SURFACE ( )  );
#38109 = ADVANCED_FACE ( 'NONE', ( #25682 ), #22774, .F. ) ;
#38110 = CARTESIAN_POINT ( 'NONE',  ( 5.895881250540457863, 14.91370150166942388, 13.49478377475549173 ) ) ;
#38111 = CARTESIAN_POINT ( 'NONE',  ( 1.114299999999999846, 0.000000000000000000, 0.000000000000000000 ) ) ;
#38112 = FACE_OUTER_BOUND ( 'NONE', #20204, .T. ) ;
#38113 = EDGE_LOOP ( 'NONE', ( #26414, #57798, #19213, #47886 ) ) ;
#38114 = DIRECTION ( 'NONE',  ( 0.000000000000000000, -0.7071067811865461294, -0.7071067811865487940 ) ) ;
#38115 = CARTESIAN_POINT ( 'NONE',  ( 3.727782113643637096, 43.95811118998071976, 0.6798797800101179512 ) ) ;
#38116 = EDGE_LOOP ( 'NONE', ( #19759, #22397, #37180, #26181 ) ) ;
#38117 = CARTESIAN_POINT ( 'NONE',  ( 0.9762797500689124330, -37.62962005162893320, -18.44821075215020656 ) ) ;
#38118 = DIRECTION ( 'NONE',  ( 0.000000000000000000, -1.224646799147332007E-16, 1.000000000000000000 ) ) ;
#38119 = CARTESIAN_POINT ( 'NONE',  ( -2.708315649062910779, 14.06540004355476903, 4.041664582652845006 ) ) ;
#38120 = CARTESIAN_POINT ( 'NONE',  ( 0.8744876279028306332, 46.30617036199629410, -16.31222353896820110 ) ) ;
#38121 = EDGE_LOOP ( 'NONE', ( #37664, #11514, #43557, #28886 ) ) ;
#38122 = VERTEX_POINT ( 'NONE', #15375 ) ;
#38123 = CARTESIAN_POINT ( 'NONE',  ( 0.3622758884714600280, 34.70015533914828865, -25.58609868863731407 ) ) ;
#38124 = CARTESIAN_POINT ( 'NONE',  ( 0.9730545539215883499, 10.61654491617622398, -41.57420493492374192 ) ) ;
#38125 = CARTESIAN_POINT ( 'NONE',  ( 0.8554163680231708922, -18.91615390926475726, -42.93465493506180053 ) ) ;
#38126 = VECTOR ( 'NONE', #40528, 1000.000000000000114 ) ;
#38127 = ORIENTED_EDGE ( 'NONE', *, *, #2000, .T. ) ;
#38128 = CARTESIAN_POINT ( 'NONE',  ( 4.956653778116990594, 2.599733001515011743, -48.02038484091096393 ) ) ;
#38129 = ORIENTED_EDGE ( 'NONE', *, *, #9772, .F. ) ;
#38130 = CARTESIAN_POINT ( 'NONE',  ( 4.834790513006555379, -15.88524143731160088, 44.49998253261117043 ) ) ;
#38131 = CARTESIAN_POINT ( 'NONE',  ( 4.975610109902397937, -40.67634447773618689, 27.16402781375239073 ) ) ;
#38132 = ORIENTED_EDGE ( 'NONE', *, *, #44443, .T. ) ;
#38133 = CARTESIAN_POINT ( 'NONE',  ( 0.8554163680231708922, 40.82560365045097228, -23.11872746688499802 ) ) ;
#38134 = EDGE_CURVE ( 'NONE', #10258, #48557, #43755, .T. ) ;
#38135 = CARTESIAN_POINT ( 'NONE',  ( 5.896782393890504181, 0.6657210432558627877, -20.10181341000305366 ) ) ;
#38136 = CARTESIAN_POINT ( 'NONE',  ( 0.9757787079277450148, 26.15233402543316288, -34.01751575780794923 ) ) ;
#38137 = B_SPLINE_CURVE_WITH_KNOTS ( 'NONE', 3,
 ( #29656, #1141, #20278, #1438 ),
 .UNSPECIFIED., .F., .F.,
 ( 4, 4 ),
 ( 0.000000000000000000, 0.005004948556313796627 ),
 .UNSPECIFIED. ) ;
#38139 = ORIENTED_EDGE ( 'NONE', *, *, #1404, .F. ) ;
#38138 = EDGE_CURVE ( 'NONE', #27827, #12730, #48264, .T. ) ;
#38140 = CARTESIAN_POINT ( 'NONE',  ( 0.5997462898726536595, -1.051648045106814422, -49.09628974305016413 ) ) ;
#38141 = FACE_OUTER_BOUND ( 'NONE', #28225, .T. ) ;
#38142 = CARTESIAN_POINT ( 'NONE',  ( -6.078075953587585900, -8.911363828324688541, -17.06993757945125623 ) ) ;
#38143 = CARTESIAN_POINT ( 'NONE',  ( 5.901764892641288895, -37.25947723020453850, 31.77613607680373420 ) ) ;
#38144 = CARTESIAN_POINT ( 'NONE',  ( 0.8557997880470599172, -44.60232077416698360, 17.48760788519201981 ) ) ;
#38145 = ORIENTED_EDGE ( 'NONE', *, *, #12902, .F. ) ;
#38146 = EDGE_CURVE ( 'NONE', #44906, #2290, #29542, .T. ) ;
#38147 = CARTESIAN_POINT ( 'NONE',  ( 2.879087469061463178, -16.21381997011050657, 40.90493513942082160 ) ) ;
#38148 = ORIENTED_EDGE ( 'NONE', *, *, #25673, .F. ) ;
#38149 = CARTESIAN_POINT ( 'NONE',  ( 0.6067099128993241886, 38.42667919752404515, 28.59222530349236990 ) ) ;
#38150 = CARTESIAN_POINT ( 'NONE',  ( 5.917102823773431552, -19.93133248418633485, -2.689182674449699384 ) ) ;
#38151 = B_SPLINE_CURVE_WITH_KNOTS ( 'NONE', 3,
 ( #32867, #51943, #47260, #56948 ),
 .UNSPECIFIED., .F., .F.,
 ( 4, 4 ),
 ( 2.414736334504793503E-17, 0.004564976165746186844 ),
 .UNSPECIFIED. ) ;
#38152 = CARTESIAN_POINT ( 'NONE',  ( 5.917102823773431552, 14.92182362672981810, 13.48439459911010374 ) ) ;
#38153 = CARTESIAN_POINT ( 'NONE',  ( -6.016489644550736315, -7.215050741357911690, -17.40716454747936481 ) ) ;
#38154 = DIRECTION ( 'NONE',  ( 0.000000000000000000, 0.000000000000000000, 1.000000000000000000 ) ) ;
#38155 = CARTESIAN_POINT ( 'NONE',  ( -6.079354080745853928, -4.283721817891188444, -18.77345686428274618 ) ) ;
#38156 = DIRECTION ( 'NONE',  ( 0.9848077530122080203, 0.09698383872753962853, 0.1440410519008961665 ) ) ;
#38157 = CARTESIAN_POINT ( 'NONE',  ( 0.9968887458511649369, -41.61262323391479612, 10.46947792236080410 ) ) ;
#38158 = FACE_OUTER_BOUND ( 'NONE', #32798, .T. ) ;
#38159 = ADVANCED_FACE ( 'NONE', ( #2479 ), #7705, .F. ) ;
#38160 = DIRECTION ( 'NONE',  ( 0.000000000000000000, 0.000000000000000000, 1.000000000000000000 ) ) ;
#38162 = ORIENTED_EDGE ( 'NONE', *, *, #2185, .F. ) ;
#38161 = CARTESIAN_POINT ( 'NONE',  ( 0.1092565886968784455, -5.321013289171980354, 42.79503959566643800 ) ) ;
#38163 = ORIENTED_EDGE ( 'NONE', *, *, #28670, .T. ) ;
#38164 = CARTESIAN_POINT ( 'NONE',  ( 0.1129192098497455998, 29.30421273086464140, 32.98810246148426728 ) ) ;
#38165 = CARTESIAN_POINT ( 'NONE',  ( 5.960221823109900008, -20.52559243573973546, -0.005450390361650292448 ) ) ;
#38166 = EDGE_CURVE ( 'NONE', #47447, #42648, #59378, .T. ) ;
#38167 = CARTESIAN_POINT ( 'NONE',  ( 58.00000000000000000, 8.437969416220405915E-15, -2.995852231480068572E-16 ) ) ;
#38168 = CARTESIAN_POINT ( 'NONE',  ( 0.9757787079277434605, 42.54650880470572361, -5.561523338226725954 ) ) ;
#38169 = CARTESIAN_POINT ( 'NONE',  ( 3.390910168358336474, 32.17648676134584917, -29.97950693774952313 ) ) ;
#38170 = ADVANCED_FACE ( 'NONE', ( #36343 ), #28807, .F. ) ;
#38171 = AXIS2_PLACEMENT_3D ( 'NONE', #49215, #11319, #25407 ) ;
#38172 = ORIENTED_EDGE ( 'NONE', *, *, #19888, .T. ) ;
#38173 = CARTESIAN_POINT ( 'NONE',  ( 4.303969348037258058, -45.22910199346963367, -16.39840148505139794 ) ) ;
#38174 = CARTESIAN_POINT ( 'NONE',  ( 0.1313383488274136313, -10.54394128763588157, 41.81465294768271690 ) ) ;
#38175 = CARTESIAN_POINT ( 'NONE',  ( 4.833616638992205949, 9.466882727842142131, -45.27110352095237999 ) ) ;
#38176 = ORIENTED_EDGE ( 'NONE', *, *, #60144, .F. ) ;
#38177 = EDGE_CURVE ( 'NONE', #20273, #722, #11588, .T. ) ;
#38178 = CARTESIAN_POINT ( 'NONE',  ( 0.5817217712918331118, 42.99501725333171009, 18.72600986313105409 ) ) ;
#38179 = DIRECTION ( 'NONE',  ( 0.000000000000000000, 0.000000000000000000, 1.000000000000000000 ) ) ;
#38180 =( BOUNDED_SURFACE ( )  B_SPLINE_SURFACE ( 3, 1, ( 
 ( #6476, #35043 ),
 ( #39752, #50048 ),
 ( #25013, #26227 ),
 ( #7102, #44456 ) ),
 .UNSPECIFIED., .F., .F., .F. ) 
 B_SPLINE_SURFACE_WITH_KNOTS ( ( 4, 4 ),
 ( 2, 2 ),
 ( 0.000000000000000000, 1.000000000000000000 ),
 ( 0.000000000000000000, 1.000000000000000000 ),
 .UNSPECIFIED. ) 
 GEOMETRIC_REPRESENTATION_ITEM ( )  RATIONAL_B_SPLINE_SURFACE ( (
 ( 1.000000000000000000, 1.000000000000000000),
 ( 0.7223157951917476005, 0.9931996967497186413),
 ( 0.7223157951917476005, 0.9931996967497186413),
 ( 1.000000000000000000, 1.000000000000000000) ) ) 
 REPRESENTATION_ITEM ( '' )  SURFACE ( )  );
#38181 = ORIENTED_EDGE ( 'NONE', *, *, #48205, .T. ) ;
#38182 = CARTESIAN_POINT ( 'NONE',  ( 4.975610109902397937, -46.59897809419034331, -14.86555238512655919 ) ) ;
#38183 = ORIENTED_EDGE ( 'NONE', *, *, #32189, .F. ) ;
#38184 = CARTESIAN_POINT ( 'NONE',  ( 0.8751705887134553219, -13.30665218149330364, -46.21789262997752701 ) ) ;
#38185 = CARTESIAN_POINT ( 'NONE',  ( -6.016761891674564211, 7.207804629151548070, -17.41015286184795130 ) ) ;
#38186 = ORIENTED_EDGE ( 'NONE', *, *, #50456, .F. ) ;
#38187 = LINE ( 'NONE', #39112, #43535 ) ;
#38188 = DIRECTION ( 'NONE',  ( 0.000000000000000000, 0.000000000000000000, -1.000000000000000000 ) ) ;
#38189 = CARTESIAN_POINT ( 'NONE',  ( 0.6253024248130484297, -48.61070664296096311, -6.960131255201589262 ) ) ;
#38190 = CARTESIAN_POINT ( 'NONE',  ( 0.5809828226811617480, -38.32755012159166341, 28.72298383114474518 ) ) ;
#38191 = B_SPLINE_CURVE_WITH_KNOTS ( 'NONE', 3,
 ( #48799, #38496, #25003, #1470 ),
 .UNSPECIFIED., .F., .F.,
 ( 4, 4 ),
 ( 5.553824967135426632E-18, 0.004566006591234647236 ),
 .UNSPECIFIED. ) ;
#38192 = ORIENTED_EDGE ( 'NONE', *, *, #16811, .T. ) ;
#38193 = CARTESIAN_POINT ( 'NONE',  ( 0.9772918015221170318, -7.379427770854193547, -41.25385923190006565 ) ) ;
#38194 = EDGE_LOOP ( 'NONE', ( #17963, #3163, #43563, #807 ) ) ;
#38195 = CARTESIAN_POINT ( 'NONE',  ( 3.661933894777874343, -43.78265458920037645, -17.19622987966910088 ) ) ;
#38196 = EDGE_LOOP ( 'NONE', ( #41185, #48620, #42556, #53268 ) ) ;
#38197 = ORIENTED_EDGE ( 'NONE', *, *, #32618, .F. ) ;
#38198 = CARTESIAN_POINT ( 'NONE',  ( 0.6026112563231247332, -42.70250234240587162, -24.24948017176923543 ) ) ;
#38199 = CARTESIAN_POINT ( 'NONE',  ( 0.9775691876210965692, -37.57309490400189844, 18.56330380952859471 ) ) ;
#38200 = ADVANCED_FACE ( 'NONE', ( #31935 ), #9978, .F. ) ;
#38201 = LINE ( 'NONE', #19386, #8246 ) ;
#38202 = CARTESIAN_POINT ( 'NONE',  ( 5.959828726073459926, 16.28681682518047324, 12.49160845136040621 ) ) ;
#38203 = ORIENTED_EDGE ( 'NONE', *, *, #28940, .T. ) ;
#38204 = CARTESIAN_POINT ( 'NONE',  ( 0.9745511491811736926, 0.3405614984926567113, -42.90705396078546130 ) ) ;
#38205 = EDGE_CURVE ( 'NONE', #49729, #58534, #2575, .T. ) ;
#38206 = CARTESIAN_POINT ( 'NONE',  ( 0.9730545539215883499, -29.98130006528840141, -30.69604515769682251 ) ) ;
#38207 = CARTESIAN_POINT ( 'NONE',  ( 2.301529144917016101, -37.31001381748753687, 30.25186323939210453 ) ) ;
#38208 = ORIENTED_EDGE ( 'NONE', *, *, #52891, .T. ) ;
#38209 = VECTOR ( 'NONE', #20232, 1000.000000000000227 ) ;
#38210 = ADVANCED_FACE ( 'NONE', ( #20137 ), #14759, .T. ) ;
#38211 = ORIENTED_EDGE ( 'NONE', *, *, #10325, .F. ) ;
#38212 = AXIS2_PLACEMENT_3D ( 'NONE', #1672, #41404, #20813 ) ;
#38213 = DIRECTION ( 'NONE',  ( 0.09835009131224567436, 0.9876177374393975139, -0.1222230102474909375 ) ) ;
#38214 = CARTESIAN_POINT ( 'NONE',  ( 0.1100053167205930493, 30.62023953839040047, 30.36644426605150215 ) ) ;
#38215 = CARTESIAN_POINT ( 'NONE',  ( 5.901764892641288895, 42.68902166415562505, 23.99247583716464760 ) ) ;
#38216 = CARTESIAN_POINT ( 'NONE',  ( 0.9787284016396609054, 38.65591695182520482, 16.18814638994915711 ) ) ;
#38217 = ORIENTED_EDGE ( 'NONE', *, *, #29823, .T. ) ;
#38218 = EDGE_CURVE ( 'NONE', #31834, #31616, #24722, .T. ) ;
#38219 = EDGE_CURVE ( 'NONE', #54223, #61565, #1138, .T. ) ;
#38220 = EDGE_LOOP ( 'NONE', ( #37919, #33149, #5366, #45421 ) ) ;
#38221 = CARTESIAN_POINT ( 'NONE',  ( 1.827326673878743257, -42.50320212329575043, -6.839036141888421128 ) ) ;
#38222 = CARTESIAN_POINT ( 'NONE',  ( 0.9784957157296372277, -41.02185128615600007, 8.575591760856571710 ) ) ;
#38223 = CARTESIAN_POINT ( 'NONE',  ( 1.479689385636123067, -38.95645166531898695, -20.59074352507356664 ) ) ;
#38224 = DIRECTION ( 'NONE',  ( 0.07500201931887538753, -0.9970919462213602147, -0.01350362464641113522 ) ) ;
#38225 = CARTESIAN_POINT ( 'NONE',  ( 1.091591847532195514, 41.90644475422998028, 0.7803070014481171546 ) ) ;
#38226 = FILL_AREA_STYLE ('',( #15333 ) ) ;
#38227 = CARTESIAN_POINT ( 'NONE',  ( 0.6017666602106489515, 0.3491145841132096694, 48.10631669010027878 ) ) ;
#38228 = EDGE_CURVE ( 'NONE', #19345, #47387, #4115, .T. ) ;
#38229 = VERTEX_POINT ( 'NONE', #693 ) ;
#38230 = CARTESIAN_POINT ( 'NONE',  ( 0.6039202388192952409, 48.99530948556955678, 3.320144765254842145 ) ) ;
#38231 = CARTESIAN_POINT ( 'NONE',  ( 2.648799415243696664, 26.90653288552037736, 40.99458441513962725 ) ) ;
#38232 = EDGE_CURVE ( 'NONE', #41264, #26843, #10108, .T. ) ;
#38233 = CARTESIAN_POINT ( 'NONE',  ( 0.6039202388192953519, -7.665580222077140071, 48.50569649750317325 ) ) ;
#38234 = CARTESIAN_POINT ( 'NONE',  ( 4.694002226626921015, -4.720386398734341959, 45.34316622924319518 ) ) ;
#38235 = CARTESIAN_POINT ( 'NONE',  ( 5.981074661064941900, -7.846517100474690309, -18.96560215432014118 ) ) ;
#38236 = DIRECTION ( 'NONE',  ( 0.09835009131224567436, -0.007732607185437541039, 0.9951218349151970122 ) ) ;
#38237 = CARTESIAN_POINT ( 'NONE',  ( -2.708315649062910779, -8.698422600177046604, -11.76894112707809015 ) ) ;
#38238 = B_SPLINE_CURVE_WITH_KNOTS ( 'NONE', 3,
 ( #50153, #28113, #17568, #51916, #31661, #7518 ),
 .UNSPECIFIED., .F., .F.,
 ( 4, 2, 4 ),
 ( 7.589415207398531038E-19, 0.0002448709889506578614, 0.0004897419779013149638 ),
 .UNSPECIFIED. ) ;
#38239 = EDGE_LOOP ( 'NONE', ( #55341, #20255, #35021, #32080 ) ) ;
#38240 = CARTESIAN_POINT ( 'NONE',  ( 2.526464513654344657, -31.23609615087156754, -29.52129845577965028 ) ) ;
#38241 = CARTESIAN_POINT ( 'NONE',  ( 0.5839880159502340851, 18.37091806000297112, -44.23273844814446676 ) ) ;
#38242 = CARTESIAN_POINT ( 'NONE',  ( 0.8751705887134553219, 38.69254731947794568, 28.56654290188667034 ) ) ;
#38243 = CARTESIAN_POINT ( 'NONE',  ( 0.8744876279028263033, -8.712669995482247742, 48.31603700562906312 ) ) ;
#38244 = EDGE_LOOP ( 'NONE', ( #9167, #58264, #49323, #57994 ) ) ;
#38245 = CARTESIAN_POINT ( 'NONE',  ( 4.963659409799330291, -2.450325214228700865, 44.68724496494572662 ) ) ;
#38246 = CARTESIAN_POINT ( 'NONE',  ( 5.894904586330512508, -4.661384928608805822, -19.56529842882498471 ) ) ;
#38247 = EDGE_CURVE ( 'NONE', #17579, #42439, #39227, .T. ) ;
#38248 = VECTOR ( 'NONE', #53217, 1000.000000000000114 ) ;
#38249 = CARTESIAN_POINT ( 'NONE',  ( 0.8557997880470599172, -7.156447707086029730, 47.37054680076704472 ) ) ;
#38250 = AXIS2_PLACEMENT_3D ( 'NONE', #40234, #17024, #6960 ) ;
#38251 = ORIENTED_EDGE ( 'NONE', *, *, #35314, .F. ) ;
#38252 = CARTESIAN_POINT ( 'NONE',  ( 5.896782393890504181, 12.99025607003297722, 15.35510775321956345 ) ) ;
#38253 = ADVANCED_FACE ( 'NONE', ( #53309 ), #48390, .F. ) ;
#38254 = CARTESIAN_POINT ( 'NONE',  ( 0.000000000000000000, 0.000000000000000000, -1.199999999999999956 ) ) ;
#38255 = ORIENTED_EDGE ( 'NONE', *, *, #53516, .F. ) ;
#38256 = CARTESIAN_POINT ( 'NONE',  ( 0.6000166863083090663, 16.46965316277509217, -46.26633772416342083 ) ) ;
#38257 = B_SPLINE_CURVE_WITH_KNOTS ( 'NONE', 3,
 ( #18003, #27077, #56189, #8896 ),
 .UNSPECIFIED., .F., .F.,
 ( 4, 4 ),
 ( 0.000000000000000000, 0.005014147105413710795 ),
 .UNSPECIFIED. ) ;
#38258 = EDGE_LOOP ( 'NONE', ( #54713, #23652, #17584, #9671 ) ) ;
#38259 = FACE_BOUND ( 'NONE', #9621, .T. ) ;
#38260 = ORIENTED_EDGE ( 'NONE', *, *, #12603, .F. ) ;
#38261 = CARTESIAN_POINT ( 'NONE',  ( 4.834790513006555379, -10.96306168285373595, -45.96085964668552037 ) ) ;
#38262 = CARTESIAN_POINT ( 'NONE',  ( 0.5980271706414711508, -14.64360625457728204, 46.87871626551400794 ) ) ;
#38263 = ORIENTED_EDGE ( 'NONE', *, *, #37430, .T. ) ;
#38264 = CARTESIAN_POINT ( 'NONE',  ( 2.528100132419513812, 39.10451633858129128, 15.26730429898167607 ) ) ;
#38265 = ORIENTED_EDGE ( 'NONE', *, *, #50720, .T. ) ;
#38266 = CARTESIAN_POINT ( 'NONE',  ( 0.5804410086790514622, 45.37396088368707581, 11.86269470150154071 ) ) ;
#38267 = CARTESIAN_POINT ( 'NONE',  ( 0.5835871038041861025, 40.27961859024754432, 24.01638563826134387 ) ) ;
#38268 = ORIENTED_EDGE ( 'NONE', *, *, #38630, .F. ) ;
#38269 = CARTESIAN_POINT ( 'NONE',  ( 0.9756950546413934999, -16.50968749804410862, -39.60512406639365679 ) ) ;
#38270 = CARTESIAN_POINT ( 'NONE',  ( 3.783198216974386963, -42.86118135813610763, 3.901161703631905731 ) ) ;
#38271 = CARTESIAN_POINT ( 'NONE',  ( 0.5837800304671200147, 16.81232615035175115, 43.77879648407090230 ) ) ;
#38272 = ORIENTED_EDGE ( 'NONE', *, *, #43119, .F. ) ;
#38273 = ADVANCED_FACE ( 'NONE', ( #57688 ), #37616, .F. ) ;
#38274 = LINE ( 'NONE', #52641, #20790 ) ;
#38275 = CARTESIAN_POINT ( 'NONE',  ( -6.001507490154110336, 16.31148204059960705, -9.435425682280646598 ) ) ;
#38276 = ORIENTED_EDGE ( 'NONE', *, *, #45093, .T. ) ;
#38277 = CARTESIAN_POINT ( 'NONE',  ( 0.5837800005270550319, 43.17478902026662979, -18.30772655731048459 ) ) ;
#38278 = B_SPLINE_CURVE_WITH_KNOTS ( 'NONE', 3,
 ( #14592, #24279, #13984, #8948 ),
 .UNSPECIFIED., .F., .F.,
 ( 4, 4 ),
 ( 0.000000000000000000, 0.004444103432399267896 ),
 .UNSPECIFIED. ) ;
#38279 = EDGE_CURVE ( 'NONE', #789, #29761, #37801, .T. ) ;
#38280 = ORIENTED_EDGE ( 'NONE', *, *, #3895, .T. ) ;
#38281 = CARTESIAN_POINT ( 'NONE',  ( -6.016489644550736315, 18.20227673842143901, 4.872725758886254255 ) ) ;
#38282 = CARTESIAN_POINT ( 'NONE',  ( 0.5834584762367753807, 11.04850436512404421, -45.57594256081847561 ) ) ;
#38283 = ORIENTED_EDGE ( 'NONE', *, *, #43272, .F. ) ;
#38284 = CARTESIAN_POINT ( 'NONE',  ( 0.9762797500689124330, -34.26226594605912368, -24.13341909939868657 ) ) ;
#38285 = CARTESIAN_POINT ( 'NONE',  ( 4.999999999999983125, 80.00000000000001421, 2.649999999999992806 ) ) ;
#38286 = CARTESIAN_POINT ( 'NONE',  ( 0.3676999524040366896, 34.11874447324979087, 27.96179284115963171 ) ) ;
#38287 = CARTESIAN_POINT ( 'NONE',  ( 0.9784957157296355623, -22.74614816786835902, -35.19866191373972697 ) ) ;
#38288 = EDGE_CURVE ( 'NONE', #4442, #50113, #42230, .T. ) ;
#38289 = ADVANCED_FACE ( 'NONE', ( #43966 ), #38108, .F. ) ;
#38290 = VERTEX_POINT ( 'NONE', #21363 ) ;
#38291 = CARTESIAN_POINT ( 'NONE',  ( 0.8554163680231738898, -0.6539261334249050206, -46.91244881397520317 ) ) ;
#38292 = EDGE_CURVE ( 'NONE', #43179, #4300, #12370, .T. ) ;
#38293 = CARTESIAN_POINT ( 'NONE',  ( -6.010958268070873523, -17.41463273278783319, 7.197664668556383205 ) ) ;
#38294 = CARTESIAN_POINT ( 'NONE',  ( 0.5786265663353153954, 24.57327059187398177, 41.11783955080247921 ) ) ;
#38295 = CONICAL_SURFACE ( 'NONE', #31293, 41.88877248453276536, 0.04450589592585735277 ) ;
#38296 = FACE_OUTER_BOUND ( 'NONE', #13898, .T. ) ;
#38297 = CARTESIAN_POINT ( 'NONE',  ( 0.6039202388192953519, -39.45949250020231602, -29.23204003273579588 ) ) ;
#38298 = VECTOR ( 'NONE', #51028, 1000.000000000000114 ) ;
#38299 = EDGE_CURVE ( 'NONE', #35006, #54810, #34012, .T. ) ;
#38300 = DIRECTION ( 'NONE',  ( 0.000000000000000000, 0.000000000000000000, 1.000000000000000000 ) ) ;
#38301 = CARTESIAN_POINT ( 'NONE',  ( 0.7948878604505665857, 46.86364170957251929, 14.64574112208839551 ) ) ;
#38302 = CARTESIAN_POINT ( 'NONE',  ( 0.8551540677456739292, -0.9122407826479072002, 47.90804413217340851 ) ) ;
#38303 = CARTESIAN_POINT ( 'NONE',  ( 0.9730545539215883499, 33.73144377768594637, -26.52009130076736554 ) ) ;
#38304 = CARTESIAN_POINT ( 'NONE',  ( 0.6029303876144825880, 48.10727438003475953, 0.1308990448397389650 ) ) ;
#38305 = DIRECTION ( 'NONE',  ( -1.000000000000000000, -0.000000000000000000, -0.000000000000000000 ) ) ;
#38306 = CARTESIAN_POINT ( 'NONE',  ( 5.917102823773431552, -13.97547681749021464, 14.46291000371417468 ) ) ;
#38307 = CARTESIAN_POINT ( 'NONE',  ( -6.016489644550737204, 14.94663725562916134, 11.47450955518493032 ) ) ;
#38308 = LINE ( 'NONE', #11890, #1740 ) ;
#38309 = B_SPLINE_CURVE_WITH_KNOTS ( 'NONE', 3,
 ( #42972, #312, #9736, #56412, #47963, #4387, #9422, #5015, #38271, #23523, #61716, #19458, #38577, #33876, #13528, #32633 ),
 .UNSPECIFIED., .F., .F.,
 ( 4, 3, 3, 3, 3, 4 ),
 ( 6.939740885162003740E-18, 0.0002732102107932011126, 0.0004098135523333842987, 0.0005464168938824958896, 0.0008195847345945464794, 0.001092771384553105915 ),
 .UNSPECIFIED. ) ;
#38310 = CARTESIAN_POINT ( 'NONE',  ( 3.407937589446178528, -12.82481284928200260, -4.815089211105192391 ) ) ;
#38311 = CARTESIAN_POINT ( 'NONE',  ( -5.995132425357893702, -18.68182899165013211, 2.468096378288054726 ) ) ;
#38312 = ORIENTED_EDGE ( 'NONE', *, *, #59594, .F. ) ;
#38313 = LINE ( 'NONE', #1285, #37939 ) ;
#38314 = CARTESIAN_POINT ( 'NONE',  ( 1.600000000000000089, -11.64055411052240352, 0.000000000000000000 ) ) ;
#38315 = DIRECTION ( 'NONE',  ( -0.07836865515943411409, -0.2503967164834531856, 0.9649662368512210708 ) ) ;
#38316 = ORIENTED_EDGE ( 'NONE', *, *, #969, .T. ) ;
#38317 = CARTESIAN_POINT ( 'NONE',  ( 3.783198216974391404, 9.462293521184873768, 41.98529422752520901 ) ) ;
#38318 = CARTESIAN_POINT ( 'NONE',  ( 4.975610109902397937, -11.44439439467527642, -47.55497076097196185 ) ) ;
#38319 = VERTEX_POINT ( 'NONE', #16667 ) ;
#38320 = ORIENTED_EDGE ( 'NONE', *, *, #32356, .T. ) ;
#38321 = EDGE_CURVE ( 'NONE', #45266, #28142, #48968, .T. ) ;
#38322 = CARTESIAN_POINT ( 'NONE',  ( 0.5998501479064708430, -37.84527566984837677, -29.69975237324600315 ) ) ;
#38323 = EDGE_LOOP ( 'NONE', ( #25064, #50467, #15801, #47465 ) ) ;
#38324 = LINE ( 'NONE', #38631, #36996 ) ;
#38325 = B_SPLINE_CURVE_WITH_KNOTS ( 'NONE', 3,
 ( #11707, #29557, #5721, #40849, #46155, #22952 ),
 .UNSPECIFIED., .F., .F.,
 ( 4, 2, 4 ),
 ( 1.259499515835350888E-16, 0.0002450741128632365705, 0.0004901482257263472652 ),
 .UNSPECIFIED. ) ;
#38326 = VERTEX_POINT ( 'NONE', #50475 ) ;
#38327 = EDGE_LOOP ( 'NONE', ( #30684, #26, #54858, #21927 ) ) ;
#38328 = CYLINDRICAL_SURFACE ( 'NONE', #2659, 72.00000000000002842 ) ;
#38329 = ORIENTED_EDGE ( 'NONE', *, *, #28293, .T. ) ;
#38330 = CARTESIAN_POINT ( 'NONE',  ( 0.1073791018717483448, 16.05399293000815675, -40.02496097243042072 ) ) ;
#38331 = DIRECTION ( 'NONE',  ( -0.000000000000000000, 0.000000000000000000, 1.000000000000000000 ) ) ;
#38332 = B_SPLINE_CURVE_WITH_KNOTS ( 'NONE', 3,
 ( #36229, #55294, #12417, #31507 ),
 .UNSPECIFIED., .F., .F.,
 ( 4, 4 ),
 ( 0.000000000000000000, 0.004444103432399266161 ),
 .UNSPECIFIED. ) ;
#38333 = AXIS2_PLACEMENT_3D ( 'NONE', #3605, #55613, #13353 ) ;
#38334 = CARTESIAN_POINT ( 'NONE',  ( -6.078726893082806448, 17.84743921491351415, 7.229312189875837014 ) ) ;
#38335 = ORIENTED_EDGE ( 'NONE', *, *, #17889, .F. ) ;
#38336 = CARTESIAN_POINT ( 'NONE',  ( 5.974727161628369032, -10.24903993264996949, -17.78288073588499074 ) ) ;
#38337 = CARTESIAN_POINT ( 'NONE',  ( 0.9787464366903567692, -39.64751462911939228, 13.57971194923611868 ) ) ;
#38338 = ORIENTED_EDGE ( 'NONE', *, *, #54861, .F. ) ;
#38339 = ORIENTED_EDGE ( 'NONE', *, *, #46152, .F. ) ;
#38340 = CARTESIAN_POINT ( 'NONE',  ( 0.6001305935487315502, -29.70149728382465426, 37.84751346122803994 ) ) ;
#38341 = ORIENTED_EDGE ( 'NONE', *, *, #44605, .T. ) ;
#38342 = CARTESIAN_POINT ( 'NONE',  ( 4.553261556744875094, 35.06776520399859010, 26.45357082552112260 ) ) ;
#38343 = CARTESIAN_POINT ( 'NONE',  ( 1.154321485836934169, -41.23280395520815489, 11.90271791109298505 ) ) ;
#38344 = DIRECTION ( 'NONE',  ( 0.09835009131224552170, -0.2500873580884774849, 0.9632152266566380572 ) ) ;
#38345 = DIRECTION ( 'NONE',  ( -1.000000000000000000, -3.135800716341489291E-16, 1.298891185607901956E-16 ) ) ;
#38346 = VECTOR ( 'NONE', #29342, 1000.000000000000000 ) ;
#38347 = ORIENTED_EDGE ( 'NONE', *, *, #44718, .T. ) ;
#38348 = CARTESIAN_POINT ( 'NONE',  ( 0.6023142530420679819, -12.19802990522833319, 46.53533807097409891 ) ) ;
#38349 = CARTESIAN_POINT ( 'NONE',  ( 5.880360259849739535, 3.090325311464862779, -47.87242051977162305 ) ) ;
#38350 = EDGE_CURVE ( 'NONE', #44883, #30283, #26673, .T. ) ;
#38351 =( BOUNDED_SURFACE ( )  B_SPLINE_SURFACE ( 3, 1, ( 
 ( #28227, #47343 ),
 ( #27929, #32635 ),
 ( #23525, #18855 ),
 ( #9424, #35420 ) ),
 .UNSPECIFIED., .F., .F., .F. ) 
 B_SPLINE_SURFACE_WITH_KNOTS ( ( 4, 4 ),
 ( 2, 2 ),
 ( 0.000000000000000000, 1.000000000000000000 ),
 ( 0.000000000000000000, 1.000000000000000000 ),
 .UNSPECIFIED. ) 
 GEOMETRIC_REPRESENTATION_ITEM ( )  RATIONAL_B_SPLINE_SURFACE ( (
 ( 1.000000000000000000, 1.000000000000000000),
 ( 0.9953390228620291325, 0.8624445117760984880),
 ( 0.9953390228620291325, 0.8624445117760984880),
 ( 1.000000000000000000, 1.000000000000000000) ) ) 
 REPRESENTATION_ITEM ( '' )  SURFACE ( )  );
#38352 = CARTESIAN_POINT ( 'NONE',  ( 0.5817217712918332229, 37.08439386095844981, -28.70509860588673590 ) ) ;
#38353 = B_SPLINE_CURVE_WITH_KNOTS ( 'NONE', 3,
 ( #47449, #52434, #9527, #28637, #4809, #112, #19262, #14565, #33665, #49909, #21094, #48671, #40238, #34280, #44614, #44929 ),
 .UNSPECIFIED., .F., .F.,
 ( 4, 3, 3, 3, 3, 4 ),
 ( 2.221635811791082109E-17, 0.0002612764279487776080, 0.0003919131003184762635, 0.0005225497727000636295, 0.0007837925190632439448, 0.001045051706266717385 ),
 .UNSPECIFIED. ) ;
#38354 = ORIENTED_EDGE ( 'NONE', *, *, #34964, .T. ) ;
#38355 = CARTESIAN_POINT ( 'NONE',  ( 2.618530812446111078, 46.37964111407201528, 7.658699584660552340 ) ) ;
#38356 = EDGE_CURVE ( 'NONE', #1298, #12205, #54694, .T. ) ;
#38357 = CARTESIAN_POINT ( 'NONE',  ( -6.077587904424778920, 12.00112336472165353, 15.05885318935882644 ) ) ;
#38358 = CARTESIAN_POINT ( 'NONE',  ( 4.975801465491694664, 45.55012473237754023, -14.85979367497125381 ) ) ;
#38359 = EDGE_CURVE ( 'NONE', #35182, #5228, #37015, .T. ) ;
#38360 = VERTEX_POINT ( 'NONE', #28211 ) ;
#38361 = VERTEX_POINT ( 'NONE', #4373 ) ;
#38362 = CARTESIAN_POINT ( 'NONE',  ( -4.000000000000000000, -2.309401076758525573, -5.599999999999999645 ) ) ;
#38363 = EDGE_CURVE ( 'NONE', #21245, #8175, #23737, .T. ) ;
#38364 = FACE_OUTER_BOUND ( 'NONE', #15112, .T. ) ;
#38365 = CARTESIAN_POINT ( 'NONE',  ( 4.834790513006553603, 37.58952546674443340, 28.62895241026735604 ) ) ;
#38366 = CARTESIAN_POINT ( 'NONE',  ( 0.7764146366350233031, -41.45356081493326883, 21.94636118885760823 ) ) ;
#38367 = CARTESIAN_POINT ( 'NONE',  ( 4.834790513006553603, -42.76900418948107330, 20.08486050647432108 ) ) ;
#38368 = DIRECTION ( 'NONE',  ( 0.000000000000000000, -0.4999999999999993339, 0.8660254037844390407 ) ) ;
#38369 =( BOUNDED_SURFACE ( )  B_SPLINE_SURFACE ( 3, 1, ( 
 ( #10710, #34213 ),
 ( #1585, #20721 ),
 ( #5963, #43315 ),
 ( #29491, #25105 ) ),
 .UNSPECIFIED., .F., .F., .F. ) 
 B_SPLINE_SURFACE_WITH_KNOTS ( ( 4, 4 ),
 ( 2, 2 ),
 ( 0.000000000000000000, 1.000000000000000000 ),
 ( 0.000000000000000000, 1.000000000000000000 ),
 .UNSPECIFIED. ) 
 GEOMETRIC_REPRESENTATION_ITEM ( )  RATIONAL_B_SPLINE_SURFACE ( (
 ( 1.000000000000000000, 1.000000000000000000),
 ( 0.9953390228620291325, 0.8624445117761032620),
 ( 0.9953390228620291325, 0.8624445117761032620),
 ( 1.000000000000000000, 1.000000000000000000) ) ) 
 REPRESENTATION_ITEM ( '' )  SURFACE ( )  );
#38370 = DIRECTION ( 'NONE',  ( -0.07906939808003035641, 0.9968364091521051407, -0.008074879317899831543 ) ) ;
#38371 = CARTESIAN_POINT ( 'NONE',  ( 0.9968887458511649369, 20.88287852258444843, 37.48500720268736330 ) ) ;
#38372 = DIRECTION ( 'NONE',  ( 1.000000000000000000, 0.000000000000000000, 0.000000000000000000 ) ) ;
#38373 = CARTESIAN_POINT ( 'NONE',  ( 0.9772918015221172539, -1.814983444719383776, -41.86935264422026393 ) ) ;
#38374 = CARTESIAN_POINT ( 'NONE',  ( 10.00000000000000533, -2.650000000000270362, 80.00000000000000000 ) ) ;
#38376 = ORIENTED_EDGE ( 'NONE', *, *, #11767, .T. ) ;
#38375 = EDGE_CURVE ( 'NONE', #31128, #14818, #34779, .T. ) ;
#38377 = DIRECTION ( 'NONE',  ( -0.000000000000000000, -0.000000000000000000, -1.000000000000000000 ) ) ;
#38378 = CARTESIAN_POINT ( 'NONE',  ( 0.1098349054025746091, -34.08267426123942556, -26.42143025179976945 ) ) ;
#38380 = EDGE_CURVE ( 'NONE', #26359, #4753, #16808, .T. ) ;
#38379 = CARTESIAN_POINT ( 'NONE',  ( 4.833616638992205949, -41.27831852777627120, -20.86133030530276500 ) ) ;
#38381 = CARTESIAN_POINT ( 'NONE',  ( 0.2279481005628803680, -26.91014123888646736, -34.96209069229257693 ) ) ;
#38382 = CARTESIAN_POINT ( 'NONE',  ( 4.975801465491694664, -46.87746200127448049, -9.906103548668065528 ) ) ;
#38383 = CARTESIAN_POINT ( 'NONE',  ( 0.8760168074886965917, 44.09317760313724932, 19.22870327415319736 ) ) ;
#38384 = CARTESIAN_POINT ( 'NONE',  ( 2.301430502907644282, -22.89309745268860752, -42.22699195640099390 ) ) ;
#38385 = LINE ( 'NONE', #57433, #54852 ) ;
#38386 = APPLICATION_CONTEXT ( 'automotive_design' ) ;
#38387 = CARTESIAN_POINT ( 'NONE',  ( 0.9757787079277466802, -11.14366644276439544, 41.43615150473007702 ) ) ;
#38388 = CARTESIAN_POINT ( 'NONE',  ( 1.827326673878744145, 27.17438009792331854, -33.38933471001448083 ) ) ;
#38390 = ORIENTED_EDGE ( 'NONE', *, *, #27087, .F. ) ;
#38389 = CARTESIAN_POINT ( 'NONE',  ( 0.9722240750034577550, -36.86535092060692875, 21.95618656573991245 ) ) ;
#38391 = ORIENTED_EDGE ( 'NONE', *, *, #33199, .T. ) ;
#38392 = B_SPLINE_CURVE_WITH_KNOTS ( 'NONE', 3,
 ( #8370, #9614, #18104, #14340 ),
 .UNSPECIFIED., .F., .F.,
 ( 4, 4 ),
 ( 1.998817200139820460E-17, 0.004444306975806115029 ),
 .UNSPECIFIED. ) ;
#38393 = CARTESIAN_POINT ( 'NONE',  ( 0.5809828226811553087, -37.66417181417572380, 29.58751527316164953 ) ) ;
#38394 = CARTESIAN_POINT ( 'NONE',  ( 0.1119898979215352142, 14.71105701693103107, -41.59983304890096889 ) ) ;
#38395 = ORIENTED_EDGE ( 'NONE', *, *, #23735, .T. ) ;
#38396 = CARTESIAN_POINT ( 'NONE',  ( -6.063463321072276813, -18.89860197674391529, 3.696389563355157559 ) ) ;
#38398 = CARTESIAN_POINT ( 'NONE',  ( 4.294020221588231045, 0.6022396715791498156, 42.05358393252018345 ) ) ;
#38397 = AXIS2_PLACEMENT_3D ( 'NONE', #470, #20527, #23989 ) ;
#38399 = CARTESIAN_POINT ( 'NONE',  ( 0.5819845079324659221, -41.70428776698881279, -23.55367910461039926 ) ) ;
#38400 = ORIENTED_EDGE ( 'NONE', *, *, #9253, .T. ) ;
#38401 = VERTEX_POINT ( 'NONE', #42341 ) ;
#38402 = ADVANCED_FACE ( 'NONE', ( #14141 ), #20882, .F. ) ;
#38403 = CARTESIAN_POINT ( 'NONE',  ( 0.3622758884714600280, 36.91764744403290166, 22.26738722580180507 ) ) ;
#38404 = CARTESIAN_POINT ( 'NONE',  ( -4.473699999999997345, 0.000000000000000000, 0.000000000000000000 ) ) ;
#38405 = CARTESIAN_POINT ( 'NONE',  ( 0.5835871038041883230, 46.89579726320849318, 0.1365721404356005364 ) ) ;
#38406 = CARTESIAN_POINT ( 'NONE',  ( 4.960386119450151732, 23.14534831554928118, 37.13124447179546195 ) ) ;
#38407 = DIRECTION ( 'NONE',  ( 0.000000000000000000, 0.000000000000000000, 1.000000000000000000 ) ) ;
#38408 = CARTESIAN_POINT ( 'NONE',  ( 0.5809828226811553087, 0.5448590168532381206, 47.89273459658653564 ) ) ;
#38409 = ORIENTED_EDGE ( 'NONE', *, *, #6764, .T. ) ;
#38410 = ORIENTED_EDGE ( 'NONE', *, *, #8630, .T. ) ;
#38411 = CARTESIAN_POINT ( 'NONE',  ( 0.09136607875274982415, 12.80000000000000071, 3.000000000000000000 ) ) ;
#38412 = VERTEX_POINT ( 'NONE', #14442 ) ;
#38413 = CARTESIAN_POINT ( 'NONE',  ( 0.3622758884714730732, -41.42293301073634382, 11.95365414648425428 ) ) ;
#38414 = CARTESIAN_POINT ( 'NONE',  ( 5.895881250540457863, 0.6675221664546298062, 20.10179334700246656 ) ) ;
#38415 = CARTESIAN_POINT ( 'NONE',  ( 2.299746137290198611, -40.05309593391260847, -28.28481648862038966 ) ) ;
#38416 = CARTESIAN_POINT ( 'NONE',  ( 1.231276596079887931, -7.805643096901414779, -41.18675402191659174 ) ) ;
#38417 = VECTOR ( 'NONE', #3893, 1000.000000000000000 ) ;
#38418 = ORIENTED_EDGE ( 'NONE', *, *, #61226, .F. ) ;
#38419 = VERTEX_POINT ( 'NONE', #33243 ) ;
#38420 = CARTESIAN_POINT ( 'NONE',  ( 3.238741278300274029, 35.19027457370178524, -24.69738534405274066 ) ) ;
#38421 = CARTESIAN_POINT ( 'NONE',  ( 0.9749527285493311268, -42.50314808877157446, -5.883724875809550170 ) ) ;
#38422 = CARTESIAN_POINT ( 'NONE',  ( 0.1097557419366048670, -37.45792859959212251, -21.36873056345880784 ) ) ;
#38423 = B_SPLINE_CURVE_WITH_KNOTS ( 'NONE', 3,
 ( #44272, #34546, #30750, #20752, #11051, #53611 ),
 .UNSPECIFIED., .F., .F.,
 ( 4, 2, 4 ),
 ( 3.144186300207962859E-18, 0.0002447193893791683528, 0.0004894387787583335614 ),
 .UNSPECIFIED. ) ;
#38424 = DIRECTION ( 'NONE',  ( 0.000000000000000000, 1.000000000000000000, 0.000000000000000000 ) ) ;
#38425 = ORIENTED_EDGE ( 'NONE', *, *, #3941, .T. ) ;
#38426 = CARTESIAN_POINT ( 'NONE',  ( 4.975801465491694664, 31.15993731089074359, 36.39623109580477234 ) ) ;
#38427 = EDGE_CURVE ( 'NONE', #38229, #11266, #48199, .T. ) ;
#38428 = ORIENTED_EDGE ( 'NONE', *, *, #37934, .T. ) ;
#38429 = CARTESIAN_POINT ( 'NONE',  ( 0.2885700199627505014, -26.88157179738480096, -33.71073713194511612 ) ) ;
#38430 = CARTESIAN_POINT ( 'NONE',  ( 4.963659409799330291, 36.94443854030254215, -25.25989740981460230 ) ) ;
#38431 = VERTEX_POINT ( 'NONE', #61095 ) ;
#38432 = CARTESIAN_POINT ( 'NONE',  ( 2.282816707992306959, 37.66448606630884655, 28.06926176030984621 ) ) ;
#38433 = ADVANCED_FACE ( 'NONE', ( #37031 ), #18034, .F. ) ;
#38434 = CARTESIAN_POINT ( 'NONE',  ( 4.322998006666165516, -40.45864630878501345, -25.80712523194260655 ) ) ;
#38435 = CARTESIAN_POINT ( 'NONE',  ( 2.500000000000000000, 2.357898499370431722, -2.818925648462311528E-15 ) ) ;
#38436 = B_SPLINE_CURVE_WITH_KNOTS ( 'NONE', 3,
 ( #31806, #50892, #13021, #51195, #8277, #27398 ),
 .UNSPECIFIED., .F., .F.,
 ( 4, 2, 4 ),
 ( 6.149443329761889321E-18, 0.0002445244328975373482, 0.0004890488657950686248 ),
 .UNSPECIFIED. ) ;
#38437 = CONICAL_SURFACE ( 'NONE', #41480, 2.055000000000000160, 0.7853981633974639331 ) ;
#38438 = EDGE_LOOP ( 'NONE', ( #57541, #49811, #52070, #35790 ) ) ;
#38439 = CARTESIAN_POINT ( 'NONE',  ( 0.5809828226811553087, -18.83114015454665946, -44.03860873105715967 ) ) ;
#38440 = CARTESIAN_POINT ( 'NONE',  ( 0.2940135542859018680, -43.64383946108019785, 6.438619866623495724 ) ) ;
#38441 = CARTESIAN_POINT ( 'NONE',  ( 5.838029081930957709, 44.62720369181010227, 15.47506862028764907 ) ) ;
#38442 = LINE ( 'NONE', #43771, #934 ) ;
#38443 = B_SPLINE_CURVE_WITH_KNOTS ( 'NONE', 3,
 ( #3334, #27467, #46595, #22465, #41590, #32180 ),
 .UNSPECIFIED., .F., .F.,
 ( 4, 2, 4 ),
 ( 1.084202172485504434E-19, 0.0002291459268755673075, 0.0004582918537511345065 ),
 .UNSPECIFIED. ) ;
#38444 = FACE_OUTER_BOUND ( 'NONE', #52331, .T. ) ;
#38445 = EDGE_LOOP ( 'NONE', ( #59069, #53226, #33363, #9375 ) ) ;
#38446 = CARTESIAN_POINT ( 'NONE',  ( 1.296416391601052265, -16.81764146547304151, 40.73664578257469771 ) ) ;
#38447 = ORIENTED_EDGE ( 'NONE', *, *, #3941, .F. ) ;
#38448 = B_SPLINE_CURVE_WITH_KNOTS ( 'NONE', 3,
 ( #7158, #17215, #31303, #44817 ),
 .UNSPECIFIED., .F., .F.,
 ( 4, 4 ),
 ( 0.002405070305343063371, 0.004447772540402989729 ),
 .UNSPECIFIED. ) ;
#38449 = CARTESIAN_POINT ( 'NONE',  ( 0.7762783648524370639, 38.54028518467420383, 28.45155609988340828 ) ) ;
#38450 = CARTESIAN_POINT ( 'NONE',  ( 0.09136607875274982415, 5.281323502666703820E-15, -43.12527911185304674 ) ) ;
#38452 = EDGE_CURVE ( 'NONE', #15681, #13767, #19801, .T. ) ;
#38451 = CARTESIAN_POINT ( 'NONE',  ( 0.6016118706126977189, 22.40471323146671168, 43.69874002531047097 ) ) ;
#38453 = CARTESIAN_POINT ( 'NONE',  ( -6.001507490154111224, 9.408444979392321272, 16.32705935667510744 ) ) ;
#38454 = B_SPLINE_CURVE_WITH_KNOTS ( 'NONE', 3,
 ( #26179, #17105, #26799, #45317, #51208, #45937 ),
 .UNSPECIFIED., .F., .F.,
 ( 4, 2, 4 ),
 ( 1.554159946372743606E-17, 0.0002293319059085091138, 0.0004586638118170027235 ),
 .UNSPECIFIED. ) ;
#38455 = CARTESIAN_POINT ( 'NONE',  ( 0.7048096507298635682, 44.76417498422291175, 17.62869676200424962 ) ) ;
#38456 = CARTESIAN_POINT ( 'NONE',  ( 53.14999999999999858, 15.50000000000000711, 1.598617295522242905E-15 ) ) ;
#38457 = CARTESIAN_POINT ( 'NONE',  ( 0.2940135542859017570, 39.39157462944580601, -19.86314166752638499 ) ) ;
#38458 = CARTESIAN_POINT ( 'NONE',  ( 4.834790513006553603, 41.39428925248056146, -22.78381351324563298 ) ) ;
#38459 = CARTESIAN_POINT ( 'NONE',  ( 5.959547316686252039, 19.82530672674362293, -5.315863417546125014 ) ) ;
#38461 = VERTEX_POINT ( 'NONE', #29141 ) ;
#38460 = LINE ( 'NONE', #52842, #52845 ) ;
#38462 = ORIENTED_EDGE ( 'NONE', *, *, #21824, .T. ) ;
#38463 = CARTESIAN_POINT ( 'NONE',  ( -2.601141883200662974, -5.629531953699331126, 13.82402971103819667 ) ) ;
#38464 = FACE_OUTER_BOUND ( 'NONE', #15422, .T. ) ;
#38465 = CIRCLE ( 'NONE', #19447, 47.91270532121795611 ) ;
#38466 = CARTESIAN_POINT ( 'NONE',  ( 1.088908134280556661, 30.89124834763388350, 29.78762923589977873 ) ) ;
#38467 = CARTESIAN_POINT ( 'NONE',  ( 5.958863334805807099, -20.34989385289155450, -2.680345151634541789 ) ) ;
#38468 = CARTESIAN_POINT ( 'NONE',  ( 0.1156495703730067298, 9.685606167693753932, -43.04801954091968241 ) ) ;
#38469 =( BOUNDED_SURFACE ( )  B_SPLINE_SURFACE ( 3, 1, ( 
 ( #60414, #55720 ),
 ( #17847, #7173 ),
 ( #12853, #26306 ),
 ( #56035, #3403 ) ),
 .UNSPECIFIED., .F., .F., .F. ) 
 B_SPLINE_SURFACE_WITH_KNOTS ( ( 4, 4 ),
 ( 2, 2 ),
 ( 0.000000000000000000, 1.000000000000000000 ),
 ( 0.000000000000000000, 1.000000000000000000 ),
 .UNSPECIFIED. ) 
 GEOMETRIC_REPRESENTATION_ITEM ( )  RATIONAL_B_SPLINE_SURFACE ( (
 ( 1.000000000000000000, 1.000000000000000000),
 ( 0.9953040768229013402, 0.8617119497784988535),
 ( 0.9953040768229013402, 0.8617119497784988535),
 ( 1.000000000000000000, 1.000000000000000000) ) ) 
 REPRESENTATION_ITEM ( '' )  SURFACE ( )  );
#38470 = VERTEX_POINT ( 'NONE', #15984 ) ;
#38471 = EDGE_CURVE ( 'NONE', #35962, #36314, #57929, .T. ) ;
#38472 = VECTOR ( 'NONE', #34335, 1000.000000000000114 ) ;
#38473 = DIRECTION ( 'NONE',  ( -0.07500201931887529039, -0.9374924185315484104, 0.3398274007403745411 ) ) ;
#38474 = CARTESIAN_POINT ( 'NONE',  ( 0.8753041380234465318, 28.81806460335508646, -39.75748332565621723 ) ) ;
#38475 = CARTESIAN_POINT ( 'NONE',  ( 0.8557997880470606944, -33.22501220301877112, -34.51495345639583689 ) ) ;
#38476 = ORIENTED_EDGE ( 'NONE', *, *, #17762, .F. ) ;
#38477 = AXIS2_PLACEMENT_3D ( 'NONE', #14443, #51705, #24130 ) ;
#38478 = EDGE_CURVE ( 'NONE', #1744, #41667, #38880, .T. ) ;
#38479 = CARTESIAN_POINT ( 'NONE',  ( 0.1129192098497455998, 20.83764143887614040, -38.89401608281131928 ) ) ;
#38480 = CARTESIAN_POINT ( 'NONE',  ( 0.9722240750034588652, -20.94823713380363017, 37.44729079646484848 ) ) ;
#38481 = ORIENTED_EDGE ( 'NONE', *, *, #38786, .T. ) ;
#38482 = EDGE_CURVE ( 'NONE', #15844, #22653, #58550, .T. ) ;
#38483 = CARTESIAN_POINT ( 'NONE',  ( 0.5980271706414734822, 23.33483692714744961, 43.21498152753393640 ) ) ;
#38484 = ORIENTED_EDGE ( 'NONE', *, *, #45361, .T. ) ;
#38485 = CARTESIAN_POINT ( 'NONE',  ( 52.49655874117198096, 15.40126909844818748, -1.751009045720654189 ) ) ;
#38486 = DIRECTION ( 'NONE',  ( 0.000000000000000000, 0.000000000000000000, 1.000000000000000000 ) ) ;
#38487 = VERTEX_POINT ( 'NONE', #301 ) ;
#38488 = FACE_BOUND ( 'NONE', #7362, .T. ) ;
#38489 = CARTESIAN_POINT ( 'NONE',  ( 4.956445790443989807, 44.30493387627029733, 15.95653108789479191 ) ) ;
#38490 = CARTESIAN_POINT ( 'NONE',  ( 0.5987334363312691865, -48.62339724184305112, -6.879545561590992619 ) ) ;
#38491 = DIRECTION ( 'NONE',  ( 0.000000000000000000, 1.000000000000000000, -1.224646799147353207E-16 ) ) ;
#38492 = ORIENTED_EDGE ( 'NONE', *, *, #206, .F. ) ;
#38493 = B_SPLINE_CURVE_WITH_KNOTS ( 'NONE', 3,
 ( #45188, #2538, #12589, #36399, #39873, #55461 ),
 .UNSPECIFIED., .F., .F.,
 ( 4, 2, 4 ),
 ( 7.007167689862070887E-18, 0.0002448709889506578614, 0.0004897419779013087839 ),
 .UNSPECIFIED. ) ;
#38494 = CARTESIAN_POINT ( 'NONE',  ( 0.6029443449137436017, -7.794573848081279621, -48.48488585642065374 ) ) ;
#38495 = VERTEX_POINT ( 'NONE', #19442 ) ;
#38496 = CARTESIAN_POINT ( 'NONE',  ( 3.238931869106853600, -35.19033040238051768, -24.69728751010273982 ) ) ;
#38497 = CIRCLE ( 'NONE', #46492, 0.05882000000000109363 ) ;
#38498 = B_SPLINE_CURVE_WITH_KNOTS ( 'NONE', 3,
 ( #48389, #131, #42785, #5449, #9551, #5141 ),
 .UNSPECIFIED., .F., .F.,
 ( 4, 2, 4 ),
 ( 0.000000000000000000, 0.0002447195606305752340, 0.0004894391212611504680 ),
 .UNSPECIFIED. ) ;
#38499 = ORIENTED_EDGE ( 'NONE', *, *, #51126, .F. ) ;
#38500 = ADVANCED_FACE ( 'NONE', ( #58237 ), #49704, .T. ) ;
#38501 = VERTEX_POINT ( 'NONE', #29749 ) ;
#38502 = CARTESIAN_POINT ( 'NONE',  ( 5.838029081930957709, -22.68231883182896880, 41.43159990350574162 ) ) ;
#38503 = CARTESIAN_POINT ( 'NONE',  ( 0.6031357023905875581, -34.04794059289672248, 33.98625823839241633 ) ) ;
#38504 = CARTESIAN_POINT ( 'NONE',  ( 0.5782707292762423457, -24.62356639979799411, 39.91761931105558858 ) ) ;
#38505 = ORIENTED_EDGE ( 'NONE', *, *, #52897, .F. ) ;
#38506 = DIRECTION ( 'NONE',  ( 1.000000000000000000, 0.000000000000000000, 0.000000000000000000 ) ) ;
#38507 = EDGE_CURVE ( 'NONE', #20167, #60001, #47415, .T. ) ;
#38508 = CARTESIAN_POINT ( 'NONE',  ( 5.896782393890504181, 8.460428369634295009, 18.24684188237239724 ) ) ;
#38509 = CARTESIAN_POINT ( 'NONE',  ( -6.057079549204054558, 19.25697688790420159, 0.008499321259854933364 ) ) ;
#38510 = ORIENTED_EDGE ( 'NONE', *, *, #15917, .T. ) ;
#38511 = EDGE_CURVE ( 'NONE', #23911, #25935, #34783, .T. ) ;
#38512 = ORIENTED_EDGE ( 'NONE', *, *, #31213, .T. ) ;
#38513 = CARTESIAN_POINT ( 'NONE',  ( 1.088313998177384834, 17.14007796983287335, -39.34193117255236416 ) ) ;
#38514 = DIRECTION ( 'NONE',  ( 0.1011922191286468153, -0.6101824289146793312, 0.7857719377984951903 ) ) ;
#38515 = FACE_OUTER_BOUND ( 'NONE', #19325, .T. ) ;
#38516 = CARTESIAN_POINT ( 'NONE',  ( -2.739355103387247858, -12.11899594566314242, 8.716507570123328108 ) ) ;
#38518 = CARTESIAN_POINT ( 'NONE',  ( 1.088908134280555107, -26.73890361625891643, -33.56490895818192399 ) ) ;
#38517 = CONICAL_SURFACE ( 'NONE', #18813, 42.08604991992415023, 1.569615340895231137 ) ;
#38519 = ORIENTED_EDGE ( 'NONE', *, *, #36628, .F. ) ;
#38520 = B_SPLINE_CURVE_WITH_KNOTS ( 'NONE', 3,
 ( #2629, #45276, #51470, #12683, #21754, #40893, #8254, #36487, #27068, #46195, #27374, #26139, #2316, #40579, #17368, #55874 ),
 .UNSPECIFIED., .F., .F.,
 ( 4, 3, 3, 3, 3, 4 ),
 ( 2.081781105835003155E-17, 0.0002612764279487750059, 0.0003919131003184785403, 0.0005225497727000651474, 0.0007837925190632448122, 0.001045051706266716084 ),
 .UNSPECIFIED. ) ;
#38521 = VERTEX_POINT ( 'NONE', #29440 ) ;
#38522 = AXIS2_PLACEMENT_3D ( 'NONE', #59617, #17648, #16725 ) ;
#38523 = CARTESIAN_POINT ( 'NONE',  ( 3.240649175237395596, -8.819624127022542837, 43.09848196463181580 ) ) ;
#38525 = EDGE_CURVE ( 'NONE', #61765, #35559, #39186, .T. ) ;
#38524 = CARTESIAN_POINT ( 'NONE',  ( 50.15454924916686252, 15.27473315039759427, 2.633196453571728490 ) ) ;
#38526 = CIRCLE ( 'NONE', #22548, 13.50000000000000178 ) ;
#38527 = CARTESIAN_POINT ( 'NONE',  ( 4.549368137175248350, 0.000000000000000000, 0.000000000000000000 ) ) ;
#38528 = CARTESIAN_POINT ( 'NONE',  ( 4.549368137175248350, 0.000000000000000000, 0.000000000000000000 ) ) ;
#38529 = CARTESIAN_POINT ( 'NONE',  ( -1.200000000000006617, 0.000000000000000000, -5.612499999999999822 ) ) ;
#38530 = CARTESIAN_POINT ( 'NONE',  ( 4.967162193818129623, 32.10009971360071290, 28.74031574030022540 ) ) ;
#38531 = ORIENTED_EDGE ( 'NONE', *, *, #20010, .F. ) ;
#38532 = CARTESIAN_POINT ( 'NONE',  ( 4.335381028904201628, 48.70445384730871297, 5.256712194872322108 ) ) ;
#38533 = FACE_OUTER_BOUND ( 'NONE', #42925, .T. ) ;
#38534 = CARTESIAN_POINT ( 'NONE',  ( 0.8560838555295158248, -8.701885300216421371, 46.09392613244839509 ) ) ;
#38535 = CARTESIAN_POINT ( 'NONE',  ( 5.958863334805807099, 17.77512673691319023, -10.26388325355069142 ) ) ;
#38536 = LINE ( 'NONE', #53519, #31248 ) ;
#38537 = DIRECTION ( 'NONE',  ( -0.07500201931887529039, 0.6834640454944322929, -0.7261209235481894675 ) ) ;
#38538 = CARTESIAN_POINT ( 'NONE',  ( -2.601141883200665639, -0.03040527887379005853, -14.92630238834806811 ) ) ;
#38539 =( BOUNDED_SURFACE ( )  B_SPLINE_SURFACE ( 3, 1, ( 
 ( #36448, #2898 ),
 ( #27643, #26714 ),
 ( #22029, #31420 ),
 ( #50518, #46777 ) ),
 .UNSPECIFIED., .F., .F., .F. ) 
 B_SPLINE_SURFACE_WITH_KNOTS ( ( 4, 4 ),
 ( 2, 2 ),
 ( 0.000000000000000000, 1.000000000000000000 ),
 ( 0.000000000000000000, 1.000000000000000000 ),
 .UNSPECIFIED. ) 
 GEOMETRIC_REPRESENTATION_ITEM ( )  RATIONAL_B_SPLINE_SURFACE ( (
 ( 1.000000000000000000, 1.000000000000000000),
 ( 0.9953485035131437453, 0.8621029689291523912),
 ( 0.9953485035131437453, 0.8621029689291523912),
 ( 1.000000000000000000, 1.000000000000000000) ) ) 
 REPRESENTATION_ITEM ( '' )  SURFACE ( )  );
#38540 = VECTOR ( 'NONE', #7368, 1000.000000000000114 ) ;
#38541 = ORIENTED_EDGE ( 'NONE', *, *, #16602, .T. ) ;
#38542 = FACE_OUTER_BOUND ( 'NONE', #50269, .T. ) ;
#38543 = EDGE_CURVE ( 'NONE', #57626, #7870, #51056, .T. ) ;
#38544 = CARTESIAN_POINT ( 'NONE',  ( 4.967162193818129623, -32.10009971360051395, -28.74031574030045633 ) ) ;
#38545 = CARTESIAN_POINT ( 'NONE',  ( 0.5997462898726536595, -47.36625756029525292, -12.96106765957508244 ) ) ;
#38546 = CARTESIAN_POINT ( 'NONE',  ( -4.000000000000000000, 0.000000000000000000, 0.000000000000000000 ) ) ;
#38547 = CARTESIAN_POINT ( 'NONE',  ( 4.956653778116997699, 42.88673967249161478, -21.75875759808661059 ) ) ;
#38548 = ORIENTED_EDGE ( 'NONE', *, *, #29132, .T. ) ;
#38549 = EDGE_CURVE ( 'NONE', #12765, #38559, #44781, .T. ) ;
#38550 = CARTESIAN_POINT ( 'NONE',  ( 4.975610109902397937, 30.94437158899635776, -37.88001153774755636 ) ) ;
#38551 = CARTESIAN_POINT ( 'NONE',  ( 1.231276596079887931, 38.25526645152051941, -17.14092645516095104 ) ) ;
#38552 = EDGE_CURVE ( 'NONE', #5530, #40357, #30204, .T. ) ;
#38553 = CARTESIAN_POINT ( 'NONE',  ( 4.000000000000003553, 2.309401076758480720, -5.599999999999999645 ) ) ;
#38554 = EDGE_LOOP ( 'NONE', ( #35613, #39875, #12628, #34110 ) ) ;
#38555 = CARTESIAN_POINT ( 'NONE',  ( 0.6254311100348686203, -44.70341307176172307, 17.77188277739541888 ) ) ;
#38556 = AXIS2_PLACEMENT_3D ( 'NONE', #19367, #38486, #14366 ) ;
#38557 = EDGE_CURVE ( 'NONE', #26909, #13226, #54829, .T. ) ;
#38558 = CARTESIAN_POINT ( 'NONE',  ( 5.960721111146673579, -2.672857320903164524, -20.35079619394245043 ) ) ;
#38559 = VERTEX_POINT ( 'NONE', #21292 ) ;
#38560 = CARTESIAN_POINT ( 'NONE',  ( 0.2224561200757606549, -17.20021002050950898, 39.54039348282952915 ) ) ;
#38561 = AXIS2_PLACEMENT_3D ( 'NONE', #38553, #14740, #5907 ) ;
#38562 = EDGE_LOOP ( 'NONE', ( #31830, #45894, #19863, #1745 ) ) ;
#38563 = FACE_BOUND ( 'NONE', #13040, .T. ) ;
#38564 = VERTEX_POINT ( 'NONE', #3088 ) ;
#38565 = CARTESIAN_POINT ( 'NONE',  ( 3.407937589446178528, -0.4592810312471026224, -13.69123696618924946 ) ) ;
#38566 = CARTESIAN_POINT ( 'NONE',  ( 0.5980271706414734822, -48.61493274831096301, 6.974063142735757559 ) ) ;
#38567 = ORIENTED_EDGE ( 'NONE', *, *, #7457, .T. ) ;
#38568 = CARTESIAN_POINT ( 'NONE',  ( 0.1129192098497447394, 9.345467776859020859, -43.12324222292247811 ) ) ;
#38569 = AXIS2_PLACEMENT_3D ( 'NONE', #13378, #41897, #36265 ) ;
#38570 = EDGE_LOOP ( 'NONE', ( #32649, #8301, #38648, #60986 ) ) ;
#38571 = CARTESIAN_POINT ( 'NONE',  ( 0.5997462898726536595, -25.00873172704203640, -42.26245340191634625 ) ) ;
#38572 = CARTESIAN_POINT ( 'NONE',  ( 0.6009453534118440743, -38.43042294376934365, 28.93865405070883412 ) ) ;
#38573 = EDGE_CURVE ( 'NONE', #53916, #49966, #5672, .T. ) ;
#38574 = ORIENTED_EDGE ( 'NONE', *, *, #44978, .F. ) ;
#38575 = CARTESIAN_POINT ( 'NONE',  ( 0.5782707292762423457, -46.74268073083585762, 3.854627323459990595 ) ) ;
#38576 = CARTESIAN_POINT ( 'NONE',  ( 0.9972139404380309102, 36.82725283858638221, -22.02214929131103105 ) ) ;
#38577 = CARTESIAN_POINT ( 'NONE',  ( 0.5830081025819928708, 17.10943265121773749, 43.66347843147279661 ) ) ;
#38578 = EDGE_LOOP ( 'NONE', ( #232, #9347, #29215, #31502 ) ) ;
#38579 = EDGE_CURVE ( 'NONE', #59637, #36737, #54042, .T. ) ;
#38580 = CARTESIAN_POINT ( 'NONE',  ( 0.5809828226811556418, 44.45562576850601744, 17.82437196699697424 ) ) ;
#38581 = DIRECTION ( 'NONE',  ( -0.07439287786467653485, -0.7144194931002968429, -0.6957517427943147315 ) ) ;
#38582 = ORIENTED_EDGE ( 'NONE', *, *, #21786, .F. ) ;
#38583 = CARTESIAN_POINT ( 'NONE',  ( 0.5786265663353196143, -18.99608782658064854, 43.97352617418609100 ) ) ;
#38584 = EDGE_CURVE ( 'NONE', #58558, #28153, #17742, .T. ) ;
#38585 = ORIENTED_EDGE ( 'NONE', *, *, #51649, .T. ) ;
#38586 = CARTESIAN_POINT ( 'NONE',  ( 1.227938101723748288, 17.20315230597897482, -39.32113113558949635 ) ) ;
#38587 = B_SPLINE_CURVE_WITH_KNOTS ( 'NONE', 3,
 ( #26820, #11188, #12126, #16194 ),
 .UNSPECIFIED., .F., .F.,
 ( 4, 4 ),
 ( 0.000000000000000000, 0.004444103432399267029 ),
 .UNSPECIFIED. ) ;
#38588 = DIRECTION ( 'NONE',  ( 1.000000000000000000, 0.000000000000000000, 0.000000000000000000 ) ) ;
#38589 = ORIENTED_EDGE ( 'NONE', *, *, #30171, .F. ) ;
#38590 = DIRECTION ( 'NONE',  ( -0.07439287786467652097, 0.01320009283086247091, 0.9971416435352943308 ) ) ;
#38591 = CARTESIAN_POINT ( 'NONE',  ( 0.1139756605157202229, 24.91714249760716982, -36.41553555076405502 ) ) ;
#38592 = CARTESIAN_POINT ( 'NONE',  ( 0.8560838555295158248, -42.27062166135473120, 20.33635607586422012 ) ) ;
#38593 = CARTESIAN_POINT ( 'NONE',  ( 0.9775691876210976794, -22.23098038610267935, -35.52628914005386207 ) ) ;
#38594 = EDGE_LOOP ( 'NONE', ( #24654, #48718, #21057, #22996 ) ) ;
#38595 = CARTESIAN_POINT ( 'NONE',  ( 4.999999999999983125, 80.00000000000001421, -3.562970397116383044E-32 ) ) ;
#38596 = CARTESIAN_POINT ( 'NONE',  ( -2.739355103387248747, -14.83685109948651260, -1.647852057280288829 ) ) ;
#38598 = EDGE_CURVE ( 'NONE', #11927, #10882, #42759, .T. ) ;
#38597 = CARTESIAN_POINT ( 'NONE',  ( 0.5834872094924171693, -44.16273175734627898, -18.53852119651611829 ) ) ;
#38599 = CARTESIAN_POINT ( 'NONE',  ( 3.660176727303411592, 1.881607889988430760, -48.00143922595152901 ) ) ;
#38600 = CARTESIAN_POINT ( 'NONE',  ( 2.500000000000000000, 1.178949249685217415, 2.041999999999998483 ) ) ;
#38601 = ADVANCED_FACE ( 'NONE', ( #35405 ), #3677, .F. ) ;
#38602 = CARTESIAN_POINT ( 'NONE',  ( 0.7948884756798515472, -35.86813339442895199, 33.52872874714461915 ) ) ;
#38603 = CARTESIAN_POINT ( 'NONE',  ( 4.553261556744875094, 0.000000000000000000, 0.000000000000000000 ) ) ;
#38604 = AXIS2_PLACEMENT_3D ( 'NONE', #3304, #27135, #36243 ) ;
#38605 = CARTESIAN_POINT ( 'NONE',  ( -16.58482686117664784, -7.842831842844969259, 1.581017821500569243 ) ) ;
#38606 = DIRECTION ( 'NONE',  ( 0.000000000000000000, 0.000000000000000000, -1.000000000000000000 ) ) ;
#38607 = CARTESIAN_POINT ( 'NONE',  ( 0.1119899015040009133, 33.95944448262266491, -28.17299129705921601 ) ) ;
#38608 = AXIS2_PLACEMENT_3D ( 'NONE', #32027, #60498, #54877 ) ;
#38609 = DIRECTION ( 'NONE',  ( 0.09835009131224552170, 0.7847759187265542780, -0.6119264800004700078 ) ) ;
#38610 = CARTESIAN_POINT ( 'NONE',  ( 1.227938101723748288, 33.52879263017863565, 26.79402671879338271 ) ) ;
#38611 = CARTESIAN_POINT ( 'NONE',  ( 0.5800708119828345000, 44.48635609075557085, 17.74761857127083431 ) ) ;
#38612 = CARTESIAN_POINT ( 'NONE',  ( 0.5839879882012675161, -23.94800997596656700, -41.47910964649822319 ) ) ;
#38614 =( BOUNDED_SURFACE ( )  B_SPLINE_SURFACE ( 3, 1, ( 
 ( #42967, #10363 ),
 ( #9416, #10049 ),
 ( #9728, #14450 ),
 ( #24760, #19157 ) ),
 .UNSPECIFIED., .F., .F., .F. ) 
 B_SPLINE_SURFACE_WITH_KNOTS ( ( 4, 4 ),
 ( 2, 2 ),
 ( 0.000000000000000000, 1.000000000000000000 ),
 ( 0.000000000000000000, 1.000000000000000000 ),
 .UNSPECIFIED. ) 
 GEOMETRIC_REPRESENTATION_ITEM ( )  RATIONAL_B_SPLINE_SURFACE ( (
 ( 1.000000000000000000, 1.000000000000000000),
 ( 0.9751682680413298332, 0.9999560080971552356),
 ( 0.9751682680413298332, 0.9999560080971552356),
 ( 1.000000000000000000, 1.000000000000000000) ) ) 
 REPRESENTATION_ITEM ( '' )  SURFACE ( )  );
#38613 =( NAMED_UNIT ( * ) SI_UNIT ( $, .STERADIAN. ) SOLID_ANGLE_UNIT ( ) );
#38615 = CARTESIAN_POINT ( 'NONE',  ( 1.088908134280551998, 34.51503525510850778, 25.50067491870050418 ) ) ;
#38616 = ORIENTED_EDGE ( 'NONE', *, *, #39355, .T. ) ;
#38617 = CARTESIAN_POINT ( 'NONE',  ( 0.5838002273316442725, 29.26514720557072380, -37.91535410490837421 ) ) ;
#38618 = CARTESIAN_POINT ( 'NONE',  ( 0.9784957157296357844, -1.167710547123469222, 41.89235621292397838 ) ) ;
#38619 = CARTESIAN_POINT ( 'NONE',  ( 0.5848930533535030563, 46.89605428954452293, -0.1821385726608810984 ) ) ;
#38620 = VERTEX_POINT ( 'NONE', #55400 ) ;
#38621 = ADVANCED_FACE ( 'NONE', ( #41046 ), #41634, .F. ) ;
#38622 = CARTESIAN_POINT ( 'NONE',  ( 0.9730545539215883499, 5.099196237954877198, 42.60426903087355299 ) ) ;
#38623 = CARTESIAN_POINT ( 'NONE',  ( -6.078075953587585900, 15.42887869085119767, -11.52149628260729308 ) ) ;
#38624 = ADVANCED_FACE ( 'NONE', ( #40421 ), #9590, .F. ) ;
#38625 = PRODUCT_DEFINITION_CONTEXT ( 'detailed design', #2759, 'design' ) ;
#38626 = ORIENTED_EDGE ( 'NONE', *, *, #11040, .T. ) ;
#38627 = EDGE_LOOP ( 'NONE', ( #40160, #5465, #47033, #20650 ) ) ;
#38628 = EDGE_CURVE ( 'NONE', #44492, #13765, #38448, .T. ) ;
#38629 = ORIENTED_EDGE ( 'NONE', *, *, #1379, .T. ) ;
#38630 = EDGE_CURVE ( 'NONE', #40451, #19905, #39893, .T. ) ;
#38631 = CARTESIAN_POINT ( 'NONE',  ( -49.49999999999975842, 5.000000000000000000, 1.078520768856852078E-29 ) ) ;
#38632 = EDGE_CURVE ( 'NONE', #61039, #61495, #7470, .T. ) ;
#38633 = VERTEX_POINT ( 'NONE', #2780 ) ;
#38634 = ORIENTED_EDGE ( 'NONE', *, *, #19067, .F. ) ;
#38635 = CARTESIAN_POINT ( 'NONE',  ( 0.6039202388192953519, -48.72646899558811384, -6.106957677189313038 ) ) ;
#38636 = ORIENTED_EDGE ( 'NONE', *, *, #30122, .F. ) ;
#38637 = CARTESIAN_POINT ( 'NONE',  ( 0.2940133293162995876, -23.55385447652355424, 37.30223168761883556 ) ) ;
#38638 = DIRECTION ( 'NONE',  ( 0.000000000000000000, 0.000000000000000000, -1.000000000000000000 ) ) ;
#38639 = CARTESIAN_POINT ( 'NONE',  ( 4.962356264823608143, 0.000000000000000000, 0.000000000000000000 ) ) ;
#38640 = VERTEX_POINT ( 'NONE', #41347 ) ;
#38641 = CARTESIAN_POINT ( 'NONE',  ( 4.960156602257181468, 45.42786611289310628, 9.558288641081908565 ) ) ;
#38642 = EDGE_CURVE ( 'NONE', #12689, #29464, #11468, .T. ) ;
#38643 = CARTESIAN_POINT ( 'NONE',  ( 0.6031356219577718170, -48.10744328000515679, 0.08729769678294060919 ) ) ;
#38644 = ORIENTED_EDGE ( 'NONE', *, *, #28089, .F. ) ;
#38645 = ORIENTED_EDGE ( 'NONE', *, *, #20508, .T. ) ;
#38646 = CARTESIAN_POINT ( 'NONE',  ( -6.016489644550736315, 14.94663725562931766, -11.47450955518472782 ) ) ;
#38647 = AXIS2_PLACEMENT_3D ( 'NONE', #20448, #54545, #43983 ) ;
#38648 = ORIENTED_EDGE ( 'NONE', *, *, #31551, .F. ) ;
#38649 = CARTESIAN_POINT ( 'NONE',  ( 2.643462169533600914, -44.89050350746163787, 17.09809940585581955 ) ) ;
#38650 = CARTESIAN_POINT ( 'NONE',  ( 0.000000000000000000, 2.357898499370431722, -2.818925648462311528E-15 ) ) ;
#38651 = CARTESIAN_POINT ( 'NONE',  ( 5.965394784446460541, 2.664747781315840225, 20.35165389555759319 ) ) ;
#38652 = CARTESIAN_POINT ( 'NONE',  ( 0.1095718737110178698, 5.374020908746366842, 42.78833451865669701 ) ) ;
#38653 = B_SPLINE_CURVE_WITH_KNOTS ( 'NONE', 3,
 ( #18943, #97, #51807, #51490 ),
 .UNSPECIFIED., .F., .F.,
 ( 4, 4 ),
 ( 8.673617379884035472E-19, 0.004048833967417086489 ),
 .UNSPECIFIED. ) ;
#38654 = ORIENTED_EDGE ( 'NONE', *, *, #16131, .F. ) ;
#38655 = DIRECTION ( 'NONE',  ( 0.000000000000000000, 0.000000000000000000, 1.000000000000000000 ) ) ;
#38656 = CARTESIAN_POINT ( 'NONE',  ( -1.129531546211690163, 8.434754829127421589E-16, 6.887500000000022382 ) ) ;
#38657 = B_SPLINE_CURVE_WITH_KNOTS ( 'NONE', 3,
 ( #4605, #9335, #28438, #23750, #16207, #25287 ),
 .UNSPECIFIED., .F., .F.,
 ( 4, 2, 4 ),
 ( 8.985151752445514084E-18, 0.0002291978881530159432, 0.0004583957763060229418 ),
 .UNSPECIFIED. ) ;
#38658 = LINE ( 'NONE', #57712, #23468 ) ;
#38659 = CARTESIAN_POINT ( 'NONE',  ( 4.694002226626921015, -10.47998749083617653, 44.36726984656654338 ) ) ;
#38660 = VERTEX_POINT ( 'NONE', #3391 ) ;
#38661 = CARTESIAN_POINT ( 'NONE',  ( 2.528190830796654076, -8.172783047358173292, 41.17596086813060197 ) ) ;
#38662 = CARTESIAN_POINT ( 'NONE',  ( 0.5997462898726536595, -14.47257175146244457, -46.92649887902442885 ) ) ;
#38663 = FACE_OUTER_BOUND ( 'NONE', #50382, .T. ) ;
#38664 = CARTESIAN_POINT ( 'NONE',  ( 0.8744876279028263033, -29.90976330662845939, -38.93271258621668096 ) ) ;
#38665 = CONICAL_SURFACE ( 'NONE', #20630, 4.000000000000000000, 1.047197551196595855 ) ;
#38666 = ORIENTED_EDGE ( 'NONE', *, *, #51983, .F. ) ;
#38667 = ORIENTED_EDGE ( 'NONE', *, *, #27230, .F. ) ;
#38668 = LINE ( 'NONE', #34266, #16911 ) ;
#38669 = CARTESIAN_POINT ( 'NONE',  ( -6.016104459813371719, 13.32039631884703113, -13.32794178584983591 ) ) ;
#38670 = CARTESIAN_POINT ( 'NONE',  ( 3.240649175237396484, -32.84582282638324102, 29.26460046293974315 ) ) ;
#38672 = EDGE_CURVE ( 'NONE', #12754, #30302, #22829, .T. ) ;
#38671 = CARTESIAN_POINT ( 'NONE',  ( 5.896278296736517710, -11.93494920661379766, 16.18900759929194422 ) ) ;
#38673 = DIRECTION ( 'NONE',  ( 0.000000000000000000, 0.000000000000000000, -1.000000000000000000 ) ) ;
#38674 = DIRECTION ( 'NONE',  ( -1.000000000000000000, -0.000000000000000000, -0.000000000000000000 ) ) ;
#38675 = LINE ( 'NONE', #58579, #1301 ) ;
#38676 = CARTESIAN_POINT ( 'NONE',  ( 0.1073791018717483448, -16.95003405440287381, -39.65380858626208038 ) ) ;
#38677 = EDGE_CURVE ( 'NONE', #55939, #37522, #26801, .T. ) ;
#38678 = DIRECTION ( 'NONE',  ( 0.8831157194574072999, 5.745494457773168027E-17, 0.4691552259617553511 ) ) ;
#38679 = CARTESIAN_POINT ( 'NONE',  ( 0.5998501479064708430, 18.89267974119668025, -44.24259072156067418 ) ) ;
#38680 = CARTESIAN_POINT ( 'NONE',  ( 0.8560838555295223751, 5.603718208093996012, 46.57221463840868125 ) ) ;
#38681 = CARTESIAN_POINT ( 'NONE',  ( 1.157643937452368155, 3.373327138002636172, -41.78065268296760593 ) ) ;
#38682 = VERTEX_POINT ( 'NONE', #61630 ) ;
#38683 = DIRECTION ( 'NONE',  ( -0.07836865515943411409, -0.3742079063794971905, 0.9240274869783773326 ) ) ;
#38684 = CARTESIAN_POINT ( 'NONE',  ( 0.1365634738349421895, -35.73818327155645846, 25.87749748472385747 ) ) ;
#38685 = B_SPLINE_CURVE_WITH_KNOTS ( 'NONE', 3,
 ( #3564, #3875, #47430, #38061, #18009, #37429 ),
 .UNSPECIFIED., .F., .F.,
 ( 4, 2, 4 ),
 ( 1.266823315017301927E-16, 0.0002450741128632368958, 0.0004901482257263470484 ),
 .UNSPECIFIED. ) ;
#38686 = CARTESIAN_POINT ( 'NONE',  ( 0.5980894510889448457, -0.7015180096008225563, 48.10766805928368228 ) ) ;
#38687 = FACE_OUTER_BOUND ( 'NONE', #40573, .T. ) ;
#38688 = CARTESIAN_POINT ( 'NONE',  ( 5.000000000000012434, -80.00000000000001421, -2.649999999999992806 ) ) ;
#38689 = CARTESIAN_POINT ( 'NONE',  ( 0.7245667037590746151, 23.33692989609111379, -42.06183421678303347 ) ) ;
#38690 = CONTEXT_DEPENDENT_SHAPE_REPRESENTATION ( #53164, #26782 ) ;
#38691 = CARTESIAN_POINT ( 'NONE',  ( 0.9740398440564312921, -25.79088785829005204, 34.29238484271522225 ) ) ;
#38692 = CARTESIAN_POINT ( 'NONE',  ( 0.5997462898726536595, 48.29911994996575686, -8.873930482211887849 ) ) ;
#38693 = CARTESIAN_POINT ( 'NONE',  ( 4.956653778116994147, 32.11725092155092653, -35.79382859084083179 ) ) ;
#38694 = AXIS2_PLACEMENT_3D ( 'NONE', #9832, #58336, #58649 ) ;
#38695 = DIRECTION ( 'NONE',  ( -0.9848077530122077983, -0.1736481776669316079, 1.387778780781445367E-17 ) ) ;
#38696 = CARTESIAN_POINT ( 'NONE',  ( 1.231276596079887264, -37.02495017545888345, 19.65781868679367150 ) ) ;
#38698 = EDGE_LOOP ( 'NONE', ( #43592, #28413, #51451, #34228 ) ) ;
#38697 = CARTESIAN_POINT ( 'NONE',  ( 0.5998501479064699549, -6.798102206413803472, -47.62484632993685807 ) ) ;
#38699 = VERTEX_POINT ( 'NONE', #46652 ) ;
#38700 = CARTESIAN_POINT ( 'NONE',  ( 5.917102823773431552, 19.70720580609864925, -4.014443593801511945 ) ) ;
#38701 = CARTESIAN_POINT ( 'NONE',  ( 0.8554163680231720024, 31.95314001164609152, -34.35407277904558754 ) ) ;
#38702 = VECTOR ( 'NONE', #46662, 1000.000000000000114 ) ;
#38703 = CARTESIAN_POINT ( 'NONE',  ( 0.6253024248130484297, -34.79435467495893164, -34.65251953568179033 ) ) ;
#38704 = ORIENTED_EDGE ( 'NONE', *, *, #61584, .F. ) ;
#38705 = CARTESIAN_POINT ( 'NONE',  ( 3.783198216974387851, 22.99723434398843480, -36.37893817280263420 ) ) ;
#38706 = CARTESIAN_POINT ( 'NONE',  ( 3.238931869106854489, -3.793313187127262065, 42.82436385108072585 ) ) ;
#38707 = DIRECTION ( 'NONE',  ( -1.000000000000000000, -0.000000000000000000, -0.000000000000000000 ) ) ;
#38708 = EDGE_CURVE ( 'NONE', #53909, #50432, #27215, .T. ) ;
#38709 = ORIENTED_EDGE ( 'NONE', *, *, #41078, .F. ) ;
#38710 = ORIENTED_EDGE ( 'NONE', *, *, #39263, .F. ) ;
#38711 = B_SPLINE_CURVE_WITH_KNOTS ( 'NONE', 3,
 ( #9956, #39097, #24661, #43485 ),
 .UNSPECIFIED., .F., .F.,
 ( 4, 4 ),
 ( 0.000000000000000000, 0.004447772540403784232 ),
 .UNSPECIFIED. ) ;
#38712 = CARTESIAN_POINT ( 'NONE',  ( 0.9745511491811759130, -39.51062171155246716, -16.73445648040612355 ) ) ;
#38713 = EDGE_CURVE ( 'NONE', #38682, #55303, #20740, .T. ) ;
#38714 = DIRECTION ( 'NONE',  ( -0.07439287786467650709, -0.6174937095821653177, -0.7830499462674573863 ) ) ;
#38715 = EDGE_CURVE ( 'NONE', #19905, #14965, #14068, .T. ) ;
#38716 = CARTESIAN_POINT ( 'NONE',  ( 3.894904216938897878, -39.85650388126904176, 18.53600363720797262 ) ) ;
#38717 = CARTESIAN_POINT ( 'NONE',  ( 1.227938101723748288, 10.28900963485380693, 41.66816631169195517 ) ) ;
#38718 = EDGE_CURVE ( 'NONE', #60263, #55634, #28654, .T. ) ;
#38719 = CARTESIAN_POINT ( 'NONE',  ( 4.962356264823608143, 0.000000000000000000, 0.000000000000000000 ) ) ;
#38720 = VECTOR ( 'NONE', #17182, 1000.000000000000227 ) ;
#38721 = CARTESIAN_POINT ( 'NONE',  ( 3.678834586032786458, -41.73552251152050729, -25.62730048832143126 ) ) ;
#38722 =( BOUNDED_SURFACE ( )  B_SPLINE_SURFACE ( 3, 1, ( 
 ( #33680, #43396 ),
 ( #52445, #5737 ),
 ( #48376, #24576 ),
 ( #435, #4511 ) ),
 .UNSPECIFIED., .F., .F., .F. ) 
 B_SPLINE_SURFACE_WITH_KNOTS ( ( 4, 4 ),
 ( 2, 2 ),
 ( 0.000000000000000000, 1.000000000000000000 ),
 ( 0.000000000000000000, 1.000000000000000000 ),
 .UNSPECIFIED. ) 
 GEOMETRIC_REPRESENTATION_ITEM ( )  RATIONAL_B_SPLINE_SURFACE ( (
 ( 1.000000000000000000, 1.000000000000000000),
 ( 0.9751682680413298332, 0.9999560080971552356),
 ( 0.9751682680413298332, 0.9999560080971552356),
 ( 1.000000000000000000, 1.000000000000000000) ) ) 
 REPRESENTATION_ITEM ( '' )  SURFACE ( )  );
#38723 = CARTESIAN_POINT ( 'NONE',  ( 0.1073791018717483448, 21.14095454447559419, -37.58707531572184735 ) ) ;
#38724 = EDGE_LOOP ( 'NONE', ( #40071, #19216, #56649, #41741 ) ) ;
#38725 = ORIENTED_EDGE ( 'NONE', *, *, #41553, .T. ) ;
#38726 = CARTESIAN_POINT ( 'NONE',  ( 0.8560838555295158248, -34.16988317699912159, -32.13708010619451727 ) ) ;
#38727 = EDGE_CURVE ( 'NONE', #42399, #6528, #12261, .T. ) ;
#38728 = CARTESIAN_POINT ( 'NONE',  ( 1.154321713695928286, 42.43366804783615720, 6.418927679455782354 ) ) ;
#38729 = VERTEX_POINT ( 'NONE', #42571 ) ;
#38730 = CARTESIAN_POINT ( 'NONE',  ( 0.1145239942831223490, 41.97809357794537277, -13.59356981318502022 ) ) ;
#38731 = CARTESIAN_POINT ( 'NONE',  ( 0.7764146366350247463, -0.6759651462121027965, 46.89971796066871690 ) ) ;
#38732 = CARTESIAN_POINT ( 'NONE',  ( -6.016761891674564211, 9.424569481870250343, 16.31696541414275359 ) ) ;
#38733 = CARTESIAN_POINT ( 'NONE',  ( 0.1135584504625007929, -40.73546803870070221, -16.95799798924523927 ) ) ;
#38734 = ORIENTED_EDGE ( 'NONE', *, *, #11772, .F. ) ;
#38735 = ORIENTED_EDGE ( 'NONE', *, *, #19061, .T. ) ;
#38736 = DIRECTION ( 'NONE',  ( 0.000000000000000000, 0.000000000000000000, -1.000000000000000000 ) ) ;
#38737 = CARTESIAN_POINT ( 'NONE',  ( 0.8554163680231708922, -2.480940174720814184, 46.85136507041470821 ) ) ;
#38738 = CARTESIAN_POINT ( 'NONE',  ( 0.1092565886968784872, -37.50119754628593682, -21.29292791075572921 ) ) ;
#38739 =( BOUNDED_SURFACE ( )  B_SPLINE_SURFACE ( 3, 1, ( 
 ( #42291, #4327 ),
 ( #23463, #53196 ),
 ( #49123, #53493 ),
 ( #48815, #44460 ) ),
 .UNSPECIFIED., .F., .F., .F. ) 
 B_SPLINE_SURFACE_WITH_KNOTS ( ( 4, 4 ),
 ( 2, 2 ),
 ( 0.000000000000000000, 1.000000000000000000 ),
 ( 0.000000000000000000, 1.000000000000000000 ),
 .UNSPECIFIED. ) 
 GEOMETRIC_REPRESENTATION_ITEM ( )  RATIONAL_B_SPLINE_SURFACE ( (
 ( 1.000000000000000000, 1.000000000000000000),
 ( 0.9953040768229013402, 0.8617119497784988535),
 ( 0.9953040768229013402, 0.8617119497784988535),
 ( 1.000000000000000000, 1.000000000000000000) ) ) 
 REPRESENTATION_ITEM ( '' )  SURFACE ( )  );
#38740 = CARTESIAN_POINT ( 'NONE',  ( 0.5839879882012674051, 29.15724166963650177, 37.99840755997057329 ) ) ;
#38741 = ORIENTED_EDGE ( 'NONE', *, *, #60043, .T. ) ;
#38742 = CARTESIAN_POINT ( 'NONE',  ( 4.999999999999996447, 2.650000000000831246, -79.99999999999998579 ) ) ;
#38743 = VERTEX_POINT ( 'NONE', #61941 ) ;
#38744 = CARTESIAN_POINT ( 'NONE',  ( -6.001507490154110336, -18.20581304543294365, -4.862106078788116292 ) ) ;
#38745 = CARTESIAN_POINT ( 'NONE',  ( 0.1147471544378676767, 10.12104602677796272, 42.94783598503057931 ) ) ;
#38746 = ORIENTED_EDGE ( 'NONE', *, *, #23573, .T. ) ;
#38747 = CARTESIAN_POINT ( 'NONE',  ( 1.231276596079887264, 15.85305549123172320, 38.80666698661448777 ) ) ;
#38748 = CIRCLE ( 'NONE', #51673, 43.92652462719577500 ) ;
#38749 = CARTESIAN_POINT ( 'NONE',  ( 0.6017667736363748743, -47.74032759880258681, 5.933018439714516923 ) ) ;
#38750 = CARTESIAN_POINT ( 'NONE',  ( 0.9757892942422826676, 26.08029006934586747, -34.07281211842300195 ) ) ;
#38751 = CARTESIAN_POINT ( 'NONE',  ( -6.017396004339686577, -7.209881890566677498, 17.40926186480777105 ) ) ;
#38752 = CARTESIAN_POINT ( 'NONE',  ( 4.549368137175248350, 0.000000000000000000, 0.000000000000000000 ) ) ;
#38753 = CARTESIAN_POINT ( 'NONE',  ( 0.2885697896453113809, 10.38006191081361784, 41.84838128162063953 ) ) ;
#38754 = CARTESIAN_POINT ( 'NONE',  ( 0.2279481005628792856, -7.789954559295118486, 43.42603015516188947 ) ) ;
#38755 = EDGE_CURVE ( 'NONE', #3487, #40811, #33223, .T. ) ;
#38756 = CARTESIAN_POINT ( 'NONE',  ( 0.9722240741986377666, 34.39263045016090103, -25.65687427836869716 ) ) ;
#38757 = ORIENTED_EDGE ( 'NONE', *, *, #982, .F. ) ;
#38758 = CARTESIAN_POINT ( 'NONE',  ( 0.5839880159502337520, -23.98728323041079946, 41.45643525694599418 ) ) ;
#38759 = DIRECTION ( 'NONE',  ( -1.000000000000000000, -0.000000000000000000, -0.000000000000000000 ) ) ;
#38760 = CARTESIAN_POINT ( 'NONE',  ( 0.6064782688330870863, 3.986484645119572345, 46.72731948863529539 ) ) ;
#38761 = B_SPLINE_CURVE_WITH_KNOTS ( 'NONE', 3,
 ( #39280, #33647, #1324, #38664 ),
 .UNSPECIFIED., .F., .F.,
 ( 4, 4 ),
 ( 0.000000000000000000, 0.004444103432399266161 ),
 .UNSPECIFIED. ) ;
#38762 = ORIENTED_EDGE ( 'NONE', *, *, #4837, .T. ) ;
#38763 = FACE_BOUND ( 'NONE', #57494, .T. ) ;
#38764 = CARTESIAN_POINT ( 'NONE',  ( -4.000000000000000000, -2.309401076758525573, -5.599999999999999645 ) ) ;
#38765 = CARTESIAN_POINT ( 'NONE',  ( 4.549368137175248350, 0.000000000000000000, 0.000000000000000000 ) ) ;
#38766 = FACE_OUTER_BOUND ( 'NONE', #935, .T. ) ;
#38767 = B_SPLINE_CURVE_WITH_KNOTS ( 'NONE', 3,
 ( #7211, #16325, #50753, #11638 ),
 .UNSPECIFIED., .F., .F.,
 ( 4, 4 ),
 ( 2.168404344971008868E-19, 0.004048833967417087357 ),
 .UNSPECIFIED. ) ;
#38768 = FACE_OUTER_BOUND ( 'NONE', #30950, .T. ) ;
#38769 = CARTESIAN_POINT ( 'NONE',  ( 3.270143674763207553, -8.113405361969586949, 11.02405647745167272 ) ) ;
#38770 = CARTESIAN_POINT ( 'NONE',  ( 19.53269999999976392, 1.645856341438826749E-14, 2.006334866415917599E-14 ) ) ;
#38771 = CARTESIAN_POINT ( 'NONE',  ( 4.962356264823594820, 34.94214251265108118, 23.45809613945535332 ) ) ;
#38772 = DIRECTION ( 'NONE',  ( 0.000000000000000000, 0.000000000000000000, 1.000000000000000000 ) ) ;
#38773 = CONICAL_SURFACE ( 'NONE', #49880, 42.92674063221959813, 1.485477209440487556 ) ;
#38774 = LINE ( 'NONE', #15263, #8423 ) ;
#38776 = ORIENTED_EDGE ( 'NONE', *, *, #10260, .T. ) ;
#38775 = CARTESIAN_POINT ( 'NONE',  ( 4.975801465491695552, -27.09127437476353251, -39.51822597168487050 ) ) ;
#38777 = ORIENTED_EDGE ( 'NONE', *, *, #55805, .T. ) ;
#38778 = CARTESIAN_POINT ( 'NONE',  ( 4.833616638992205949, -38.20222678111919379, -26.07076047129122287 ) ) ;
#38779 = DIRECTION ( 'NONE',  ( -1.000000000000000000, -0.000000000000000000, -0.000000000000000000 ) ) ;
#38780 = CARTESIAN_POINT ( 'NONE',  ( 50.50000000000000000, 15.27178771460631168, -2.649999999999992806 ) ) ;
#38781 = LINE ( 'NONE', #1750, #20505 ) ;
#38782 = DIRECTION ( 'NONE',  ( -1.000000000000000000, -0.000000000000000000, -0.000000000000000000 ) ) ;
#38783 = CARTESIAN_POINT ( 'NONE',  ( 5.895596859100789899, -11.92767122914705880, 16.19440774656069237 ) ) ;
#38784 = B_SPLINE_CURVE_WITH_KNOTS ( 'NONE', 3,
 ( #33709, #8959, #43112, #23982, #19606, #149 ),
 .UNSPECIFIED., .F., .F.,
 ( 4, 2, 4 ),
 ( 5.275955480050202716E-18, 0.0002445244328975379987, 0.0004890488657950707932 ),
 .UNSPECIFIED. ) ;
#38785 = ORIENTED_EDGE ( 'NONE', *, *, #17289, .T. ) ;
#38786 = EDGE_CURVE ( 'NONE', #30298, #7613, #56022, .T. ) ;
#38787 = CARTESIAN_POINT ( 'NONE',  ( 0.5804410086790514622, -14.41595396256411910, -44.62846763227064883 ) ) ;
#38788 = AXIS2_PLACEMENT_3D ( 'NONE', #20452, #26381, #59263 ) ;
#38789 = CARTESIAN_POINT ( 'NONE',  ( 0.2885700199627505569, -10.38006184593231573, 41.84838128711406569 ) ) ;
#38790 = AXIS2_PLACEMENT_3D ( 'NONE', #40055, #20907, #5850 ) ;
#38791 = CARTESIAN_POINT ( 'NONE',  ( 4.691466044806102076, 9.025781474741469523, -43.66525414675633954 ) ) ;
#38792 = ORIENTED_EDGE ( 'NONE', *, *, #25961, .F. ) ;
#38793 = EDGE_CURVE ( 'NONE', #12765, #35637, #26429, .T. ) ;
#38794 = B_SPLINE_CURVE_WITH_KNOTS ( 'NONE', 3,
 ( #7859, #31058, #21349, #46105, #44875, #7533 ),
 .UNSPECIFIED., .F., .F.,
 ( 4, 2, 4 ),
 ( 8.741117365843378158E-19, 0.0002450742804987334172, 0.0004901485609974659671 ),
 .UNSPECIFIED. ) ;
#38795 = CARTESIAN_POINT ( 'NONE',  ( 0.5817216825391131607, 43.35051279402986779, 17.88764916645309455 ) ) ;
#38796 = DIRECTION ( 'NONE',  ( 1.000000000000000000, 0.000000000000000000, 0.000000000000000000 ) ) ;
#38797 = VERTEX_POINT ( 'NONE', #53472 ) ;
#38798 = FACE_OUTER_BOUND ( 'NONE', #43802, .T. ) ;
#38799 = ORIENTED_EDGE ( 'NONE', *, *, #12857, .F. ) ;
#38800 = CARTESIAN_POINT ( 'NONE',  ( 52.79985433695213715, 15.44369255379625372, -1.327983408852838387 ) ) ;
#38801 = EDGE_CURVE ( 'NONE', #19244, #56336, #39419, .T. ) ;
#38802 = CARTESIAN_POINT ( 'NONE',  ( 4.549368137175248350, 0.000000000000000000, 0.000000000000000000 ) ) ;
#38803 = B_SPLINE_CURVE_WITH_KNOTS ( 'NONE', 3,
 ( #14702, #58496, #54106, #10930 ),
 .UNSPECIFIED., .F., .F.,
 ( 4, 4 ),
 ( 2.120273707634171606E-17, 0.004444306975806115029 ),
 .UNSPECIFIED. ) ;
#38804 = ORIENTED_EDGE ( 'NONE', *, *, #8319, .F. ) ;
#38805 = CARTESIAN_POINT ( 'NONE',  ( 0.5997462898726536595, 16.46871699354475993, 46.26373299606117229 ) ) ;
#38806 = DIRECTION ( 'NONE',  ( 1.000000000000000000, 1.836909530733573776E-16, 0.000000000000000000 ) ) ;
#38807 = DIRECTION ( 'NONE',  ( 0.000000000000000000, 1.000000000000000000, 0.000000000000000000 ) ) ;
#38808 = DIRECTION ( 'NONE',  ( -0.07836865515943411409, -0.8593913859058586180, 0.5052769534812658891 ) ) ;
#38809 = EDGE_CURVE ( 'NONE', #31065, #29981, #34659, .T. ) ;
#38810 = VECTOR ( 'NONE', #34650, 1000.000000000000227 ) ;
#38811 = ORIENTED_EDGE ( 'NONE', *, *, #21786, .T. ) ;
#38812 = CARTESIAN_POINT ( 'NONE',  ( 5.838029081930955932, -37.05692651727511588, -29.28906374820117620 ) ) ;
#38813 = EDGE_LOOP ( 'NONE', ( #30052, #2539, #11615, #44028 ) ) ;
#38814 = CARTESIAN_POINT ( 'NONE',  ( 0.9762797500689124330, 40.55021165774366665, -10.58324712448374605 ) ) ;
#38815 = ORIENTED_EDGE ( 'NONE', *, *, #17919, .F. ) ;
#38816 = CONICAL_SURFACE ( 'NONE', #12791, 43.08621763946400307, 1.568696531533066763 ) ;
#38817 = VERTEX_POINT ( 'NONE', #48188 ) ;
#38818 = CARTESIAN_POINT ( 'NONE',  ( 0.8554163680231738898, -20.57434774096721242, 42.16517150618003740 ) ) ;
#38819 = CARTESIAN_POINT ( 'NONE',  ( 0.9790724872846768845, 36.07885981586515101, -21.32254873059516243 ) ) ;
#38820 = CARTESIAN_POINT ( 'NONE',  ( 0.9730545539215883499, 25.71816799638778406, 34.34678117142565412 ) ) ;
#38821 = ORIENTED_EDGE ( 'NONE', *, *, #56524, .T. ) ;
#38822 = CARTESIAN_POINT ( 'NONE',  ( 4.975610109902397937, 0.000000000000000000, 0.000000000000000000 ) ) ;
#38823 = CARTESIAN_POINT ( 'NONE',  ( 0.1368894036331269326, -38.12855930276679572, 22.20527620676512726 ) ) ;
#38824 = CARTESIAN_POINT ( 'NONE',  ( 4.975610109902397937, -27.50982196586606321, 40.44328253918227034 ) ) ;
#38825 = ORIENTED_EDGE ( 'NONE', *, *, #29902, .T. ) ;
#38826 = B_SPLINE_CURVE_WITH_KNOTS ( 'NONE', 3,
 ( #25545, #6404, #49351, #11459 ),
 .UNSPECIFIED., .F., .F.,
 ( 4, 4 ),
 ( 2.033478910116247305E-17, 0.004444306975806115029 ),
 .UNSPECIFIED. ) ;
#38827 = ORIENTED_EDGE ( 'NONE', *, *, #1811, .F. ) ;
#38828 = CARTESIAN_POINT ( 'NONE',  ( 0.9790724872846771065, -31.05450468904443895, -28.14165859539148684 ) ) ;
#38829 = CARTESIAN_POINT ( 'NONE',  ( 0.8753041380234530822, 48.01981714478404939, -10.25843502950054109 ) ) ;
#38830 = CARTESIAN_POINT ( 'NONE',  ( 4.549368137175248350, 28.14399996863497577, -32.41327393324110773 ) ) ;
#38831 = EDGE_CURVE ( 'NONE', #13574, #54025, #48724, .T. ) ;
#38832 = CARTESIAN_POINT ( 'NONE',  ( 0.1064266418746774440, 30.09411284098529649, 30.88821921809858750 ) ) ;
#38833 = CARTESIAN_POINT ( 'NONE',  ( 0.8551540677456715978, -29.88829867897840131, 37.45266983663486116 ) ) ;
#38834 = ORIENTED_EDGE ( 'NONE', *, *, #14591, .F. ) ;
#38835 = B_SPLINE_CURVE_WITH_KNOTS ( 'NONE', 3,
 ( #3063, #50673, #59778, #41934 ),
 .UNSPECIFIED., .F., .F.,
 ( 4, 4 ),
 ( 8.673617379884035472E-19, 0.004050076154993000749 ),
 .UNSPECIFIED. ) ;
#38836 = CARTESIAN_POINT ( 'NONE',  ( 0.9783242366443547500, -41.83210916748958397, 2.531626513875353091 ) ) ;
#38837 = ORIENTED_EDGE ( 'NONE', *, *, #48647, .T. ) ;
#38838 = CIRCLE ( 'NONE', #40891, 0.1000000000000002554 ) ;
#38839 = CARTESIAN_POINT ( 'NONE',  ( 2.648799415243708655, -47.06172439114165229, 13.77358198225216235 ) ) ;
#38840 = CARTESIAN_POINT ( 'NONE',  ( 4.256459001490160432, 0.6428830997700460959, 47.05679116045861576 ) ) ;
#38841 = CARTESIAN_POINT ( 'NONE',  ( 0.1147471544378677044, -42.60137459085243705, 11.49239189390608828 ) ) ;
#38842 = DIRECTION ( 'NONE',  ( 1.000000000000000000, 0.000000000000000000, 0.000000000000000000 ) ) ;
#38843 = CARTESIAN_POINT ( 'NONE',  ( 0.6001305935487422083, -41.40054608060309960, 24.50730504006385857 ) ) ;
#38844 = CARTESIAN_POINT ( 'NONE',  ( 5.981074661064941900, 18.95903134304789361, -7.862380442163942718 ) ) ;
#38845 =( BOUNDED_SURFACE ( )  B_SPLINE_SURFACE ( 3, 1, ( 
 ( #17142, #53767 ),
 ( #10901, #54082 ),
 ( #6454, #29990 ),
 ( #20903, #49101 ) ),
 .UNSPECIFIED., .F., .F., .F. ) 
 B_SPLINE_SURFACE_WITH_KNOTS ( ( 4, 4 ),
 ( 2, 2 ),
 ( 0.000000000000000000, 1.000000000000000000 ),
 ( 0.000000000000000000, 1.000000000000000000 ),
 .UNSPECIFIED. ) 
 GEOMETRIC_REPRESENTATION_ITEM ( )  RATIONAL_B_SPLINE_SURFACE ( (
 ( 1.000000000000000000, 1.000000000000000000),
 ( 0.9754377213608244057, 0.9999580625633939235),
 ( 0.9754377213608244057, 0.9999580625633939235),
 ( 1.000000000000000000, 1.000000000000000000) ) ) 
 REPRESENTATION_ITEM ( '' )  SURFACE ( )  );
#38846 = EDGE_LOOP ( 'NONE', ( #5835, #3247, #7167, #61690, #10920 ) ) ;
#38847 = CARTESIAN_POINT ( 'NONE',  ( 0.6001305935487315502, -6.798494447612580593, 47.62765676940931314 ) ) ;
#38848 = CARTESIAN_POINT ( 'NONE',  ( 4.956445790444004018, -45.55738122058057371, -11.91902120403893761 ) ) ;
#38849 = CARTESIAN_POINT ( 'NONE',  ( 0.6846871229502932144, 47.90045233486063836, 0.8641397935261219132 ) ) ;
#38850 = CARTESIAN_POINT ( 'NONE',  ( 2.301430502907646058, 22.89309745268831620, 42.22699195640115022 ) ) ;
#38851 = AXIS2_PLACEMENT_3D ( 'NONE', #45685, #20938, #2735 ) ;
#38852 = FILL_AREA_STYLE_COLOUR ( '', #48246 ) ;
#38853 = CARTESIAN_POINT ( 'NONE',  ( -6.077587904424778920, 7.800189710370596607, 17.60548385805284255 ) ) ;
#38854 = CONICAL_SURFACE ( 'NONE', #49828, 42.92674063221959813, 1.485477209440487556 ) ;
#38855 = CARTESIAN_POINT ( 'NONE',  ( 5.960221823109900008, 20.52559243573973546, -0.005450390361510015769 ) ) ;
#38856 = PRESENTATION_LAYER_ASSIGNMENT (  '', '', ( #34860 ) ) ;
#38857 = ORIENTED_EDGE ( 'NONE', *, *, #58031, .F. ) ;
#38858 = EDGE_CURVE ( 'NONE', #36643, #28137, #56713, .T. ) ;
#38859 = VECTOR ( 'NONE', #61740, 1000.000000000000227 ) ;
#38860 = DIRECTION ( 'NONE',  ( 0.07500201931887537365, -0.2442817726706159320, 0.9667994169624807288 ) ) ;
#38861 = CARTESIAN_POINT ( 'NONE',  ( 0.7057020205115015488, 47.37450661940669505, 7.085441699093776968 ) ) ;
#38862 = CARTESIAN_POINT ( 'NONE',  ( 2.009741617377216460, 40.25399224802043108, 17.86393533685553336 ) ) ;
#38863 = CARTESIAN_POINT ( 'NONE',  ( 5.896782393890504181, -17.30835043929363692, 10.24436879210309925 ) ) ;
#38864 = ORIENTED_EDGE ( 'NONE', *, *, #61164, .F. ) ;
#38865 = EDGE_CURVE ( 'NONE', #11980, #16218, #21226, .T. ) ;
#38866 = CARTESIAN_POINT ( 'NONE',  ( 0.6253024248130452101, 32.50267139205902822, 36.81060417593644729 ) ) ;
#38867 = CARTESIAN_POINT ( 'NONE',  ( 1.199999999999998845, 6.728125000000023448, 0.000000000000000000 ) ) ;
#38868 = EDGE_CURVE ( 'NONE', #15318, #25828, #222, .T. ) ;
#38869 = FACE_OUTER_BOUND ( 'NONE', #50396, .T. ) ;
#38870 = ORIENTED_EDGE ( 'NONE', *, *, #61422, .T. ) ;
#38871 = CARTESIAN_POINT ( 'NONE',  ( 4.549368137175248350, -40.71620287708353914, 13.59764261105679317 ) ) ;
#38872 = CARTESIAN_POINT ( 'NONE',  ( 4.967162193818130511, -40.93989340068619498, 13.42934394584149871 ) ) ;
#38873 = ORIENTED_EDGE ( 'NONE', *, *, #25322, .T. ) ;
#38874 = CIRCLE ( 'NONE', #39864, 10.00000000000000711 ) ;
#38875 = CARTESIAN_POINT ( 'NONE',  ( 2.281448460670575162, 37.24544744441619315, -30.23587867650717698 ) ) ;
#38876 = AXIS2_PLACEMENT_3D ( 'NONE', #54435, #1825, #20953 ) ;
#38877 = ORIENTED_EDGE ( 'NONE', *, *, #49242, .T. ) ;
#38878 = CARTESIAN_POINT ( 'NONE',  ( 0.8557997880470697982, -47.89938907511594834, 0.9121262075944505110 ) ) ;
#38879 = EDGE_LOOP ( 'NONE', ( #52386, #19441 ) ) ;
#38880 = LINE ( 'NONE', #15059, #30705 ) ;
#38881 = CARTESIAN_POINT ( 'NONE',  ( 3.678748215320120973, -48.94071388080758567, 1.849145515207392343 ) ) ;
#38882 = ORIENTED_EDGE ( 'NONE', *, *, #12148, .T. ) ;
#38883 = CARTESIAN_POINT ( 'NONE',  ( 0.8744876279028306332, 3.827863332835647281, -48.94586308039347955 ) ) ;
#38884 = EDGE_CURVE ( 'NONE', #59386, #51399, #36893, .T. ) ;
#38885 = VERTEX_POINT ( 'NONE', #34400 ) ;
#38886 = CARTESIAN_POINT ( 'NONE',  ( 1.231276596079887264, 14.27346765619334512, -39.41503383336959132 ) ) ;
#38887 = CARTESIAN_POINT ( 'NONE',  ( 4.975610109902397937, 48.90928568712962488, -0.5754830253892166958 ) ) ;
#38888 = CARTESIAN_POINT ( 'NONE',  ( 3.783278058412224087, 43.00370293663097954, -1.726763838446331523 ) ) ;
#38889 = EDGE_LOOP ( 'NONE', ( #57470, #3904, #48585, #34297 ) ) ;
#38890 = LINE ( 'NONE', #13001, #61375 ) ;
#38891 = DIRECTION ( 'NONE',  ( 0.000000000000000000, 0.000000000000000000, -1.000000000000000000 ) ) ;
#38892 = AXIS2_PLACEMENT_3D ( 'NONE', #662, #18878, #47365 ) ;
#38893 = CARTESIAN_POINT ( 'NONE',  ( 2.528100132419516477, 16.21066372738161476, 38.72296683042027610 ) ) ;
#38894 = CARTESIAN_POINT ( 'NONE',  ( 5.959828726073459926, -7.858992891710012252, -18.96145866559668747 ) ) ;
#38895 = ORIENTED_EDGE ( 'NONE', *, *, #40193, .T. ) ;
#38896 = CARTESIAN_POINT ( 'NONE',  ( 4.549368137175248350, -13.59764261105780214, 40.71620287708320518 ) ) ;
#38897 = CARTESIAN_POINT ( 'NONE',  ( 0.1156495703730067298, -17.73599580866132541, 40.40269057756201931 ) ) ;
#38898 = VERTEX_POINT ( 'NONE', #14681 ) ;
#38899 = DIRECTION ( 'NONE',  ( 1.000000000000000000, 0.000000000000000000, 0.000000000000000000 ) ) ;
#38900 = B_SPLINE_CURVE_WITH_KNOTS ( 'NONE', 3,
 ( #43901, #48870, #25065, #1240, #53855, #49178 ),
 .UNSPECIFIED., .F., .F.,
 ( 4, 2, 4 ),
 ( 8.547914836739547564E-17, 0.0002293366620881469363, 0.0004586733241762083833 ),
 .UNSPECIFIED. ) ;
#38901 = B_SPLINE_CURVE_WITH_KNOTS ( 'NONE', 3,
 ( #31921, #50696, #27833, #27213 ),
 .UNSPECIFIED., .F., .F.,
 ( 4, 4 ),
 ( 0.000000000000000000, 0.004446090762761349506 ),
 .UNSPECIFIED. ) ;
#38902 = ORIENTED_EDGE ( 'NONE', *, *, #59760, .T. ) ;
#38903 =( GEOMETRIC_REPRESENTATION_CONTEXT ( 3 ) GLOBAL_UNCERTAINTY_ASSIGNED_CONTEXT ( ( #37391 ) ) GLOBAL_UNIT_ASSIGNED_CONTEXT ( ( #22795, #51587, #23111 ) ) REPRESENTATION_CONTEXT ( 'NONE', 'WORKASPACE' ) );
#38904 = CARTESIAN_POINT ( 'NONE',  ( 7.999999999999996447, 8.394250489469390599E-13, -80.00000000000001421 ) ) ;
#38905 = FACE_OUTER_BOUND ( 'NONE', #58451, .T. ) ;
#38906 = ORIENTED_EDGE ( 'NONE', *, *, #37868, .T. ) ;
#38907 = CARTESIAN_POINT ( 'NONE',  ( -6.016104459813371719, -4.871830707673185934, 18.20253432612965838 ) ) ;
#38908 = DIRECTION ( 'NONE',  ( -1.000000000000000000, -0.000000000000000000, 1.925929944387235853E-32 ) ) ;
#38909 = CARTESIAN_POINT ( 'NONE',  ( 2.282803330402976449, 46.71114521383905327, -4.956391859874321959 ) ) ;
#38910 = CARTESIAN_POINT ( 'NONE',  ( 0.5998501479064699549, -48.10473956285919428, 0.5236536531313263909 ) ) ;
#38911 = ORIENTED_EDGE ( 'NONE', *, *, #23837, .T. ) ;
#38912 = CARTESIAN_POINT ( 'NONE',  ( 5.917102823773431552, 0.6806365918031147544, 20.10040924662084194 ) ) ;
#38913 = AXIS2_PLACEMENT_3D ( 'NONE', #61602, #51911, #9001 ) ;
#38914 = EDGE_CURVE ( 'NONE', #38229, #53499, #25290, .T. ) ;
#38915 = DIRECTION ( 'NONE',  ( 0.09835009131224552170, -0.9632152266566406107, -0.2500873580884673819 ) ) ;
#38916 = CARTESIAN_POINT ( 'NONE',  ( 0.9789889208857707192, 41.52179126368472595, -5.681174904662252167 ) ) ;
#38917 = EDGE_CURVE ( 'NONE', #58012, #53765, #22669, .T. ) ;
#38918 = CARTESIAN_POINT ( 'NONE',  ( 5.959547316686252039, -17.77392908783926728, -10.26589671991357022 ) ) ;
#38919 = CARTESIAN_POINT ( 'NONE',  ( 2.528100132419517365, -41.36196155245985295, -7.172301943233399868 ) ) ;
#38920 =( BOUNDED_SURFACE ( )  B_SPLINE_SURFACE ( 3, 1, ( 
 ( #18961, #24566 ),
 ( #58055, #53358 ),
 ( #425, #15480 ),
 ( #20187, #48368 ) ),
 .UNSPECIFIED., .F., .F., .F. ) 
 B_SPLINE_SURFACE_WITH_KNOTS ( ( 4, 4 ),
 ( 2, 2 ),
 ( 0.000000000000000000, 1.000000000000000000 ),
 ( 0.000000000000000000, 1.000000000000000000 ),
 .UNSPECIFIED. ) 
 GEOMETRIC_REPRESENTATION_ITEM ( )  RATIONAL_B_SPLINE_SURFACE ( (
 ( 1.000000000000000000, 1.000000000000000000),
 ( 0.9952954269826590483, 0.8620686068821307169),
 ( 0.9952954269826590483, 0.8620686068821307169),
 ( 1.000000000000000000, 1.000000000000000000) ) ) 
 REPRESENTATION_ITEM ( '' )  SURFACE ( )  );
#38921 = DIRECTION ( 'NONE',  ( -1.000000000000000000, 0.000000000000000000, 0.000000000000000000 ) ) ;
#38922 = EDGE_CURVE ( 'NONE', #51483, #34855, #43502, .T. ) ;
#38923 = CARTESIAN_POINT ( 'NONE',  ( 4.549368137175248350, 0.000000000000000000, 0.000000000000000000 ) ) ;
#38924 = VECTOR ( 'NONE', #42217, 1000.000000000000000 ) ;
#38925 = CARTESIAN_POINT ( 'NONE',  ( -15.94139450991274209, -7.982454930101551049, -0.5465034650385233173 ) ) ;
#38926 = CARTESIAN_POINT ( 'NONE',  ( 1.231276596079881047, 5.037240371906286818, -41.61613846158368091 ) ) ;
#38927 = CARTESIAN_POINT ( 'NONE',  ( 5.838029081930955932, 13.97520979541447339, 45.11938130479041575 ) ) ;
#38928 = CARTESIAN_POINT ( 'NONE',  ( 0.1147471544378676073, -43.80064347916233913, -5.334399618003720533 ) ) ;
#38929 = CARTESIAN_POINT ( 'NONE',  ( 0.1157506346131639274, 39.79465037914078351, 19.06112433737277101 ) ) ;
#38930 = EDGE_CURVE ( 'NONE', #33742, #60718, #55600, .T. ) ;
#38931 = CARTESIAN_POINT ( 'NONE',  ( 0.7044674535452954967, -45.19827881396718539, -19.20724642070773669 ) ) ;
#38932 = CARTESIAN_POINT ( 'NONE',  ( 4.322998006666165516, 47.80838462754065432, -4.155494336618213325 ) ) ;
#38933 = ORIENTED_EDGE ( 'NONE', *, *, #10768, .F. ) ;
#38934 = VECTOR ( 'NONE', #40145, 1000.000000000000000 ) ;
#38935 = CARTESIAN_POINT ( 'NONE',  ( 0.1365634738349416066, -44.11867064301219443, -0.6368047712308788633 ) ) ;
#38936 = CARTESIAN_POINT ( 'NONE',  ( 0.7413678028165013867, 19.56431516233115886, -39.51864957205928874 ) ) ;
#38937 = CARTESIAN_POINT ( 'NONE',  ( 0.7048096507298579061, -24.78213711671627451, 41.23648859290882740 ) ) ;
#38938 = ORIENTED_EDGE ( 'NONE', *, *, #58959, .F. ) ;
#38939 = CARTESIAN_POINT ( 'NONE',  ( 5.272379999999998290, 0.000000000000000000, 0.000000000000000000 ) ) ;
#38940 = CARTESIAN_POINT ( 'NONE',  ( 2.879087469061463622, 26.57443547924880178, 35.06994519161131052 ) ) ;
#38941 = EDGE_CURVE ( 'NONE', #371, #20909, #59256, .T. ) ;
#38942 = PRODUCT_DEFINITION_FORMATION_WITH_SPECIFIED_SOURCE ( 'ANY', '', #16255, .NOT_KNOWN. ) ;
#38943 = ORIENTED_EDGE ( 'NONE', *, *, #44713, .F. ) ;
#38944 = ORIENTED_EDGE ( 'NONE', *, *, #21395, .T. ) ;
#38945 = CARTESIAN_POINT ( 'NONE',  ( 0.5980271706414734822, 22.09347986454800861, -43.86259671196490473 ) ) ;
#38946 = ORIENTED_EDGE ( 'NONE', *, *, #49452, .T. ) ;
#38947 = CARTESIAN_POINT ( 'NONE',  ( 4.975610109902397937, 47.45567470742105343, -11.84940273605426242 ) ) ;
#38948 = ORIENTED_EDGE ( 'NONE', *, *, #32508, .F. ) ;
#38949 = VERTEX_POINT ( 'NONE', #45050 ) ;
#38950 = CARTESIAN_POINT ( 'NONE',  ( 0.1098349054025746646, 10.95525583467218134, 41.70974743324818235 ) ) ;
#38951 = ORIENTED_EDGE ( 'NONE', *, *, #35305, .F. ) ;
#38952 = DIRECTION ( 'NONE',  ( 0.1736481776669315524, -0.9848077530122079093, 5.551115123125782702E-17 ) ) ;
#38953 = CARTESIAN_POINT ( 'NONE',  ( 0.9722240741986383217, 39.41582013185147559, 16.95645453362478960 ) ) ;
#38954 = EDGE_CURVE ( 'NONE', #52762, #57626, #33891, .T. ) ;
#38955 = CARTESIAN_POINT ( 'NONE',  ( 0.9789233960466696693, -17.52144526371232303, -38.07014161653558659 ) ) ;
#38956 = VERTEX_POINT ( 'NONE', #2078 ) ;
#38957 = CARTESIAN_POINT ( 'NONE',  ( -90.00000000000000000, 8.434754829127421589E-16, 6.887500000000022382 ) ) ;
#38958 = VECTOR ( 'NONE', #357, 1000.000000000000114 ) ;
#38959 = CARTESIAN_POINT ( 'NONE',  ( 0.9736507210033056303, -33.76542629919387650, -26.47691119766824741 ) ) ;
#38960 = ORIENTED_EDGE ( 'NONE', *, *, #50077, .F. ) ;
#38961 = ORIENTED_EDGE ( 'NONE', *, *, #32900, .F. ) ;
#38962 = CIRCLE ( 'NONE', #45988, 2.041999999999999815 ) ;
#38963 = CARTESIAN_POINT ( 'NONE',  ( 48.74944754206161690, 12.34007061358912871, 1.996972717666336550 ) ) ;
#38964 = CARTESIAN_POINT ( 'NONE',  ( 0.6001305935487315502, 5.760103278698018414, -47.76436356026962216 ) ) ;
#38965 = DIRECTION ( 'NONE',  ( -0.07906939808003034253, 0.4861426559824175153, 0.8702949777642189355 ) ) ;
#38966 = DIRECTION ( 'NONE',  ( 1.000000000000000000, 0.000000000000000000, 0.000000000000000000 ) ) ;
#38967 = ORIENTED_EDGE ( 'NONE', *, *, #34770, .F. ) ;
#38968 = CARTESIAN_POINT ( 'NONE',  ( 4.322998006666165516, 2.120302895116279451, -47.94177812210862299 ) ) ;
#38969 = CARTESIAN_POINT ( 'NONE',  ( 4.962356264823601926, -41.65024625884322518, 6.040909239515423579 ) ) ;
#38970 = ORIENTED_EDGE ( 'NONE', *, *, #43146, .T. ) ;
#38971 = CARTESIAN_POINT ( 'NONE',  ( 5.981074661064941900, -17.77917279944625051, -10.25489689131124216 ) ) ;
#38972 = CARTESIAN_POINT ( 'NONE',  ( 0.1149546198390367646, 37.12868760141555668, -23.84129027589972338 ) ) ;
#38973 = CARTESIAN_POINT ( 'NONE',  ( 0.9762797500689124330, -22.97506929404208975, 35.04955029839425151 ) ) ;
#38974 = DIRECTION ( 'NONE',  ( 0.000000000000000000, 0.000000000000000000, 1.000000000000000000 ) ) ;
#38975 = ORIENTED_EDGE ( 'NONE', *, *, #24947, .T. ) ;
#38976 = ORIENTED_EDGE ( 'NONE', *, *, #40830, .F. ) ;
#38977 = CARTESIAN_POINT ( 'NONE',  ( 5.960721111146673579, 16.28018152803675633, 12.50019045452743782 ) ) ;
#38978 = CARTESIAN_POINT ( 'NONE',  ( 0.7057020205115038802, -13.20843872046520673, 46.04437542275042006 ) ) ;
#38979 = EDGE_CURVE ( 'NONE', #38501, #5305, #684, .T. ) ;
#38980 = CARTESIAN_POINT ( 'NONE',  ( 1.827326673878742369, -37.88339879236874452, 20.44853789448387360 ) ) ;
#38981 = CARTESIAN_POINT ( 'NONE',  ( -6.016104459813374383, 9.416989654584305924, 16.32137543786086198 ) ) ;
#38982 = CARTESIAN_POINT ( 'NONE',  ( 4.967162193818130511, 7.970725651239789045, 42.34252806656596846 ) ) ;
#38983 = EDGE_CURVE ( 'NONE', #2858, #52304, #51834, .T. ) ;
#38984 = CARTESIAN_POINT ( 'NONE',  ( 0.1152809850208375425, -31.85007772001079829, 30.53715493819007776 ) ) ;
#38985 = CARTESIAN_POINT ( 'NONE',  ( 30.00000000000001066, 4.342925291379521108E-15, -1.386669559958810165E-30 ) ) ;
#38986 = CARTESIAN_POINT ( 'NONE',  ( -6.079354080745853928, -17.34954932540436090, -8.353807123313488958 ) ) ;
#38987 = CARTESIAN_POINT ( 'NONE',  ( 0.5804410086790514622, -44.12183670707856464, -15.89916279082931005 ) ) ;
#38988 = EDGE_CURVE ( 'NONE', #44297, #22420, #23441, .T. ) ;
#38989 = CARTESIAN_POINT ( 'NONE',  ( 2.528190830796658517, -11.27641220880940409, -40.43632851595235422 ) ) ;
#38990 =( BOUNDED_SURFACE ( )  B_SPLINE_SURFACE ( 3, 1, ( 
 ( #51304, #36322 ),
 ( #8389, #51003 ),
 ( #31600, #27512 ),
 ( #7780, #16904 ) ),
 .UNSPECIFIED., .F., .F., .F. ) 
 B_SPLINE_SURFACE_WITH_KNOTS ( ( 4, 4 ),
 ( 2, 2 ),
 ( 0.000000000000000000, 1.000000000000000000 ),
 ( 0.000000000000000000, 1.000000000000000000 ),
 .UNSPECIFIED. ) 
 GEOMETRIC_REPRESENTATION_ITEM ( )  RATIONAL_B_SPLINE_SURFACE ( (
 ( 1.000000000000000000, 1.000000000000000000),
 ( 0.9953485035131437453, 0.8621029689291515030),
 ( 0.9953485035131437453, 0.8621029689291515030),
 ( 1.000000000000000000, 1.000000000000000000) ) ) 
 REPRESENTATION_ITEM ( '' )  SURFACE ( )  );
#38991 = EDGE_CURVE ( 'NONE', #18385, #5387, #30596, .T. ) ;
#38992 = CARTESIAN_POINT ( 'NONE',  ( 4.967162193818130511, -2.375726030842277403, -43.02067033766020643 ) ) ;
#38993 = EDGE_LOOP ( 'NONE', ( #58962, #12450, #36889, #48315 ) ) ;
#38994 = EDGE_CURVE ( 'NONE', #59424, #36040, #20445, .T. ) ;
#38995 = CARTESIAN_POINT ( 'NONE',  ( 0.6067375320500716374, -28.59217831626991213, -38.42671567536882549 ) ) ;
#38996 = CARTESIAN_POINT ( 'NONE',  ( 0.8557997880470690211, 23.15977007032381607, -41.93815086860232810 ) ) ;
#38997 = CARTESIAN_POINT ( 'NONE',  ( 2.648799415243708655, -43.38879977521469300, -22.84577679475856371 ) ) ;
#38998 = CARTESIAN_POINT ( 'NONE',  ( 0.1119899015040011631, -27.07006270142763782, -34.84498548619703939 ) ) ;
#38999 = B_SPLINE_CURVE_WITH_KNOTS ( 'NONE', 3,
 ( #25190, #29579, #39944, #24893 ),
 .UNSPECIFIED., .F., .F.,
 ( 4, 4 ),
 ( 2.343940034265376918E-17, 0.004564976165746186844 ),
 .UNSPECIFIED. ) ;
#39000 = CARTESIAN_POINT ( 'NONE',  ( -90.00000000000000000, 0.000000000000000000, -7.500000000000022204 ) ) ;
#39001 = CARTESIAN_POINT ( 'NONE',  ( 0.6016118706126977189, 33.27208259263638013, -36.11813359979602467 ) ) ;
#39002 = CARTESIAN_POINT ( 'NONE',  ( 43.00000000000000000, 0.000000000000000000, 0.000000000000000000 ) ) ;
#39003 = CARTESIAN_POINT ( 'NONE',  ( 5.959547316686252039, -2.682663672455063431, 20.34955788964371948 ) ) ;
#39004 = AXIS2_PLACEMENT_3D ( 'NONE', #34225, #24189, #29195 ) ;
#39005 = CARTESIAN_POINT ( 'NONE',  ( 0.6253024248130506502, 48.32746506278895282, -8.712080579434449135 ) ) ;
#39006 = EDGE_CURVE ( 'NONE', #5333, #12545, #45105, .T. ) ;
#39007 = CARTESIAN_POINT ( 'NONE',  ( 0.9730545539215892381, -10.61654491617593266, 41.57420493492382008 ) ) ;
#39008 = EDGE_CURVE ( 'NONE', #22114, #49237, #54774, .T. ) ;
#39009 = CARTESIAN_POINT ( 'NONE',  ( 0.5980894510889448457, -13.12879507229320630, 46.28687279963669710 ) ) ;
#39010 = CARTESIAN_POINT ( 'NONE',  ( -6.078457390727109555, 3.068934028528590652, -19.00989623764546721 ) ) ;
#39012 = ORIENTED_EDGE ( 'NONE', *, *, #54172, .F. ) ;
#39011 = CARTESIAN_POINT ( 'NONE',  ( 0.9730545539215883499, -30.69604515769629316, -29.98130006528894498 ) ) ;
#39013 = ORIENTED_EDGE ( 'NONE', *, *, #41633, .T. ) ;
#39014 = AXIS2_PLACEMENT_3D ( 'NONE', #60025, #36249, #30589 ) ;
#39015 = CARTESIAN_POINT ( 'NONE',  ( 1.000110580585048980, 36.38996880054845207, -20.78912344152613301 ) ) ;
#39016 = CARTESIAN_POINT ( 'NONE',  ( 3.559346040607745287, 43.70094520706050645, -4.863915043612893285 ) ) ;
#39017 = CARTESIAN_POINT ( 'NONE',  ( 0.7242486021783847150, -34.69771184318253887, -34.74306053331289235 ) ) ;
#39018 = VERTEX_POINT ( 'NONE', #16212 ) ;
#39019 = CARTESIAN_POINT ( 'NONE',  ( 2.528100132419517365, 40.15111052815427684, -12.25324862997623931 ) ) ;
#39020 = LINE ( 'NONE', #28974, #53150 ) ;
#39021 = CARTESIAN_POINT ( 'NONE',  ( 0.5839879882012689594, -41.47913983251933701, -23.94795769224428739 ) ) ;
#39022 = ORIENTED_EDGE ( 'NONE', *, *, #49831, .T. ) ;
#39023 = ORIENTED_EDGE ( 'NONE', *, *, #46686, .F. ) ;
#39024 = B_SPLINE_CURVE_WITH_KNOTS ( 'NONE', 3,
 ( #16803, #60602, #17721, #51515 ),
 .UNSPECIFIED., .F., .F.,
 ( 4, 4 ),
 ( 0.000000000000000000, 0.004447772540403811120 ),
 .UNSPECIFIED. ) ;
#39025 = CARTESIAN_POINT ( 'NONE',  ( 0.6025881611877910160, -23.86454577211535977, -41.77096849334441941 ) ) ;
#39026 = VECTOR ( 'NONE', #17399, 1000.000000000000000 ) ;
#39027 = DIRECTION ( 'NONE',  ( 0.000000000000000000, 0.000000000000000000, -1.000000000000000000 ) ) ;
#39028 = CARTESIAN_POINT ( 'NONE',  ( -6.010958268070873523, -4.863021950010519845, -18.20513189769813778 ) ) ;
#39029 = CARTESIAN_POINT ( 'NONE',  ( 0.1365634738349393862, 14.63942591880842770, 41.62390933575277074 ) ) ;
#39030 = CARTESIAN_POINT ( 'NONE',  ( 0.9772918015221183641, -41.14952526578677805, -7.940618751146248933 ) ) ;
#39031 = EDGE_CURVE ( 'NONE', #8791, #1476, #37764, .T. ) ;
#39032 = CARTESIAN_POINT ( 'NONE',  ( 0.8560838555295223751, -13.02223058219873764, 45.06433561859954295 ) ) ;
#39033 = EDGE_CURVE ( 'NONE', #56156, #33009, #29381, .T. ) ;
#39034 = CARTESIAN_POINT ( 'NONE',  ( 0.9756008150404590351, 42.55970871350812956, 5.459718823765672191 ) ) ;
#39035 = VERTEX_POINT ( 'NONE', #50938 ) ;
#39036 = ORIENTED_EDGE ( 'NONE', *, *, #10941, .F. ) ;
#39037 = CARTESIAN_POINT ( 'NONE',  ( 4.691466044806103852, 39.84135254923136671, -20.01963481131618039 ) ) ;
#39038 = CARTESIAN_POINT ( 'NONE',  ( 1.479689385636123067, 44.03253894626729448, 1.649047971753838215 ) ) ;
#39039 = ORIENTED_EDGE ( 'NONE', *, *, #24176, .T. ) ;
#39040 = CARTESIAN_POINT ( 'NONE',  ( -5.995132425357893702, -13.31880955509736530, 13.33084941932902723 ) ) ;
#39041 = CARTESIAN_POINT ( 'NONE',  ( -6.057079549204054558, 17.84642505839074644, 7.234386203056984321 ) ) ;
#39042 = CARTESIAN_POINT ( 'NONE',  ( 2.299652685299202748, -21.01913371789099827, 44.29986165449697211 ) ) ;
#39043 = CARTESIAN_POINT ( 'NONE',  ( 4.962356264823608143, -9.332162870646227404, -41.03835198954849517 ) ) ;
#39044 = VERTEX_POINT ( 'NONE', #42200 ) ;
#39045 = CARTESIAN_POINT ( 'NONE',  ( 0.5806925824938502512, 46.40146083665138832, -6.791670970259978013 ) ) ;
#39046 = CARTESIAN_POINT ( 'NONE',  ( 0.9758171775293911221, -42.54217005300507992, -5.594812732687539203 ) ) ;
#39047 = CARTESIAN_POINT ( 'NONE',  ( 4.958415959904820980, 40.76596448693046426, -20.03347431857393346 ) ) ;
#39048 = CARTESIAN_POINT ( 'NONE',  ( 5.895881250540457863, -11.92688455204506681, 16.19497164216380369 ) ) ;
#39049 = EDGE_LOOP ( 'NONE', ( #8807, #56163, #55721, #40722 ) ) ;
#39050 = CARTESIAN_POINT ( 'NONE',  ( 0.6016117650947689910, 4.368597403151937009, -48.91284505090327883 ) ) ;
#39051 = ORIENTED_EDGE ( 'NONE', *, *, #23844, .F. ) ;
#39052 = CARTESIAN_POINT ( 'NONE',  ( 5.896782393890504181, -9.660289833039602314, 17.64100017628490136 ) ) ;
#39053 = CARTESIAN_POINT ( 'NONE',  ( 0.5832366564991493529, 23.71163571971582229, -41.61464700196751210 ) ) ;
#39054 = ORIENTED_EDGE ( 'NONE', *, *, #49536, .T. ) ;
#39055 = CARTESIAN_POINT ( 'NONE',  ( 0.8751705887134553219, -5.393078191593054349, 47.79200036674269825 ) ) ;
#39056 = DIRECTION ( 'NONE',  ( -1.000000000000000000, -0.000000000000000000, -0.000000000000000000 ) ) ;
#39057 = EDGE_CURVE ( 'NONE', #20008, #25113, #16745, .T. ) ;
#39058 = DIRECTION ( 'NONE',  ( -1.000000000000000000, -0.000000000000000000, -0.000000000000000000 ) ) ;
#39059 = B_SPLINE_CURVE_WITH_KNOTS ( 'NONE', 3,
 ( #47218, #4265, #37212, #41918 ),
 .UNSPECIFIED., .F., .F.,
 ( 4, 4 ),
 ( 0.000000000000000000, 0.005014147105413703856 ),
 .UNSPECIFIED. ) ;
#39060 = EDGE_CURVE ( 'NONE', #61765, #15970, #1738, .T. ) ;
#39061 = CARTESIAN_POINT ( 'NONE',  ( 0.7056555295713272669, -19.10539864320367798, -43.92642606846697362 ) ) ;
#39062 = CARTESIAN_POINT ( 'NONE',  ( 0.8554163680231738898, 17.71207986799998224, -43.44522643353823099 ) ) ;
#39063 = CARTESIAN_POINT ( 'NONE',  ( 2.185380717157382691, 21.63101079767031010, 38.35256412468753950 ) ) ;
#39064 = CLOSED_SHELL ( 'NONE', ( #44378, #47250, #44862, #34514, #8484, #15713, #14170, #42687, #10257, #57707, #18995, #2090, #21718, #47115, #44709, #13110, #41676, #12184, #21504, #30982, #57484, #44555, #27127, #7405, #20799, #15204, #24083, #9992, #46732, #41266, #16322, #22569, #26329, #22636, #13300, #61090, #13750, #18910, #27574, #35515, #53455, #57847, #57544, #56935, #56832, #58594, #35360, #29125, #41847, #35832, #29139, #30812, #49669, #12620, #39643, #13306, #60406, #40554, #37266, #12803, #32874, #55147, #13220, #8461, #30448, #30975, #35090, #58650, #59356, #41677, #49883, #38624, #33904, #8989, #26097, #53822, #33418, #10835, #55443, #11820, #39506, #4995, #24671, #4812, #26967, #39075, #31056, #33373, #10843, #53111, #11119, #58491, #37445, #36734, #39286, #11079, #42018, #8244, #26616, #32116, #41506, #46143, #35507, #54353, #26026, #25047, #7179, #42895, #27456, #5088, #59527, #12598, #567, #48573, #18292, #39819, #36646, #43736, #46406, #35947, #1428, #30301, #28277, #57919, #40297, #56744, #57820, #46434, #1211, #2896, #13730, #39815, #1375, #39322, #38402, #59167, #61752, #17427, #48173, #41051, #9386, #36304, #61882, #16404, #56008, #43049, #15360, #2542, #54231, #28632, #42080, #48584, #38200, #4058, #11822, #12295, #10476, #28375, #11157, #17161, #17274, #59831, #19777, #58533, #5012, #54551, #3362, #22084, #9068, #33881, #37502, #40564, #8472, #31982, #25824, #11115, #54450, #34738, #49317, #7346, #56696, #17553, #37580, #24409, #30060, #9108, #53672, #60400, #1576, #56144, #36210, #1981, #8881, #57267, #50328, #20442, #59388, #51554, #41745, #51479, #42100, #48723, #533, #24863, #26261, #15948, #23784, #50756, #339, #1533, #35041, #9080, #16069, #29128, #3227, #36313, #13880, #6828, #35555, #34109, #27084, #45493, #9154, #48434, #31476, #7373, #15335, #51187, #14885, #51602, #5268, #43984, #60721, #48523, #43244, #56443, #17900, #31273, #5846, #39363, #20316, #16946, #58176, #30755, #60444, #55823, #10130, #23606, #14799, #11654, #60592, #45837, #54511, #40131, #12056, #5461, #2234, #47835, #8767, #7176, #1198, #57234, #57852, #2152, #16056, #27790, #43506, #42310, #36846, #27253, #1463, #33758, #13179, #43104, #24323, #37794, #58929, #2600, #3522, #59633, #8841, #8336, #48116, #4508, #36338, #23415, #52204, #45887, #11838, #57054, #57212, #51475, #31915 ) ) ;
#39065 = CARTESIAN_POINT ( 'NONE',  ( 0.6025881611877910160, 29.45877655626793512, -38.03302298778312718 ) ) ;
#39066 = CARTESIAN_POINT ( 'NONE',  ( 0.8760168074886960365, 7.161346975773699164, -47.56749362999706676 ) ) ;
#39067 = ORIENTED_EDGE ( 'NONE', *, *, #3125, .T. ) ;
#39068 = CARTESIAN_POINT ( 'NONE',  ( 0.8554163680231816613, 46.90810212776801791, -0.9140174411379278219 ) ) ;
#39069 = EDGE_CURVE ( 'NONE', #57986, #12452, #11764, .T. ) ;
#39070 = DIRECTION ( 'NONE',  ( -1.000000000000000000, -0.000000000000000000, -0.000000000000000000 ) ) ;
#39071 = EDGE_CURVE ( 'NONE', #25523, #31232, #46601, .T. ) ;
#39072 = FACE_OUTER_BOUND ( 'NONE', #36677, .T. ) ;
#39073 = VECTOR ( 'NONE', #27957, 1000.000000000000227 ) ;
#39074 = VERTEX_POINT ( 'NONE', #32788 ) ;
#39075 = ADVANCED_FACE ( 'NONE', ( #17440 ), #29172, .F. ) ;
#39076 = CARTESIAN_POINT ( 'NONE',  ( -15.92917370011572409, -12.49037116071005116, 0.5520084180848008337 ) ) ;
#39077 = CARTESIAN_POINT ( 'NONE',  ( 1.231276596079887264, 32.36747132271594296, -26.63876069172940930 ) ) ;
#39078 = CARTESIAN_POINT ( 'NONE',  ( 0.7948878604505662526, 10.07807612458116253, -48.05341849364687334 ) ) ;
#39079 = CARTESIAN_POINT ( 'NONE',  ( 0.1073791018717578927, 42.68962945260945929, 6.109314776652849943 ) ) ;
#39080 = FACE_OUTER_BOUND ( 'NONE', #24193, .T. ) ;
#39081 = CARTESIAN_POINT ( 'NONE',  ( 0.6027935024548037868, 38.27223087442848026, -29.14731236071028775 ) ) ;
#39082 = DIRECTION ( 'NONE',  ( -1.000000000000000000, -3.135800716341495207E-16, 1.298891185607918966E-16 ) ) ;
#39083 = CARTESIAN_POINT ( 'NONE',  ( 0.8557997880470697982, -7.156447707085392018, -47.37054680076713709 ) ) ;
#39084 = DIRECTION ( 'NONE',  ( 1.000000000000000000, 0.000000000000000000, 0.000000000000000000 ) ) ;
#39085 = CARTESIAN_POINT ( 'NONE',  ( 5.959547316686252039, 19.82715097195162457, -5.308980600728250288 ) ) ;
#39086 = EDGE_LOOP ( 'NONE', ( #43197, #4063 ) ) ;
#39087 = EDGE_LOOP ( 'NONE', ( #6081, #38129, #57209, #37575 ) ) ;
#39088 = CARTESIAN_POINT ( 'NONE',  ( 3.660087539127319101, -27.72868323267833901, 39.22752134874908592 ) ) ;
#39089 = FACE_BOUND ( 'NONE', #4236, .T. ) ;
#39090 = CARTESIAN_POINT ( 'NONE',  ( 3.238741278300274473, -29.07934833201346336, -31.66556122967947928 ) ) ;
#39091 = CARTESIAN_POINT ( 'NONE',  ( 0.1147471544378676767, -22.60761324532118266, 37.89258518263465447 ) ) ;
#39092 = CARTESIAN_POINT ( 'NONE',  ( 0.5850706913938533704, 47.46255051844953954, 6.431767090162980871 ) ) ;
#39093 = CARTESIAN_POINT ( 'NONE',  ( 0.1147471544378676350, 9.515620283457987938, -43.08602046017117004 ) ) ;
#39094 =( BOUNDED_SURFACE ( )  B_SPLINE_SURFACE ( 3, 1, ( 
 ( #1581, #20409 ),
 ( #1900, #44858 ),
 ( #54196, #58912 ),
 ( #29487, #39858 ) ),
 .UNSPECIFIED., .F., .F., .F. ) 
 B_SPLINE_SURFACE_WITH_KNOTS ( ( 4, 4 ),
 ( 2, 2 ),
 ( 0.000000000000000000, 1.000000000000000000 ),
 ( 0.000000000000000000, 1.000000000000000000 ),
 .UNSPECIFIED. ) 
 GEOMETRIC_REPRESENTATION_ITEM ( )  RATIONAL_B_SPLINE_SURFACE ( (
 ( 1.000000000000000000, 1.000000000000000000),
 ( 0.7282232189291694135, 0.9929344683865672927),
 ( 0.7282232189291694135, 0.9929344683865672927),
 ( 1.000000000000000000, 1.000000000000000000) ) ) 
 REPRESENTATION_ITEM ( '' )  SURFACE ( )  );
#39095 = B_SPLINE_CURVE_WITH_KNOTS ( 'NONE', 3,
 ( #31227, #20600, #7394, #21211, #35023, #2705 ),
 .UNSPECIFIED., .F., .F.,
 ( 4, 2, 4 ),
 ( 1.205235924680983448E-16, 0.0002448718616795927169, 0.0004897437233590649789 ),
 .UNSPECIFIED. ) ;
#39096 = ORIENTED_EDGE ( 'NONE', *, *, #43935, .T. ) ;
#39097 = CARTESIAN_POINT ( 'NONE',  ( 3.661933894777863685, 44.83346409145190137, 14.23346979875768170 ) ) ;
#39098 = FACE_BOUND ( 'NONE', #7246, .T. ) ;
#39099 = CARTESIAN_POINT ( 'NONE',  ( 4.956653778116990594, -32.11725092155016625, -35.79382859084151391 ) ) ;
#39100 = ORIENTED_EDGE ( 'NONE', *, *, #1344, .F. ) ;
#39101 = CARTESIAN_POINT ( 'NONE',  ( 0.5806925824938499181, 42.95845041307745760, 18.80940989108190209 ) ) ;
#39102 = CARTESIAN_POINT ( 'NONE',  ( 0.5819845079324661441, 47.42480735454296337, -6.701571823032242747 ) ) ;
#39103 = ORIENTED_EDGE ( 'NONE', *, *, #55163, .T. ) ;
#39104 =( BOUNDED_SURFACE ( )  B_SPLINE_SURFACE ( 3, 1, ( 
 ( #16765, #58712 ),
 ( #11141, #35877 ),
 ( #21762, #25841 ),
 ( #25223, #7016 ) ),
 .UNSPECIFIED., .F., .F., .F. ) 
 B_SPLINE_SURFACE_WITH_KNOTS ( ( 4, 4 ),
 ( 2, 2 ),
 ( 0.000000000000000000, 1.000000000000000000 ),
 ( 0.000000000000000000, 1.000000000000000000 ),
 .UNSPECIFIED. ) 
 GEOMETRIC_REPRESENTATION_ITEM ( )  RATIONAL_B_SPLINE_SURFACE ( (
 ( 1.000000000000000000, 1.000000000000000000),
 ( 0.7282232189291693025, 0.9929344683865674037),
 ( 0.7282232189291693025, 0.9929344683865674037),
 ( 1.000000000000000000, 1.000000000000000000) ) ) 
 REPRESENTATION_ITEM ( '' )  SURFACE ( )  );
#39105 = CIRCLE ( 'NONE', #53062, 42.92674063221959813 ) ;
#39106 = EDGE_CURVE ( 'NONE', #38290, #34547, #51120, .T. ) ;
#39107 = CARTESIAN_POINT ( 'NONE',  ( 2.299652685299201416, -47.08666796816785904, -13.67945263940299405 ) ) ;
#39108 = ORIENTED_EDGE ( 'NONE', *, *, #32687, .T. ) ;
#39109 = CARTESIAN_POINT ( 'NONE',  ( 0.1073791018717578927, -37.10214135362874543, -21.98088480513651888 ) ) ;
#39110 = CARTESIAN_POINT ( 'NONE',  ( 0.5998501479064708430, 33.64490850298796687, 34.38546660123309096 ) ) ;
#39111 = ORIENTED_EDGE ( 'NONE', *, *, #50030, .T. ) ;
#39112 = CARTESIAN_POINT ( 'NONE',  ( -2.739355103387247858, 5.401627249124374863, -13.91653656670847461 ) ) ;
#39113 = CARTESIAN_POINT ( 'NONE',  ( 8.000000000000000000, 0.000000000000000000, 0.000000000000000000 ) ) ;
#39114 = CARTESIAN_POINT ( 'NONE',  ( 0.9790724872846766624, 40.40890317131761833, 11.11106450672177814 ) ) ;
#39115 = CARTESIAN_POINT ( 'NONE',  ( 1.227938101723756947, 33.52879263017899092, -26.79402671879293507 ) ) ;
#39116 = B_SPLINE_CURVE_WITH_KNOTS ( 'NONE', 3,
 ( #52674, #49451, #11566, #52987, #57663, #59147, #2127, #43316, #20956, #14796, #21263, #35693, #26260, #25645, #6819, #5049, #25963, #25340, #45097 ),
 .UNSPECIFIED., .F., .F.,
 ( 4, 3, 3, 3, 3, 3, 4 ),
 ( 1.214354834101861570E-17, 0.0002732106629380600467, 0.0004098138914053718000, 0.0005464171197651384497, 0.0006830203481512496944, 0.0008196235766963560435, 0.001011968216111135523 ),
 .UNSPECIFIED. ) ;
#39117 = ORIENTED_EDGE ( 'NONE', *, *, #53974, .T. ) ;
#39118 = CARTESIAN_POINT ( 'NONE',  ( 3.661921753702005677, -46.43414857639643856, -7.516712700321615870 ) ) ;
#39119 = CARTESIAN_POINT ( 'NONE',  ( 4.553261556744873317, -33.59363643963353496, -28.30206982864260112 ) ) ;
#39120 = ORIENTED_EDGE ( 'NONE', *, *, #3609, .T. ) ;
#39121 = CARTESIAN_POINT ( 'NONE',  ( 0.2230388203127561253, 20.89822698305265547, -37.71673103297341356 ) ) ;
#39122 = ORIENTED_EDGE ( 'NONE', *, *, #47061, .F. ) ;
#39123 = CARTESIAN_POINT ( 'NONE',  ( 5.959547316686252039, -14.51128755440551465, 14.51632612601503602 ) ) ;
#39124 = ORIENTED_EDGE ( 'NONE', *, *, #15238, .F. ) ;
#39125 = CARTESIAN_POINT ( 'NONE',  ( 4.291220156522060236, 0.5803847665930184085, 47.10681639453469671 ) ) ;
#39126 = CARTESIAN_POINT ( 'NONE',  ( 0.6021447746440204973, -30.82182302570912924, -38.23030688420319478 ) ) ;
#39127 = CARTESIAN_POINT ( 'NONE',  ( 5.917102823773431552, 19.71063251686268458, 3.997584750438410328 ) ) ;
#39128 = ORIENTED_EDGE ( 'NONE', *, *, #47930, .T. ) ;
#39129 = CARTESIAN_POINT ( 'NONE',  ( 4.691466044806103852, 29.64918311951081975, 33.30232861642443254 ) ) ;
#39130 = CARTESIAN_POINT ( 'NONE',  ( 0.5839879882012706247, -6.251648354650508388, 47.48621496524026497 ) ) ;
#39131 = CARTESIAN_POINT ( 'NONE',  ( 0.1129192098497455998, -38.68182264534154058, 21.22895156665764915 ) ) ;
#39132 = VERTEX_POINT ( 'NONE', #5472 ) ;
#39133 = B_SPLINE_CURVE_WITH_KNOTS ( 'NONE', 3,
 ( #20914, #59111, #45986, #40063 ),
 .UNSPECIFIED., .F., .F.,
 ( 4, 4 ),
 ( 4.336808689942017736E-19, 0.004041751736740999482 ),
 .UNSPECIFIED. ) ;
#39134 = ADVANCED_FACE ( 'NONE', ( #24609 ), #33583, .F. ) ;
#39135 = B_SPLINE_CURVE_WITH_KNOTS ( 'NONE', 3,
 ( #10945, #20336, #39457, #45089 ),
 .UNSPECIFIED., .F., .F.,
 ( 4, 4 ),
 ( 6.254634441385501517E-18, 0.004566006591234645501 ),
 .UNSPECIFIED. ) ;
#39136 = ORIENTED_EDGE ( 'NONE', *, *, #14108, .F. ) ;
#39137 = CARTESIAN_POINT ( 'NONE',  ( 0.5834872094924171693, 18.11905305011518763, 44.33648115256904987 ) ) ;
#39138 = CARTESIAN_POINT ( 'NONE',  ( 4.960156602257180580, 30.99165383632812976, -34.56254177294235319 ) ) ;
#39139 = B_SPLINE_CURVE_WITH_KNOTS ( 'NONE', 3,
 ( #58279, #43620, #5650, #21028 ),
 .UNSPECIFIED., .F., .F.,
 ( 4, 4 ),
 ( 0.000000000000000000, 0.004444878191957700800 ),
 .UNSPECIFIED. ) ;
#39140 = LINE ( 'NONE', #15628, #29965 ) ;
#39141 = DIRECTION ( 'NONE',  ( -1.000000000000000000, -0.000000000000000000, -0.000000000000000000 ) ) ;
#39142 = CARTESIAN_POINT ( 'NONE',  ( 4.694002226626921015, 44.00857453008718778, 11.89664403417603467 ) ) ;
#39143 = VERTEX_POINT ( 'NONE', #29604 ) ;
#39144 = EDGE_CURVE ( 'NONE', #5090, #39984, #19003, .T. ) ;
#39145 = CARTESIAN_POINT ( 'NONE',  ( 3.782542959838395280, -21.14749290209289967, -36.33209871934869994 ) ) ;
#39146 = ORIENTED_EDGE ( 'NONE', *, *, #10970, .T. ) ;
#39147 = EDGE_CURVE ( 'NONE', #39207, #44040, #48715, .T. ) ;
#39148 = CARTESIAN_POINT ( 'NONE',  ( 0.2279481005628797297, -42.86255399062842031, 10.45490088300113918 ) ) ;
#39149 = CARTESIAN_POINT ( 'NONE',  ( 0.8557997880470599172, -38.55640757422458620, 28.43566216844957140 ) ) ;
#39150 = CARTESIAN_POINT ( 'NONE',  ( 4.962356264823608143, 0.000000000000000000, 0.000000000000000000 ) ) ;
#39151 = CARTESIAN_POINT ( 'NONE',  ( 5.959828726073459926, -2.683617577144532973, 20.34941966491234311 ) ) ;
#39152 = CARTESIAN_POINT ( 'NONE',  ( 1.296416391601052487, 10.88712986132706639, 42.70571129789034615 ) ) ;
#39153 = CARTESIAN_POINT ( 'NONE',  ( 5.896782393890504181, -13.98685533979004347, -14.45316451791091161 ) ) ;
#39154 = VECTOR ( 'NONE', #38609, 1000.000000000000114 ) ;
#39155 = DIRECTION ( 'NONE',  ( 0.000000000000000000, 0.000000000000000000, -1.000000000000000000 ) ) ;
#39156 = DIRECTION ( 'NONE',  ( 0.000000000000000000, 0.000000000000000000, 1.000000000000000000 ) ) ;
#39157 = CARTESIAN_POINT ( 'NONE',  ( -6.057079549204054558, 3.081801865088773518, 19.00878029659119761 ) ) ;
#39159 = EDGE_CURVE ( 'NONE', #14082, #26555, #14540, .T. ) ;
#39158 = CARTESIAN_POINT ( 'NONE',  ( 3.238018933889920792, 11.38191749426280097, -7.061122185704434173 ) ) ;
#39160 = CARTESIAN_POINT ( 'NONE',  ( 3.407937589446174087, 11.62731850632884090, 7.243367523631064842 ) ) ;
#39161 = EDGE_CURVE ( 'NONE', #42575, #22617, #11540, .T. ) ;
#39162 = CARTESIAN_POINT ( 'NONE',  ( -6.072942160501519915, 7.807899065004430206, 17.60229742049949309 ) ) ;
#39163 = LINE ( 'NONE', #23806, #1636 ) ;
#39164 = ORIENTED_EDGE ( 'NONE', *, *, #39057, .T. ) ;
#39165 = DIRECTION ( 'NONE',  ( -0.07500201931887527651, 0.8647811570515492319, 0.4965161100172628683 ) ) ;
#39166 = FACE_OUTER_BOUND ( 'NONE', #27379, .T. ) ;
#39167 = CARTESIAN_POINT ( 'NONE',  ( 4.975801465491695552, -2.564218696447830403, 47.84403947906839250 ) ) ;
#39168 = B_SPLINE_CURVE_WITH_KNOTS ( 'NONE', 3,
 ( #48148, #5200, #43464, #42235 ),
 .UNSPECIFIED., .F., .F.,
 ( 4, 4 ),
 ( 4.336808689942017736E-19, 0.005014147105413693448 ),
 .UNSPECIFIED. ) ;
#39169 = CARTESIAN_POINT ( 'NONE',  ( 5.917102823773431552, 12.97825203069038835, 15.36407147469780554 ) ) ;
#39170 = CARTESIAN_POINT ( 'NONE',  ( 3.783198216974388739, 39.06945274417391545, 18.05208553945161043 ) ) ;
#39171 = ORIENTED_EDGE ( 'NONE', *, *, #21933, .T. ) ;
#39172 = CARTESIAN_POINT ( 'NONE',  ( 0.5997462898726536595, 37.72933316221968170, 31.43324751403423534 ) ) ;
#39173 = CARTESIAN_POINT ( 'NONE',  ( 0.6024113833632038784, 28.27346982169563816, -40.15162230025745771 ) ) ;
#39174 = CARTESIAN_POINT ( 'NONE',  ( 5.917102823773431552, 10.82912387347634464, -16.94756012482760354 ) ) ;
#39175 = ORIENTED_EDGE ( 'NONE', *, *, #60177, .F. ) ;
#39176 = DIRECTION ( 'NONE',  ( 0.1011922191286468153, -0.9589869809184693450, 0.2647717983787155616 ) ) ;
#39177 = EDGE_CURVE ( 'NONE', #35968, #4749, #3957, .T. ) ;
#39178 = CARTESIAN_POINT ( 'NONE',  ( 4.956445790444026223, 7.299064093731650438, -46.52162629890785439 ) ) ;
#39179 = ORIENTED_EDGE ( 'NONE', *, *, #9250, .T. ) ;
#39180 = B_SPLINE_CURVE_WITH_KNOTS ( 'NONE', 3,
 ( #61265, #41277, #22457, #8043 ),
 .UNSPECIFIED., .F., .F.,
 ( 4, 4 ),
 ( 0.000000000000000000, 0.004444103432399269631 ),
 .UNSPECIFIED. ) ;
#39181 = ADVANCED_FACE ( 'NONE', ( #23988 ), #8749, .T. ) ;
#39182 = CARTESIAN_POINT ( 'NONE',  ( 4.956653778116959508, -15.97476558431919180, 45.35992544608522792 ) ) ;
#39183 = ORIENTED_EDGE ( 'NONE', *, *, #60668, .F. ) ;
#39184 = CARTESIAN_POINT ( 'NONE',  ( 2.299746137290199055, -38.51195501985936431, 30.34980491262615843 ) ) ;
#39185 = ORIENTED_EDGE ( 'NONE', *, *, #25953, .T. ) ;
#39186 = LINE ( 'NONE', #48551, #9731 ) ;
#39187 = CARTESIAN_POINT ( 'NONE',  ( 0.7246131072078566548, -28.62741613354265624, -38.65593150731038463 ) ) ;
#39188 = VERTEX_POINT ( 'NONE', #792 ) ;
#39189 = CARTESIAN_POINT ( 'NONE',  ( 4.967162193818131399, -38.83676580803778933, 18.65818244221244981 ) ) ;
#39190 = VECTOR ( 'NONE', #51555, 1000.000000000000114 ) ;
#39191 = VERTEX_POINT ( 'NONE', #34024 ) ;
#39192 = CARTESIAN_POINT ( 'NONE',  ( 5.895596859100789899, 16.58392706178506160, 11.37987462241481929 ) ) ;
#39193 = CARTESIAN_POINT ( 'NONE',  ( 0.1129192098497447394, -0.9297496242502409913, 44.11448008785053077 ) ) ;
#39194 = VECTOR ( 'NONE', #28051, 1000.000000000000000 ) ;
#39195 = CARTESIAN_POINT ( 'NONE',  ( 0.6025881611877910160, -38.29866377863859128, 29.11258673756348614 ) ) ;
#39196 = EDGE_LOOP ( 'NONE', ( #11860, #47279, #26134, #33574 ) ) ;
#39197 = DIRECTION ( 'NONE',  ( 1.000000000000000000, 0.000000000000000000, 0.000000000000000000 ) ) ;
#39198 = CARTESIAN_POINT ( 'NONE',  ( -4.908599999999999852, 0.000000000000000000, -3.000000000000000000 ) ) ;
#39199 = CARTESIAN_POINT ( 'NONE',  ( -6.072942160501519915, 13.84283391500573224, 13.38581755032494414 ) ) ;
#39200 = LINE ( 'NONE', #26003, #18697 ) ;
#39201 = ORIENTED_EDGE ( 'NONE', *, *, #50453, .T. ) ;
#39202 = CARTESIAN_POINT ( 'NONE',  ( 0.5980271706414734822, 27.52111707190191225, -40.67723390247095239 ) ) ;
#39203 = CARTESIAN_POINT ( 'NONE',  ( -6.078457390727109555, -1.844660340668231147, 19.16746564533437791 ) ) ;
#39204 = B_SPLINE_CURVE_WITH_KNOTS ( 'NONE', 3,
 ( #58692, #44345, #60471, #10495, #39637, #3159 ),
 .UNSPECIFIED., .F., .F.,
 ( 4, 2, 4 ),
 ( 4.553649124439118623E-18, 0.0002447193893791687323, 0.0004894387787583329109 ),
 .UNSPECIFIED. ) ;
#39205 = VERTEX_POINT ( 'NONE', #4542 ) ;
#39206 = CARTESIAN_POINT ( 'NONE',  ( 0.5835226383429314989, -46.80316998458874167, -2.950551463651092998 ) ) ;
#39207 = VERTEX_POINT ( 'NONE', #29298 ) ;
#39208 = B_SPLINE_CURVE_WITH_KNOTS ( 'NONE', 3,
 ( #37106, #36792, #41491, #26433 ),
 .UNSPECIFIED., .F., .F.,
 ( 4, 4 ),
 ( 2.023134036479838731E-17, 0.004444306975806115896 ),
 .UNSPECIFIED. ) ;
#39209 = CARTESIAN_POINT ( 'NONE',  ( 1.227938101723748288, -34.55893248994524214, 25.45152231597044690 ) ) ;
#39210 =( BOUNDED_SURFACE ( )  B_SPLINE_SURFACE ( 3, 1, ( 
 ( #10498, #34313 ),
 ( #58697, #53390 ),
 ( #2306, #30823 ),
 ( #15821, #39642 ) ),
 .UNSPECIFIED., .F., .F., .F. ) 
 B_SPLINE_SURFACE_WITH_KNOTS ( ( 4, 4 ),
 ( 2, 2 ),
 ( 0.000000000000000000, 1.000000000000000000 ),
 ( 0.000000000000000000, 1.000000000000000000 ),
 .UNSPECIFIED. ) 
 GEOMETRIC_REPRESENTATION_ITEM ( )  RATIONAL_B_SPLINE_SURFACE ( (
 ( 1.000000000000000000, 1.000000000000000000),
 ( 0.9754377213608244057, 0.9999580625633939235),
 ( 0.9754377213608244057, 0.9999580625633939235),
 ( 1.000000000000000000, 1.000000000000000000) ) ) 
 REPRESENTATION_ITEM ( '' )  SURFACE ( )  );
#39211 = CARTESIAN_POINT ( 'NONE',  ( 0.9790320750461911636, 40.44225345157877882, -10.98914320138077905 ) ) ;
#39212 = VERTEX_POINT ( 'NONE', #48110 ) ;
#39213 = CARTESIAN_POINT ( 'NONE',  ( 0.08486401232817714080, 0.000000000000000000, 10.00000000000000000 ) ) ;
#39214 = CARTESIAN_POINT ( 'NONE',  ( 0.7954190325252769034, 37.62416463577109482, -29.96539637359175501 ) ) ;
#39215 = CARTESIAN_POINT ( 'NONE',  ( 4.963659409799330291, -25.25989740981525244, 36.94443854030213004 ) ) ;
#39216 = FACE_OUTER_BOUND ( 'NONE', #20146, .T. ) ;
#39217 = EDGE_CURVE ( 'NONE', #50690, #21453, #10755, .T. ) ;
#39218 = ORIENTED_EDGE ( 'NONE', *, *, #29785, .F. ) ;
#39219 = CARTESIAN_POINT ( 'NONE',  ( 0.1154773475650540809, -40.83160922148467620, 16.72493104410563447 ) ) ;
#39220 = EDGE_CURVE ( 'NONE', #39984, #22663, #30147, .T. ) ;
#39221 = B_SPLINE_CURVE_WITH_KNOTS ( 'NONE', 3,
 ( #19254, #47752, #28628, #28327 ),
 .UNSPECIFIED., .F., .F.,
 ( 4, 4 ),
 ( 0.000000000000000000, 0.005013413432710149380 ),
 .UNSPECIFIED. ) ;
#39222 = CARTESIAN_POINT ( 'NONE',  ( 0.9790724872846782167, 41.54009254446635424, -5.545802140234084021 ) ) ;
#39223 = CARTESIAN_POINT ( 'NONE',  ( 3.270143674763207553, 12.53844339339242531, -5.490410281242639634 ) ) ;
#39224 = CARTESIAN_POINT ( 'NONE',  ( 4.291220156522059348, -42.97446925027733755, 19.30243481954189022 ) ) ;
#39225 = CARTESIAN_POINT ( 'NONE',  ( 1.296416391601052265, -8.128596768097615666, -43.31550863902941018 ) ) ;
#39226 = CARTESIAN_POINT ( 'NONE',  ( 4.967162193818130511, 0.000000000000000000, 0.000000000000000000 ) ) ;
#39227 = B_SPLINE_CURVE_WITH_KNOTS ( 'NONE', 3,
 ( #29206, #19833, #58941, #39254, #15747, #11345 ),
 .UNSPECIFIED., .F., .F.,
 ( 4, 2, 4 ),
 ( 9.828040028768063295E-18, 0.0002291966416970815722, 0.0004583932833941532781 ),
 .UNSPECIFIED. ) ;
#39228 = CARTESIAN_POINT ( 'NONE',  ( -17.29528526743291295, -7.748184832854354553, -1.992127074845276402 ) ) ;
#39229 = LINE ( 'NONE', #25404, #49390 ) ;
#39230 = CARTESIAN_POINT ( 'NONE',  ( -6.016761891674565099, 9.424569481870481269, -16.31696541414262214 ) ) ;
#39231 = EDGE_CURVE ( 'NONE', #46648, #59248, #56335, .T. ) ;
#39232 = LINE ( 'NONE', #14487, #22129 ) ;
#39233 = CARTESIAN_POINT ( 'NONE',  ( 4.833616638992208614, -41.27831852777658384, 20.86133030530218235 ) ) ;
#39234 = VECTOR ( 'NONE', #12641, 1000.000000000000000 ) ;
#39235 = DIRECTION ( 'NONE',  ( -0.07836865515943411409, 0.1379401902675563285, 0.9873352307081176837 ) ) ;
#39236 = VECTOR ( 'NONE', #60942, 1000.000000000000114 ) ;
#39237 = CARTESIAN_POINT ( 'NONE',  ( 3.783278058412225864, 29.18720354295088981, -31.62921638229637722 ) ) ;
#39238 = CARTESIAN_POINT ( 'NONE',  ( 4.962356264823601926, -42.08379584346671720, 0.4355746408606013254 ) ) ;
#39239 = VERTEX_POINT ( 'NONE', #54312 ) ;
#39240 = CARTESIAN_POINT ( 'NONE',  ( 4.975610109902397937, -43.81605102859474954, 21.73943604138237973 ) ) ;
#39241 = CARTESIAN_POINT ( 'NONE',  ( 0.9769922540276050338, -1.841908291151032273, 41.86811351055972352 ) ) ;
#39242 = CARTESIAN_POINT ( 'NONE',  ( 0.6001305935487315502, -24.50730504006486754, 41.40054608060250985 ) ) ;
#39243 = ORIENTED_EDGE ( 'NONE', *, *, #28910, .T. ) ;
#39244 = DIRECTION ( 'NONE',  ( -0.1024043820194934645, 0.1428674944016148363, -0.9844298967354710994 ) ) ;
#39245 = CARTESIAN_POINT ( 'NONE',  ( 3.050102900204245682, 26.63270562985675127, 35.01605688839702424 ) ) ;
#39246 = ORIENTED_EDGE ( 'NONE', *, *, #28989, .F. ) ;
#39247 = ORIENTED_EDGE ( 'NONE', *, *, #31122, .F. ) ;
#39248 = B_SPLINE_CURVE_WITH_KNOTS ( 'NONE', 3,
 ( #8434, #27560, #51972, #23173 ),
 .UNSPECIFIED., .F., .F.,
 ( 4, 4 ),
 ( 6.254634441385501517E-18, 0.004566006591234646368 ),
 .UNSPECIFIED. ) ;
#39249 = FACE_OUTER_BOUND ( 'NONE', #53106, .T. ) ;
#39250 = VERTEX_POINT ( 'NONE', #20526 ) ;
#39251 = CARTESIAN_POINT ( 'NONE',  ( 0.9722240750034568668, 25.65687433776948012, -34.39263040572760843 ) ) ;
#39252 = ORIENTED_EDGE ( 'NONE', *, *, #61563, .F. ) ;
#39253 = ORIENTED_EDGE ( 'NONE', *, *, #27751, .F. ) ;
#39254 = CARTESIAN_POINT ( 'NONE',  ( 1.088313998177382169, 25.50107284445311606, 34.51470853099723968 ) ) ;
#39255 = ORIENTED_EDGE ( 'NONE', *, *, #10222, .T. ) ;
#39256 = CARTESIAN_POINT ( 'NONE',  ( 0.6009453534118438522, -29.63106322864213737, 37.89911869481681350 ) ) ;
#39257 = LINE ( 'NONE', #53610, #42105 ) ;
#39258 = ADVANCED_FACE ( 'NONE', ( #31147 ), #35607, .F. ) ;
#39259 = VERTEX_POINT ( 'NONE', #30516 ) ;
#39260 = CARTESIAN_POINT ( 'NONE',  ( 2.282803330402960906, 36.03600629612929396, 30.13143139119534197 ) ) ;
#39261 = CARTESIAN_POINT ( 'NONE',  ( 0.6001305935487315502, -5.760103278698373686, 47.76436356026957952 ) ) ;
#39262 = ORIENTED_EDGE ( 'NONE', *, *, #37511, .T. ) ;
#39263 = EDGE_CURVE ( 'NONE', #4666, #3997, #61545, .T. ) ;
#39264 = VERTEX_POINT ( 'NONE', #59334 ) ;
#39265 = CARTESIAN_POINT ( 'NONE',  ( 0.6023142530420679819, -18.16775455049974042, 44.54505940664454755 ) ) ;
#39266 = CARTESIAN_POINT ( 'NONE',  ( 1.091591847532195070, -37.05036493332335823, -19.59666934107434244 ) ) ;
#39267 = CARTESIAN_POINT ( 'NONE',  ( 0.1092355843206037486, -30.70542469027345334, 30.28032287551026158 ) ) ;
#39268 = CARTESIAN_POINT ( 'NONE',  ( 5.965394784446458765, -16.29267539192334624, -12.48356622107671221 ) ) ;
#39269 = ORIENTED_EDGE ( 'NONE', *, *, #55010, .T. ) ;
#39270 = CARTESIAN_POINT ( 'NONE',  ( 0.1140933569871964842, -1.035112909008395476, -44.11211275091581285 ) ) ;
#39271 = CARTESIAN_POINT ( 'NONE',  ( 2.299652685299200972, -47.74024202747411039, 11.18709149047902507 ) ) ;
#39272 =( BOUNDED_SURFACE ( )  B_SPLINE_SURFACE ( 3, 1, ( 
 ( #61512, #33973 ),
 ( #29863, #44007 ),
 ( #38986, #25164 ),
 ( #54260, #48061 ) ),
 .UNSPECIFIED., .F., .F., .F. ) 
 B_SPLINE_SURFACE_WITH_KNOTS ( ( 4, 4 ),
 ( 2, 2 ),
 ( 0.000000000000000000, 1.000000000000000000 ),
 ( 0.000000000000000000, 1.000000000000000000 ),
 .UNSPECIFIED. ) 
 GEOMETRIC_REPRESENTATION_ITEM ( )  RATIONAL_B_SPLINE_SURFACE ( (
 ( 1.000000000000000000, 1.000000000000000000),
 ( 0.9754377213608244057, 0.9999580625633939235),
 ( 0.9754377213608244057, 0.9999580625633939235),
 ( 1.000000000000000000, 1.000000000000000000) ) ) 
 REPRESENTATION_ITEM ( '' )  SURFACE ( )  );
#39273 = VECTOR ( 'NONE', #9813, 1000.000000000000114 ) ;
#39274 = DIRECTION ( 'NONE',  ( 1.000000000000000000, 0.000000000000000000, 0.000000000000000000 ) ) ;
#39275 = CARTESIAN_POINT ( 'NONE',  ( -6.079354080745853928, 9.981161348512202380, 16.46722117975975408 ) ) ;
#39276 = ORIENTED_EDGE ( 'NONE', *, *, #3713, .F. ) ;
#39277 = CARTESIAN_POINT ( 'NONE',  ( 0.5807400328401637335, -34.25275203086212628, -33.48217046439146571 ) ) ;
#39278 = CARTESIAN_POINT ( 'NONE',  ( 0.6027444965799114707, -13.84715149815399649, -47.11469952440122455 ) ) ;
#39279 = DIRECTION ( 'NONE',  ( 0.09835009131224554946, -0.6981896185982771064, 0.7091251765523951534 ) ) ;
#39280 = CARTESIAN_POINT ( 'NONE',  ( 4.975610109902397937, -28.45381238669758872, -39.78479568629688856 ) ) ;
#39281 = EDGE_CURVE ( 'NONE', #44200, #45745, #54748, .T. ) ;
#39282 = VERTEX_POINT ( 'NONE', #30836 ) ;
#39283 = ORIENTED_EDGE ( 'NONE', *, *, #41663, .T. ) ;
#39284 = DIRECTION ( 'NONE',  ( 1.000000000000000000, -0.000000000000000000, -0.000000000000000000 ) ) ;
#39285 = DIRECTION ( 'NONE',  ( 0.000000000000000000, 0.000000000000000000, -1.000000000000000000 ) ) ;
#39286 = ADVANCED_FACE ( 'NONE', ( #44657 ), #11627, .F. ) ;
#39287 = CARTESIAN_POINT ( 'NONE',  ( 4.553261556744873317, -41.75933753256789771, -13.62707946203816967 ) ) ;
#39288 = CARTESIAN_POINT ( 'NONE',  ( 4.960386119450145515, 6.813122688534734905, -43.22057176742709572 ) ) ;
#39289 = DIRECTION ( 'NONE',  ( 0.000000000000000000, 0.000000000000000000, 1.000000000000000000 ) ) ;
#39290 = EDGE_CURVE ( 'NONE', #9871, #19218, #30740, .T. ) ;
#39291 = CARTESIAN_POINT ( 'NONE',  ( 0.3622758884714600280, -43.10531414739104861, -0.8252992914326565677 ) ) ;
#39292 = DIRECTION ( 'NONE',  ( -0.07439287786467650709, -0.8569499480575021311, 0.5100024374914848835 ) ) ;
#39293 = CARTESIAN_POINT ( 'NONE',  ( 0.6028618097248862329, -18.57111736963418736, -44.37846879336927941 ) ) ;
#39294 = CARTESIAN_POINT ( 'NONE',  ( 0.5807400328401574052, 34.25275203086236075, 33.48217046439123834 ) ) ;
#39295 = VERTEX_POINT ( 'NONE', #21756 ) ;
#39296 = CARTESIAN_POINT ( 'NONE',  ( 0.1158403557922069033, -7.004826579936690223, -43.56458093186288494 ) ) ;
#39297 = CARTESIAN_POINT ( 'NONE',  ( 0.7056555295713283771, -41.05687446835452903, 24.67549844185522545 ) ) ;
#39298 = CARTESIAN_POINT ( 'NONE',  ( -6.077587904424778920, -8.901182807328959612, 17.07527352707539592 ) ) ;
#39299 = FACE_OUTER_BOUND ( 'NONE', #30923, .T. ) ;
#39300 = ADVANCED_FACE ( 'NONE', ( #7318, #26447 ), #17070, .F. ) ;
#39301 = CARTESIAN_POINT ( 'NONE',  ( 0.6030672727741701600, -24.12926094634015328, 41.61859040196942061 ) ) ;
#39302 = CARTESIAN_POINT ( 'NONE',  ( 0.5809828226811617480, -41.74875432577665890, 23.47450554821694979 ) ) ;
#39303 = CARTESIAN_POINT ( 'NONE',  ( 0.7764139734771241530, 45.46540455849966378, -11.52985078996363910 ) ) ;
#39304 = CARTESIAN_POINT ( 'NONE',  ( 0.5807400328401637335, 37.66660715020866235, 29.58941477093028993 ) ) ;
#39305 = CARTESIAN_POINT ( 'NONE',  ( 0.6252788684277205133, 23.32025617012770624, 43.21585337967175633 ) ) ;
#39306 = CARTESIAN_POINT ( 'NONE',  ( 4.553261556744873317, 27.56395660609696563, 34.20186927699770507 ) ) ;
#39308 = ORIENTED_EDGE ( 'NONE', *, *, #56953, .F. ) ;
#39307 = CARTESIAN_POINT ( 'NONE',  ( 0.000000000000000000, 0.000000000000000000, 0.000000000000000000 ) ) ;
#39309 = ORIENTED_EDGE ( 'NONE', *, *, #36413, .T. ) ;
#39310 = CARTESIAN_POINT ( 'NONE',  ( 4.694002226626920127, -44.68037479411238877, 9.052562051915485242 ) ) ;
#39311 = CARTESIAN_POINT ( 'NONE',  ( 0.1129192098497447394, -43.82135468580274562, -5.161459220630158384 ) ) ;
#39312 = CARTESIAN_POINT ( 'NONE',  ( 0.1154773475650540809, 41.93263902776148200, 13.73307737594076094 ) ) ;
#39313 = EDGE_LOOP ( 'NONE', ( #40191, #10890 ) ) ;
#39314 = EDGE_LOOP ( 'NONE', ( #51469, #211, #28519, #37315 ) ) ;
#39315 = CARTESIAN_POINT ( 'NONE',  ( 0.1084644655670283231, -10.77688306151832798, 41.75632203164214218 ) ) ;
#39316 = DIRECTION ( 'NONE',  ( -1.836970198721033632E-16, 1.000000000000000000, 0.000000000000000000 ) ) ;
#39317 = CARTESIAN_POINT ( 'NONE',  ( 5.960721111146673579, 5.306302591836305815, 19.82781442290499996 ) ) ;
#39318 = AXIS2_PLACEMENT_3D ( 'NONE', #594, #49151, #57593 ) ;
#39319 = ORIENTED_EDGE ( 'NONE', *, *, #13321, .F. ) ;
#39320 = ORIENTED_EDGE ( 'NONE', *, *, #2749, .T. ) ;
#39321 = CARTESIAN_POINT ( 'NONE',  ( 0.6028618097248863439, -24.20479143424861945, -41.57478760529395601 ) ) ;
#39322 = ADVANCED_FACE ( 'NONE', ( #10825 ), #22410, .F. ) ;
#39323 = CARTESIAN_POINT ( 'NONE',  ( -6.078075953587585900, -17.35139778253833498, -8.350099953848438616 ) ) ;
#39324 = CARTESIAN_POINT ( 'NONE',  ( 0.5988103564986360094, -46.30780741915676657, 13.03604522143276512 ) ) ;
#39325 = CARTESIAN_POINT ( 'NONE',  ( 4.967162193818130511, 42.34252806656603241, -7.970725651239366272 ) ) ;
#39326 = EDGE_CURVE ( 'NONE', #26558, #1848, #5511, .T. ) ;
#39327 = CARTESIAN_POINT ( 'NONE',  ( 2.281448460670572942, 4.956513608981858887, -47.71650330356582259 ) ) ;
#39328 = EDGE_CURVE ( 'NONE', #5134, #38412, #2525, .T. ) ;
#39329 = DIRECTION ( 'NONE',  ( 0.1011922191286468153, -0.8049255303601264844, -0.5846836968500909171 ) ) ;
#39330 = CIRCLE ( 'NONE', #53290, 47.91270532121795611 ) ;
#39331 = CARTESIAN_POINT ( 'NONE',  ( 0.1152809850208375148, 15.44635349940774027, -41.33225672596513078 ) ) ;
#39332 = VERTEX_POINT ( 'NONE', #3244 ) ;
#39333 = ADVANCED_FACE ( 'NONE', ( #18609 ), #20765, .F. ) ;
#39334 = EDGE_CURVE ( 'NONE', #13574, #22672, #12990, .T. ) ;
#39335 = ORIENTED_EDGE ( 'NONE', *, *, #34595, .T. ) ;
#39336 = CARTESIAN_POINT ( 'NONE',  ( 1.084202172485504434E-14, 4.618802153517020059, -0.3572655899081733644 ) ) ;
#39337 = CARTESIAN_POINT ( 'NONE',  ( -16.98648177666931858, 7.159091074317976755, -1.550344604434408250E-15 ) ) ;
#39338 = B_SPLINE_CURVE_WITH_KNOTS ( 'NONE', 3,
 ( #51502, #38373, #27400, #3575, #22707, #60907, #8591, #27718, #46847, #3888, #42158, #18334, #61515, #37765, #56822, #13951, #15473, #34582, #24870 ),
 .UNSPECIFIED., .F., .F.,
 ( 4, 3, 3, 3, 3, 3, 4 ),
 ( 9.107943584450270299E-18, 0.0002732106629380616730, 0.0004098138914053771668, 0.0005464171197651476655, 0.0006830203481512577175, 0.0008196235766963648256, 0.001011968216111140727 ),
 .UNSPECIFIED. ) ;
#39339 = VERTEX_POINT ( 'NONE', #46500 ) ;
#39340 = CARTESIAN_POINT ( 'NONE',  ( 3.783278058412225864, 20.00643011788508119, -38.10568111914483325 ) ) ;
#39341 = CARTESIAN_POINT ( 'NONE',  ( 0.8751705887134553219, 44.76769609654211735, 17.57879340691559378 ) ) ;
#39342 = CARTESIAN_POINT ( 'NONE',  ( -6.016104459813371719, 9.426230926598641702, 16.31603998697573132 ) ) ;
#39343 = DIRECTION ( 'NONE',  ( 0.07906939808003032866, -0.2389416749771389459, 0.9678093336222693965 ) ) ;
#39344 = ORIENTED_EDGE ( 'NONE', *, *, #3485, .F. ) ;
#39345 = CARTESIAN_POINT ( 'NONE',  ( 4.975610109902397937, 48.58133226360784818, -5.683622315980244366 ) ) ;
#39346 = DIRECTION ( 'NONE',  ( 0.000000000000000000, 0.000000000000000000, 1.000000000000000000 ) ) ;
#39347 = CARTESIAN_POINT ( 'NONE',  ( 4.960386119450149955, 39.26151414358990621, -19.31243050019935126 ) ) ;
#39348 = CARTESIAN_POINT ( 'NONE',  ( -2.708315649062916552, 12.80362818457435914, 7.087851317224007630 ) ) ;
#39349 = ORIENTED_EDGE ( 'NONE', *, *, #34467, .T. ) ;
#39350 = CARTESIAN_POINT ( 'NONE',  ( 5.958863334805807099, -10.26388325355099695, 17.77512673691301259 ) ) ;
#39351 = CARTESIAN_POINT ( 'NONE',  ( 3.727782113643637540, -29.04977724543226358, -32.99830628830427770 ) ) ;
#39352 = ORIENTED_EDGE ( 'NONE', *, *, #35466, .T. ) ;
#39353 = CARTESIAN_POINT ( 'NONE',  ( 0.8560838555295158248, -2.480523550131575661, 46.84250032821661591 ) ) ;
#39354 = CARTESIAN_POINT ( 'NONE',  ( 0.5839879327111923146, 23.86931774877355750, -41.52454255611482381 ) ) ;
#39355 = EDGE_CURVE ( 'NONE', #48936, #18068, #24963, .T. ) ;
#39356 =( BOUNDED_SURFACE ( )  B_SPLINE_SURFACE ( 3, 1, ( 
 ( #11880, #7122 ),
 ( #60363, #41013 ),
 ( #12483, #3352 ),
 ( #54428, #50066 ) ),
 .UNSPECIFIED., .F., .F., .F. ) 
 B_SPLINE_SURFACE_WITH_KNOTS ( ( 4, 4 ),
 ( 2, 2 ),
 ( 0.000000000000000000, 1.000000000000000000 ),
 ( 0.000000000000000000, 1.000000000000000000 ),
 .UNSPECIFIED. ) 
 GEOMETRIC_REPRESENTATION_ITEM ( )  RATIONAL_B_SPLINE_SURFACE ( (
 ( 1.000000000000000000, 1.000000000000000000),
 ( 0.7211978278499968642, 0.9934217856018975334),
 ( 0.7211978278499968642, 0.9934217856018975334),
 ( 1.000000000000000000, 1.000000000000000000) ) ) 
 REPRESENTATION_ITEM ( '' )  SURFACE ( )  );
#39357 = ORIENTED_EDGE ( 'NONE', *, *, #54222, .F. ) ;
#39358 = CARTESIAN_POINT ( 'NONE',  ( 0.1064266418746774578, 39.62374465289870074, 17.02047513535245926 ) ) ;
#39359 = ADVANCED_FACE ( 'NONE', ( #4166 ), #48026, .F. ) ;
#39360 = DIRECTION ( 'NONE',  ( 0.07906939808003035641, 0.9443293062557466255, -0.3193590324913357370 ) ) ;
#39361 = CARTESIAN_POINT ( 'NONE',  ( 4.694002226626920127, 12.64038892846120810, -43.80074587473789904 ) ) ;
#39362 = VECTOR ( 'NONE', #14662, 1000.000000000000114 ) ;
#39363 = ADVANCED_FACE ( 'NONE', ( #61486 ), #59163, .F. ) ;
#39364 = CARTESIAN_POINT ( 'NONE',  ( 2.643462169533613793, -48.01657676222236404, 1.382267876918295890 ) ) ;
#39365 = CARTESIAN_POINT ( 'NONE',  ( 0.8560838555295223751, -18.91252766612315739, 42.92655508376904550 ) ) ;
#39366 = CARTESIAN_POINT ( 'NONE',  ( 0.8557997880470690211, 5.347802024197924275, -47.60865952216993691 ) ) ;
#39367 = CARTESIAN_POINT ( 'NONE',  ( 4.000000000000003553, -1.933795701539622103, -0.2488376576623028413 ) ) ;
#39368 = CARTESIAN_POINT ( 'NONE',  ( 1.088313998177377950, 34.51470853099749547, -25.50107284445278921 ) ) ;
#39369 = ORIENTED_EDGE ( 'NONE', *, *, #14589, .T. ) ;
#39370 = CARTESIAN_POINT ( 'NONE',  ( 0.9756950546413922787, 39.60512406639371363, -16.50968749804397717 ) ) ;
#39371 = CARTESIAN_POINT ( 'NONE',  ( 0.9791128995231621612, 41.53542872017264642, 5.580823888783615239 ) ) ;
#39372 =( BOUNDED_SURFACE ( )  B_SPLINE_SURFACE ( 3, 1, ( 
 ( #4167, #42429 ),
 ( #56797, #33030 ),
 ( #5929, #15379 ),
 ( #58559, #34482 ) ),
 .UNSPECIFIED., .F., .F., .F. ) 
 B_SPLINE_SURFACE_WITH_KNOTS ( ( 4, 4 ),
 ( 2, 2 ),
 ( 0.000000000000000000, 1.000000000000000000 ),
 ( 0.000000000000000000, 1.000000000000000000 ),
 .UNSPECIFIED. ) 
 GEOMETRIC_REPRESENTATION_ITEM ( )  RATIONAL_B_SPLINE_SURFACE ( (
 ( 1.000000000000000000, 1.000000000000000000),
 ( 0.9729067724841187204, 0.9999501103223794596),
 ( 0.9729067724841187204, 0.9999501103223794596),
 ( 1.000000000000000000, 1.000000000000000000) ) ) 
 REPRESENTATION_ITEM ( '' )  SURFACE ( )  );
#39373 = CARTESIAN_POINT ( 'NONE',  ( 0.5837800005270556980, 27.81773451563321231, -37.75458786769539898 ) ) ;
#39374 = ORIENTED_EDGE ( 'NONE', *, *, #22012, .T. ) ;
#39376 = FACE_OUTER_BOUND ( 'NONE', #38570, .T. ) ;
#39375 =( BOUNDED_SURFACE ( )  B_SPLINE_SURFACE ( 3, 1, ( 
 ( #17446, #51248 ),
 ( #51870, #37496 ),
 ( #13685, #18687 ),
 ( #12768, #28077 ) ),
 .UNSPECIFIED., .F., .F., .F. ) 
 B_SPLINE_SURFACE_WITH_KNOTS ( ( 4, 4 ),
 ( 2, 2 ),
 ( 0.000000000000000000, 1.000000000000000000 ),
 ( 0.000000000000000000, 1.000000000000000000 ),
 .UNSPECIFIED. ) 
 GEOMETRIC_REPRESENTATION_ITEM ( )  RATIONAL_B_SPLINE_SURFACE ( (
 ( 1.000000000000000000, 1.000000000000000000),
 ( 0.9953485035131437453, 0.8621029689291523912),
 ( 0.9953485035131437453, 0.8621029689291523912),
 ( 1.000000000000000000, 1.000000000000000000) ) ) 
 REPRESENTATION_ITEM ( '' )  SURFACE ( )  );
#39377 = CARTESIAN_POINT ( 'NONE',  ( -6.001507490154111224, 4.892199142591558747, -18.19774963328903539 ) ) ;
#39378 = CARTESIAN_POINT ( 'NONE',  ( 0.6016117650947688800, 23.02239457412811063, 43.37649596633706750 ) ) ;
#39379 = CARTESIAN_POINT ( 'NONE',  ( 4.694002226626920127, 28.15356303305734187, -35.85612444185512970 ) ) ;
#39380 = EDGE_CURVE ( 'NONE', #29507, #13900, #735, .T. ) ;
#39381 = VECTOR ( 'NONE', #56225, 1000.000000000000114 ) ;
#39382 = CARTESIAN_POINT ( 'NONE',  ( 5.896782393890504181, -13.97772289704291460, 14.46199673252260354 ) ) ;
#39383 = CARTESIAN_POINT ( 'NONE',  ( 0.6028618097248863439, 38.05975027458337223, -29.42431480658691356 ) ) ;
#39384 = DIRECTION ( 'NONE',  ( -1.829550196521986996E-16, 0.9999920064717846557, -0.003998373736173961579 ) ) ;
#39385 = LINE ( 'NONE', #58745, #24892 ) ;
#39386 = EDGE_CURVE ( 'NONE', #16923, #26391, #15198, .T. ) ;
#39387 = DIRECTION ( 'NONE',  ( 0.07439287786467665975, -0.7830499462674513911, -0.6174937095821728672 ) ) ;
#39388 = CARTESIAN_POINT ( 'NONE',  ( 0.9790850452238870627, 29.09817565893450819, -30.16013102731797346 ) ) ;
#39390 = ORIENTED_EDGE ( 'NONE', *, *, #11045, .F. ) ;
#39389 = DIRECTION ( 'NONE',  ( 0.09722883295013595717, -0.2759265041300154597, 0.9562484605800645188 ) ) ;
#39391 = ORIENTED_EDGE ( 'NONE', *, *, #15553, .F. ) ;
#39392 = CARTESIAN_POINT ( 'NONE',  ( 45.00000000000001421, 1.592040838891559293E-15, -13.00000000000000178 ) ) ;
#39393 = CARTESIAN_POINT ( 'NONE',  ( 5.974727161628369032, 20.34732802718243860, 2.694421823322989074 ) ) ;
#39394 = CARTESIAN_POINT ( 'NONE',  ( 5.895596859100789899, -9.669028665050335647, 17.63627137143570067 ) ) ;
#39395 = FACE_OUTER_BOUND ( 'NONE', #59178, .T. ) ;
#39396 = CARTESIAN_POINT ( 'NONE',  ( 1.091591847532195958, -41.22213727214368362, 7.582505500979439539 ) ) ;
#39397 = VERTEX_POINT ( 'NONE', #57706 ) ;
#39398 = ORIENTED_EDGE ( 'NONE', *, *, #42443, .T. ) ;
#39399 = CARTESIAN_POINT ( 'NONE',  ( 5.895596859100789899, 5.955534046174260965, 19.21092911436994299 ) ) ;
#39400 = CARTESIAN_POINT ( 'NONE',  ( 4.694002226626921015, 28.69237940071596071, -35.42643272715312719 ) ) ;
#39401 = CARTESIAN_POINT ( 'NONE',  ( 0.6028777368367060907, 37.33615699143113886, 31.89907851995540966 ) ) ;
#39402 = ORIENTED_EDGE ( 'NONE', *, *, #36796, .F. ) ;
#39403 = ADVANCED_FACE ( 'NONE', ( #44825 ), #32779, .F. ) ;
#39404 = CIRCLE ( 'NONE', #17348, 6.728125000000023448 ) ;
#39405 = EDGE_CURVE ( 'NONE', #20457, #22596, #13788, .T. ) ;
#39406 = FACE_OUTER_BOUND ( 'NONE', #4702, .T. ) ;
#39407 = DIRECTION ( 'NONE',  ( 0.000000000000000000, 0.000000000000000000, 1.000000000000000000 ) ) ;
#39408 = ORIENTED_EDGE ( 'NONE', *, *, #969, .F. ) ;
#39409 = CARTESIAN_POINT ( 'NONE',  ( 0.5806925824938499181, 17.36345040154836994, -43.56297685531297503 ) ) ;
#39410 = ORIENTED_EDGE ( 'NONE', *, *, #47396, .T. ) ;
#39411 = EDGE_CURVE ( 'NONE', #13765, #30850, #24165, .T. ) ;
#39412 = EDGE_CURVE ( 'NONE', #1725, #20243, #56756, .T. ) ;
#39413 = CARTESIAN_POINT ( 'NONE',  ( 1.231276596079881047, 5.037240371906286818, -41.61613846158368091 ) ) ;
#39414 = CARTESIAN_POINT ( 'NONE',  ( 4.956445790444027111, 14.46717203539434671, -44.81337951368921324 ) ) ;
#39415 = ORIENTED_EDGE ( 'NONE', *, *, #128, .T. ) ;
#39416 = LINE ( 'NONE', #49400, #58508 ) ;
#39417 = ADVANCED_FACE ( 'NONE', ( #29528 ), #27673, .T. ) ;
#39418 = CARTESIAN_POINT ( 'NONE',  ( 5.895596859100789899, 18.99884588797230478, 6.600911917119146821 ) ) ;
#39419 = LINE ( 'NONE', #33479, #2697 ) ;
#39420 = CARTESIAN_POINT ( 'NONE',  ( 2.526464513654346877, 33.34586834545809353, -27.11556434133515125 ) ) ;
#39421 = B_SPLINE_CURVE_WITH_KNOTS ( 'NONE', 3,
 ( #61309, #46323, #13418, #17497 ),
 .UNSPECIFIED., .F., .F.,
 ( 4, 4 ),
 ( 0.000000000000000000, 0.005004948556313593665 ),
 .UNSPECIFIED. ) ;
#39422 = AXIS2_PLACEMENT_3D ( 'NONE', #54166, #15068, #11602 ) ;
#39423 = VERTEX_POINT ( 'NONE', #57396 ) ;
#39424 = CARTESIAN_POINT ( 'NONE',  ( 0.8753041380234471980, -26.21158409634572095, 41.52217705074212972 ) ) ;
#39425 = CARTESIAN_POINT ( 'NONE',  ( 5.910764540655178756, -7.242942773736176676, -18.76275615269638308 ) ) ;
#39426 = EDGE_LOOP ( 'NONE', ( #12910, #35460, #3225, #13712 ) ) ;
#39427 = CARTESIAN_POINT ( 'NONE',  ( 0.3622758884714730732, 20.83792692158972670, -37.74294673546565804 ) ) ;
#39428 = EDGE_CURVE ( 'NONE', #55454, #17384, #60766, .T. ) ;
#39429 = ORIENTED_EDGE ( 'NONE', *, *, #43085, .F. ) ;
#39430 = CARTESIAN_POINT ( 'NONE',  ( 0.9762797500689124330, -11.93232144563832975, 40.17392798947675914 ) ) ;
#39431 = ORIENTED_EDGE ( 'NONE', *, *, #25512, .F. ) ;
#39432 = CARTESIAN_POINT ( 'NONE',  ( 0.1129192098497447394, 36.71339784380064231, -24.47607416535520741 ) ) ;
#39433 = CARTESIAN_POINT ( 'NONE',  ( 0.6026112563231247332, -30.48163520784209979, -38.50208968303211776 ) ) ;
#39434 = CARTESIAN_POINT ( 'NONE',  ( 5.901463166500146684, 19.71248269111027440, 3.991979019648623783 ) ) ;
#39435 = ORIENTED_EDGE ( 'NONE', *, *, #11314, .T. ) ;
#39436 = CARTESIAN_POINT ( 'NONE',  ( 0.6041374136657476912, -18.24862627831563699, 44.51224464244968715 ) ) ;
#39437 = CARTESIAN_POINT ( 'NONE',  ( 0.8760168074887090262, -44.77533136581869400, -17.58183840866385594 ) ) ;
#39438 = DIRECTION ( 'NONE',  ( 1.000000000000000000, 0.000000000000000000, 0.000000000000000000 ) ) ;
#39439 = ORIENTED_EDGE ( 'NONE', *, *, #2245, .F. ) ;
#39440 = ORIENTED_EDGE ( 'NONE', *, *, #17240, .F. ) ;
#39441 = CARTESIAN_POINT ( 'NONE',  ( 0.9790320750461900534, -31.02392677839150181, -28.17539883996666106 ) ) ;
#39442 = CARTESIAN_POINT ( 'NONE',  ( 4.963659409799330291, 13.93274247732079374, -42.53037318520974708 ) ) ;
#39443 = CARTESIAN_POINT ( 'NONE',  ( 1.227938101723748288, 39.32113113558966688, 17.20315230597858047 ) ) ;
#39444 = CARTESIAN_POINT ( 'NONE',  ( 0.8751705887134423323, -42.09020928323391075, 23.27176129838352736 ) ) ;
#39445 = CARTESIAN_POINT ( 'NONE',  ( 0.9785694773339246311, -26.88704742894960731, -32.14688299459353260 ) ) ;
#39446 = FACE_OUTER_BOUND ( 'NONE', #37826, .T. ) ;
#39447 = ORIENTED_EDGE ( 'NONE', *, *, #59231, .F. ) ;
#39448 = CARTESIAN_POINT ( 'NONE',  ( 4.956445790443998689, 1.033212179477464909, 47.07940656732852602 ) ) ;
#39449 = ORIENTED_EDGE ( 'NONE', *, *, #52731, .T. ) ;
#39450 = CARTESIAN_POINT ( 'NONE',  ( 4.962356264823608143, 0.000000000000000000, 0.000000000000000000 ) ) ;
#39451 = CARTESIAN_POINT ( 'NONE',  ( 0.6845945791218034371, -0.7015599581307697674, -46.90324439033072679 ) ) ;
#39452 = CARTESIAN_POINT ( 'NONE',  ( 0.5806925824938511393, -42.09901922557415332, -20.66143612114853312 ) ) ;
#39453 = CONICAL_SURFACE ( 'NONE', #9371, 42.92674063221959813, 1.485477209440487556 ) ;
#39454 = CARTESIAN_POINT ( 'NONE',  ( 3.407937589446178528, 8.699069120706768743, 10.58239600294641747 ) ) ;
#39455 = CARTESIAN_POINT ( 'NONE',  ( 0.3676999524040366896, 10.61898383218289155, 42.81574203134493928 ) ) ;
#39456 =( LENGTH_UNIT ( ) NAMED_UNIT ( * ) SI_UNIT ( .MILLI., .METRE. ) );
#39457 = CARTESIAN_POINT ( 'NONE',  ( 1.827119703190778877, -17.60659059422150463, -39.28489939038881573 ) ) ;
#39458 =( BOUNDED_SURFACE ( )  B_SPLINE_SURFACE ( 3, 1, ( 
 ( #31358, #55452 ),
 ( #31665, #50758 ),
 ( #7848, #26968 ),
 ( #41397, #60455 ) ),
 .UNSPECIFIED., .F., .F., .F. ) 
 B_SPLINE_SURFACE_WITH_KNOTS ( ( 4, 4 ),
 ( 2, 2 ),
 ( 0.000000000000000000, 1.000000000000000000 ),
 ( 0.000000000000000000, 1.000000000000000000 ),
 .UNSPECIFIED. ) 
 GEOMETRIC_REPRESENTATION_ITEM ( )  RATIONAL_B_SPLINE_SURFACE ( (
 ( 1.000000000000000000, 1.000000000000000000),
 ( 0.9953485035131437453, 0.8621029689291523912),
 ( 0.9953485035131437453, 0.8621029689291523912),
 ( 1.000000000000000000, 1.000000000000000000) ) ) 
 REPRESENTATION_ITEM ( '' )  SURFACE ( )  );
#39459 = EDGE_CURVE ( 'NONE', #46746, #41690, #52562, .T. ) ;
#39460 = CARTESIAN_POINT ( 'NONE',  ( 4.962356264823608143, -10.17958088187436871, 40.83640203215416165 ) ) ;
#39461 = CARTESIAN_POINT ( 'NONE',  ( 0.3676999524040323597, 30.26295534861902681, -32.09523511193413725 ) ) ;
#39462 = CARTESIAN_POINT ( 'NONE',  ( 2.648799415243696664, -6.455064903435647317, -48.60915140569758108 ) ) ;
#39463 =( BOUNDED_SURFACE ( )  B_SPLINE_SURFACE ( 3, 1, ( 
 ( #16835, #56251 ),
 ( #17438, #36561 ),
 ( #50323, #36254 ),
 ( #13062, #51545 ) ),
 .UNSPECIFIED., .F., .F., .F. ) 
 B_SPLINE_SURFACE_WITH_KNOTS ( ( 4, 4 ),
 ( 2, 2 ),
 ( 0.000000000000000000, 1.000000000000000000 ),
 ( 0.000000000000000000, 1.000000000000000000 ),
 .UNSPECIFIED. ) 
 GEOMETRIC_REPRESENTATION_ITEM ( )  RATIONAL_B_SPLINE_SURFACE ( (
 ( 1.000000000000000000, 1.000000000000000000),
 ( 0.7211978278499968642, 0.9934217856018975334),
 ( 0.7211978278499968642, 0.9934217856018975334),
 ( 1.000000000000000000, 1.000000000000000000) ) ) 
 REPRESENTATION_ITEM ( '' )  SURFACE ( )  );
#39464 = DIRECTION ( 'NONE',  ( 0.09835009131224549395, -0.7091251765524022588, -0.6981896185982696679 ) ) ;
#39465 = CARTESIAN_POINT ( 'NONE',  ( 4.549368137175248350, 0.000000000000000000, 0.000000000000000000 ) ) ;
#39466 = LINE ( 'NONE', #31505, #26147 ) ;
#39467 = CIRCLE ( 'NONE', #12444, 48.91267123290010943 ) ;
#39468 = CARTESIAN_POINT ( 'NONE',  ( 0.7954196712028480665, 11.60747899261454741, 46.67728755034890042 ) ) ;
#39469 = LINE ( 'NONE', #38538, #4621 ) ;
#39470 = EDGE_LOOP ( 'NONE', ( #11145, #21588, #22346, #61231 ) ) ;
#39471 = CARTESIAN_POINT ( 'NONE',  ( 3.240649175237395152, -41.42738255131205705, 14.79989501127953133 ) ) ;
#39472 = LINE ( 'NONE', #43247, #29896 ) ;
#39473 = CARTESIAN_POINT ( 'NONE',  ( 0.5837374860065642768, 18.16107481025659354, -44.31936661703453240 ) ) ;
#39474 = CARTESIAN_POINT ( 'NONE',  ( 3.221118495291108719, 40.41289623301514666, 17.36546105697460618 ) ) ;
#39475 = FACE_OUTER_BOUND ( 'NONE', #41795, .T. ) ;
#39476 = ORIENTED_EDGE ( 'NONE', *, *, #38321, .T. ) ;
#39477 = CARTESIAN_POINT ( 'NONE',  ( 0.9756354156337461170, -37.22481466014910723, 21.34128958497367279 ) ) ;
#39478 = CARTESIAN_POINT ( 'NONE',  ( 0.6021447746440204973, 27.88050730053805992, -40.42546786065847897 ) ) ;
#39479 = B_SPLINE_CURVE_WITH_KNOTS ( 'NONE', 3,
 ( #51045, #41379, #60434, #50740, #21948, #1336, #12871, #15781, #15468, #30164, #41085, #34895, #7508, #24866, #60141, #17250, #7829, #44006, #32898 ),
 .UNSPECIFIED., .F., .F.,
 ( 4, 3, 3, 3, 3, 3, 4 ),
 ( 1.040890552917501732E-17, 0.0002732106629380605888, 0.0004098138914053724505, 0.0005464171197651409434, 0.0006830203481512540312, 0.0008196235766963588625, 0.001011968216111140510 ),
 .UNSPECIFIED. ) ;
#39480 = EDGE_CURVE ( 'NONE', #61, #40810, #25725, .T. ) ;
#39481 = DIRECTION ( 'NONE',  ( -1.836970198721032153E-16, 1.000000000000000000, -1.110223024625156540E-16 ) ) ;
#39482 = ORIENTED_EDGE ( 'NONE', *, *, #39734, .F. ) ;
#39483 = CARTESIAN_POINT ( 'NONE',  ( 4.553261556744875094, 0.000000000000000000, 0.000000000000000000 ) ) ;
#39484 = AXIS2_PLACEMENT_3D ( 'NONE', #61144, #32672, #42691 ) ;
#39485 = EDGE_CURVE ( 'NONE', #29768, #33332, #32391, .T. ) ;
#39486 = CARTESIAN_POINT ( 'NONE',  ( 0.7057020205115056566, 23.21851350879818554, 41.89806668505389098 ) ) ;
#39487 = VERTEX_POINT ( 'NONE', #28605 ) ;
#39488 = B_SPLINE_CURVE_WITH_KNOTS ( 'NONE', 3,
 ( #5137, #57141, #47467, #47778, #4516, #14274, #28656, #43403, #14580, #3908, #32443, #51521, #9546, #56536, #4825, #23965, #43092, #33380, #8611 ),
 .UNSPECIFIED., .F., .F.,
 ( 4, 3, 3, 3, 3, 3, 4 ),
 ( 1.185767046459373819E-16, 0.0002618519381806248868, 0.0003927759815485986857, 0.0005237000248299433216, 0.0006546240681325007525, 0.0007855481115631354197, 0.0009699050456655109419 ),
 .UNSPECIFIED. ) ;
#39489 = EDGE_CURVE ( 'NONE', #27511, #33696, #21179, .T. ) ;
#39490 = CARTESIAN_POINT ( 'NONE',  ( -6.001507490154110336, 4.862106078788180241, -18.20581304543292589 ) ) ;
#39491 = ORIENTED_EDGE ( 'NONE', *, *, #58541, .F. ) ;
#39492 = DIRECTION ( 'NONE',  ( 1.000000000000000000, 1.836909530733573776E-16, 0.000000000000000000 ) ) ;
#39493 = ADVANCED_FACE ( 'NONE', ( #41058 ), #42014, .F. ) ;
#39494 = ORIENTED_EDGE ( 'NONE', *, *, #52133, .F. ) ;
#39495 = CARTESIAN_POINT ( 'NONE',  ( 4.975610109902397937, 48.43414999183889336, 6.825138951393308950 ) ) ;
#39496 = CARTESIAN_POINT ( 'NONE',  ( 0.1129192098497447394, 43.99990943031675528, -3.310552508128703497 ) ) ;
#39497 = ORIENTED_EDGE ( 'NONE', *, *, #13250, .T. ) ;
#39498 = CARTESIAN_POINT ( 'NONE',  ( 4.975610109902397937, -32.45573888811652807, 36.59336579715199633 ) ) ;
#39499 = ORIENTED_EDGE ( 'NONE', *, *, #38713, .T. ) ;
#39500 = CARTESIAN_POINT ( 'NONE',  ( 0.5782707292762442330, -38.25309408463849081, -27.13737545635934012 ) ) ;
#39501 = CARTESIAN_POINT ( 'NONE',  ( 4.834790513006555379, 47.24803566211424766, -0.4609414235693951589 ) ) ;
#39502 = AXIS2_PLACEMENT_3D ( 'NONE', #51396, #22609, #45507 ) ;
#39503 = ORIENTED_EDGE ( 'NONE', *, *, #15430, .T. ) ;
#39504 = CARTESIAN_POINT ( 'NONE',  ( 5.895596859100789899, 16.57987064389762111, 11.38578379577399069 ) ) ;
#39505 = CARTESIAN_POINT ( 'NONE',  ( 3.559346040607745287, -36.42883594846195194, -24.62458513319633369 ) ) ;
#39506 = ADVANCED_FACE ( 'NONE', ( #2790 ), #40012, .F. ) ;
#39507 = VECTOR ( 'NONE', #9609, 1000.000000000000000 ) ;
#39508 = CARTESIAN_POINT ( 'NONE',  ( 0.5797568599927140909, -34.35528703333429235, -31.92083271984328618 ) ) ;
#39509 = CARTESIAN_POINT ( 'NONE',  ( 0.5998501479064708430, 44.24259072156059602, 18.89267974119682947 ) ) ;
#39510 = ORIENTED_EDGE ( 'NONE', *, *, #23085, .T. ) ;
#39511 = CARTESIAN_POINT ( 'NONE',  ( 3.270143674763207553, 6.605065939546987508, -11.98875605389972421 ) ) ;
#39512 = EDGE_CURVE ( 'NONE', #45872, #22599, #8612, .T. ) ;
#39513 = CARTESIAN_POINT ( 'NONE',  ( 0.1135584504625008623, -18.25492125837011770, 40.17100822715256214 ) ) ;
#39514 = AXIS2_PLACEMENT_3D ( 'NONE', #33890, #48283, #52966 ) ;
#39515 = B_SPLINE_CURVE_WITH_KNOTS ( 'NONE', 3,
 ( #26855, #3333, #25932, #26542, #22161, #30936 ),
 .UNSPECIFIED., .F., .F.,
 ( 4, 2, 4 ),
 ( 3.476216610979977084E-18, 0.0002291966416970788345, 0.0004583932833941541996 ),
 .UNSPECIFIED. ) ;
#39516 = ORIENTED_EDGE ( 'NONE', *, *, #27468, .T. ) ;
#39517 = CARTESIAN_POINT ( 'NONE',  ( -1.200000000000006617, 0.000000000000000000, -6.728125000000022560 ) ) ;
#39518 = ORIENTED_EDGE ( 'NONE', *, *, #579, .T. ) ;
#39519 = CARTESIAN_POINT ( 'NONE',  ( 4.962356264823609031, -3.779019546646985361, -41.91604238389410853 ) ) ;
#39520 = CARTESIAN_POINT ( 'NONE',  ( 0.1156867017252034557, 25.14158812297082335, 36.26076879949014398 ) ) ;
#39521 = ORIENTED_EDGE ( 'NONE', *, *, #1552, .F. ) ;
#39522 = CARTESIAN_POINT ( 'NONE',  ( 4.975801465491694664, 3.702618843597456522, -47.76942479135481534 ) ) ;
#39523 = CARTESIAN_POINT ( 'NONE',  ( 2.528100132419517365, -36.90587533319831692, 20.00525292323244386 ) ) ;
#39524 = CARTESIAN_POINT ( 'NONE',  ( 0.6001305935487422083, 47.62765676940934867, 6.798494447612372760 ) ) ;
#39525 = CARTESIAN_POINT ( 'NONE',  ( 1.399999999999998579, 0.000000000000000000, 0.000000000000000000 ) ) ;
#39526 = ORIENTED_EDGE ( 'NONE', *, *, #45787, .F. ) ;
#39527 = CARTESIAN_POINT ( 'NONE',  ( -2.569797478183790229, -14.62602397812941035, -0.4487456364278306631 ) ) ;
#39528 = DIRECTION ( 'NONE',  ( 0.09722883295013597105, 0.6635018476521645781, 0.7418300696286974638 ) ) ;
#39529 = CARTESIAN_POINT ( 'NONE',  ( 2.281351352603296245, 1.314116150904124369, -47.95523304704244794 ) ) ;
#39530 = CARTESIAN_POINT ( 'NONE',  ( 0.6000166863083090663, 46.44114019838971785, 15.97009639238173051 ) ) ;
#39531 = CIRCLE ( 'NONE', #24513, 2.649999999999999467 ) ;
#39532 = EDGE_CURVE ( 'NONE', #3838, #13148, #6614, .T. ) ;
#39533 = CARTESIAN_POINT ( 'NONE',  ( 0.3622758884714600280, 6.444611261694588755, -42.62881903538203687 ) ) ;
#39534 = CARTESIAN_POINT ( 'NONE',  ( 4.956653778116994147, 32.11725092155092653, -35.79382859084083179 ) ) ;
#39535 = CARTESIAN_POINT ( 'NONE',  ( -16.69190930225257929, -7.824346355838889266, -1.669031402509471240 ) ) ;
#39536 = DIRECTION ( 'NONE',  ( 1.836766033387207149E-16, -1.000000000000000000, 0.000000000000000000 ) ) ;
#39537 = CARTESIAN_POINT ( 'NONE',  ( 0.5998501479064699549, 47.62484632993687939, -6.798102206413639159 ) ) ;
#39538 = CARTESIAN_POINT ( 'NONE',  ( -6.063463321072278589, -1.833563764454256395, -19.16920698414909197 ) ) ;
#39539 = FACE_OUTER_BOUND ( 'NONE', #57092, .T. ) ;
#39540 = CARTESIAN_POINT ( 'NONE',  ( 0.7056555295713315967, 44.57023068418428835, 17.55111680842054511 ) ) ;
#39541 = B_SPLINE_CURVE_WITH_KNOTS ( 'NONE', 3,
 ( #57587, #48525, #15341, #18807, #14723, #5285, #48232, #42932, #24727, #14416, #4348, #43547, #591, #19125, #20046, #43242, #52600, #34447, #42966 ),
 .UNSPECIFIED., .F., .F.,
 ( 4, 3, 3, 3, 3, 3, 4 ),
 ( 3.469446951953614189E-18, 0.0002732106629380643293, 0.0004098138914053842683, 0.0005464171197651466897, 0.0006830203481512559828, 0.0008196235766963655845, 0.001011968216111143546 ),
 .UNSPECIFIED. ) ;
#39542 = DIRECTION ( 'NONE',  ( 1.000000000000000000, 0.000000000000000000, 0.000000000000000000 ) ) ;
#39543 = CARTESIAN_POINT ( 'NONE',  ( 0.8554163680231720024, -46.86440027434175448, -2.221139355847800090 ) ) ;
#39544 = ORIENTED_EDGE ( 'NONE', *, *, #35510, .F. ) ;
#39545 = CARTESIAN_POINT ( 'NONE',  ( 0.1119899015040012186, -44.12081468926701433, -0.5612658441996505321 ) ) ;
#39546 = VECTOR ( 'NONE', #28414, 1000.000000000000114 ) ;
#39547 = CARTESIAN_POINT ( 'NONE',  ( 3.221118495291109163, 18.65183604292354147, -39.83554231951222135 ) ) ;
#39548 = CARTESIAN_POINT ( 'NONE',  ( 0.9754292589017243831, 38.35198883237011813, -16.89533721169931724 ) ) ;
#39549 = EDGE_LOOP ( 'NONE', ( #26380, #18752, #24953, #23926 ) ) ;
#39550 = CARTESIAN_POINT ( 'NONE',  ( -16.98648177666932213, 7.159091074317976755, -1.550344604434408250E-15 ) ) ;
#39551 = TOROIDAL_SURFACE ( 'NONE', #8477, 15.38217999999999996, 0.05882000000000109363 ) ;
#39552 = CARTESIAN_POINT ( 'NONE',  ( 0.1157506346131639274, 4.329268483212691088, 43.91125247818713717 ) ) ;
#39553 = B_SPLINE_CURVE_WITH_KNOTS ( 'NONE', 3,
 ( #18372, #52474, #19295, #5159 ),
 .UNSPECIFIED., .F., .F.,
 ( 4, 4 ),
 ( 0.000000000000000000, 0.005014147105413702989 ),
 .UNSPECIFIED. ) ;
#39554 = EDGE_LOOP ( 'NONE', ( #44879, #34537, #12071, #9664 ) ) ;
#39555 = ORIENTED_EDGE ( 'NONE', *, *, #22998, .T. ) ;
#39556 = CARTESIAN_POINT ( 'NONE',  ( 5.959828726073459926, 16.28130559351264495, -12.49879082830551269 ) ) ;
#39557 = EDGE_CURVE ( 'NONE', #40367, #45029, #293, .T. ) ;
#39558 = ORIENTED_EDGE ( 'NONE', *, *, #15305, .T. ) ;
#39559 = FACE_OUTER_BOUND ( 'NONE', #38194, .T. ) ;
#39560 = ORIENTED_EDGE ( 'NONE', *, *, #51726, .F. ) ;
#39561 = EDGE_CURVE ( 'NONE', #11576, #40053, #57647, .T. ) ;
#39562 = VERTEX_POINT ( 'NONE', #40748 ) ;
#39563 = CARTESIAN_POINT ( 'NONE',  ( 0.7242486021783869354, -48.79688800429393325, 5.465819560722072090 ) ) ;
#39564 = VERTEX_POINT ( 'NONE', #22232 ) ;
#39565 = CARTESIAN_POINT ( 'NONE',  ( 2.282803330402960018, 26.79503163932819376, 38.58138394231581714 ) ) ;
#39566 = CARTESIAN_POINT ( 'NONE',  ( 4.967162193818130511, -18.65818244221228284, -38.83676580803786749 ) ) ;
#39567 = ORIENTED_EDGE ( 'NONE', *, *, #2670, .F. ) ;
#39568 = CARTESIAN_POINT ( 'NONE',  ( 1.000433927950263868, -21.99288785380132083, 35.67536350905153597 ) ) ;
#39569 = APPLICATION_CONTEXT ( 'automotive_design' ) ;
#39570 =( BOUNDED_SURFACE ( )  B_SPLINE_SURFACE ( 3, 1, ( 
 ( #14345, #28116 ),
 ( #33764, #19052 ),
 ( #57838, #47857 ),
 ( #42546, #9007 ) ),
 .UNSPECIFIED., .F., .F., .F. ) 
 B_SPLINE_SURFACE_WITH_KNOTS ( ( 4, 4 ),
 ( 2, 2 ),
 ( 0.000000000000000000, 1.000000000000000000 ),
 ( 0.000000000000000000, 1.000000000000000000 ),
 .UNSPECIFIED. ) 
 GEOMETRIC_REPRESENTATION_ITEM ( )  RATIONAL_B_SPLINE_SURFACE ( (
 ( 1.000000000000000000, 1.000000000000000000),
 ( 0.7269869731126817891, 0.9931720237060910339),
 ( 0.7269869731126817891, 0.9931720237060910339),
 ( 1.000000000000000000, 1.000000000000000000) ) ) 
 REPRESENTATION_ITEM ( '' )  SURFACE ( )  );
#39571 = CARTESIAN_POINT ( 'NONE',  ( 3.270143674763207553, 11.71453292426878967, 7.080034332678304843 ) ) ;
#39572 = ORIENTED_EDGE ( 'NONE', *, *, #17624, .F. ) ;
#39573 = ORIENTED_EDGE ( 'NONE', *, *, #34721, .F. ) ;
#39574 = CARTESIAN_POINT ( 'NONE',  ( 5.896782393890504181, -9.660289833039353624, -17.64100017628503991 ) ) ;
#39575 = ADVANCED_FACE ( 'NONE', ( #40431 ), #25269, .F. ) ;
#39576 = CARTESIAN_POINT ( 'NONE',  ( 50.15363872391542799, 12.21587082446438188, 2.649999999999994138 ) ) ;
#39577 = CARTESIAN_POINT ( 'NONE',  ( 5.910764540655178756, -4.647344284407041393, 19.56791837603970308 ) ) ;
#39578 = CARTESIAN_POINT ( 'NONE',  ( 0.2224561200757617097, 0.7594684977685240979, -43.11279565427788896 ) ) ;
#39579 = ADVANCED_FACE ( 'NONE', ( #2483 ), #18394, .F. ) ;
#39580 = ORIENTED_EDGE ( 'NONE', *, *, #39290, .F. ) ;
#39581 = CARTESIAN_POINT ( 'NONE',  ( -6.078726893082806448, 7.797636468844645563, 17.60655862934219584 ) ) ;
#39582 = CARTESIAN_POINT ( 'NONE',  ( 0.1084644655670283508, 41.75632203164217771, 10.77688306151818232 ) ) ;
#39583 = FACE_OUTER_BOUND ( 'NONE', #37186, .T. ) ;
#39584 = CARTESIAN_POINT ( 'NONE',  ( 4.975610109902397937, -11.44439439467595143, 47.55497076097179843 ) ) ;
#39585 = CIRCLE ( 'NONE', #1529, 42.92674063221959813 ) ;
#39586 = ORIENTED_EDGE ( 'NONE', *, *, #19186, .T. ) ;
#39587 = CARTESIAN_POINT ( 'NONE',  ( 4.226256110419178924, -43.04997224218647034, -8.804949740581237805 ) ) ;
#39588 = CARTESIAN_POINT ( 'NONE',  ( 0.2885697896453112699, 42.63514065501006201, 6.424755442172748410 ) ) ;
#39589 = CARTESIAN_POINT ( 'NONE',  ( 5.917102823773431552, 20.06644099299511552, -1.351911212464495415 ) ) ;
#39590 = CARTESIAN_POINT ( 'NONE',  ( 0.7413678028165009426, -6.114974495787087072, 43.67027797811822154 ) ) ;
#39592 = ORIENTED_EDGE ( 'NONE', *, *, #770, .F. ) ;
#39591 = VECTOR ( 'NONE', #12664, 999.9999999999998863 ) ;
#39593 = ORIENTED_EDGE ( 'NONE', *, *, #54980, .F. ) ;
#39594 = CARTESIAN_POINT ( 'NONE',  ( 1.129531546211735016, 0.000000000000000000, 0.000000000000000000 ) ) ;
#39595 = DIRECTION ( 'NONE',  ( -1.000000000000000000, -0.000000000000000000, -0.000000000000000000 ) ) ;
#39596 = CARTESIAN_POINT ( 'NONE',  ( 0.9775691876210985676, 15.41418421489670365, -38.97097168379585952 ) ) ;
#39597 = VECTOR ( 'NONE', #5634, 1000.000000000000114 ) ;
#39598 = CARTESIAN_POINT ( 'NONE',  ( 0.9722240750034584211, -33.68410530487889076, 26.58024222649031643 ) ) ;
#39599 = DIRECTION ( 'NONE',  ( -1.836970198721032153E-16, 1.000000000000000000, -1.110223024625156540E-16 ) ) ;
#39600 = CARTESIAN_POINT ( 'NONE',  ( 0.2224561200757614321, -43.11279565427786764, -0.7594684977683735516 ) ) ;
#39601 = CARTESIAN_POINT ( 'NONE',  ( 2.624215991343620935, 47.39206852872467834, -7.662883702704190725 ) ) ;
#39602 = CARTESIAN_POINT ( 'NONE',  ( 1.154321713695928064, 37.57248787340968477, -20.73950268329786439 ) ) ;
#39603 = EDGE_CURVE ( 'NONE', #31065, #10036, #22538, .T. ) ;
#39604 = CARTESIAN_POINT ( 'NONE',  ( 0.6001305935487315502, 37.84751346122855864, -29.70149728382397214 ) ) ;
#39605 = CARTESIAN_POINT ( 'NONE',  ( 0.6023142530420679819, -18.65157113320520921, -44.34465601638692789 ) ) ;
#39606 = B_SPLINE_CURVE_WITH_KNOTS ( 'NONE', 3,
 ( #24959, #29334, #48442, #53435, #5507, #39081, #58134, #15258, #34363, #10546, #1128, #39383, #58435, #15559, #58743, #15870 ),
 .UNSPECIFIED., .F., .F.,
 ( 4, 3, 3, 3, 3, 4 ),
 ( 1.962735358247464152E-17, 0.0002618515315864419226, 0.0003927756766342003765, 0.0005236998216950570226, 0.0007855159896329932598, 0.001047349442285927870 ),
 .UNSPECIFIED. ) ;
#39607 = CARTESIAN_POINT ( 'NONE',  ( -6.072942160501519915, -12.93525546908874624, 14.26475826077785136 ) ) ;
#39608 = CARTESIAN_POINT ( 'NONE',  ( 0.7057020205115022149, -28.48867101281799563, -38.50899875908083203 ) ) ;
#39609 = CARTESIAN_POINT ( 'NONE',  ( 5.895881250540457863, -13.97904524590137854, -14.46077368681714326 ) ) ;
#39610 = CARTESIAN_POINT ( 'NONE',  ( 0.8760168074886960365, 37.61398439004493355, 29.98565522133359451 ) ) ;
#39611 = LINE ( 'NONE', #57744, #21144 ) ;
#39612 = CARTESIAN_POINT ( 'NONE',  ( 0.5839879327111930918, -41.43370681949794943, 24.02664985973689582 ) ) ;
#39613 = CARTESIAN_POINT ( 'NONE',  ( 5.960221823109900008, -20.35070456576733022, -2.673723662181264782 ) ) ;
#39614 = LINE ( 'NONE', #5434, #41905 ) ;
#39615 = CARTESIAN_POINT ( 'NONE',  ( 4.967162193818130511, -28.07411493385318124, 32.68434214048159703 ) ) ;
#39616 = CARTESIAN_POINT ( 'NONE',  ( 5.895596859100789899, -19.93295055289972950, -2.684337063064522244 ) ) ;
#39617 = CARTESIAN_POINT ( 'NONE',  ( 0.6008123274975391004, 49.03265588904381644, -2.711679852983228223 ) ) ;
#39619 = ORIENTED_EDGE ( 'NONE', *, *, #49652, .F. ) ;
#39618 = CARTESIAN_POINT ( 'NONE',  ( 0.8744876279028263033, -19.05609938968970241, -45.24616145519706834 ) ) ;
#39620 = ORIENTED_EDGE ( 'NONE', *, *, #24185, .F. ) ;
#39621 = CARTESIAN_POINT ( 'NONE',  ( 4.291220156522059348, -46.54716543045785215, 7.262946213162170039 ) ) ;
#39622 = CARTESIAN_POINT ( 'NONE',  ( 0.1145239942831223490, 41.77227326564666043, 14.21346780081533900 ) ) ;
#39623 = EDGE_LOOP ( 'NONE', ( #6941, #47403, #5325, #34610 ) ) ;
#39624 = ORIENTED_EDGE ( 'NONE', *, *, #56900, .F. ) ;
#39625 = CARTESIAN_POINT ( 'NONE',  ( 0.6000166863083090663, -2.096232480231297046, -49.06556115135418850 ) ) ;
#39626 = CARTESIAN_POINT ( 'NONE',  ( 4.956445790443991584, 39.12691469763999663, 26.20348443209871903 ) ) ;
#39627 = DIRECTION ( 'NONE',  ( -1.000000000000000000, -0.000000000000000000, -0.000000000000000000 ) ) ;
#39628 = B_SPLINE_CURVE_WITH_KNOTS ( 'NONE', 3,
 ( #37976, #4389, #13849, #32953, #37339, #61410, #5326, #635, #28845, #47966, #24143, #24455, #8816, #43593, #56723, #9121 ),
 .UNSPECIFIED., .F., .F.,
 ( 4, 3, 3, 3, 3, 4 ),
 ( 9.813676791237319219E-18, 0.0002724568934985570649, 0.0004086836638483829116, 0.0005449104342063630429, 0.0008173270854453619028, 0.001089761613562694647 ),
 .UNSPECIFIED. ) ;
#39629 =( BOUNDED_SURFACE ( )  B_SPLINE_SURFACE ( 3, 1, ( 
 ( #35335, #54394 ),
 ( #15911, #30600 ),
 ( #58174, #49717 ),
 ( #1166, #48796 ) ),
 .UNSPECIFIED., .F., .F., .F. ) 
 B_SPLINE_SURFACE_WITH_KNOTS ( ( 4, 4 ),
 ( 2, 2 ),
 ( 0.000000000000000000, 1.000000000000000000 ),
 ( 0.000000000000000000, 1.000000000000000000 ),
 .UNSPECIFIED. ) 
 GEOMETRIC_REPRESENTATION_ITEM ( )  RATIONAL_B_SPLINE_SURFACE ( (
 ( 1.000000000000000000, 1.000000000000000000),
 ( 0.9751682680413298332, 0.9999560080971552356),
 ( 0.9751682680413298332, 0.9999560080971552356),
 ( 1.000000000000000000, 1.000000000000000000) ) ) 
 REPRESENTATION_ITEM ( '' )  SURFACE ( )  );
#39630 = ORIENTED_EDGE ( 'NONE', *, *, #8939, .T. ) ;
#39631 = ORIENTED_EDGE ( 'NONE', *, *, #8855, .F. ) ;
#39632 = CARTESIAN_POINT ( 'NONE',  ( -6.017396004339687465, -18.20140164570672425, 4.875835690939116063 ) ) ;
#39633 = EDGE_CURVE ( 'NONE', #46967, #47555, #10046, .T. ) ;
#39634 = CARTESIAN_POINT ( 'NONE',  ( 4.956653778116987041, -47.94889704119048446, -3.690426056930470988 ) ) ;
#39635 = CIRCLE ( 'NONE', #26592, 85.00000000000001421 ) ;
#39636 = CARTESIAN_POINT ( 'NONE',  ( -6.078726893082806448, -12.94330610022648820, 14.25709887966552003 ) ) ;
#39637 = CARTESIAN_POINT ( 'NONE',  ( 0.5987334363312690755, 36.99765863950310774, 32.29142551308128617 ) ) ;
#39638 = EDGE_CURVE ( 'NONE', #57068, #60263, #31677, .T. ) ;
#39640 = CARTESIAN_POINT ( 'NONE',  ( 0.9780106845699476636, -41.00520688714551198, -8.654724409120960971 ) ) ;
#39639 = AXIS2_PLACEMENT_3D ( 'NONE', #28510, #52624, #48256 ) ;
#39641 = B_SPLINE_CURVE_WITH_KNOTS ( 'NONE', 3,
 ( #8278, #56206, #12708, #27399, #23028, #13022 ),
 .UNSPECIFIED., .F., .F.,
 ( 4, 2, 4 ),
 ( 3.471140604459641645E-18, 0.0002291966416970775606, 0.0004583932833941516518 ),
 .UNSPECIFIED. ) ;
#39642 = CARTESIAN_POINT ( 'NONE',  ( 0.6000166863083106206, 41.44150143800074204, -26.35195325346179018 ) ) ;
#39643 = ADVANCED_FACE ( 'NONE', ( #23765, #23154 ), #3706, .F. ) ;
#39644 =( BOUNDED_SURFACE ( )  B_SPLINE_SURFACE ( 3, 1, ( 
 ( #3355, #50070 ),
 ( #55365, #2747 ),
 ( #36606, #12187 ),
 ( #51286, #21566 ) ),
 .UNSPECIFIED., .F., .F., .F. ) 
 B_SPLINE_SURFACE_WITH_KNOTS ( ( 4, 4 ),
 ( 2, 2 ),
 ( 0.000000000000000000, 1.000000000000000000 ),
 ( 0.000000000000000000, 1.000000000000000000 ),
 .UNSPECIFIED. ) 
 GEOMETRIC_REPRESENTATION_ITEM ( )  RATIONAL_B_SPLINE_SURFACE ( (
 ( 1.000000000000000000, 1.000000000000000000),
 ( 0.9732289882329797637, 0.9999525324661233672),
 ( 0.9732289882329797637, 0.9999525324661233672),
 ( 1.000000000000000000, 1.000000000000000000) ) ) 
 REPRESENTATION_ITEM ( '' )  SURFACE ( )  );
#39645 = CARTESIAN_POINT ( 'NONE',  ( 0.1157991065609915438, 15.31532217366139470, -41.38095301288571193 ) ) ;
#39646 = VERTEX_POINT ( 'NONE', #41655 ) ;
#39647 = AXIS2_PLACEMENT_3D ( 'NONE', #9003, #60367, #36607 ) ;
#39648 = EDGE_LOOP ( 'NONE', ( #37636, #4468, #31300, #48841 ) ) ;
#39649 = CARTESIAN_POINT ( 'NONE',  ( 1.231276596079887264, -30.51591784428387655, 28.74118176309011830 ) ) ;
#39650 = LINE ( 'NONE', #7004, #26554 ) ;
#39651 = VERTEX_POINT ( 'NONE', #19088 ) ;
#39652 = CARTESIAN_POINT ( 'NONE',  ( -6.015611763856276717, -18.20278301740940208, 4.870987357968111553 ) ) ;
#39653 = CARTESIAN_POINT ( 'NONE',  ( 5.965394784446460541, 14.52385693119002852, -14.50338846149118233 ) ) ;
#39654 = CARTESIAN_POINT ( 'NONE',  ( 3.661921753702001237, 18.64961689156368507, 43.18359542270576412 ) ) ;
#39655 = DIRECTION ( 'NONE',  ( -1.000000000000000000, -0.000000000000000000, -0.000000000000000000 ) ) ;
#39656 = EDGE_CURVE ( 'NONE', #57391, #2702, #53288, .T. ) ;
#39657 = VERTEX_POINT ( 'NONE', #27537 ) ;
#39658 = CARTESIAN_POINT ( 'NONE',  ( 0.5835871038041883230, 46.49557224142410661, -6.115244463143569398 ) ) ;
#39659 = CARTESIAN_POINT ( 'NONE',  ( -2.739355103387248747, 14.91194544146094003, 0.6938660547319468463 ) ) ;
#39660 = CARTESIAN_POINT ( 'NONE',  ( 0.9762797500689124330, -40.96497924994810091, -8.842808390835211085 ) ) ;
#39661 = CARTESIAN_POINT ( 'NONE',  ( 0.6845945791218023269, -42.25019583682482249, -20.37958469802306638 ) ) ;
#39662 = ORIENTED_EDGE ( 'NONE', *, *, #49902, .T. ) ;
#39663 = CARTESIAN_POINT ( 'NONE',  ( 0.5807400328401637335, 46.40483864045162221, -11.87003418057193826 ) ) ;
#39664 = CARTESIAN_POINT ( 'NONE',  ( 4.691466044806103852, 44.51344083442435107, 2.583163953528638146 ) ) ;
#39665 = VERTEX_POINT ( 'NONE', #9659 ) ;
#39666 = DIRECTION ( 'NONE',  ( -1.000000000000000000, -0.000000000000000000, -0.000000000000000000 ) ) ;
#39667 = CARTESIAN_POINT ( 'NONE',  ( 4.975610109902397937, -36.86873347511144772, 32.14258700041067840 ) ) ;
#39668 = ORIENTED_EDGE ( 'NONE', *, *, #21903, .T. ) ;
#39669 = LINE ( 'NONE', #34643, #5860 ) ;
#39670 = CARTESIAN_POINT ( 'NONE',  ( 0.6031356755773454870, -47.69587413076377658, 6.279306815850017820 ) ) ;
#39671 = CARTESIAN_POINT ( 'NONE',  ( 4.303969348037246512, 47.93217632892353919, -4.133486515472823974 ) ) ;
#39672 = B_SPLINE_CURVE_WITH_KNOTS ( 'NONE', 3,
 ( #10897, #35638, #50023, #11833, #24990, #30287, #34395, #53467, #59095, #44130, #58775, #1158, #16206, #58468, #15595, #34700 ),
 .UNSPECIFIED., .F., .F.,
 ( 4, 3, 3, 3, 3, 4 ),
 ( 3.469446951953614189E-18, 0.0002732102107932004621, 0.0004098135523333870092, 0.0005464168938825021780, 0.0008195847345945489731, 0.001092771384553111336 ),
 .UNSPECIFIED. ) ;
#39673 = CARTESIAN_POINT ( 'NONE',  ( 0.6001305935487422083, 18.89378601236063560, -44.24520387813809918 ) ) ;
#39674 = CARTESIAN_POINT ( 'NONE',  ( 5.896782393890504181, -7.222780579330736472, 18.77118876312459150 ) ) ;
#39675 = CARTESIAN_POINT ( 'NONE',  ( 0.3676999524040366896, 21.13209774130265473, 38.72189339863005841 ) ) ;
#39676 = CARTESIAN_POINT ( 'NONE',  ( 0.5804410086790514622, 16.34485605153989951, -43.95867983128970735 ) ) ;
#39677 = CARTESIAN_POINT ( 'NONE',  ( 4.975610109902397937, 0.000000000000000000, 0.000000000000000000 ) ) ;
#39678 = ORIENTED_EDGE ( 'NONE', *, *, #56524, .F. ) ;
#39679 = CARTESIAN_POINT ( 'NONE',  ( 5.838029081930955932, 47.13000430274632890, -3.134924652369159404 ) ) ;
#39680 = CONICAL_SURFACE ( 'NONE', #7616, 2.500000000000002220, 0.9599310885968777018 ) ;
#39681 = CARTESIAN_POINT ( 'NONE',  ( 0.9788927965476035276, 41.55338940985792107, 5.445405511482348970 ) ) ;
#39682 = CARTESIAN_POINT ( 'NONE',  ( 0.5835226383429273911, 27.67095686594207038, -37.86239058312538930 ) ) ;
#39683 = ORIENTED_EDGE ( 'NONE', *, *, #40543, .T. ) ;
#39684 = VECTOR ( 'NONE', #4855, 1000.000000000000000 ) ;
#39685 = CIRCLE ( 'NONE', #28657, 2.649999999999999467 ) ;
#39686 = EDGE_CURVE ( 'NONE', #43289, #19080, #653, .T. ) ;
#39687 = CARTESIAN_POINT ( 'NONE',  ( 4.956445790444005794, -33.12351118015950391, -33.47194433010255921 ) ) ;
#39688 = CARTESIAN_POINT ( 'NONE',  ( -6.079354080745853928, -14.66163526140127615, 12.48316493161076224 ) ) ;
#39689 = CARTESIAN_POINT ( 'NONE',  ( 0.8557997880470697982, -11.51622788066490166, 46.50333260518556244 ) ) ;
#39690 = CARTESIAN_POINT ( 'NONE',  ( 0.3622758884714730732, -39.50828911767010965, 17.25816669464924047 ) ) ;
#39691 = CARTESIAN_POINT ( 'NONE',  ( 0.3676999524040323597, -6.224421213753346116, -43.67158302462387098 ) ) ;
#39692 = CARTESIAN_POINT ( 'NONE',  ( 2.299746137290200831, -36.10727851862707638, -33.17447476094279324 ) ) ;
#39693 = EDGE_CURVE ( 'NONE', #8791, #11235, #8733, .T. ) ;
#39694 = DIRECTION ( 'NONE',  ( -1.000000000000000000, -1.836909530733572050E-16, 1.836909530733589800E-16 ) ) ;
#39695 = CARTESIAN_POINT ( 'NONE',  ( 0.8554163680231816613, 28.56078411578431187, 37.22213163970302929 ) ) ;
#39696 = LINE ( 'NONE', #58746, #48705 ) ;
#39697 = EDGE_CURVE ( 'NONE', #35927, #33554, #51854, .T. ) ;
#39698 = AXIS2_PLACEMENT_3D ( 'NONE', #40397, #59459, #25965 ) ;
#39699 = CARTESIAN_POINT ( 'NONE',  ( 4.960156602257177028, 20.07163247083200019, -41.85906677498932993 ) ) ;
#39701 = ORIENTED_EDGE ( 'NONE', *, *, #18676, .T. ) ;
#39700 = CARTESIAN_POINT ( 'NONE',  ( -6.015611763856276717, -7.205255340944737519, 17.41126425312535275 ) ) ;
#39702 = ORIENTED_EDGE ( 'NONE', *, *, #27073, .F. ) ;
#39703 = CARTESIAN_POINT ( 'NONE',  ( 0.5809828226811560858, -11.86925843957200222, 46.40184912890835278 ) ) ;
#39704 = B_SPLINE_CURVE_WITH_KNOTS ( 'NONE', 3,
 ( #31709, #2871, #27309, #50494, #60195, #3480 ),
 .UNSPECIFIED., .F., .F.,
 ( 4, 2, 4 ),
 ( 1.191143508120180971E-16, 0.0002448718616795919037, 0.0004897437233590647620 ),
 .UNSPECIFIED. ) ;
#39705 = CARTESIAN_POINT ( 'NONE',  ( 4.834790513006555379, -4.078087887156410574, 47.07396881620466189 ) ) ;
#39706 = CARTESIAN_POINT ( 'NONE',  ( 4.958415959904820092, -41.61824873627301002, -18.19684934125545439 ) ) ;
#39707 = CARTESIAN_POINT ( 'NONE',  ( 0.1129192098497447394, -22.45785791439742241, 37.98152716363431125 ) ) ;
#39708 = CARTESIAN_POINT ( 'NONE',  ( 0.5809828226811617480, 24.41822904836982389, -41.20389530892281726 ) ) ;
#39709 = CARTESIAN_POINT ( 'NONE',  ( 0.1139756605157204034, 9.430567968997152661, -43.10475156496261917 ) ) ;
#39710 = ORIENTED_EDGE ( 'NONE', *, *, #19382, .T. ) ;
#39711 = ORIENTED_EDGE ( 'NONE', *, *, #12320, .F. ) ;
#39712 = CARTESIAN_POINT ( 'NONE',  ( 4.963659409799330291, 33.33129552235126880, -29.86601237216371985 ) ) ;
#39713 = EDGE_CURVE ( 'NONE', #16197, #58621, #12211, .T. ) ;
#39714 = CARTESIAN_POINT ( 'NONE',  ( 4.962356264823608143, 0.000000000000000000, 0.000000000000000000 ) ) ;
#39715 = CARTESIAN_POINT ( 'NONE',  ( 0.3676999524040323597, -34.85286720109652947, -27.04123205746306979 ) ) ;
#39716 = EDGE_CURVE ( 'NONE', #43165, #59959, #27901, .T. ) ;
#39717 = VERTEX_POINT ( 'NONE', #4619 ) ;
#39718 = CARTESIAN_POINT ( 'NONE',  ( 4.975801465491695552, 45.55012473237732706, 14.85979367497190040 ) ) ;
#39719 = EDGE_CURVE ( 'NONE', #9930, #57761, #48197, .T. ) ;
#39720 = CARTESIAN_POINT ( 'NONE',  ( 5.960721111146673579, -20.52557019979492026, -0.006321279846748652925 ) ) ;
#39721 = ORIENTED_EDGE ( 'NONE', *, *, #52398, .T. ) ;
#39722 = DIRECTION ( 'NONE',  ( -1.000000000000000000, -0.000000000000000000, -0.000000000000000000 ) ) ;
#39723 = ORIENTED_EDGE ( 'NONE', *, *, #2966, .F. ) ;
#39724 =( BOUNDED_SURFACE ( )  B_SPLINE_SURFACE ( 3, 1, ( 
 ( #17103, #31493 ),
 ( #50288, #12720 ),
 ( #26795, #2979 ),
 ( #36524, #31816 ) ),
 .UNSPECIFIED., .F., .F., .F. ) 
 B_SPLINE_SURFACE_WITH_KNOTS ( ( 4, 4 ),
 ( 2, 2 ),
 ( 0.000000000000000000, 1.000000000000000000 ),
 ( 0.000000000000000000, 1.000000000000000000 ),
 .UNSPECIFIED. ) 
 GEOMETRIC_REPRESENTATION_ITEM ( )  RATIONAL_B_SPLINE_SURFACE ( (
 ( 1.000000000000000000, 1.000000000000000000),
 ( 0.7223157951917476005, 0.9931996967497186413),
 ( 0.7223157951917476005, 0.9931996967497186413),
 ( 1.000000000000000000, 1.000000000000000000) ) ) 
 REPRESENTATION_ITEM ( '' )  SURFACE ( )  );
#39725 = B_SPLINE_CURVE_WITH_KNOTS ( 'NONE', 3,
 ( #729, #28321, #48057, #408 ),
 .UNSPECIFIED., .F., .F.,
 ( 4, 4 ),
 ( 0.000000000000000000, 0.004445488388166993383 ),
 .UNSPECIFIED. ) ;
#39726 = CARTESIAN_POINT ( 'NONE',  ( 0.2224561200757647350, -36.95704201588776527, -22.21411683958040229 ) ) ;
#39727 = CARTESIAN_POINT ( 'NONE',  ( 0.000000000000000000, 0.000000000000000000, 4.000000000000000000 ) ) ;
#39728 = CIRCLE ( 'NONE', #59675, 49.35315702047511621 ) ;
#39729 = ORIENTED_EDGE ( 'NONE', *, *, #25693, .F. ) ;
#39730 = CARTESIAN_POINT ( 'NONE',  ( 2.301529144917016101, -25.12312032040481569, -40.93948199333324567 ) ) ;
#39731 = CARTESIAN_POINT ( 'NONE',  ( 3.661933894777871679, -31.78301468154000275, 34.67666568031975771 ) ) ;
#39732 = CARTESIAN_POINT ( 'NONE',  ( 0.5834872094924170582, 41.59216540884697366, -23.75111410077667529 ) ) ;
#39733 = CARTESIAN_POINT ( 'NONE',  ( 0.1073791018717578927, 43.12183934961191056, 0.4849339620934667305 ) ) ;
#39734 = EDGE_CURVE ( 'NONE', #61015, #30313, #24237, .T. ) ;
#39735 = VERTEX_POINT ( 'NONE', #33804 ) ;
#39736 = CARTESIAN_POINT ( 'NONE',  ( -9.500000000000000000, 1.163414459189985485E-15, 0.000000000000000000 ) ) ;
#39737 = CARTESIAN_POINT ( 'NONE',  ( -4.915099999999998914, 6.044018577294158388E-15, -49.35315702047512332 ) ) ;
#39738 = ORIENTED_EDGE ( 'NONE', *, *, #47185, .T. ) ;
#39739 = CARTESIAN_POINT ( 'NONE',  ( -99.49999999999975842, 2.999999999999992895, -1.500000000000000666 ) ) ;
#39740 = EDGE_LOOP ( 'NONE', ( #4072, #3622, #60408, #31191 ) ) ;
#39741 = CARTESIAN_POINT ( 'NONE',  ( 0.5807400328401637335, 12.92266817606080487, -46.12278621143483548 ) ) ;
#39742 = ORIENTED_EDGE ( 'NONE', *, *, #991, .F. ) ;
#39743 = CARTESIAN_POINT ( 'NONE',  ( 2.281351352603276261, -37.24546109640797908, -30.23585463601414602 ) ) ;
#39745 = CIRCLE ( 'NONE', #48700, 48.09070567114147110 ) ;
#39744 = CARTESIAN_POINT ( 'NONE',  ( 0.9788927965476033055, 35.98586392618627627, -21.47915757467643516 ) ) ;
#39746 =( BOUNDED_SURFACE ( )  B_SPLINE_SURFACE ( 3, 1, ( 
 ( #18716, #14030 ),
 ( #52203, #37848 ),
 ( #33131, #19961 ),
 ( #30248, #57821 ) ),
 .UNSPECIFIED., .F., .F., .F. ) 
 B_SPLINE_SURFACE_WITH_KNOTS ( ( 4, 4 ),
 ( 2, 2 ),
 ( 0.000000000000000000, 1.000000000000000000 ),
 ( 0.000000000000000000, 1.000000000000000000 ),
 .UNSPECIFIED. ) 
 GEOMETRIC_REPRESENTATION_ITEM ( )  RATIONAL_B_SPLINE_SURFACE ( (
 ( 1.000000000000000000, 1.000000000000000000),
 ( 0.7269869731126817891, 0.9931720237060910339),
 ( 0.7269869731126817891, 0.9931720237060910339),
 ( 1.000000000000000000, 1.000000000000000000) ) ) 
 REPRESENTATION_ITEM ( '' )  SURFACE ( )  );
#39747 = CARTESIAN_POINT ( 'NONE',  ( 5.000000000000000888, 0.000000000000000000, 0.000000000000000000 ) ) ;
#39748 = ORIENTED_EDGE ( 'NONE', *, *, #54275, .F. ) ;
#39749 = CARTESIAN_POINT ( 'NONE',  ( 3.660176727303399158, 22.37119938028490296, 42.51126973288290145 ) ) ;
#39750 = DIRECTION ( 'NONE',  ( -0.07906939808003035641, 0.3658060745126643365, 0.9273262350095013984 ) ) ;
#39751 =( BOUNDED_SURFACE ( )  B_SPLINE_SURFACE ( 3, 1, ( 
 ( #43671, #29531 ),
 ( #14231, #712 ),
 ( #58324, #38968 ),
 ( #1021, #38349 ) ),
 .UNSPECIFIED., .F., .F., .F. ) 
 B_SPLINE_SURFACE_WITH_KNOTS ( ( 4, 4 ),
 ( 2, 2 ),
 ( 0.000000000000000000, 1.000000000000000000 ),
 ( 0.000000000000000000, 1.000000000000000000 ),
 .UNSPECIFIED. ) 
 GEOMETRIC_REPRESENTATION_ITEM ( )  RATIONAL_B_SPLINE_SURFACE ( (
 ( 1.000000000000000000, 1.000000000000000000),
 ( 0.7223157951917480446, 0.9931996967497186413),
 ( 0.7223157951917480446, 0.9931996967497186413),
 ( 1.000000000000000000, 1.000000000000000000) ) ) 
 REPRESENTATION_ITEM ( '' )  SURFACE ( )  );
#39752 = CARTESIAN_POINT ( 'NONE',  ( -6.001507490154111224, -14.94036486426005261, -11.48377994779716893 ) ) ;
#39753 = ORIENTED_EDGE ( 'NONE', *, *, #36764, .T. ) ;
#39754 = B_SPLINE_CURVE_WITH_KNOTS ( 'NONE', 3,
 ( #5661, #49526, #26043, #11642 ),
 .UNSPECIFIED., .F., .F.,
 ( 4, 4 ),
 ( 7.589415207398531038E-19, 0.004446298630425091040 ),
 .UNSPECIFIED. ) ;
#39755 = AXIS2_PLACEMENT_3D ( 'NONE', #4900, #9308, #60997 ) ;
#39756 = EDGE_LOOP ( 'NONE', ( #25649, #5839, #21695, #7427 ) ) ;
#39757 = CARTESIAN_POINT ( 'NONE',  ( 0.5827359174754822568, 17.99288944686893643, 44.38786494726102205 ) ) ;
#39758 = CARTESIAN_POINT ( 'NONE',  ( 5.959547316686252039, 19.82530672674362293, -5.315863417546125014 ) ) ;
#39759 = CARTESIAN_POINT ( 'NONE',  ( 0.1129192098497455998, 24.84520063729130612, 36.46461014570008530 ) ) ;
#39760 = CARTESIAN_POINT ( 'NONE',  ( 0.9722240750034586432, -0.5819398758577144504, -42.90442369954358526 ) ) ;
#39761 = CARTESIAN_POINT ( 'NONE',  ( 0.9762797500689124330, -27.44172181261391330, -31.67454323498310842 ) ) ;
#39762 = CARTESIAN_POINT ( 'NONE',  ( 0.9789233960466703355, 38.53168644443766766, 16.48168275935076821 ) ) ;
#39763 = ORIENTED_EDGE ( 'NONE', *, *, #17062, .F. ) ;
#39764 = CARTESIAN_POINT ( 'NONE',  ( 0.5326698147273788431, 5.141974873329280286E-15, 41.88877248453276536 ) ) ;
#39765 = ORIENTED_EDGE ( 'NONE', *, *, #10617, .F. ) ;
#39766 = EDGE_CURVE ( 'NONE', #14707, #26754, #9252, .T. ) ;
#39767 = DIRECTION ( 'NONE',  ( 1.836766033387207149E-16, -1.000000000000000000, 0.000000000000000000 ) ) ;
#39768 = CARTESIAN_POINT ( 'NONE',  ( 5.895596859100789899, -2.016778947467960048, -20.01151633159111043 ) ) ;
#39769 = CARTESIAN_POINT ( 'NONE',  ( -6.078075953587585900, -16.13536320617218323, -10.50929248103985714 ) ) ;
#39770 = CARTESIAN_POINT ( 'NONE',  ( 0.6000166863083106206, -47.36892948402883263, 12.96179004788911726 ) ) ;
#39771 = CARTESIAN_POINT ( 'NONE',  ( 2.301430502907646947, -19.56449039932759959, 43.86847929982153715 ) ) ;
#39772 = EDGE_CURVE ( 'NONE', #3804, #995, #42139, .T. ) ;
#39773 = CARTESIAN_POINT ( 'NONE',  ( 5.895881250540457863, -17.30282815192068924, -10.25377099185475060 ) ) ;
#39774 = CARTESIAN_POINT ( 'NONE',  ( 0.6029442701453591180, 37.33617409675466803, -31.89914307587434550 ) ) ;
#39775 = CARTESIAN_POINT ( 'NONE',  ( -0.2111111111111110827, -9.497654031326126400, 0.000000000000000000 ) ) ;
#39776 = AXIS2_PLACEMENT_3D ( 'NONE', #20982, #54783, #11918 ) ;
#39777 = EDGE_CURVE ( 'NONE', #61467, #44269, #46698, .T. ) ;
#39778 = CARTESIAN_POINT ( 'NONE',  ( 0.1145239942831223490, 29.42216488540841368, 32.88284802386364447 ) ) ;
#39779 = EDGE_CURVE ( 'NONE', #4631, #41953, #60839, .T. ) ;
#39780 = DIRECTION ( 'NONE',  ( 0.000000000000000000, 0.000000000000000000, -1.000000000000000000 ) ) ;
#39781 =( GEOMETRIC_REPRESENTATION_CONTEXT ( 3 ) GLOBAL_UNCERTAINTY_ASSIGNED_CONTEXT ( ( #14202 ) ) GLOBAL_UNIT_ASSIGNED_CONTEXT ( ( #17870, #56669, #51665 ) ) REPRESENTATION_CONTEXT ( 'NONE', 'WORKASPACE' ) );
#39782 = B_SPLINE_CURVE_WITH_KNOTS ( 'NONE', 3,
 ( #51402, #21761, #9122, #46745, #52025, #18857, #42655, #61411, #28228, #56415, #13850, #4390, #61720, #37977, #2325, #3788, #23230, #36190, #8491 ),
 .UNSPECIFIED., .F., .F.,
 ( 4, 3, 3, 3, 3, 3, 4 ),
 ( 1.355252715606880543E-20, 0.0002612768053151653122, 0.0003919133833142877813, 0.0005225499612322621629, 0.0006531865391693346574, 0.0008112755173415177974, 0.0009693688056799715973 ),
 .UNSPECIFIED. ) ;
#39783 = AXIS2_PLACEMENT_3D ( 'NONE', #18449, #5244, #28447 ) ;
#39784 = EDGE_CURVE ( 'NONE', #37845, #13905, #54845, .T. ) ;
#39785 = DIRECTION ( 'NONE',  ( -1.000000000000000000, -3.673819061467147552E-16, 1.925929944387234758E-32 ) ) ;
#39786 = DIRECTION ( 'NONE',  ( 0.1011922191286468153, -0.5266864627877008154, -0.8440151092865576521 ) ) ;
#39787 = CARTESIAN_POINT ( 'NONE',  ( 3.050102900204245682, -19.44795466911843818, -39.46140276733677865 ) ) ;
#39788 = B_SPLINE_CURVE_WITH_KNOTS ( 'NONE', 3,
 ( #11108, #44034, #44330, #53983 ),
 .UNSPECIFIED., .F., .F.,
 ( 4, 4 ),
 ( 3.127317220692750759E-18, 0.004050076154992999014 ),
 .UNSPECIFIED. ) ;
#39789 = CARTESIAN_POINT ( 'NONE',  ( -6.016104459813371719, -18.68131780085933258, 2.464823636987379274 ) ) ;
#39790 = FACE_OUTER_BOUND ( 'NONE', #32026, .T. ) ;
#39791 = B_SPLINE_CURVE_WITH_KNOTS ( 'NONE', 3,
 ( #32599, #32289, #51370, #51685 ),
 .UNSPECIFIED., .F., .F.,
 ( 4, 4 ),
 ( 1.084202172485504434E-19, 0.004444878191957680851 ),
 .UNSPECIFIED. ) ;
#39792 = EDGE_CURVE ( 'NONE', #56157, #52785, #35465, .T. ) ;
#39793 = EDGE_LOOP ( 'NONE', ( #42183, #3577, #60064 ) ) ;
#39794 = CARTESIAN_POINT ( 'NONE',  ( 1.157644175074336923, 24.19453189427239437, 34.22903594751417700 ) ) ;
#39795 = EDGE_CURVE ( 'NONE', #23158, #47724, #44146, .T. ) ;
#39796 = CARTESIAN_POINT ( 'NONE',  ( 0.1103744047535531458, 43.12441516302519773, 0.03874731383746862767 ) ) ;
#39797 = CARTESIAN_POINT ( 'NONE',  ( 0.9757402383260940226, -26.05362288587344821, -34.09320464257837102 ) ) ;
#39798 = CARTESIAN_POINT ( 'NONE',  ( 4.390527457369401532, 40.60156772890515242, 16.78386232616756857 ) ) ;
#39799 = CARTESIAN_POINT ( 'NONE',  ( 0.1073791018717578927, -41.77800844988522755, 10.69234304549982895 ) ) ;
#39800 = ORIENTED_EDGE ( 'NONE', *, *, #815, .F. ) ;
#39801 = DIRECTION ( 'NONE',  ( 0.1011922191286468015, -0.4144321176143268559, -0.9044369268652869831 ) ) ;
#39802 = CARTESIAN_POINT ( 'NONE',  ( 0.6029443199889047422, 28.09514691971974898, -40.27654852906047722 ) ) ;
#39803 = AXIS2_PLACEMENT_3D ( 'NONE', #53881, #21318, #54812 ) ;
#39804 = DIRECTION ( 'NONE',  ( 0.07836865515943411409, -0.7956898808744553575, 0.6006129930017304330 ) ) ;
#39805 = VERTEX_POINT ( 'NONE', #54094 ) ;
#39806 = LINE ( 'NONE', #46259, #17049 ) ;
#39807 = CARTESIAN_POINT ( 'NONE',  ( 2.648799415243696664, 40.32403112341478391, 27.90143324719133844 ) ) ;
#39808 = EDGE_LOOP ( 'NONE', ( #22801, #34369, #24274, #36733 ) ) ;
#39809 = CARTESIAN_POINT ( 'NONE',  ( 1.231276596079881047, -26.41281459480337546, -32.55211200826465756 ) ) ;
#39810 = ORIENTED_EDGE ( 'NONE', *, *, #36019, .T. ) ;
#39811 = VERTEX_POINT ( 'NONE', #34111 ) ;
#39812 = CARTESIAN_POINT ( 'NONE',  ( 0.1145239942831223490, 29.90569479618491755, -32.44371895239680725 ) ) ;
#39813 = CARTESIAN_POINT ( 'NONE',  ( 7.000000000000016875, -56.56854249492331377, -56.56854249492430142 ) ) ;
#39814 = ORIENTED_EDGE ( 'NONE', *, *, #57658, .T. ) ;
#39815 = ADVANCED_FACE ( 'NONE', ( #11216 ), #44508, .F. ) ;
#39816 = ORIENTED_EDGE ( 'NONE', *, *, #32914, .T. ) ;
#39817 = CARTESIAN_POINT ( 'NONE',  ( 0.8751705887134553219, -13.30665218149330364, -46.21789262997752701 ) ) ;
#39818 = CARTESIAN_POINT ( 'NONE',  ( 4.956653778116475451, 47.27023054223744225, 8.845409907520236814 ) ) ;
#39819 = ADVANCED_FACE ( 'NONE', ( #14691 ), #56786, .F. ) ;
#39820 = ORIENTED_EDGE ( 'NONE', *, *, #23271, .F. ) ;
#39821 = ORIENTED_EDGE ( 'NONE', *, *, #11710, .F. ) ;
#39822 = DIRECTION ( 'NONE',  ( 0.1024043820194936449, 0.9139094329506630698, -0.3927886084231606567 ) ) ;
#39823 = CARTESIAN_POINT ( 'NONE',  ( 3.050102900204245682, -36.30976962477565451, -24.84000561541360952 ) ) ;
#39824 = VECTOR ( 'NONE', #49514, 1000.000000000000227 ) ;
#39825 = B_SPLINE_CURVE_WITH_KNOTS ( 'NONE', 3,
 ( #31787, #22075, #60261, #42432 ),
 .UNSPECIFIED., .F., .F.,
 ( 4, 4 ),
 ( 1.734723475976807094E-17, 0.005004948556313830454 ),
 .UNSPECIFIED. ) ;
#39826 = CARTESIAN_POINT ( 'NONE',  ( 0.6027935024548037868, 23.90242449907755784, 41.74929432965625864 ) ) ;
#39827 = CIRCLE ( 'NONE', #36680, 1.000000000000000666 ) ;
#39828 = CARTESIAN_POINT ( 'NONE',  ( 0.5980894510889448457, 34.51330645350402904, -33.52121017007792148 ) ) ;
#39829 = ORIENTED_EDGE ( 'NONE', *, *, #42375, .T. ) ;
#39830 = DIRECTION ( 'NONE',  ( -1.000000000000000000, -1.836909530733573776E-16, 1.925929944387235853E-32 ) ) ;
#39831 = DIRECTION ( 'NONE',  ( 7.985424459127866231E-16, -4.551914400963141816E-15, 1.000000000000000000 ) ) ;
#39832 = EDGE_LOOP ( 'NONE', ( #49396, #29137, #37431, #53538 ) ) ;
#39833 = CARTESIAN_POINT ( 'NONE',  ( 21.00000000000000355, 0.000000000000000000, 0.000000000000000000 ) ) ;
#39834 =( BOUNDED_SURFACE ( )  B_SPLINE_SURFACE ( 3, 1, ( 
 ( #61050, #17852 ),
 ( #18159, #8741 ),
 ( #28157, #51960 ),
 ( #61345, #22850 ) ),
 .UNSPECIFIED., .F., .F., .F. ) 
 B_SPLINE_SURFACE_WITH_KNOTS ( ( 4, 4 ),
 ( 2, 2 ),
 ( 0.000000000000000000, 1.000000000000000000 ),
 ( 0.000000000000000000, 1.000000000000000000 ),
 .UNSPECIFIED. ) 
 GEOMETRIC_REPRESENTATION_ITEM ( )  RATIONAL_B_SPLINE_SURFACE ( (
 ( 1.000000000000000000, 1.000000000000000000),
 ( 0.9953485035131437453, 0.8621029689291523912),
 ( 0.9953485035131437453, 0.8621029689291523912),
 ( 1.000000000000000000, 1.000000000000000000) ) ) 
 REPRESENTATION_ITEM ( '' )  SURFACE ( )  );
#39835 = ORIENTED_EDGE ( 'NONE', *, *, #56096, .F. ) ;
#39836 = CARTESIAN_POINT ( 'NONE',  ( 0.9754402186311939005, 33.92707563620680133, -26.26956909363283543 ) ) ;
#39837 = CARTESIAN_POINT ( 'NONE',  ( 3.660087539127335976, 40.62968541507479614, -25.63019641081286082 ) ) ;
#39838 = ORIENTED_EDGE ( 'NONE', *, *, #56209, .T. ) ;
#39839 = CARTESIAN_POINT ( 'NONE',  ( 0.9790850452238869517, -12.46487240820922793, -40.01205176081654713 ) ) ;
#39840 = CARTESIAN_POINT ( 'NONE',  ( 4.553261556744875094, 0.000000000000000000, 0.000000000000000000 ) ) ;
#39841 = CARTESIAN_POINT ( 'NONE',  ( 50.84822255766327004, 12.21965688190746491, -2.632713613759657623 ) ) ;
#39842 = CARTESIAN_POINT ( 'NONE',  ( -18.65399042163502941, -12.34045889288082343, 1.991456727128138926 ) ) ;
#39843 = AXIS2_PLACEMENT_3D ( 'NONE', #60666, #13094, #17784 ) ;
#39844 = ORIENTED_EDGE ( 'NONE', *, *, #49652, .T. ) ;
#39845 = CARTESIAN_POINT ( 'NONE',  ( 0.3622758884714730732, -22.26738722580142138, -36.91764744403313614 ) ) ;
#39846 = CARTESIAN_POINT ( 'NONE',  ( -6.078075953587585900, 18.62761703674214075, -4.879247665328125372 ) ) ;
#39847 = CARTESIAN_POINT ( 'NONE',  ( 0.9788927965476039716, 41.51561430229724436, -5.726288652754957020 ) ) ;
#39848 = B_SPLINE_CURVE_WITH_KNOTS ( 'NONE', 3,
 ( #8670, #22475, #36911, #32192, #17472, #3048 ),
 .UNSPECIFIED., .F., .F.,
 ( 4, 2, 4 ),
 ( 0.000000000000000000, 0.0002447195606305747461, 0.0004894391212611494922 ),
 .UNSPECIFIED. ) ;
#39849 = EDGE_CURVE ( 'NONE', #5090, #56628, #17480, .T. ) ;
#39850 = FILL_AREA_STYLE_COLOUR ( '', #8702 ) ;
#39851 = CARTESIAN_POINT ( 'NONE',  ( 1.000433927950267421, 20.71612682160601082, 36.43159023655132955 ) ) ;
#39852 = CARTESIAN_POINT ( 'NONE',  ( 0.5549461598389363592, -7.904200586800755879, -43.39056704573498280 ) ) ;
#39853 = AXIS2_PLACEMENT_3D ( 'NONE', #54965, #46767, #41766 ) ;
#39854 = CARTESIAN_POINT ( 'NONE',  ( 0.7044674535453004927, -47.71057267246421674, -11.64061759858214273 ) ) ;
#39855 = EDGE_CURVE ( 'NONE', #57538, #34181, #49414, .T. ) ;
#39856 = EDGE_CURVE ( 'NONE', #21001, #2809, #18262, .T. ) ;
#39857 = CARTESIAN_POINT ( 'NONE',  ( -16.91999570892151539, -7.790225163110376272, 1.821671769791115558 ) ) ;
#39858 = CARTESIAN_POINT ( 'NONE',  ( 5.838029081930957709, 42.14833990873939484, -21.32094043634769776 ) ) ;
#39859 = CARTESIAN_POINT ( 'NONE',  ( 0.2940135542859021456, -26.87228822145753426, 34.98743595112873095 ) ) ;
#39860 = CARTESIAN_POINT ( 'NONE',  ( 0.8744876279028306332, -45.16590161815026505, 19.24555484778404590 ) ) ;
#39861 = CARTESIAN_POINT ( 'NONE',  ( 4.958415959904820092, -39.33684062738397103, 22.71160327406307644 ) ) ;
#39862 = CARTESIAN_POINT ( 'NONE',  ( 0.5832367798473389042, 33.67436043247259647, 34.05962365606829678 ) ) ;
#39863 = CARTESIAN_POINT ( 'NONE',  ( 0.1157991065609915715, 36.93546633102171484, 24.13946338358953980 ) ) ;
#39864 = AXIS2_PLACEMENT_3D ( 'NONE', #54459, #2467, #53842 ) ;
#39865 = ORIENTED_EDGE ( 'NONE', *, *, #30200, .T. ) ;
#39866 = CIRCLE ( 'NONE', #31840, 2.649999999999997691 ) ;
#39867 = CARTESIAN_POINT ( 'NONE',  ( 4.962356264823602814, -33.29728444345256122, -25.73958909062380229 ) ) ;
#39868 = CARTESIAN_POINT ( 'NONE',  ( 4.975801465491695552, -43.22084481528207078, -20.67815041659126862 ) ) ;
#39869 = CARTESIAN_POINT ( 'NONE',  ( 0.8760168074886965917, -24.81951362746107392, 41.20610493656867135 ) ) ;
#39870 = VERTEX_POINT ( 'NONE', #2092 ) ;
#39871 = CARTESIAN_POINT ( 'NONE',  ( 0.1129192098497447394, 39.54191224844646513, -19.58032082273713570 ) ) ;
#39872 = CARTESIAN_POINT ( 'NONE',  ( 0.1152339509894530906, 4.459257806557805459, 43.89826545855652284 ) ) ;
#39873 = CARTESIAN_POINT ( 'NONE',  ( 0.7764146366350230810, -14.74570993613317427, -44.52644733356332551 ) ) ;
#39874 = PRODUCT_DEFINITION_CONTEXT ( 'detailed design', #60057, 'design' ) ;
#39875 = ORIENTED_EDGE ( 'NONE', *, *, #9451, .F. ) ;
#39876 = ORIENTED_EDGE ( 'NONE', *, *, #36666, .T. ) ;
#39877 = CARTESIAN_POINT ( 'NONE',  ( -6.078457390727109555, -8.910533588204446076, 17.07035155499113444 ) ) ;
#39878 = ORIENTED_EDGE ( 'NONE', *, *, #24223, .F. ) ;
#39879 = CARTESIAN_POINT ( 'NONE',  ( 0.6026112563231247332, 10.75757372951007973, 47.91467001199488607 ) ) ;
#39880 = ORIENTED_EDGE ( 'NONE', *, *, #7037, .T. ) ;
#39881 = ORIENTED_EDGE ( 'NONE', *, *, #22081, .F. ) ;
#39882 = CARTESIAN_POINT ( 'NONE',  ( 3.783278058412226752, -41.98530666033908432, -9.462251542474252375 ) ) ;
#39883 = ORIENTED_EDGE ( 'NONE', *, *, #49575, .T. ) ;
#39884 = CARTESIAN_POINT ( 'NONE',  ( 3.680974057930773924, 47.77138393978996334, -4.423547572561821184 ) ) ;
#39885 = CARTESIAN_POINT ( 'NONE',  ( 0.9730545539215883499, 5.099196237955498923, -42.60426903087348194 ) ) ;
#39886 = ORIENTED_EDGE ( 'NONE', *, *, #54788, .F. ) ;
#39887 = CARTESIAN_POINT ( 'NONE',  ( 0.1103573494271547495, 0.06145187104178059107, 43.12440049163654976 ) ) ;
#39888 = EDGE_CURVE ( 'NONE', #4699, #37185, #59735, .T. ) ;
#39889 = DIRECTION ( 'NONE',  ( 0.07439287786467665975, 0.9262902123089796769, -0.3693942911085615899 ) ) ;
#39890 = VECTOR ( 'NONE', #51976, 1000.000000000000114 ) ;
#39891 = ORIENTED_EDGE ( 'NONE', *, *, #61049, .T. ) ;
#39892 = CARTESIAN_POINT ( 'NONE',  ( 3.240649175237395596, 34.65332694999099772, -27.10003410873642693 ) ) ;
#39893 = B_SPLINE_CURVE_WITH_KNOTS ( 'NONE', 3,
 ( #6529, #26287, #11592, #2150 ),
 .UNSPECIFIED., .F., .F.,
 ( 4, 4 ),
 ( 6.992893892674702526E-18, 0.004042984057420969356 ),
 .UNSPECIFIED. ) ;
#39894 = CARTESIAN_POINT ( 'NONE',  ( 0.1129192098497455998, 10.29049805561888498, -42.90754522869442411 ) ) ;
#39895 = CARTESIAN_POINT ( 'NONE',  ( 0.8554163680231738898, 11.76336166872350475, -45.41837508500966436 ) ) ;
#39896 = CARTESIAN_POINT ( 'NONE',  ( 0.1073791018717578927, 0.4849339620933161288, -43.12183934961191056 ) ) ;
#39897 = EDGE_LOOP ( 'NONE', ( #54927, #42327, #61704, #8794, #46135 ) ) ;
#39898 = ORIENTED_EDGE ( 'NONE', *, *, #31728, .F. ) ;
#39899 = CARTESIAN_POINT ( 'NONE',  ( -6.078457390727109555, 17.84708778612959890, -7.230212209312498750 ) ) ;
#39900 = CARTESIAN_POINT ( 'NONE',  ( 0.6845945791218023269, -14.72268806499601901, -44.53817437721004069 ) ) ;
#39901 = ORIENTED_EDGE ( 'NONE', *, *, #51450, .F. ) ;
#39902 = CARTESIAN_POINT ( 'NONE',  ( 3.894904216938898323, -43.02812409911978619, -8.983588870098012436 ) ) ;
#39903 = CARTESIAN_POINT ( 'NONE',  ( 0.5997462898726536595, 48.09935696025624452, 9.899671214447447909 ) ) ;
#39904 = CARTESIAN_POINT ( 'NONE',  ( 5.838029081930957709, -47.23414715677122899, 0.02001313068585724997 ) ) ;
#39905 = CARTESIAN_POINT ( 'NONE',  ( 4.967162193818129623, -40.65506779172174845, 14.26841313271267886 ) ) ;
#39906 = CIRCLE ( 'NONE', #5859, 4.250000000000000000 ) ;
#39907 = CONICAL_SURFACE ( 'NONE', #61849, 4.000000000000000000, 1.047197551196595855 ) ;
#39908 = VERTEX_POINT ( 'NONE', #50638 ) ;
#39909 = VERTEX_POINT ( 'NONE', #30608 ) ;
#39910 = DIRECTION ( 'NONE',  ( 0.000000000000000000, 1.000000000000000000, 0.000000000000000000 ) ) ;
#39911 = CARTESIAN_POINT ( 'NONE',  ( 0.1084644655670282815, 34.45367667780531917, 25.93599432281509820 ) ) ;
#39912 = CARTESIAN_POINT ( 'NONE',  ( 0.9740398440564319582, -16.03656236596777873, 39.79907313245126232 ) ) ;
#39913 = EDGE_CURVE ( 'NONE', #23672, #39035, #56293, .T. ) ;
#39914 = CARTESIAN_POINT ( 'NONE',  ( -2.708315649062916552, 3.532515819624345799, -14.20182604343557031 ) ) ;
#39915 = CARTESIAN_POINT ( 'NONE',  ( 0.2940135542859014794, 15.98885814221885937, 41.11686957927879149 ) ) ;
#39916 = EDGE_CURVE ( 'NONE', #43148, #38326, #39133, .T. ) ;
#39917 = B_SPLINE_CURVE_WITH_KNOTS ( 'NONE', 3,
 ( #16463, #61131, #25858, #54652 ),
 .UNSPECIFIED., .F., .F.,
 ( 4, 4 ),
 ( 0.000000000000000000, 0.004444103432399267029 ),
 .UNSPECIFIED. ) ;
#39918 = B_SPLINE_CURVE_WITH_KNOTS ( 'NONE', 3,
 ( #45005, #40612, #54661, #2040 ),
 .UNSPECIFIED., .F., .F.,
 ( 4, 4 ),
 ( 0.000000000000000000, 0.005013413432710143308 ),
 .UNSPECIFIED. ) ;
#39919 = CARTESIAN_POINT ( 'NONE',  ( 0.8753041380234465318, 16.12068986424767658, 46.38169559399183584 ) ) ;
#39920 = CARTESIAN_POINT ( 'NONE',  ( 0.5807400328401574052, -44.45848844984429604, -17.82553128098455630 ) ) ;
#39921 = FACE_OUTER_BOUND ( 'NONE', #6489, .T. ) ;
#39922 = EDGE_CURVE ( 'NONE', #8036, #31957, #7727, .T. ) ;
#39923 = FACE_OUTER_BOUND ( 'NONE', #23770, .T. ) ;
#39924 = CARTESIAN_POINT ( 'NONE',  ( 0.6031356219577718170, -6.192730535896502353, 47.70727206974374468 ) ) ;
#39925 = VECTOR ( 'NONE', #35736, 1000.000000000000227 ) ;
#39926 = EDGE_CURVE ( 'NONE', #20551, #9409, #37672, .T. ) ;
#39927 = FACE_OUTER_BOUND ( 'NONE', #13781, .T. ) ;
#39928 = DIRECTION ( 'NONE',  ( 0.000000000000000000, 1.000000000000000000, 0.000000000000000000 ) ) ;
#39929 = CARTESIAN_POINT ( 'NONE',  ( 5.896782393890504181, 14.92098591823861220, 13.48666994130638663 ) ) ;
#39930 = CARTESIAN_POINT ( 'NONE',  ( 0.8554163680231720024, -34.17638377241251391, 32.14312158693672217 ) ) ;
#39931 = CARTESIAN_POINT ( 'NONE',  ( 0.6009453534118440743, -46.57942464365182644, 12.02914401651092113 ) ) ;
#39932 = CARTESIAN_POINT ( 'NONE',  ( 0.8551540677456715978, 47.37911285756620572, 7.157691013574528860 ) ) ;
#39933 = ITEM_DEFINED_TRANSFORMATION ( 'NONE', 'NONE', #4863,  #14677 ) ;
#39934 = CARTESIAN_POINT ( 'NONE',  ( 0.9749527285493297946, -26.34702925571524545, 33.86694354778348526 ) ) ;
#39935 = AXIS2_PLACEMENT_3D ( 'NONE', #14035, #15872, #2045 ) ;
#39936 = CARTESIAN_POINT ( 'NONE',  ( 0.1103936448916684188, -0.03072591687012675085, -43.12443171339901227 ) ) ;
#39937 = CARTESIAN_POINT ( 'NONE',  ( 0.7948878604505646983, 23.47568002599128434, 43.12297641183513974 ) ) ;
#39938 = CARTESIAN_POINT ( 'NONE',  ( 0.6026112563231247332, 49.01739703219963928, -2.972504515036971551 ) ) ;
#39940 = ORIENTED_EDGE ( 'NONE', *, *, #12473, .F. ) ;
#39939 = LINE ( 'NONE', #52761, #15355 ) ;
#39941 = ORIENTED_EDGE ( 'NONE', *, *, #28205, .F. ) ;
#39942 = EDGE_CURVE ( 'NONE', #24195, #26516, #40697, .T. ) ;
#39943 = CARTESIAN_POINT ( 'NONE',  ( 1.657374760986086271, 43.86835707583708199, -4.056808440030005514 ) ) ;
#39944 = CARTESIAN_POINT ( 'NONE',  ( 3.238741278300274917, -35.19027457370196288, 24.69738534405251329 ) ) ;
#39945 = ORIENTED_EDGE ( 'NONE', *, *, #46886, .T. ) ;
#39946 = ADVANCED_FACE ( 'NONE', ( #59421 ), #54771, .F. ) ;
#39947 = VERTEX_POINT ( 'NONE', #21223 ) ;
#39948 = DIRECTION ( 'NONE',  ( 0.000000000000000000, 0.000000000000000000, 1.000000000000000000 ) ) ;
#39949 = CARTESIAN_POINT ( 'NONE',  ( -6.057079549204054558, -4.293366707802514171, 18.77227299535331539 ) ) ;
#39950 = CARTESIAN_POINT ( 'NONE',  ( 0.5998501479064708430, 5.759754759340140140, 47.76154736470759588 ) ) ;
#39951 = ORIENTED_EDGE ( 'NONE', *, *, #22995, .T. ) ;
#39952 = EDGE_LOOP ( 'NONE', ( #10857, #14364, #33128, #24297 ) ) ;
#39953 =( BOUNDED_SURFACE ( )  B_SPLINE_SURFACE ( 3, 1, ( 
 ( #9420, #48801 ),
 ( #48486, #33258 ),
 ( #61713, #13526 ),
 ( #3783, #32631 ) ),
 .UNSPECIFIED., .F., .F., .F. ) 
 B_SPLINE_SURFACE_WITH_KNOTS ( ( 4, 4 ),
 ( 2, 2 ),
 ( 0.000000000000000000, 1.000000000000000000 ),
 ( 0.000000000000000000, 1.000000000000000000 ),
 .UNSPECIFIED. ) 
 GEOMETRIC_REPRESENTATION_ITEM ( )  RATIONAL_B_SPLINE_SURFACE ( (
 ( 1.000000000000000000, 1.000000000000000000),
 ( 0.9952954269826590483, 0.8620686068821307169),
 ( 0.9952954269826590483, 0.8620686068821307169),
 ( 1.000000000000000000, 1.000000000000000000) ) ) 
 REPRESENTATION_ITEM ( '' )  SURFACE ( )  );
#39954 = CARTESIAN_POINT ( 'NONE',  ( 3.407937589446174087, -3.099921468254910106, -13.34359005742692617 ) ) ;
#39955 = VECTOR ( 'NONE', #8433, 1000.000000000000000 ) ;
#39956 = CARTESIAN_POINT ( 'NONE',  ( -1.200000000000006617, 0.000000000000000000, 0.000000000000000000 ) ) ;
#39957 = CARTESIAN_POINT ( 'NONE',  ( 0.8744876279028306332, -0.6840263623749832655, 49.09055060105833235 ) ) ;
#39958 = B_SPLINE_CURVE_WITH_KNOTS ( 'NONE', 3,
 ( #30165, #10775, #19561, #44609 ),
 .UNSPECIFIED., .F., .F.,
 ( 4, 4 ),
 ( 0.000000000000000000, 0.004445488388166993383 ),
 .UNSPECIFIED. ) ;
#39959 = CARTESIAN_POINT ( 'NONE',  ( -6.077587904424778920, -19.21610359950803115, -1.239912838430589970 ) ) ;
#39960 = ORIENTED_EDGE ( 'NONE', *, *, #51332, .T. ) ;
#39961 = CARTESIAN_POINT ( 'NONE',  ( 0.5782707292762423457, 5.414380361654348661, 46.58777563918405917 ) ) ;
#39962 = DIRECTION ( 'NONE',  ( 0.000000000000000000, 0.000000000000000000, -1.000000000000000000 ) ) ;
#39963 = ADVANCED_FACE ( 'NONE', ( #16528 ), #8067, .F. ) ;
#39964 = B_SPLINE_CURVE_WITH_KNOTS ( 'NONE', 3,
 ( #7759, #29044, #14342, #9620 ),
 .UNSPECIFIED., .F., .F.,
 ( 4, 4 ),
 ( 6.254634441385501517E-18, 0.004566006591234645501 ),
 .UNSPECIFIED. ) ;
#39965 = AXIS2_PLACEMENT_3D ( 'NONE', #11530, #35350, #1181 ) ;
#39966 = CARTESIAN_POINT ( 'NONE',  ( 0.1129192098497455998, 15.69290830752535726, -41.23935519181593889 ) ) ;
#39967 = ORIENTED_EDGE ( 'NONE', *, *, #6532, .F. ) ;
#39968 = ORIENTED_EDGE ( 'NONE', *, *, #38166, .F. ) ;
#39969 = CARTESIAN_POINT ( 'NONE',  ( 4.962356264823608143, 34.44911810793244200, 24.17630781256866612 ) ) ;
#39970 = DIRECTION ( 'NONE',  ( 0.9848077530122079093, 0.1736481776669314414, -5.551115123125783935E-17 ) ) ;
#39971 = AXIS2_PLACEMENT_3D ( 'NONE', #5332, #34190, #14466 ) ;
#39972 = ORIENTED_EDGE ( 'NONE', *, *, #37375, .T. ) ;
#39973 = CARTESIAN_POINT ( 'NONE',  ( 0.5836750258453368145, 44.31929073742215763, -18.16108240858296696 ) ) ;
#39974 = DIRECTION ( 'NONE',  ( 1.000000000000000000, 1.836970198721027962E-16, -2.033782021272921061E-31 ) ) ;
#39975 = CARTESIAN_POINT ( 'NONE',  ( 43.00000000000000000, 0.000000000000000000, 0.000000000000000000 ) ) ;
#39976 = CARTESIAN_POINT ( 'NONE',  ( 3.782625744892851749, 41.85823871763314230, 3.889210145086195336 ) ) ;
#39977 = ORIENTED_EDGE ( 'NONE', *, *, #18541, .F. ) ;
#39978 = CARTESIAN_POINT ( 'NONE',  ( 0.5837800304671220131, -13.93760103191574196, 44.77700983378232280 ) ) ;
#39979 = CARTESIAN_POINT ( 'NONE',  ( 2.282816707992324723, 46.36091564783490071, -7.560586399367689836 ) ) ;
#39980 = CARTESIAN_POINT ( 'NONE',  ( 4.960386119450148179, -26.33153931528526925, 34.94404816216813714 ) ) ;
#39981 = ORIENTED_EDGE ( 'NONE', *, *, #9824, .F. ) ;
#39982 = DIRECTION ( 'NONE',  ( 0.000000000000000000, -1.000000000000000000, -0.000000000000000000 ) ) ;
#39983 = CARTESIAN_POINT ( 'NONE',  ( 5.838029081930957709, -28.00222738077776796, 38.03866874468847215 ) ) ;
#39984 = VERTEX_POINT ( 'NONE', #45664 ) ;
#39985 = CARTESIAN_POINT ( 'NONE',  ( 0.7057020205114996614, 33.27137945725718282, 34.46103118762803064 ) ) ;
#39986 = CARTESIAN_POINT ( 'NONE',  ( 0.1156867017252034419, 9.696689235465189682, 43.04552270731533525 ) ) ;
#39987 = EDGE_LOOP ( 'NONE', ( #20621, #7242 ) ) ;
#39988 = FACE_OUTER_BOUND ( 'NONE', #24498, .T. ) ;
#39989 = DIRECTION ( 'NONE',  ( -0.1024043820194934645, -0.4859385467930338875, -0.8679729669084632615 ) ) ;
#39990 = CARTESIAN_POINT ( 'NONE',  ( 4.975610109902397937, 13.36434394399761949, -47.05150069959838532 ) ) ;
#39991 = B_SPLINE_CURVE_WITH_KNOTS ( 'NONE', 3,
 ( #53387, #23668, #42795, #14906 ),
 .UNSPECIFIED., .F., .F.,
 ( 4, 4 ),
 ( 0.000000000000000000, 0.005013413432710138104 ),
 .UNSPECIFIED. ) ;
#39992 = CARTESIAN_POINT ( 'NONE',  ( 2.533389852662419894, 21.74902146992863905, 38.26787943999772779 ) ) ;
#39993 = CIRCLE ( 'NONE', #32958, 43.08621763946400307 ) ;
#39994 = CARTESIAN_POINT ( 'NONE',  ( 4.834790513006553603, -47.18049212391683511, 2.567197668549032308 ) ) ;
#39995 = DIRECTION ( 'NONE',  ( 0.000000000000000000, 0.000000000000000000, -1.000000000000000000 ) ) ;
#39996 = CARTESIAN_POINT ( 'NONE',  ( 0.1097557419366048670, -41.71221507312540666, -10.94578341459255633 ) ) ;
#39998 = EDGE_CURVE ( 'NONE', #51084, #45511, #15273, .T. ) ;
#39997 = DIRECTION ( 'NONE',  ( -1.000000000000000000, 0.000000000000000000, 0.000000000000000000 ) ) ;
#39999 = FACE_BOUND ( 'NONE', #37643, .T. ) ;
#40000 = CARTESIAN_POINT ( 'NONE',  ( 0.9788927965476018622, 15.19445284419454012, 39.05720439813027411 ) ) ;
#40001 = ORIENTED_EDGE ( 'NONE', *, *, #61664, .F. ) ;
#40002 = EDGE_CURVE ( 'NONE', #38122, #20520, #244, .T. ) ;
#40003 = CARTESIAN_POINT ( 'NONE',  ( 0.7246131072078557667, -0.8205838906006461819, 48.09507913767665599 ) ) ;
#40004 = DIRECTION ( 'NONE',  ( -1.000000000000000000, -0.000000000000000000, -0.000000000000000000 ) ) ;
#40005 = CARTESIAN_POINT ( 'NONE',  ( 0.5800708119828332787, -13.00144522946626324, -46.09746484493492602 ) ) ;
#40006 = DIRECTION ( 'NONE',  ( -1.000000000000000000, -5.380183451256670742E-17, 1.298891185607911324E-16 ) ) ;
#40007 = CARTESIAN_POINT ( 'NONE',  ( 5.959828726073459926, 19.82504517499705443, 5.316791119501156793 ) ) ;
#40008 = FACE_OUTER_BOUND ( 'NONE', #48225, .T. ) ;
#40009 = EDGE_CURVE ( 'NONE', #2478, #19981, #7622, .T. ) ;
#40010 = DIRECTION ( 'NONE',  ( 7.112851796247055846E-15, -0.7071067811865389130, -0.7071067811865561215 ) ) ;
#40011 = CARTESIAN_POINT ( 'NONE',  ( 4.958415959904821868, 37.73202888843214708, 25.28829669600464669 ) ) ;
#40012 =( BOUNDED_SURFACE ( )  B_SPLINE_SURFACE ( 3, 1, ( 
 ( #60409, #50712 ),
 ( #60119, #55408 ),
 ( #40137, #6860 ),
 ( #17527, #8117 ) ),
 .UNSPECIFIED., .F., .F., .F. ) 
 B_SPLINE_SURFACE_WITH_KNOTS ( ( 4, 4 ),
 ( 2, 2 ),
 ( 0.000000000000000000, 1.000000000000000000 ),
 ( 0.000000000000000000, 1.000000000000000000 ),
 .UNSPECIFIED. ) 
 GEOMETRIC_REPRESENTATION_ITEM ( )  RATIONAL_B_SPLINE_SURFACE ( (
 ( 1.000000000000000000, 1.000000000000000000),
 ( 0.7282232189291693025, 0.9929344683865674037),
 ( 0.7282232189291693025, 0.9929344683865674037),
 ( 1.000000000000000000, 1.000000000000000000) ) ) 
 REPRESENTATION_ITEM ( '' )  SURFACE ( )  );
#40013 = CARTESIAN_POINT ( 'NONE',  ( 3.270143674763207553, 3.806843787666105428, -13.14781761974165164 ) ) ;
#40014 = CARTESIAN_POINT ( 'NONE',  ( 4.833616638992205949, 41.27831852777612198, 20.86133030530305632 ) ) ;
#40016 = ORIENTED_EDGE ( 'NONE', *, *, #19477, .F. ) ;
#40015 = CARTESIAN_POINT ( 'NONE',  ( 4.322998006666165516, 20.30542865297649158, -43.48102276965681767 ) ) ;
#40017 = ORIENTED_EDGE ( 'NONE', *, *, #21075, .F. ) ;
#40019 = AXIS2_PLACEMENT_3D ( 'NONE', #39150, #43855, #33823 ) ;
#40018 = CARTESIAN_POINT ( 'NONE',  ( 4.335381028904201628, -3.692956800737033696, 48.84791620665343004 ) ) ;
#40020 = B_SPLINE_CURVE_WITH_KNOTS ( 'NONE', 3,
 ( #11386, #54263, #2584, #45849, #30469, #40531 ),
 .UNSPECIFIED., .F., .F.,
 ( 4, 2, 4 ),
 ( 8.510565793060200234E-17, 0.0002293366620881441987, 0.0004586733241762032875 ),
 .UNSPECIFIED. ) ;
#40021 = CARTESIAN_POINT ( 'NONE',  ( 4.553261556744873317, -3.993093339917161977, 43.74465420371208069 ) ) ;
#40022 = CARTESIAN_POINT ( 'NONE',  ( 4.975610109902397937, -27.50982196586548412, -40.44328253918266824 ) ) ;
#40023 = EDGE_CURVE ( 'NONE', #29392, #51504, #58631, .T. ) ;
#40024 = ORIENTED_EDGE ( 'NONE', *, *, #31728, .T. ) ;
#40025 = CARTESIAN_POINT ( 'NONE',  ( 0.1152339509894530906, -22.68230489146504425, 37.84779696714015529 ) ) ;
#40026 = CARTESIAN_POINT ( 'NONE',  ( 0.5809828226811548646, -47.41188724015884048, 6.791453954330148868 ) ) ;
#40027 = CARTESIAN_POINT ( 'NONE',  ( -6.016761891674565099, -14.95139917749712488, 11.46828378093553980 ) ) ;
#40028 =( BOUNDED_SURFACE ( )  B_SPLINE_SURFACE ( 3, 1, ( 
 ( #57588, #20047 ),
 ( #34449, #53522 ),
 ( #38855, #49148 ),
 ( #29114, #15036 ) ),
 .UNSPECIFIED., .F., .F., .F. ) 
 B_SPLINE_SURFACE_WITH_KNOTS ( ( 4, 4 ),
 ( 2, 2 ),
 ( 0.000000000000000000, 1.000000000000000000 ),
 ( 0.000000000000000000, 1.000000000000000000 ),
 .UNSPECIFIED. ) 
 GEOMETRIC_REPRESENTATION_ITEM ( )  RATIONAL_B_SPLINE_SURFACE ( (
 ( 1.000000000000000000, 1.000000000000000000),
 ( 0.9953390228620291325, 0.8624445117761032620),
 ( 0.9953390228620291325, 0.8624445117761032620),
 ( 1.000000000000000000, 1.000000000000000000) ) ) 
 REPRESENTATION_ITEM ( '' )  SURFACE ( )  );
#40029 = EDGE_LOOP ( 'NONE', ( #45649, #9392, #58201, #3528 ) ) ;
#40030 = ORIENTED_EDGE ( 'NONE', *, *, #49512, .T. ) ;
#40031 = CARTESIAN_POINT ( 'NONE',  ( 1.231276596079887264, 29.74482033789320568, 29.53849072116790353 ) ) ;
#40032 = CARTESIAN_POINT ( 'NONE',  ( 0.1097557419366048670, -39.92664986079722667, -16.29667732266738867 ) ) ;
#40033 = DIRECTION ( 'NONE',  ( 0.000000000000000000, 0.000000000000000000, 1.000000000000000000 ) ) ;
#40034 = VERTEX_POINT ( 'NONE', #27461 ) ;
#40035 = B_SPLINE_CURVE_WITH_KNOTS ( 'NONE', 3,
 ( #55755, #17881, #13184, #42010, #17261, #51675, #3744, #18185, #27571, #32283, #13488, #61072, #50452, #40786, #50751, #8447 ),
 .UNSPECIFIED., .F., .F.,
 ( 4, 3, 3, 3, 3, 4 ),
 ( 1.127622383284612036E-17, 0.0002724568934985560891, 0.0004086836638483819901, 0.0005449104342063619587, 0.0008173270854453694922, 0.001089761613562688575 ),
 .UNSPECIFIED. ) ;
#40036 = CARTESIAN_POINT ( 'NONE',  ( 1.000433927950263424, -27.55767315202177414, -31.57520115690769913 ) ) ;
#40037 = DIRECTION ( 'NONE',  ( 0.000000000000000000, 0.000000000000000000, 1.000000000000000000 ) ) ;
#40038 = B_SPLINE_CURVE_WITH_KNOTS ( 'NONE', 3,
 ( #19469, #23533, #48277, #8821 ),
 .UNSPECIFIED., .F., .F.,
 ( 4, 4 ),
 ( 0.000000000000000000, 0.004447772540403792906 ),
 .UNSPECIFIED. ) ;
#40039 = ORIENTED_EDGE ( 'NONE', *, *, #33615, .T. ) ;
#40040 = B_SPLINE_CURVE_WITH_KNOTS ( 'NONE', 3,
 ( #14556, #23326, #61510, #24239 ),
 .UNSPECIFIED., .F., .F.,
 ( 4, 4 ),
 ( 2.180944827630287554E-17, 0.004564976165746189446 ),
 .UNSPECIFIED. ) ;
#40041 = CARTESIAN_POINT ( 'NONE',  ( 0.6000166863083106206, -14.47337940799656586, -46.92914627628159252 ) ) ;
#40042 = CARTESIAN_POINT ( 'NONE',  ( 0.9752132459055868896, 41.38545930839060816, -11.33038172416108935 ) ) ;
#40043 = ORIENTED_EDGE ( 'NONE', *, *, #4718, .T. ) ;
#40044 = DIRECTION ( 'NONE',  ( 0.000000000000000000, 0.000000000000000000, -1.000000000000000000 ) ) ;
#40046 = CARTESIAN_POINT ( 'NONE',  ( 5.981074661064941900, 19.82752479807527379, -5.303881226583471609 ) ) ;
#40045 = VECTOR ( 'NONE', #61567, 1000.000000000000000 ) ;
#40047 = ORIENTED_EDGE ( 'NONE', *, *, #41124, .F. ) ;
#40048 = CARTESIAN_POINT ( 'NONE',  ( -6.078726893082806448, 3.069885851706299462, 19.00973019603943825 ) ) ;
#40049 = CARTESIAN_POINT ( 'NONE',  ( 2.282803330402963571, -31.31874722888088058, 35.00904139605154342 ) ) ;
#40050 = CARTESIAN_POINT ( 'NONE',  ( 0.5819845079324655890, 41.25022834067384281, -24.34013310064351998 ) ) ;
#40051 = FILL_AREA_STYLE ('',( #16838 ) ) ;
#40052 = ADVANCED_FACE ( 'NONE', ( #4250 ), #24790, .F. ) ;
#40053 = VERTEX_POINT ( 'NONE', #60648 ) ;
#40054 = EDGE_CURVE ( 'NONE', #7870, #49156, #54064, .T. ) ;
#40055 = CARTESIAN_POINT ( 'NONE',  ( 4.975801465491695552, 0.000000000000000000, 0.000000000000000000 ) ) ;
#40056 = CARTESIAN_POINT ( 'NONE',  ( 0.7764146366350229700, -18.93147413529521828, 42.91433048218058843 ) ) ;
#40057 = ORIENTED_EDGE ( 'NONE', *, *, #38718, .F. ) ;
#40058 = CARTESIAN_POINT ( 'NONE',  ( 0.1073791018717578927, -30.83464511437158961, 30.14884492832337060 ) ) ;
#40059 = ORIENTED_EDGE ( 'NONE', *, *, #21148, .T. ) ;
#40060 = CARTESIAN_POINT ( 'NONE',  ( 5.959828726073459926, -5.308046411395388020, 19.82738831247204203 ) ) ;
#40061 = EDGE_CURVE ( 'NONE', #885, #43681, #28671, .T. ) ;
#40062 = ORIENTED_EDGE ( 'NONE', *, *, #31857, .F. ) ;
#40063 = CARTESIAN_POINT ( 'NONE',  ( 4.962356264823603702, -40.70360067759225586, -10.69824704058845022 ) ) ;
#40064 = DIRECTION ( 'NONE',  ( 0.1736481776669314969, -0.9848077530122079093, -4.496403249731880833E-15 ) ) ;
#40065 = VECTOR ( 'NONE', #3053, 1000.000000000000227 ) ;
#40066 = CARTESIAN_POINT ( 'NONE',  ( 5.896782393890504181, 19.71107130340470448, 3.999969368646206558 ) ) ;
#40067 = ORIENTED_EDGE ( 'NONE', *, *, #50212, .T. ) ;
#40068 = CARTESIAN_POINT ( 'NONE',  ( 4.833616638992208614, 30.83411269743515959, 34.47248434257923577 ) ) ;
#40069 = CARTESIAN_POINT ( 'NONE',  ( 0.5832367798473389042, -6.521664418777500138, 47.44985149964048077 ) ) ;
#40070 = DIRECTION ( 'NONE',  ( 0.000000000000000000, 0.000000000000000000, 1.000000000000000000 ) ) ;
#40071 = ORIENTED_EDGE ( 'NONE', *, *, #6790, .F. ) ;
#40072 = VERTEX_POINT ( 'NONE', #28386 ) ;
#40073 = CARTESIAN_POINT ( 'NONE',  ( 0.5819845079324649229, 18.74766465427224915, 44.07435181061346441 ) ) ;
#40074 = CARTESIAN_POINT ( 'NONE',  ( -6.077587904424778920, -18.90214787454608469, 3.674891443665150970 ) ) ;
#40075 = CARTESIAN_POINT ( 'NONE',  ( 0.6026112563231247332, 32.88584477487121660, 36.47001793730409247 ) ) ;
#40076 = CARTESIAN_POINT ( 'NONE',  ( 0.1103310638050662290, 30.43528225250897989, 30.55179781598007338 ) ) ;
#40077 = LINE ( 'NONE', #42150, #31574 ) ;
#40078 = CARTESIAN_POINT ( 'NONE',  ( 0.6000166863083090663, 40.87138819217380359, -27.22780029589407036 ) ) ;
#40079 = EDGE_LOOP ( 'NONE', ( #40411, #60133, #38960, #23378 ) ) ;
#40080 = EDGE_CURVE ( 'NONE', #55180, #50728, #43717, .T. ) ;
#40081 = CARTESIAN_POINT ( 'NONE',  ( 1.091591847532196624, -40.91128483460986587, -9.111847460162190160 ) ) ;
#40082 = CARTESIAN_POINT ( 'NONE',  ( 2.301529144917015657, 13.67115311793999943, 46.04684498357985944 ) ) ;
#40083 = EDGE_LOOP ( 'NONE', ( #2912, #11623, #11502, #50657 ) ) ;
#40084 = ADVANCED_FACE ( 'NONE', ( #27158 ), #31186, .F. ) ;
#40085 = CARTESIAN_POINT ( 'NONE',  ( 4.975801465491694664, -14.85979367497141546, -45.55012473237748338 ) ) ;
#40086 = CARTESIAN_POINT ( 'NONE',  ( 47.85000000000001563, 15.50000000000001243, 0.1751081065780700774 ) ) ;
#40087 = CARTESIAN_POINT ( 'NONE',  ( 0.5837799406558229487, 45.25381588408496469, 12.30185748196357487 ) ) ;
#40088 = CARTESIAN_POINT ( 'NONE',  ( 4.335381028904216727, 12.96255624111825888, 47.24117889469092546 ) ) ;
#40089 = CARTESIAN_POINT ( 'NONE',  ( 2.533389852662419894, 11.33089370753568303, 42.53306219310039182 ) ) ;
#40090 = ADVANCED_FACE ( 'NONE', ( #1399, #47822 ), #20539, .T. ) ;
#40091 = CARTESIAN_POINT ( 'NONE',  ( 0.8554163680231720024, 40.82560365045065964, 23.11872746688557712 ) ) ;
#40092 = CARTESIAN_POINT ( 'NONE',  ( 1.827119703190777988, -43.03226500438893964, 1.232688548475876500 ) ) ;
#40093 = CARTESIAN_POINT ( 'NONE',  ( 0.5800708119828329457, -5.628966929618073323, 47.56394195701285810 ) ) ;
#40094 = CARTESIAN_POINT ( 'NONE',  ( 5.960221823109900008, -20.52559243573973546, 0.005450390361653345561 ) ) ;
#40095 = B_SPLINE_CURVE_WITH_KNOTS ( 'NONE', 3,
 ( #9337, #57861, #5238, #4609 ),
 .UNSPECIFIED., .F., .F.,
 ( 4, 4 ),
 ( 0.000000000000000000, 0.004447772540403798977 ),
 .UNSPECIFIED. ) ;
#40096 = CARTESIAN_POINT ( 'NONE',  ( 0.8760168074887076939, 46.22580377597785883, -13.30888447662032625 ) ) ;
#40097 = CARTESIAN_POINT ( 'NONE',  ( -6.010958268070873523, -14.94067681728557950, 11.48268200989191534 ) ) ;
#40098 = DIRECTION ( 'NONE',  ( 0.000000000000000000, 0.000000000000000000, -1.000000000000000000 ) ) ;
#40100 = ADVANCED_FACE ( 'NONE', ( #52804 ), #31674, .F. ) ;
#40099 = B_SPLINE_CURVE_WITH_KNOTS ( 'NONE', 3,
 ( #16568, #50081, #15960, #59784 ),
 .UNSPECIFIED., .F., .F.,
 ( 4, 4 ),
 ( 2.409784148528075715E-17, 0.004564976165746189446 ),
 .UNSPECIFIED. ) ;
#40101 = CARTESIAN_POINT ( 'NONE',  ( -6.015611763856276717, -18.68122482568281839, 2.465697960550983225 ) ) ;
#40102 = CARTESIAN_POINT ( 'NONE',  ( 4.967162193818130511, -42.96271701169384016, -3.259922920618186115 ) ) ;
#40103 = VECTOR ( 'NONE', #37633, 1000.000000000000114 ) ;
#40104 = ORIENTED_EDGE ( 'NONE', *, *, #16476, .T. ) ;
#40105 = CARTESIAN_POINT ( 'NONE',  ( 2.282816707992305183, 33.58715780361674774, 32.83899811326333662 ) ) ;
#40106 =( BOUNDED_SURFACE ( )  B_SPLINE_SURFACE ( 3, 1, ( 
 ( #40027, #59078 ),
 ( #16190, #35303 ),
 ( #30575, #59697 ),
 ( #6744, #25889 ) ),
 .UNSPECIFIED., .F., .F., .F. ) 
 B_SPLINE_SURFACE_WITH_KNOTS ( ( 4, 4 ),
 ( 2, 2 ),
 ( 0.000000000000000000, 1.000000000000000000 ),
 ( 0.000000000000000000, 1.000000000000000000 ),
 .UNSPECIFIED. ) 
 GEOMETRIC_REPRESENTATION_ITEM ( )  RATIONAL_B_SPLINE_SURFACE ( (
 ( 1.000000000000000000, 1.000000000000000000),
 ( 0.9751682680413298332, 0.9999560080971552356),
 ( 0.9751682680413298332, 0.9999560080971552356),
 ( 1.000000000000000000, 1.000000000000000000) ) ) 
 REPRESENTATION_ITEM ( '' )  SURFACE ( )  );
#40107 = AXIS2_PLACEMENT_3D ( 'NONE', #49562, #35808, #17007 ) ;
#40108 = CARTESIAN_POINT ( 'NONE',  ( 0.5832655196449147983, -19.53343502719934222, -42.63425968644826725 ) ) ;
#40109 = CARTESIAN_POINT ( 'NONE',  ( 0.8751705887134553219, -47.55935879196475469, 7.160166390003496417 ) ) ;
#40110 = CARTESIAN_POINT ( 'NONE',  ( 5.895596859100789899, -13.97974974393973291, 14.46010996878324129 ) ) ;
#40111 = DIRECTION ( 'NONE',  ( 0.000000000000000000, 0.000000000000000000, 1.000000000000000000 ) ) ;
#40112 = EDGE_LOOP ( 'NONE', ( #29158, #47130, #38785, #59194 ) ) ;
#40113 = CARTESIAN_POINT ( 'NONE',  ( 4.834790513006553603, -15.88524143731098448, -44.49998253261139780 ) ) ;
#40114 = CARTESIAN_POINT ( 'NONE',  ( 0.6026112563231248442, 28.23784955160265753, -40.17667043951328765 ) ) ;
#40115 = CARTESIAN_POINT ( 'NONE',  ( 4.549368137175248350, 38.40568845698277300, -19.17571786012283042 ) ) ;
#40116 = ORIENTED_EDGE ( 'NONE', *, *, #11455, .F. ) ;
#40117 = CARTESIAN_POINT ( 'NONE',  ( 0.3676999524040366896, -44.10520818713899871, 0.8253448321555690859 ) ) ;
#40118 = CARTESIAN_POINT ( 'NONE',  ( 4.962356264823602814, -36.43094049105359744, -21.07183363638911189 ) ) ;
#40119 = EDGE_LOOP ( 'NONE', ( #14452, #24016, #36230, #46108 ) ) ;
#40120 = EDGE_CURVE ( 'NONE', #34089, #41352, #5458, .T. ) ;
#40121 = DIRECTION ( 'NONE',  ( 0.000000000000000000, 0.000000000000000000, -1.000000000000000000 ) ) ;
#40122 = ORIENTED_EDGE ( 'NONE', *, *, #4226, .T. ) ;
#40123 = CARTESIAN_POINT ( 'NONE',  ( -6.078726893082806448, 13.83016815118539000, -13.39852567182887455 ) ) ;
#40124 = EDGE_LOOP ( 'NONE', ( #875, #21661 ) ) ;
#40125 = DIRECTION ( 'NONE',  ( 1.000000000000000000, 0.000000000000000000, 0.000000000000000000 ) ) ;
#40126 = CARTESIAN_POINT ( 'NONE',  ( 0.1139756605157204866, 20.76085607197808613, 38.93510080703057952 ) ) ;
#40127 = ADVANCED_FACE ( 'NONE', ( #14310 ), #16639, .T. ) ;
#40128 =( BOUNDED_SURFACE ( )  B_SPLINE_SURFACE ( 3, 1, ( 
 ( #54550, #6619 ),
 ( #53625, #25446 ),
 ( #26076, #11681 ),
 ( #6942, #54872 ) ),
 .UNSPECIFIED., .F., .F., .F. ) 
 B_SPLINE_SURFACE_WITH_KNOTS ( ( 4, 4 ),
 ( 2, 2 ),
 ( 0.000000000000000000, 1.000000000000000000 ),
 ( 0.000000000000000000, 1.000000000000000000 ),
 .UNSPECIFIED. ) 
 GEOMETRIC_REPRESENTATION_ITEM ( )  RATIONAL_B_SPLINE_SURFACE ( (
 ( 1.000000000000000000, 1.000000000000000000),
 ( 0.9732289882329797637, 0.9999525324661233672),
 ( 0.9732289882329797637, 0.9999525324661233672),
 ( 1.000000000000000000, 1.000000000000000000) ) ) 
 REPRESENTATION_ITEM ( '' )  SURFACE ( )  );
#40129 = ORIENTED_EDGE ( 'NONE', *, *, #33052, .T. ) ;
#40130 = ORIENTED_EDGE ( 'NONE', *, *, #9977, .F. ) ;
#40131 = ADVANCED_FACE ( 'NONE', ( #4869 ), #61178, .F. ) ;
#40132 = CARTESIAN_POINT ( 'NONE',  ( 0.9790850452238872847, 20.09612553610694974, -36.77612090338274697 ) ) ;
#40133 = CARTESIAN_POINT ( 'NONE',  ( 4.975610109902397937, 0.000000000000000000, 0.000000000000000000 ) ) ;
#40134 = ORIENTED_EDGE ( 'NONE', *, *, #52235, .T. ) ;
#40135 = EDGE_CURVE ( 'NONE', #35054, #45423, #25679, .T. ) ;
#40136 = ORIENTED_EDGE ( 'NONE', *, *, #26369, .T. ) ;
#40137 = CARTESIAN_POINT ( 'NONE',  ( 5.901463166500145796, -15.77541139567702544, -12.47614786854420643 ) ) ;
#40139 = EDGE_CURVE ( 'NONE', #44340, #50198, #11489, .T. ) ;
#40138 = CARTESIAN_POINT ( 'NONE',  ( -6.077587904424778920, -17.35179747939703887, 8.349320069797363075 ) ) ;
#40140 = CARTESIAN_POINT ( 'NONE',  ( 2.526464513654346433, -20.43088802552588490, 37.81242626108687688 ) ) ;
#40141 = CARTESIAN_POINT ( 'NONE',  ( 0.1119898979215348811, -32.08462161508800392, -30.29089572905457928 ) ) ;
#40142 = CARTESIAN_POINT ( 'NONE',  ( 4.958415959904821868, -11.02103540056480924, -44.06518730837458264 ) ) ;
#40143 = VERTEX_POINT ( 'NONE', #33728 ) ;
#40144 = CARTESIAN_POINT ( 'NONE',  ( 0.000000000000000000, 0.000000000000000000, -5.574599999999999334 ) ) ;
#40145 = DIRECTION ( 'NONE',  ( 1.000000000000000000, 0.000000000000000000, 0.000000000000000000 ) ) ;
#40146 = VERTEX_POINT ( 'NONE', #43441 ) ;
#40147 = CARTESIAN_POINT ( 'NONE',  ( 1.231276596079887264, -21.83837404314831332, 35.78214904347716185 ) ) ;
#40148 = EDGE_LOOP ( 'NONE', ( #43258, #4364, #55473, #34949 ) ) ;
#40149 = CIRCLE ( 'NONE', #57071, 2.649999999999999467 ) ;
#40150 = CARTESIAN_POINT ( 'NONE',  ( 2.282816707992310512, -46.76237757432279807, 4.447135033303774243 ) ) ;
#40151 = CARTESIAN_POINT ( 'NONE',  ( 5.860006189529234355, -43.25137511473265306, 21.34829429597452588 ) ) ;
#40152 = VERTEX_POINT ( 'NONE', #5784 ) ;
#40153 = CARTESIAN_POINT ( 'NONE',  ( 0.9769922540276041456, -11.99378815008531696, -40.15570446271611615 ) ) ;
#40154 = DIRECTION ( 'NONE',  ( -0.1011922191286467460, -0.3314939457937330358, -0.9380148712520081089 ) ) ;
#40155 = CARTESIAN_POINT ( 'NONE',  ( 3.270143674763207553, -1.514386915940690415, 13.60381564321233583 ) ) ;
#40156 = FACE_OUTER_BOUND ( 'NONE', #51324, .T. ) ;
#40157 = EDGE_CURVE ( 'NONE', #43273, #8104, #59281, .T. ) ;
#40158 = ORIENTED_EDGE ( 'NONE', *, *, #6842, .F. ) ;
#40159 = CARTESIAN_POINT ( 'NONE',  ( 5.000000000000010658, -72.00000000000002842, 8.817456953860944867E-15 ) ) ;
#40160 = ORIENTED_EDGE ( 'NONE', *, *, #36518, .F. ) ;
#40161 = CARTESIAN_POINT ( 'NONE',  ( 3.238931869106855377, 31.66562935062897921, 29.07925862215142843 ) ) ;
#40162 = CARTESIAN_POINT ( 'NONE',  ( 3.344563996438205677, 2.687817229851463097, -5.441324518471517102 ) ) ;
#40163 = EDGE_CURVE ( 'NONE', #50298, #5968, #8460, .T. ) ;
#40164 = CARTESIAN_POINT ( 'NONE',  ( -6.078726893082806448, -18.27610589745688330, -6.064486333867170842 ) ) ;
#40165 = CARTESIAN_POINT ( 'NONE',  ( 2.528100132419516477, -39.24302147699968657, 14.90768405849201983 ) ) ;
#40166 = LINE ( 'NONE', #6259, #49861 ) ;
#40167 = CARTESIAN_POINT ( 'NONE',  ( 0.9741495583595179975, 37.35596046161894890, -21.11077839432095971 ) ) ;
#40168 = DIRECTION ( 'NONE',  ( 0.000000000000000000, 0.000000000000000000, 1.000000000000000000 ) ) ;
#40169 = CARTESIAN_POINT ( 'NONE',  ( 4.549368137175248350, -38.59302160394766901, 18.79584381673463866 ) ) ;
#40170 = EDGE_CURVE ( 'NONE', #56576, #33426, #18144, .T. ) ;
#40171 = DIRECTION ( 'NONE',  ( 0.000000000000000000, 0.000000000000000000, 1.000000000000000000 ) ) ;
#40172 = EDGE_CURVE ( 'NONE', #40335, #47955, #43665, .T. ) ;
#40173 = CARTESIAN_POINT ( 'NONE',  ( 0.5837374860065636106, 33.99581326751435029, 33.73893264285563021 ) ) ;
#40174 = CARTESIAN_POINT ( 'NONE',  ( 0.1158816050234198897, 36.98303739194169992, 24.06651172420720997 ) ) ;
#40175 = EDGE_LOOP ( 'NONE', ( #20421, #48884, #13461, #60551 ) ) ;
#40176 = CARTESIAN_POINT ( 'NONE',  ( 0.6253024248130512053, -19.24752319158097436, -45.17717430746637319 ) ) ;
#40177 = CARTESIAN_POINT ( 'NONE',  ( 3.270143674763207553, -1.514386915940500788, -13.60381564321235892 ) ) ;
#40178 = CARTESIAN_POINT ( 'NONE',  ( 2.009741617377216460, -42.23114984276965345, 12.49135943684998473 ) ) ;
#40179 = EDGE_LOOP ( 'NONE', ( #32573, #21372, #39560, #54465 ) ) ;
#40180 = CARTESIAN_POINT ( 'NONE',  ( 5.981074661064941900, 5.320466518160661629, 19.82308078259092810 ) ) ;
#40181 = CARTESIAN_POINT ( 'NONE',  ( 4.956653778116966613, 0.000000000000000000, 0.000000000000000000 ) ) ;
#40182 = B_SPLINE_CURVE_WITH_KNOTS ( 'NONE', 3,
 ( #56812, #42442, #3257, #47434 ),
 .UNSPECIFIED., .F., .F.,
 ( 4, 4 ),
 ( 1.551583845779545699E-17, 0.005004741218457433617 ),
 .UNSPECIFIED. ) ;
#40183 = CARTESIAN_POINT ( 'NONE',  ( 0.6028618097248863439, -12.61968633793883754, -46.42282207635398805 ) ) ;
#40185 = EDGE_LOOP ( 'NONE', ( #22972, #52827, #20672, #23827 ) ) ;
#40184 = AXIS2_PLACEMENT_3D ( 'NONE', #58434, #54048, #49366 ) ;
#40186 = DIRECTION ( 'NONE',  ( -1.000000000000000000, -0.000000000000000000, -0.000000000000000000 ) ) ;
#40187 = CARTESIAN_POINT ( 'NONE',  ( 1.500000000000000444, 6.245698675651501825E-16, 5.100000000000000533 ) ) ;
#40188 = VERTEX_POINT ( 'NONE', #59972 ) ;
#40189 = CARTESIAN_POINT ( 'NONE',  ( 0.3622758884714600280, -41.42293301073617329, -11.95365414648482627 ) ) ;
#40190 = ORIENTED_EDGE ( 'NONE', *, *, #52100, .F. ) ;
#40191 = ORIENTED_EDGE ( 'NONE', *, *, #53515, .T. ) ;
#40192 = CARTESIAN_POINT ( 'NONE',  ( 0.1157506346131639274, 44.03933932887103708, 2.734456304164842866 ) ) ;
#40193 = EDGE_CURVE ( 'NONE', #35413, #536, #51626, .T. ) ;
#40194 = EDGE_LOOP ( 'NONE', ( #21669, #56972, #23681, #15497 ) ) ;
#40195 = CARTESIAN_POINT ( 'NONE',  ( 0.1129192098497455998, -13.01845098534629486, 42.16007260106758281 ) ) ;
#40196 = CARTESIAN_POINT ( 'NONE',  ( 0.9780303403264768436, -17.93405777852207095, -37.87755516122598465 ) ) ;
#40197 = EDGE_LOOP ( 'NONE', ( #60389, #42415, #37260, #40977 ) ) ;
#40198 = EDGE_CURVE ( 'NONE', #15929, #16052, #47668, .T. ) ;
#40199 = CARTESIAN_POINT ( 'NONE',  ( -2.708315649062910779, -13.61924161399637612, 5.356004933109226762 ) ) ;
#40200 =( BOUNDED_SURFACE ( )  B_SPLINE_SURFACE ( 3, 1, ( 
 ( #43934, #58276 ),
 ( #11017, #29794 ),
 ( #53579, #1271 ),
 ( #1895, #25098 ) ),
 .UNSPECIFIED., .F., .F., .F. ) 
 B_SPLINE_SURFACE_WITH_KNOTS ( ( 4, 4 ),
 ( 2, 2 ),
 ( 0.000000000000000000, 1.000000000000000000 ),
 ( 0.000000000000000000, 1.000000000000000000 ),
 .UNSPECIFIED. ) 
 GEOMETRIC_REPRESENTATION_ITEM ( )  RATIONAL_B_SPLINE_SURFACE ( (
 ( 1.000000000000000000, 1.000000000000000000),
 ( 0.9953390228620291325, 0.8624445117761032620),
 ( 0.9953390228620291325, 0.8624445117761032620),
 ( 1.000000000000000000, 1.000000000000000000) ) ) 
 REPRESENTATION_ITEM ( '' )  SURFACE ( )  );
#40201 = CARTESIAN_POINT ( 'NONE',  ( -4.908599999999998964, 0.000000000000000000, 10.00000000000000000 ) ) ;
#40202 = EDGE_CURVE ( 'NONE', #39143, #30590, #133, .T. ) ;
#40203 = ORIENTED_EDGE ( 'NONE', *, *, #33403, .T. ) ;
#40204 = EDGE_CURVE ( 'NONE', #1749, #13688, #29633, .T. ) ;
#40205 = CARTESIAN_POINT ( 'NONE',  ( 0.1158516988532803660, 43.30104365222493357, -8.483028790526823570 ) ) ;
#40206 = B_SPLINE_CURVE_WITH_KNOTS ( 'NONE', 3,
 ( #19789, #29470, #963, #15705, #53272, #20099 ),
 .UNSPECIFIED., .F., .F.,
 ( 4, 2, 4 ),
 ( 1.223756431218073065E-16, 0.0002448718616795922832, 0.0004897437233590622684 ),
 .UNSPECIFIED. ) ;
#40207 = CARTESIAN_POINT ( 'NONE',  ( 49.32549503994585649, 12.27117319987102917, 2.381776070573418558 ) ) ;
#40208 = CARTESIAN_POINT ( 'NONE',  ( 0.1084644655670281704, -30.21121552071019067, 30.77359411724674132 ) ) ;
#40209 = CARTESIAN_POINT ( 'NONE',  ( 4.956653778116966613, 0.000000000000000000, 0.000000000000000000 ) ) ;
#40211 = EDGE_CURVE ( 'NONE', #58295, #60046, #32345, .T. ) ;
#40210 = ORIENTED_EDGE ( 'NONE', *, *, #47047, .F. ) ;
#40212 = B_SPLINE_CURVE_WITH_KNOTS ( 'NONE', 3,
 ( #22334, #49592, #35835, #44933 ),
 .UNSPECIFIED., .F., .F.,
 ( 4, 4 ),
 ( 9.697399036122160616E-19, 0.004050076154993000749 ),
 .UNSPECIFIED. ) ;
#40213 = ORIENTED_EDGE ( 'NONE', *, *, #58612, .F. ) ;
#40214 = CARTESIAN_POINT ( 'NONE',  ( 0.5800708057587401489, -37.61306623599821108, -29.65250565429482776 ) ) ;
#40215 = CARTESIAN_POINT ( 'NONE',  ( -6.078726893082806448, -6.653559303940370206, 18.06998035022918359 ) ) ;
#40216 = ADVANCED_FACE ( 'NONE', ( #2644 ), #24640, .F. ) ;
#40217 = CARTESIAN_POINT ( 'NONE',  ( 4.694002226626920127, -25.79840873770053733, 37.58625916540072609 ) ) ;
#40218 = EDGE_LOOP ( 'NONE', ( #54281, #56611, #2050, #44264 ) ) ;
#40219 = FACE_OUTER_BOUND ( 'NONE', #59842, .T. ) ;
#40220 = CARTESIAN_POINT ( 'NONE',  ( 3.661921753702022109, -3.452423898254273205, -46.91174578994899491 ) ) ;
#40221 = CARTESIAN_POINT ( 'NONE',  ( 5.896782393890504181, -20.11283288166117345, -0.006352352428112362746 ) ) ;
#40222 = EDGE_LOOP ( 'NONE', ( #4868, #18129, #51252, #48619 ) ) ;
#40223 = ORIENTED_EDGE ( 'NONE', *, *, #55926, .T. ) ;
#40224 = CARTESIAN_POINT ( 'NONE',  ( 4.960386119450149955, 12.51307094103702511, 41.92683532413238368 ) ) ;
#40225 = CARTESIAN_POINT ( 'NONE',  ( 0.1081432562775997697, 33.95357233988193002, 26.58728936586528491 ) ) ;
#40226 = CARTESIAN_POINT ( 'NONE',  ( 0.3622758884714600280, -37.74294673546600620, 20.83792692158906235 ) ) ;
#40227 = CARTESIAN_POINT ( 'NONE',  ( 0.000000000000000000, 0.000000000000000000, -5.574599999999999334 ) ) ;
#40228 = B_SPLINE_CURVE_WITH_KNOTS ( 'NONE', 3,
 ( #20244, #48424, #49648, #25538, #10842, #39055 ),
 .UNSPECIFIED., .F., .F.,
 ( 4, 2, 4 ),
 ( 1.764953265579307567E-18, 0.0002450742804987335256, 0.0004901485609974652081 ),
 .UNSPECIFIED. ) ;
#40229 = VECTOR ( 'NONE', #15302, 1000.000000000000114 ) ;
#40230 = CARTESIAN_POINT ( 'NONE',  ( 0.1084644655670282537, 33.96951444491424610, -26.56696682929019815 ) ) ;
#40231 = B_SPLINE_CURVE_WITH_KNOTS ( 'NONE', 3,
 ( #51924, #9013, #28120, #52851 ),
 .UNSPECIFIED., .F., .F.,
 ( 4, 4 ),
 ( 2.602085213965210642E-18, 0.004050076154993001616 ),
 .UNSPECIFIED. ) ;
#40232 = CARTESIAN_POINT ( 'NONE',  ( 0.3676999524040366896, -41.19158123804976412, -15.78620342045500280 ) ) ;
#40233 = CARTESIAN_POINT ( 'NONE',  ( 4.967162193818130511, -13.42934394584192148, 40.93989340068605998 ) ) ;
#40234 = CARTESIAN_POINT ( 'NONE',  ( -90.00000000000000000, 0.000000000000000000, 0.000000000000000000 ) ) ;
#40235 = CARTESIAN_POINT ( 'NONE',  ( 3.270143674763207553, -12.74832469035448668, -4.983712007628368745 ) ) ;
#40236 = FACE_OUTER_BOUND ( 'NONE', #32063, .T. ) ;
#40237 = CARTESIAN_POINT ( 'NONE',  ( 0.8751705887134553219, 7.160166390003662507, 47.55935879196473337 ) ) ;
#40238 = CARTESIAN_POINT ( 'NONE',  ( 0.6021447746440204973, 41.29831215267225275, 26.57048272856424020 ) ) ;
#40239 = CARTESIAN_POINT ( 'NONE',  ( -6.016104459813374383, -17.41090761020841171, 7.206059014950020547 ) ) ;
#40240 = B_SPLINE_CURVE_WITH_KNOTS ( 'NONE', 3,
 ( #24141, #29152, #19457, #38576, #52329, #23841 ),
 .UNSPECIFIED., .F., .F.,
 ( 4, 2, 4 ),
 ( 9.745765416140531346E-18, 0.0002291978881530162956, 0.0004583957763060228334 ),
 .UNSPECIFIED. ) ;
#40241 = CARTESIAN_POINT ( 'NONE',  ( 2.359973842542475886, 41.28141064895650914, -15.29643845686700843 ) ) ;
#40242 = CARTESIAN_POINT ( 'NONE',  ( 0.5837800304671216800, -13.85068106606779281, -44.80397266075372897 ) ) ;
#40243 = CARTESIAN_POINT ( 'NONE',  ( 0.6254087463353924514, -19.04342133628015432, -44.17672642933494132 ) ) ;
#40244 = CARTESIAN_POINT ( 'NONE',  ( 0.9775691876210965692, -22.86778163026855992, 35.11977039076914053 ) ) ;
#40245 = EDGE_CURVE ( 'NONE', #49095, #14998, #6115, .T. ) ;
#40246 = DIRECTION ( 'NONE',  ( -1.000000000000000000, -0.000000000000000000, -0.000000000000000000 ) ) ;
#40247 = CARTESIAN_POINT ( 'NONE',  ( 4.549368137175248350, 24.02461520945271900, -35.57418903283089406 ) ) ;
#40248 = CARTESIAN_POINT ( 'NONE',  ( 3.240649175237397372, 28.19680434710399553, 33.76692378658126614 ) ) ;
#40249 = ORIENTED_EDGE ( 'NONE', *, *, #27670, .T. ) ;
#40250 = ORIENTED_EDGE ( 'NONE', *, *, #47468, .F. ) ;
#40251 = CARTESIAN_POINT ( 'NONE',  ( 0.6029443449137436017, 17.00082651214890817, -46.07072211163124109 ) ) ;
#40252 = CARTESIAN_POINT ( 'NONE',  ( 2.009741617377216460, 2.862416983765094791, -43.94667958599486468 ) ) ;
#40253 = CARTESIAN_POINT ( 'NONE',  ( -1.600000000000000089, -11.64055411052240352, -1.199999999999999956 ) ) ;
#40254 = VERTEX_POINT ( 'NONE', #21456 ) ;
#40255 = ORIENTED_EDGE ( 'NONE', *, *, #40204, .F. ) ;
#40256 = CARTESIAN_POINT ( 'NONE',  ( 0.9762797500689124330, -22.97506929404158171, -35.04955029839458547 ) ) ;
#40257 = FACE_OUTER_BOUND ( 'NONE', #37110, .T. ) ;
#40258 = CARTESIAN_POINT ( 'NONE',  ( 0.6029303876144825880, 6.149480157545950121, 47.71279573267361229 ) ) ;
#40259 = ORIENTED_EDGE ( 'NONE', *, *, #43455, .T. ) ;
#40260 = EDGE_LOOP ( 'NONE', ( #33508, #54159, #56765, #51724 ) ) ;
#40261 = DIRECTION ( 'NONE',  ( 0.07439287786467665975, 0.2453289374370069276, 0.9665813013808205456 ) ) ;
#40262 = CARTESIAN_POINT ( 'NONE',  ( 0.8751705887134553219, -38.69254731947813752, -28.56654290188640033 ) ) ;
#40263 = CARTESIAN_POINT ( 'NONE',  ( 0.5830082357119573677, -38.50772913779835704, -26.76540363208243534 ) ) ;
#40264 = VERTEX_POINT ( 'NONE', #31160 ) ;
#40265 = EDGE_CURVE ( 'NONE', #45486, #43576, #10711, .T. ) ;
#40266 = CARTESIAN_POINT ( 'NONE',  ( 0.3676999524040366896, 5.056646555325087000, 43.82215089355334925 ) ) ;
#40267 = VECTOR ( 'NONE', #20342, 1000.000000000000114 ) ;
#40268 = CARTESIAN_POINT ( 'NONE',  ( 5.838029081930957709, -45.55059156558392175, 12.49834653777350724 ) ) ;
#40269 = EDGE_CURVE ( 'NONE', #17907, #56898, #12943, .T. ) ;
#40270 = TOROIDAL_SURFACE ( 'NONE', #14233, 15.38217999999999996, 0.05882000000000066342 ) ;
#40271 = B_SPLINE_CURVE_WITH_KNOTS ( 'NONE', 3,
 ( #16889, #36003, #35378, #54436 ),
 .UNSPECIFIED., .F., .F.,
 ( 4, 4 ),
 ( 0.000000000000000000, 0.004041751736740996012 ),
 .UNSPECIFIED. ) ;
#40272 = CARTESIAN_POINT ( 'NONE',  ( 0.1073791018717483448, 21.98088480513615295, 37.10214135362896570 ) ) ;
#40273 = EDGE_CURVE ( 'NONE', #1309, #4904, #34959, .T. ) ;
#40274 = ORIENTED_EDGE ( 'NONE', *, *, #26032, .T. ) ;
#40275 = ORIENTED_EDGE ( 'NONE', *, *, #56286, .F. ) ;
#40276 = EDGE_CURVE ( 'NONE', #61466, #10506, #42787, .T. ) ;
#40277 = CARTESIAN_POINT ( 'NONE',  ( 0.8751705887134423323, 46.21789262997739201, 13.30665218149378504 ) ) ;
#40278 = CARTESIAN_POINT ( 'NONE',  ( -5.995132425357893702, 13.31880955509745590, -13.33084941932893486 ) ) ;
#40279 = ORIENTED_EDGE ( 'NONE', *, *, #11544, .F. ) ;
#40280 = CARTESIAN_POINT ( 'NONE',  ( 3.238931869106854489, -42.82436385108076848, -3.793313187126794883 ) ) ;
#40281 = EDGE_CURVE ( 'NONE', #50035, #20684, #55508, .T. ) ;
#40282 = CARTESIAN_POINT ( 'NONE',  ( -6.077587904424778920, 15.43577113102541887, -11.51229738082424348 ) ) ;
#40283 = CARTESIAN_POINT ( 'NONE',  ( 0.5839879327111926477, 12.30864801674776565, -46.28746210677699224 ) ) ;
#40284 = ORIENTED_EDGE ( 'NONE', *, *, #50773, .T. ) ;
#40285 = CARTESIAN_POINT ( 'NONE',  ( 3.782625744892852193, 40.96637710780765218, 9.433665817480269666 ) ) ;
#40286 = CARTESIAN_POINT ( 'NONE',  ( 0.5804410086790514622, -13.37224000219898734, 44.95223074752782111 ) ) ;
#40287 = CARTESIAN_POINT ( 'NONE',  ( 0.9740398440564311811, -21.81228698783116116, -36.95080095316296109 ) ) ;
#40288 = ORIENTED_EDGE ( 'NONE', *, *, #32900, .T. ) ;
#40289 = DIRECTION ( 'NONE',  ( -0.1024043820194934368, 0.8679729669084648158, -0.4859385467930307234 ) ) ;
#40290 = CARTESIAN_POINT ( 'NONE',  ( 0.7245667037590759474, -47.79072416626839725, -5.464144792999212186 ) ) ;
#40291 = ORIENTED_EDGE ( 'NONE', *, *, #24541, .T. ) ;
#40292 = DIRECTION ( 'NONE',  ( 0.000000000000000000, 0.000000000000000000, 1.000000000000000000 ) ) ;
#40293 = EDGE_CURVE ( 'NONE', #12657, #37577, #17361, .T. ) ;
#40294 = ORIENTED_EDGE ( 'NONE', *, *, #31573, .F. ) ;
#40295 = CARTESIAN_POINT ( 'NONE',  ( 1.157643937452369709, -13.20506546943684079, -39.78226389413553221 ) ) ;
#40296 = DIRECTION ( 'NONE',  ( -1.000000000000000000, -0.000000000000000000, -0.000000000000000000 ) ) ;
#40297 = ADVANCED_FACE ( 'NONE', ( #11447 ), #3540, .F. ) ;
#40298 = CARTESIAN_POINT ( 'NONE',  ( 0.2279481005628794799, -42.47734836628340105, -11.92385687780218184 ) ) ;
#40299 = PRODUCT_DEFINITION_SHAPE ( 'NONE', 'NONE',  #61976 ) ;
#40300 = CARTESIAN_POINT ( 'NONE',  ( 0.09136607875274982415, 0.000000000000000000, 0.000000000000000000 ) ) ;
#40301 = DIRECTION ( 'NONE',  ( -1.000000000000000000, -0.000000000000000000, -0.000000000000000000 ) ) ;
#40302 = CARTESIAN_POINT ( 'NONE',  ( -6.015611763856276717, 18.19956619163658118, 4.882992715191364574 ) ) ;
#40303 = CARTESIAN_POINT ( 'NONE',  ( 0.9757892942422827787, -5.651566539685542345, -42.53466646637867399 ) ) ;
#40304 = CARTESIAN_POINT ( 'NONE',  ( -6.077587904424778920, -19.21689618909968544, 1.227567615773810239 ) ) ;
#40305 = CARTESIAN_POINT ( 'NONE',  ( -6.072942160501519027, -19.21763696748628547, 1.219258657924985334 ) ) ;
#40306 = CARTESIAN_POINT ( 'NONE',  ( 3.661921753702030546, 44.83346572263544516, -14.23346321635423628 ) ) ;
#40307 = EDGE_LOOP ( 'NONE', ( #53482, #58442, #34534, #53397 ) ) ;
#40308 = CARTESIAN_POINT ( 'NONE',  ( 3.783198216974387851, 42.41041696600780142, 7.325057189010560244 ) ) ;
#40309 = DIRECTION ( 'NONE',  ( 0.000000000000000000, 0.000000000000000000, -1.000000000000000000 ) ) ;
#40310 = CARTESIAN_POINT ( 'NONE',  ( -6.057079549204054558, -14.66865672308385804, -12.47644745270323874 ) ) ;
#40311 = CARTESIAN_POINT ( 'NONE',  ( 0.6000166863083090663, 5.235566842224464779, 48.83044461756470866 ) ) ;
#40312 = CARTESIAN_POINT ( 'NONE',  ( 0.6000166863083106206, -47.63401213562553949, -11.95091500980295685 ) ) ;
#40313 = CARTESIAN_POINT ( 'NONE',  ( 5.901463166500145796, 19.70672075163017922, 4.020326797401583718 ) ) ;
#40314 = DIRECTION ( 'NONE',  ( 7.112851796247059002E-15, -0.7071067811865536790, 0.7071067811865413555 ) ) ;
#40315 = CARTESIAN_POINT ( 'NONE',  ( 0.8744876279028306332, 23.49358985382604459, 43.10917867646859492 ) ) ;
#40316 = EDGE_CURVE ( 'NONE', #38620, #1988, #7972, .T. ) ;
#40317 = CARTESIAN_POINT ( 'NONE',  ( 2.706805983486679779, 35.95399731719180636, -25.37885320961369828 ) ) ;
#40318 = CARTESIAN_POINT ( 'NONE',  ( 0.1073791018717578927, 0.4849339620933161288, -43.12183934961191056 ) ) ;
#40320 = VERTEX_POINT ( 'NONE', #18317 ) ;
#40319 = CARTESIAN_POINT ( 'NONE',  ( 5.896782393890504181, -18.51439742298330771, -7.857682542699298445 ) ) ;
#40321 = ORIENTED_EDGE ( 'NONE', *, *, #37026, .F. ) ;
#40322 = CARTESIAN_POINT ( 'NONE',  ( 0.1064266418746778603, -34.55203617814607497, 25.80493189480173299 ) ) ;
#40323 = CARTESIAN_POINT ( 'NONE',  ( 4.962356264823608143, 0.000000000000000000, 0.000000000000000000 ) ) ;
#40324 = FACE_OUTER_BOUND ( 'NONE', #40260, .T. ) ;
#40325 = VERTEX_POINT ( 'NONE', #41512 ) ;
#40326 = CARTESIAN_POINT ( 'NONE',  ( 4.975801465491695552, -40.15204426031515794, -26.14269827151666092 ) ) ;
#40327 = CARTESIAN_POINT ( 'NONE',  ( 5.910764540655178756, 3.360528482494880897, 19.82947520201943092 ) ) ;
#40328 = CARTESIAN_POINT ( 'NONE',  ( 2.500000000000000000, 2.357898499370431722, -2.818925648462311528E-15 ) ) ;
#40329 = ORIENTED_EDGE ( 'NONE', *, *, #27779, .T. ) ;
#40330 = ORIENTED_EDGE ( 'NONE', *, *, #33850, .T. ) ;
#40331 = CARTESIAN_POINT ( 'NONE',  ( 3.680882792899937250, -47.28852514876961521, 8.091276083384595808 ) ) ;
#40332 = CARTESIAN_POINT ( 'NONE',  ( 0.1095718737110178559, -10.91304379105033640, -41.72082389913612843 ) ) ;
#40333 = CARTESIAN_POINT ( 'NONE',  ( 0.9730545539215883499, -41.57420493492377744, -10.61654491617608009 ) ) ;
#40334 = ORIENTED_EDGE ( 'NONE', *, *, #55372, .T. ) ;
#40335 = VERTEX_POINT ( 'NONE', #17690 ) ;
#40336 = CARTESIAN_POINT ( 'NONE',  ( 5.960221823109900008, -0.005450390361581681532, -20.52559243573973546 ) ) ;
#40337 = CARTESIAN_POINT ( 'NONE',  ( 5.894904586330512508, 10.82137050184791427, -16.95368256525344464 ) ) ;
#40338 = VERTEX_POINT ( 'NONE', #56806 ) ;
#40339 = FACE_OUTER_BOUND ( 'NONE', #13619, .T. ) ;
#40340 = DIRECTION ( 'NONE',  ( 0.000000000000000000, 0.000000000000000000, -1.000000000000000000 ) ) ;
#40341 = EDGE_CURVE ( 'NONE', #60557, #2175, #8577, .T. ) ;
#40342 = VERTEX_POINT ( 'NONE', #46210 ) ;
#40343 = LINE ( 'NONE', #45346, #35864 ) ;
#40344 = CARTESIAN_POINT ( 'NONE',  ( 0.1119898979215349782, -6.487605684152662811, 43.64484254455250323 ) ) ;
#40345 = VERTEX_POINT ( 'NONE', #8901 ) ;
#40346 = CARTESIAN_POINT ( 'NONE',  ( 5.901764892641307547, 25.42221402738085700, -41.85334516362722468 ) ) ;
#40347 = CARTESIAN_POINT ( 'NONE',  ( 4.956445790443495092, 1.033212179477288384, -47.07940656732829865 ) ) ;
#40348 = ADVANCED_FACE ( 'NONE', ( #51185 ), #50871, .F. ) ;
#40349 = CARTESIAN_POINT ( 'NONE',  ( 2.299746137290199943, 48.35891443790075783, 8.105352063540024687 ) ) ;
#40350 = CARTESIAN_POINT ( 'NONE',  ( 2.648799415243696664, -42.02883204265787498, -25.26053721557904552 ) ) ;
#40351 = VECTOR ( 'NONE', #42185, 1000.000000000000114 ) ;
#40352 = EDGE_LOOP ( 'NONE', ( #28931, #47241, #44056, #40666 ) ) ;
#40353 = CARTESIAN_POINT ( 'NONE',  ( 0.8557997880470690211, -33.22501220301925429, 34.51495345639537504 ) ) ;
#40354 = CARTESIAN_POINT ( 'NONE',  ( 0.1158516988532803660, 39.73311795087249010, -19.18909838254134925 ) ) ;
#40355 = ORIENTED_EDGE ( 'NONE', *, *, #47913, .T. ) ;
#40356 = CARTESIAN_POINT ( 'NONE',  ( 0.6039202388192952409, -30.48176006895440082, -38.50228585353977451 ) ) ;
#40357 = VERTEX_POINT ( 'NONE', #22694 ) ;
#40358 = CARTESIAN_POINT ( 'NONE',  ( 0.5839879882012706247, -18.32896541547101421, 44.25011577017261288 ) ) ;
#40359 = EDGE_LOOP ( 'NONE', ( #2837, #46596, #26895, #43669 ) ) ;
#40360 = CARTESIAN_POINT ( 'NONE',  ( -2.739355103387247858, 13.33354922980902302, 6.712974891005939249 ) ) ;
#40361 = CARTESIAN_POINT ( 'NONE',  ( -6.016761891674565099, 7.214149619366596156, -17.40752468084775373 ) ) ;
#40362 = CARTESIAN_POINT ( 'NONE',  ( 4.956653778116975495, -8.845409907521238679, 47.27023054223749909 ) ) ;
#40363 = ORIENTED_EDGE ( 'NONE', *, *, #23657, .T. ) ;
#40364 = CARTESIAN_POINT ( 'NONE',  ( 0.5832366564991519065, 6.521686574606105680, 47.44984844891988018 ) ) ;
#40365 = EDGE_CURVE ( 'NONE', #25700, #31789, #20359, .T. ) ;
#40366 = CARTESIAN_POINT ( 'NONE',  ( 4.553261556744873317, -36.69060082144796553, 24.15241969627054530 ) ) ;
#40367 = VERTEX_POINT ( 'NONE', #55887 ) ;
#40368 = AXIS2_PLACEMENT_3D ( 'NONE', #11479, #43793, #43472 ) ;
#40369 =( BOUNDED_SURFACE ( )  B_SPLINE_SURFACE ( 3, 1, ( 
 ( #39758, #2419 ),
 ( #21544, #40681 ),
 ( #1188, #35977 ),
 ( #55041, #48816 ) ),
 .UNSPECIFIED., .F., .F., .F. ) 
 B_SPLINE_SURFACE_WITH_KNOTS ( ( 4, 4 ),
 ( 2, 2 ),
 ( 0.000000000000000000, 1.000000000000000000 ),
 ( 0.000000000000000000, 1.000000000000000000 ),
 .UNSPECIFIED. ) 
 GEOMETRIC_REPRESENTATION_ITEM ( )  RATIONAL_B_SPLINE_SURFACE ( (
 ( 1.000000000000000000, 1.000000000000000000),
 ( 0.9953390228620291325, 0.8624445117761032620),
 ( 0.9953390228620291325, 0.8624445117761032620),
 ( 1.000000000000000000, 1.000000000000000000) ) ) 
 REPRESENTATION_ITEM ( '' )  SURFACE ( )  );
#40370 = ORIENTED_EDGE ( 'NONE', *, *, #39713, .T. ) ;
#40371 = CARTESIAN_POINT ( 'NONE',  ( 2.281351352603290028, 17.13758816714750211, 44.80774876812563434 ) ) ;
#40372 = CARTESIAN_POINT ( 'NONE',  ( -6.063463321072278589, -18.90456390296430200, 3.665776332267008275 ) ) ;
#40373 = CARTESIAN_POINT ( 'NONE',  ( 0.9788927965476033055, 38.52767114616671051, -16.49106329757458766 ) ) ;
#40374 = CARTESIAN_POINT ( 'NONE',  ( 1.088908134280557105, -0.7803765577538801512, -42.90644581410506930 ) ) ;
#40375 = CARTESIAN_POINT ( 'NONE',  ( 4.303969348037258058, 35.51084504003198106, 32.45857549159314459 ) ) ;
#40376 = CARTESIAN_POINT ( 'NONE',  ( 0.6253024248130498730, -45.77087648984584689, 17.78963441920380717 ) ) ;
#40377 = ORIENTED_EDGE ( 'NONE', *, *, #24223, .T. ) ;
#40378 = CARTESIAN_POINT ( 'NONE',  ( 0.5809828226811617480, -23.47450554821680413, -41.74875432577673706 ) ) ;
#40379 = FACE_BOUND ( 'NONE', #5053, .T. ) ;
#40380 = ORIENTED_EDGE ( 'NONE', *, *, #14451, .T. ) ;
#40381 = CARTESIAN_POINT ( 'NONE',  ( -6.015611763856276717, 11.47596948473810841, 14.94556629257429492 ) ) ;
#40382 = CARTESIAN_POINT ( 'NONE',  ( 0.6008122571543323964, 44.43158886499384153, 20.91383421081539140 ) ) ;
#40383 = CARTESIAN_POINT ( 'NONE',  ( 0.5837800005270553649, 45.22975938364896820, 12.38967815316459564 ) ) ;
#40384 = B_SPLINE_CURVE_WITH_KNOTS ( 'NONE', 3,
 ( #18907, #38030, #23897, #43027 ),
 .UNSPECIFIED., .F., .F.,
 ( 4, 4 ),
 ( 0.000000000000000000, 0.005013413432710142441 ),
 .UNSPECIFIED. ) ;
#40385 = CARTESIAN_POINT ( 'NONE',  ( 5.860006189529234355, 43.26650951066869766, 21.31760477694597711 ) ) ;
#40386 = CARTESIAN_POINT ( 'NONE',  ( 0.5997462898726536595, 46.43852004798843325, 15.96920429754989890 ) ) ;
#40387 = FILL_AREA_STYLE ('',( #25031 ) ) ;
#40388 =( BOUNDED_SURFACE ( )  B_SPLINE_SURFACE ( 3, 1, ( 
 ( #25112, #57989 ),
 ( #5365, #58925 ),
 ( #24809, #24184 ),
 ( #675, #5665 ) ),
 .UNSPECIFIED., .F., .F., .F. ) 
 B_SPLINE_SURFACE_WITH_KNOTS ( ( 4, 4 ),
 ( 2, 2 ),
 ( 0.000000000000000000, 1.000000000000000000 ),
 ( 0.000000000000000000, 1.000000000000000000 ),
 .UNSPECIFIED. ) 
 GEOMETRIC_REPRESENTATION_ITEM ( )  RATIONAL_B_SPLINE_SURFACE ( (
 ( 1.000000000000000000, 1.000000000000000000),
 ( 0.9751682680413298332, 0.9999560080971552356),
 ( 0.9751682680413298332, 0.9999560080971552356),
 ( 1.000000000000000000, 1.000000000000000000) ) ) 
 REPRESENTATION_ITEM ( '' )  SURFACE ( )  );
#40389 = EDGE_CURVE ( 'NONE', #40072, #39717, #41697, .T. ) ;
#40390 = CARTESIAN_POINT ( 'NONE',  ( 0.9736507210033060744, -39.81239086052226384, 16.00326134587904292 ) ) ;
#40391 = CARTESIAN_POINT ( 'NONE',  ( 0.6016118706126977189, 23.02238442462318702, -43.37650135947801999 ) ) ;
#40392 = CARTESIAN_POINT ( 'NONE',  ( -2.708315649062910779, 11.44805714186559875, 9.116606751444367163 ) ) ;
#40393 = CARTESIAN_POINT ( 'NONE',  ( 5.901463166500146684, 3.331057597888285482, -19.83486641296551056 ) ) ;
#40394 = CARTESIAN_POINT ( 'NONE',  ( -2.739355103387248747, 14.60025052884540209, -3.111310245855684720 ) ) ;
#40395 = STYLED_ITEM ( 'NONE', ( #19559 ), #32179 ) ;
#40396 = CARTESIAN_POINT ( 'NONE',  ( 1.231276596079887264, 14.27346765619334512, -39.41503383336959132 ) ) ;
#40397 = CARTESIAN_POINT ( 'NONE',  ( -5.272380000000000067, 0.000000000000000000, 0.000000000000000000 ) ) ;
#40398 = EDGE_CURVE ( 'NONE', #61473, #23542, #22382, .T. ) ;
#40399 = VERTEX_POINT ( 'NONE', #50881 ) ;
#40400 = EDGE_CURVE ( 'NONE', #54983, #26937, #21125, .T. ) ;
#40401 = CARTESIAN_POINT ( 'NONE',  ( 0.1097557419366048670, 10.94578341459270376, -41.71221507312537824 ) ) ;
#40402 = CARTESIAN_POINT ( 'NONE',  ( 0.1103310638050661874, 43.12437788119554227, 0.08238894504410687603 ) ) ;
#40403 = CARTESIAN_POINT ( 'NONE',  ( 0.9741495583595175534, -25.80610403442885570, -34.28086552274318421 ) ) ;
#40404 = CARTESIAN_POINT ( 'NONE',  ( 2.648799415243708655, 31.92790172191037712, -37.21728838759792524 ) ) ;
#40405 = CARTESIAN_POINT ( 'NONE',  ( 4.956653778116992370, 15.97476558431944937, -45.35992544608513555 ) ) ;
#40406 = EDGE_LOOP ( 'NONE', ( #56312, #17066, #5391, #19223 ) ) ;
#40407 = CARTESIAN_POINT ( 'NONE',  ( 4.956653778116975495, -31.29546495791875316, 36.51451553856407628 ) ) ;
#40408 = CARTESIAN_POINT ( 'NONE',  ( 0.9740398440564311811, 16.03656236596804163, -39.79907313245115574 ) ) ;
#40409 = AXIS2_PLACEMENT_3D ( 'NONE', #4857, #39655, #48111 ) ;
#40410 = CARTESIAN_POINT ( 'NONE',  ( 0.8744876279028263033, -42.33402326122615733, -24.86323641237110493 ) ) ;
#40411 = ORIENTED_EDGE ( 'NONE', *, *, #19531, .F. ) ;
#40412 = CARTESIAN_POINT ( 'NONE',  ( -6.057079549204054558, -16.14367994231336567, -10.49822980410923812 ) ) ;
#40413 = ADVANCED_FACE ( 'NONE', ( #47429 ), #30658, .F. ) ;
#40414 = VERTEX_POINT ( 'NONE', #10448 ) ;
#40415 = CARTESIAN_POINT ( 'NONE',  ( 4.967162193818130511, -32.68434214048189546, 28.07411493385282242 ) ) ;
#40416 = CARTESIAN_POINT ( 'NONE',  ( -6.016761891674564211, -13.32657647165345693, -13.32172022638605569 ) ) ;
#40417 = ORIENTED_EDGE ( 'NONE', *, *, #61226, .T. ) ;
#40418 = CARTESIAN_POINT ( 'NONE',  ( 4.335381028904216727, -27.18827219542376383, -40.74990432739557633 ) ) ;
#40420 = EDGE_LOOP ( 'NONE', ( #8027, #33266, #59207, #19540 ) ) ;
#40419 = EDGE_CURVE ( 'NONE', #52535, #1876, #9938, .T. ) ;
#40421 = FACE_OUTER_BOUND ( 'NONE', #52382, .T. ) ;
#40422 = CARTESIAN_POINT ( 'NONE',  ( 0.1156867017252034696, 20.29825183744268458, 39.17810331829427639 ) ) ;
#40423 = ORIENTED_EDGE ( 'NONE', *, *, #58497, .F. ) ;
#40424 = B_SPLINE_CURVE_WITH_KNOTS ( 'NONE', 3,
 ( #61211, #4493, #55580, #42452 ),
 .UNSPECIFIED., .F., .F.,
 ( 4, 4 ),
 ( 0.000000000000000000, 0.004447772540403798110 ),
 .UNSPECIFIED. ) ;
#40425 = ORIENTED_EDGE ( 'NONE', *, *, #40491, .T. ) ;
#40426 = CARTESIAN_POINT ( 'NONE',  ( 0.9769922540276034795, 20.52688070952990884, -36.53736065211683126 ) ) ;
#40427 = EDGE_CURVE ( 'NONE', #45184, #22660, #48048, .T. ) ;
#40428 = CARTESIAN_POINT ( 'NONE',  ( 5.896278296736517710, 16.58497454171988039, -11.37829508603494588 ) ) ;
#40429 = VERTEX_POINT ( 'NONE', #19549 ) ;
#40430 = ORIENTED_EDGE ( 'NONE', *, *, #35034, .T. ) ;
#40431 = FACE_OUTER_BOUND ( 'NONE', #11008, .T. ) ;
#40432 = CARTESIAN_POINT ( 'NONE',  ( 7.999999999999986677, 56.56854249492450037, -56.56854249492312192 ) ) ;
#40433 = CARTESIAN_POINT ( 'NONE',  ( 3.238018933889920792, -5.387504234938370828, 12.26304572633462975 ) ) ;
#40434 = CARTESIAN_POINT ( 'NONE',  ( 0.1129192098497447394, -32.03190746134960420, -30.34647742609823595 ) ) ;
#40435 = CARTESIAN_POINT ( 'NONE',  ( 0.6030672727741701600, 44.41203814406380701, 18.49051564326148878 ) ) ;
#40436 = VERTEX_POINT ( 'NONE', #47740 ) ;
#40437 = CARTESIAN_POINT ( 'NONE',  ( 0.2999999999999897193, -13.49666625504239192, -1.199999999999999956 ) ) ;
#40438 = EDGE_CURVE ( 'NONE', #5400, #61383, #48752, .T. ) ;
#40439 = CARTESIAN_POINT ( 'NONE',  ( 0.000000000000000000, 0.6959691356230525150, -1.199999999999999956 ) ) ;
#40440 = VERTEX_POINT ( 'NONE', #14238 ) ;
#40441 = AXIS2_PLACEMENT_3D ( 'NONE', #49213, #34513, #20110 ) ;
#40442 = B_SPLINE_CURVE_WITH_KNOTS ( 'NONE', 3,
 ( #33532, #48531, #57914, #44186 ),
 .UNSPECIFIED., .F., .F.,
 ( 4, 4 ),
 ( 2.302551629917872730E-17, 0.004564976165746190313 ),
 .UNSPECIFIED. ) ;
#40443 = ORIENTED_EDGE ( 'NONE', *, *, #29937, .F. ) ;
#40444 = CARTESIAN_POINT ( 'NONE',  ( 4.975801465491694664, -8.787181743659814970, -47.10002938642139014 ) ) ;
#40445 = CARTESIAN_POINT ( 'NONE',  ( 0.8753041380234465318, -35.88662119133365280, 33.51550010581227212 ) ) ;
#40446 = LINE ( 'NONE', #49502, #23976 ) ;
#40447 = ORIENTED_EDGE ( 'NONE', *, *, #860, .T. ) ;
#40448 = CARTESIAN_POINT ( 'NONE',  ( 0.1092565886968784872, -42.79503959566649485, -5.321013289171513172 ) ) ;
#40449 = CARTESIAN_POINT ( 'NONE',  ( 51.82890873906638518, 12.28711123495430790, -2.299226249064501015 ) ) ;
#40450 = CARTESIAN_POINT ( 'NONE',  ( 0.6025881611877910160, -29.11258673756386628, -38.29866377863830706 ) ) ;
#40451 = VERTEX_POINT ( 'NONE', #34568 ) ;
#40452 = CARTESIAN_POINT ( 'NONE',  ( 4.694002226626921015, -43.15593359350871339, 14.69184015427610923 ) ) ;
#40453 = EDGE_LOOP ( 'NONE', ( #17163, #19430, #45497, #14143 ) ) ;
#40454 = CARTESIAN_POINT ( 'NONE',  ( 0.7044674535453004927, -47.28336972574665964, 13.26972758534445340 ) ) ;
#40455 = CARTESIAN_POINT ( 'NONE',  ( 0.5804410086790514622, -13.37224000219835673, -44.95223074752801296 ) ) ;
#40456 =( GEOMETRIC_REPRESENTATION_CONTEXT ( 3 ) GLOBAL_UNCERTAINTY_ASSIGNED_CONTEXT ( ( #32375 ) ) GLOBAL_UNIT_ASSIGNED_CONTEXT ( ( #25774, #54560, #26389 ) ) REPRESENTATION_CONTEXT ( 'NONE', 'WORKASPACE' ) );
#40457 = B_SPLINE_CURVE_WITH_KNOTS ( 'NONE', 3,
 ( #42665, #15086, #47663, #4709 ),
 .UNSPECIFIED., .F., .F.,
 ( 4, 4 ),
 ( 0.000000000000000000, 0.005004948556313801832 ),
 .UNSPECIFIED. ) ;
#40458 = B_SPLINE_CURVE_WITH_KNOTS ( 'NONE', 3,
 ( #32854, #53681, #10812, #33154, #52229, #29899 ),
 .UNSPECIFIED., .F., .F.,
 ( 4, 2, 4 ),
 ( 1.015220885719448790E-17, 0.0002291978881530158890, 0.0004583957763060215866 ),
 .UNSPECIFIED. ) ;
#40459 = CARTESIAN_POINT ( 'NONE',  ( 5.974727161628367256, -7.868887636447487566, -18.95664195401514007 ) ) ;
#40460 = ORIENTED_EDGE ( 'NONE', *, *, #48464, .F. ) ;
#40461 = CARTESIAN_POINT ( 'NONE',  ( 4.549368137175248350, 40.58005590356690817, -13.99871866169321599 ) ) ;
#40462 = CARTESIAN_POINT ( 'NONE',  ( 0.8751705887134423323, 13.30665218149362516, -46.21789262997744885 ) ) ;
#40463 = CARTESIAN_POINT ( 'NONE',  ( 0.1158516988532803382, -35.33224402766282424, 26.43056357330432604 ) ) ;
#40464 = CARTESIAN_POINT ( 'NONE',  ( 5.959828726073459926, 20.35060134307034829, -2.674641840415962868 ) ) ;
#40465 = CARTESIAN_POINT ( 'NONE',  ( 4.956653778116975495, 15.97476558431885252, 45.35992544608534160 ) ) ;
#40466 = EDGE_CURVE ( 'NONE', #9584, #37089, #718, .T. ) ;
#40467 = LINE ( 'NONE', #2199, #53020 ) ;
#40468 = CARTESIAN_POINT ( 'NONE',  ( 5.959828726073459926, -19.82504517499708996, -5.316791119501019125 ) ) ;
#40469 = DIRECTION ( 'NONE',  ( 0.000000000000000000, 0.000000000000000000, 1.000000000000000000 ) ) ;
#40470 = ADVANCED_FACE ( 'NONE', ( #53631 ), #5184, .F. ) ;
#40471 = EDGE_CURVE ( 'NONE', #47638, #46904, #43560, .T. ) ;
#40472 = DIRECTION ( 'NONE',  ( 0.000000000000000000, 0.000000000000000000, -1.000000000000000000 ) ) ;
#40473 = CARTESIAN_POINT ( 'NONE',  ( 5.896278296736517710, 20.06757494133106690, 1.348857141599983489 ) ) ;
#40474 = EDGE_LOOP ( 'NONE', ( #30999, #11829, #9292, #283 ) ) ;
#40475 = CARTESIAN_POINT ( 'NONE',  ( 3.894904216938898323, -3.630410452522087272, -43.80575821079255405 ) ) ;
#40476 = CARTESIAN_POINT ( 'NONE',  ( 0.5834872094924179464, 46.20467604622299262, 12.61552836343307327 ) ) ;
#40477 = DIRECTION ( 'NONE',  ( 0.000000000000000000, 0.000000000000000000, 1.000000000000000000 ) ) ;
#40478 = VERTEX_POINT ( 'NONE', #33646 ) ;
#40479 = FACE_OUTER_BOUND ( 'NONE', #25999, .T. ) ;
#40480 = CARTESIAN_POINT ( 'NONE',  ( 1.088908134280555329, -4.826714665689156192, 42.64123480278976075 ) ) ;
#40481 = DIRECTION ( 'NONE',  ( 0.07906939808003035641, 0.02523889567980490412, 0.9965495614529794599 ) ) ;
#40482 = ORIENTED_EDGE ( 'NONE', *, *, #3713, .T. ) ;
#40483 = CARTESIAN_POINT ( 'NONE',  ( 4.691466044806102076, 33.30232861642391384, 29.64918311951140595 ) ) ;
#40484 = SHAPE_REPRESENTATION ( 'instrument roller bearing_iso_ISO 1224 - 171015 - R,24,SI,NC,24', ( #14677 ), #6659 ) ;
#40485 = DIRECTION ( 'NONE',  ( 0.1024043820194936311, -0.9844298967354744301, 0.1428674944015907999 ) ) ;
#40486 = VECTOR ( 'NONE', #16444, 1000.000000000000114 ) ;
#40487 = ADVANCED_FACE ( 'NONE', ( #43994 ), #58788, .F. ) ;
#40488 = ORIENTED_EDGE ( 'NONE', *, *, #30370, .F. ) ;
#40489 = CARTESIAN_POINT ( 'NONE',  ( 2.643462169533600914, -38.93558293168558748, 28.13401304854654938 ) ) ;
#40490 = B_SPLINE_CURVE_WITH_KNOTS ( 'NONE', 3,
 ( #29260, #24883, #119, #53975, #29879, #19892, #5128, #44322, #48076, #33675, #30181, #15184, #25481, #52757, #6042, #20487 ),
 .UNSPECIFIED., .F., .F.,
 ( 4, 3, 3, 3, 3, 4 ),
 ( 1.962735358247463844E-17, 0.0002612764279487724581, 0.0003919131003184757214, 0.0005225497727000657979, 0.0007837925190632480648, 0.001045051706266718252 ),
 .UNSPECIFIED. ) ;
#40492 = ORIENTED_EDGE ( 'NONE', *, *, #30542, .T. ) ;
#40491 = EDGE_CURVE ( 'NONE', #47841, #27088, #32651, .T. ) ;
#40493 = ORIENTED_EDGE ( 'NONE', *, *, #26383, .F. ) ;
#40494 = CARTESIAN_POINT ( 'NONE',  ( 0.1156495703730067298, 44.04204243056376100, 2.690994569948411907 ) ) ;
#40495 = EDGE_LOOP ( 'NONE', ( #42885, #35044, #28053, #22051 ) ) ;
#40496 = CARTESIAN_POINT ( 'NONE',  ( -6.077587904424778920, 19.25606354205735116, -0.006185319731011218458 ) ) ;
#40497 = VECTOR ( 'NONE', #4074, 1000.000000000000114 ) ;
#40498 = ORIENTED_EDGE ( 'NONE', *, *, #36817, .F. ) ;
#40499 = CARTESIAN_POINT ( 'NONE',  ( 3.238018933889920792, -4.230209958195113806, 12.70876925895028897 ) ) ;
#40500 = ADVANCED_FACE ( 'NONE', ( #38663 ), #46394, .F. ) ;
#40501 = CARTESIAN_POINT ( 'NONE',  ( 0.5980894510889457338, -5.583794302585608271, 47.78766676462066698 ) ) ;
#40502 = B_SPLINE_CURVE_WITH_KNOTS ( 'NONE', 3,
 ( #12478, #31570, #36289, #22175, #45688, #41008, #50662, #3347, #60068, #17174, #55665, #7747, #41302, #60358, #17474, #4267, #9932, #56902, #24328 ),
 .UNSPECIFIED., .F., .F.,
 ( 4, 3, 3, 3, 3, 3, 4 ),
 ( 4.907736672678014827E-18, 0.0002724573126191874107, 0.0004086839781548697818, 0.0005449106435902069650, 0.0006811373090491784545, 0.0008459866663933876974, 0.001010840725717217919 ),
 .UNSPECIFIED. ) ;
#40503 = VERTEX_POINT ( 'NONE', #38973 ) ;
#40504 = B_SPLINE_CURVE_WITH_KNOTS ( 'NONE', 3,
 ( #39761, #44464, #25021, #20326, #44162, #54108, #20627, #573, #58499, #30016, #15934, #1491, #1191, #39445, #15629, #11231, #35052, #19707, #33816 ),
 .UNSPECIFIED., .F., .F.,
 ( 4, 3, 3, 3, 3, 3, 4 ),
 ( 9.813676791237319219E-18, 0.0002732106629380643835, 0.0004098138914053805820, 0.0005464171197651613264, 0.0006830203481512775584, 0.0008196235766963826065, 0.001011968216111132053 ),
 .UNSPECIFIED. ) ;
#40505 = FACE_OUTER_BOUND ( 'NONE', #698, .T. ) ;
#40506 = CARTESIAN_POINT ( 'NONE',  ( 0.1104177457020373010, -30.49013195371476570, 30.49705356371253018 ) ) ;
#40507 = CARTESIAN_POINT ( 'NONE',  ( 0.9789233960466710016, 35.99109370129050234, 21.47039592129751284 ) ) ;
#40508 = ORIENTED_EDGE ( 'NONE', *, *, #61847, .F. ) ;
#40509 = EDGE_CURVE ( 'NONE', #28286, #2384, #25558, .T. ) ;
#40510 = ORIENTED_EDGE ( 'NONE', *, *, #34754, .T. ) ;
#40511 = CARTESIAN_POINT ( 'NONE',  ( 0.1102144999581333440, 41.62223437741653953, 11.28312052188161907 ) ) ;
#40512 = EDGE_CURVE ( 'NONE', #5770, #25596, #15146, .T. ) ;
#40513 = LINE ( 'NONE', #58326, #20474 ) ;
#40514 = AXIS2_PLACEMENT_3D ( 'NONE', #18348, #8603, #4817 ) ;
#40515 = CARTESIAN_POINT ( 'NONE',  ( 4.390527457369401532, 12.80762060415681525, -42.02558971732101156 ) ) ;
#40516 = ORIENTED_EDGE ( 'NONE', *, *, #44516, .F. ) ;
#40517 = CARTESIAN_POINT ( 'NONE',  ( 30.00000000000001066, 4.342925291379521108E-15, -1.386669559958810165E-30 ) ) ;
#40518 = PLANE ( 'NONE',  #53280 ) ;
#40519 = CARTESIAN_POINT ( 'NONE',  ( 0.9762797500689124330, -34.26226594605947895, 24.13341909939818564 ) ) ;
#40520 = FACE_OUTER_BOUND ( 'NONE', #31250, .T. ) ;
#40521 = ORIENTED_EDGE ( 'NONE', *, *, #7992, .F. ) ;
#40522 = ORIENTED_EDGE ( 'NONE', *, *, #34726, .F. ) ;
#40523 = CARTESIAN_POINT ( 'NONE',  ( 0.5806925824938502512, 22.05663578530182889, -41.38510819338409163 ) ) ;
#40524 = CARTESIAN_POINT ( 'NONE',  ( 2.879087469061463178, 42.27281810937363815, 12.21108209272179401 ) ) ;
#40525 = CARTESIAN_POINT ( 'NONE',  ( 0.9752570700956809668, -16.63323182627896202, 39.55341424149101925 ) ) ;
#40526 = DIRECTION ( 'NONE',  ( -0.000000000000000000, -0.000000000000000000, 1.000000000000000000 ) ) ;
#40527 = B_SPLINE_CURVE_WITH_KNOTS ( 'NONE', 3,
 ( #17605, #56107, #55799, #26686, #41129, #7245 ),
 .UNSPECIFIED., .F., .F.,
 ( 4, 2, 4 ),
 ( 1.520334456564901176E-16, 0.0002445252820015204908, 0.0004890505640028888681 ),
 .UNSPECIFIED. ) ;
#40528 = DIRECTION ( 'NONE',  ( -0.07836865515943411409, -0.3887811538706065217, -0.9179910502197401456 ) ) ;
#40529 = AXIS2_PLACEMENT_3D ( 'NONE', #12465, #17463, #26548 ) ;
#40530 = CARTESIAN_POINT ( 'NONE',  ( 0.7056759521545020730, -24.52215593799390447, -39.98015379247183887 ) ) ;
#40531 = CARTESIAN_POINT ( 'NONE',  ( 0.1073791018717483448, -6.109314776652422729, -42.68962945260951614 ) ) ;
#40532 = CARTESIAN_POINT ( 'NONE',  ( 0.5998501479064699549, -5.759754759341138453, 47.76154736470748219 ) ) ;
#40533 = CARTESIAN_POINT ( 'NONE',  ( 4.975801465491694664, 8.787181743659507660, 47.10002938642145409 ) ) ;
#40534 = CARTESIAN_POINT ( 'NONE',  ( 0.8554163680231720024, 33.26717477998049333, 33.08323677136276331 ) ) ;
#40535 = EDGE_CURVE ( 'NONE', #41641, #24034, #21692, .T. ) ;
#40536 = CARTESIAN_POINT ( 'NONE',  ( 0.8557997880470697982, 29.88293891557470516, 37.44587306708108088 ) ) ;
#40537 = AXIS2_PLACEMENT_3D ( 'NONE', #45661, #60337, #51557 ) ;
#40538 = CARTESIAN_POINT ( 'NONE',  ( 3.727782113643637540, 41.00064633199524877, -15.86583676534648824 ) ) ;
#40539 = B_SPLINE_CURVE_WITH_KNOTS ( 'NONE', 3,
 ( #1005, #39884, #5681, #57691 ),
 .UNSPECIFIED., .F., .F.,
 ( 4, 4 ),
 ( 0.000000000000000000, 0.004445488388166993383 ),
 .UNSPECIFIED. ) ;
#40540 = CARTESIAN_POINT ( 'NONE',  ( 4.975610109902397937, 45.11887670192734134, 18.88746601040093154 ) ) ;
#40541 = CARTESIAN_POINT ( 'NONE',  ( 2.955597489168904524, 0.3322054216400753268, -43.99767708311318160 ) ) ;
#40543 = EDGE_CURVE ( 'NONE', #34863, #1980, #28547, .T. ) ;
#40542 = CARTESIAN_POINT ( 'NONE',  ( 4.833616638992205949, -35.06988470649588407, 30.15290813935842351 ) ) ;
#40544 = DIRECTION ( 'NONE',  ( 0.07500201931887538753, -0.4673421949333655956, -0.8808893062882278135 ) ) ;
#40545 = EDGE_CURVE ( 'NONE', #10882, #11927, #39685, .T. ) ;
#40546 = CARTESIAN_POINT ( 'NONE',  ( 0.6001305935487422083, -47.76436356026964347, -5.760103278697848772 ) ) ;
#40547 = CARTESIAN_POINT ( 'NONE',  ( 0.6021448801613057400, 48.15124027138728025, 9.643609228607319395 ) ) ;
#40548 = EDGE_CURVE ( 'NONE', #27319, #26757, #12669, .T. ) ;
#40550 = VERTEX_POINT ( 'NONE', #40837 ) ;
#40549 = CARTESIAN_POINT ( 'NONE',  ( 5.894904586330512508, 17.95060305802250511, 9.072224750024437512 ) ) ;
#40551 = VERTEX_POINT ( 'NONE', #30152 ) ;
#40552 = DIRECTION ( 'NONE',  ( -1.000000000000000000, 0.000000000000000000, 0.000000000000000000 ) ) ;
#40553 = CARTESIAN_POINT ( 'NONE',  ( 0.7413678028165010536, 3.304446308179310954, -43.97234046951110287 ) ) ;
#40554 = ADVANCED_FACE ( 'NONE', ( #11070 ), #33219, .F. ) ;
#40555 = CARTESIAN_POINT ( 'NONE',  ( 0.6001305935487315502, -47.62765676940938420, -6.798494447612060121 ) ) ;
#40556 = ORIENTED_EDGE ( 'NONE', *, *, #27151, .F. ) ;
#40557 = ORIENTED_EDGE ( 'NONE', *, *, #17270, .F. ) ;
#40558 = CARTESIAN_POINT ( 'NONE',  ( 3.894904216938897434, -29.98771076940676750, 32.13816322204189646 ) ) ;
#40559 = CARTESIAN_POINT ( 'NONE',  ( 0.1087620492084205442, -37.52665900408533872, 21.24797679669894990 ) ) ;
#40560 =( BOUNDED_SURFACE ( )  B_SPLINE_SURFACE ( 3, 1, ( 
 ( #21783, #21465 ),
 ( #44995, #11156 ),
 ( #49655, #20549 ),
 ( #40302, #15545 ) ),
 .UNSPECIFIED., .F., .F., .F. ) 
 B_SPLINE_SURFACE_WITH_KNOTS ( ( 4, 4 ),
 ( 2, 2 ),
 ( 0.000000000000000000, 1.000000000000000000 ),
 ( 0.000000000000000000, 1.000000000000000000 ),
 .UNSPECIFIED. ) 
 GEOMETRIC_REPRESENTATION_ITEM ( )  RATIONAL_B_SPLINE_SURFACE ( (
 ( 1.000000000000000000, 1.000000000000000000),
 ( 0.7223157951917476005, 0.9931996967497186413),
 ( 0.7223157951917476005, 0.9931996967497186413),
 ( 1.000000000000000000, 1.000000000000000000) ) ) 
 REPRESENTATION_ITEM ( '' )  SURFACE ( )  );
#40561 = B_SPLINE_CURVE_WITH_KNOTS ( 'NONE', 3,
 ( #985, #53593, #57364, #43014, #53294, #15414, #38617, #352, #15109, #34525, #53, #19202, #58289, #43631, #19502, #33915 ),
 .UNSPECIFIED., .F., .F.,
 ( 4, 3, 3, 3, 3, 4 ),
 ( 1.250973872328959318E-17, 0.0002724568934985643833, 0.0004086836638483846464, 0.0005449104342063632598, 0.0008173270854453735038, 0.001089761613562689009 ),
 .UNSPECIFIED. ) ;
#40562 = ORIENTED_EDGE ( 'NONE', *, *, #58886, .F. ) ;
#40563 = EDGE_LOOP ( 'NONE', ( #29207, #1536, #22736, #49559, #24825, #7791, #13081, #18838, #48081, #22230, #40806, #53570, #2645, #11038, #18107, #18745, #24505, #21233, #16374, #38825, #46876, #52033, #31761, #35729, #52821, #6853, #40776, #22062, #24142, #12472, #9877, #41428, #48046, #23894, #61170, #19923, #39023, #32460, #36716, #48448, #57766, #36419, #54477, #57161, #7221, #52551, #60630, #26430, #6209, #52890, #50620, #20523, #21117, #18920, #48567, #2818, #37268, #53879, #6425, #47757, #41527, #60347, #60093, #10996, #43251, #29651, #57943, #10724, #8418, #5276, #43898, #31699, #7178, #61242, #48346, #28098, #49099, #11666, #12155, #48318, #53459, #53985, #28966, #60334, #26197, #50952, #29000, #40024, #56231, #52009, #617, #9107, #17455, #7547, #5139, #17014, #1707, #49856, #22728, #2141, #40134, #27514, #4821, #3240, #52078, #6695, #31746, #43900, #42177, #57923, #17223, #51562, #18924, #7538, #50909, #32485, #40842, #50129, #24384, #74, #58478, #174, #1979, #20441, #19083, #27842, #35630, #59238, #53273, #57477, #24784, #7157, #23431, #49681, #28617, #34147, #57244, #39668, #29081, #55631, #1612, #57034, #54496, #9678, #47106, #46655, #47903, #54306 ) ) ;
#40564 = ADVANCED_FACE ( 'NONE', ( #44913 ), #16370, .F. ) ;
#40565 = CARTESIAN_POINT ( 'NONE',  ( 30.00000000000001066, 4.342925291379521108E-15, -1.386669559958810165E-30 ) ) ;
#40566 = CARTESIAN_POINT ( 'NONE',  ( 0.5807400328401574052, 44.45848844984443105, 17.82553128098425077 ) ) ;
#40567 = CARTESIAN_POINT ( 'NONE',  ( 0.5837157313716032636, -38.61143574556265179, -26.61567382668169301 ) ) ;
#40568 = ORIENTED_EDGE ( 'NONE', *, *, #40198, .T. ) ;
#40569 = CARTESIAN_POINT ( 'NONE',  ( -6.015611763856276717, -2.453375430804198398, 18.68284711750057525 ) ) ;
#40570 = DIRECTION ( 'NONE',  ( 1.836766033387207149E-16, -1.000000000000000000, 0.000000000000000000 ) ) ;
#40571 = B_SPLINE_CURVE_WITH_KNOTS ( 'NONE', 3,
 ( #54577, #49587, #58985, #39297, #6643, #10466 ),
 .UNSPECIFIED., .F., .F.,
 ( 4, 2, 4 ),
 ( 1.084202172485504434E-19, 0.0002445244328975368061, 0.0004890488657950735037 ),
 .UNSPECIFIED. ) ;
#40572 = CARTESIAN_POINT ( 'NONE',  ( 0.3676999524040366896, 43.96170928169366476, -3.649479463524768263 ) ) ;
#40573 = EDGE_LOOP ( 'NONE', ( #19363, #55124, #56460, #37500 ) ) ;
#40574 = VERTEX_POINT ( 'NONE', #12015 ) ;
#40575 = CARTESIAN_POINT ( 'NONE',  ( -6.078726893082806448, -1.852420388636693227, 19.16670498475111373 ) ) ;
#40576 = CARTESIAN_POINT ( 'NONE',  ( 0.1365634738349428001, -40.65536331164525308, -17.14654640507459149 ) ) ;
#40577 = VECTOR ( 'NONE', #33614, 1000.000000000000000 ) ;
#40578 = VERTEX_POINT ( 'NONE', #40519 ) ;
#40579 = CARTESIAN_POINT ( 'NONE',  ( 0.6016117650947689910, -48.65860227857874776, 6.625064417769112701 ) ) ;
#40580 = CARTESIAN_POINT ( 'NONE',  ( 0.1368894036331304576, 37.32310111198702884, 23.53396373983203915 ) ) ;
#40581 = CARTESIAN_POINT ( 'NONE',  ( 0.6031356219577718170, 46.49081620741438314, 12.36679943215677113 ) ) ;
#40582 = CARTESIAN_POINT ( 'NONE',  ( 3.050102900204245682, -43.82680816383815880, -3.825720239143000523 ) ) ;
#40583 = CONICAL_SURFACE ( 'NONE', #13556, 42.92674063221959813, 1.485477209440487556 ) ;
#40584 = EDGE_CURVE ( 'NONE', #43185, #7798, #4670, .T. ) ;
#40585 = ORIENTED_EDGE ( 'NONE', *, *, #14789, .T. ) ;
#40586 = CARTESIAN_POINT ( 'NONE',  ( 1.231276596079887931, 40.64579686208652731, 10.25650859035686757 ) ) ;
#40587 = CARTESIAN_POINT ( 'NONE',  ( 0.6023143664670691511, 18.16777128831328625, 44.54505257464866474 ) ) ;
#40588 = FACE_OUTER_BOUND ( 'NONE', #42634, .T. ) ;
#40589 = ADVANCED_FACE ( 'NONE', ( #42367 ), #1168, .F. ) ;
#40590 = CARTESIAN_POINT ( 'NONE',  ( 0.9752570700956793015, -21.25416333281073022, -37.27462300504097925 ) ) ;
#40591 = EDGE_LOOP ( 'NONE', ( #61093, #51632, #46748, #37866 ) ) ;
#40592 = CARTESIAN_POINT ( 'NONE',  ( 5.959547316686252039, -19.82530672674365846, 5.315863417545987346 ) ) ;
#40593 = CARTESIAN_POINT ( 'NONE',  ( 0.5786265663353196143, -5.535668456753627176, -47.58023467411543095 ) ) ;
#40594 = DIRECTION ( 'NONE',  ( 0.09722883295013592941, 0.2140925343086658994, -0.9719624173785975652 ) ) ;
#40595 = CARTESIAN_POINT ( 'NONE',  ( 0.8751705887134423323, 7.160166390004303771, -47.55935879196464100 ) ) ;
#40596 = ORIENTED_EDGE ( 'NONE', *, *, #45528, .F. ) ;
#40597 = B_SPLINE_CURVE_WITH_KNOTS ( 'NONE', 3,
 ( #34711, #53775, #10907, #6158 ),
 .UNSPECIFIED., .F., .F.,
 ( 4, 4 ),
 ( 0.000000000000000000, 0.004444103432399266161 ),
 .UNSPECIFIED. ) ;
#40598 = CARTESIAN_POINT ( 'NONE',  ( -6.072942160501519915, 15.42355008158977192, -11.52901839575739373 ) ) ;
#40599 = LINE ( 'NONE', #31477, #21674 ) ;
#40600 = PRODUCT_DEFINITION ( 'UNKNOWN', '', #19936, #30423 ) ;
#40601 = FACE_OUTER_BOUND ( 'NONE', #33314, .T. ) ;
#40602 = CARTESIAN_POINT ( 'NONE',  ( 1.157644175074337811, -23.24616985789975132, 34.88004963323383834 ) ) ;
#40603 = CARTESIAN_POINT ( 'NONE',  ( 0.5837157313716030416, -46.79729193653216868, 3.041468557951020557 ) ) ;
#40604 = CARTESIAN_POINT ( 'NONE',  ( 0.5839879882012674051, 46.26394433311401855, -12.39641777360473540 ) ) ;
#40605 = CARTESIAN_POINT ( 'NONE',  ( 0.9757402383260934675, -5.516496958496793113, -42.55239275983117864 ) ) ;
#40606 = CARTESIAN_POINT ( 'NONE',  ( 0.1100247026804066219, -41.61078157869243910, -11.32523219034893636 ) ) ;
#40607 = FACE_OUTER_BOUND ( 'NONE', #31752, .T. ) ;
#40608 = CARTESIAN_POINT ( 'NONE',  ( 0.5839880159502344181, 37.97080096460581444, 29.19321933421507964 ) ) ;
#40609 = CARTESIAN_POINT ( 'NONE',  ( 4.967162193818130511, 0.000000000000000000, 0.000000000000000000 ) ) ;
#40610 = ORIENTED_EDGE ( 'NONE', *, *, #57972, .F. ) ;
#40611 = CARTESIAN_POINT ( 'NONE',  ( -17.97369999999976642, -12.32233744059949210, -2.099999999999997424 ) ) ;
#40612 = CARTESIAN_POINT ( 'NONE',  ( 4.834790513006553603, -4.078087887155715130, -47.07396881620473295 ) ) ;
#40613 = CARTESIAN_POINT ( 'NONE',  ( 0.5809828226811544205, 5.711058609466008740, -47.55412398569200150 ) ) ;
#40614 = DIRECTION ( 'NONE',  ( -1.000000000000000000, -0.000000000000000000, -0.000000000000000000 ) ) ;
#40615 = FACE_OUTER_BOUND ( 'NONE', #41289, .T. ) ;
#40616 = SHAPE_DEFINITION_REPRESENTATION ( #18325, #16880 ) ;
#40618 = EDGE_CURVE ( 'NONE', #21198, #41494, #51109, .T. ) ;
#40617 = CARTESIAN_POINT ( 'NONE',  ( 4.975610109902397937, 24.86209007718959185, 42.12274782266089801 ) ) ;
#40619 = CARTESIAN_POINT ( 'NONE',  ( 4.226256110419178924, 35.46064522245336548, -25.94937167629463204 ) ) ;
#40620 = EDGE_CURVE ( 'NONE', #33924, #58761, #3141, .T. ) ;
#40621 = DIRECTION ( 'NONE',  ( -0.1011922191286467460, -0.8407325376063348177, 0.5319106456895111856 ) ) ;
#40622 = ADVANCED_FACE ( 'NONE', ( #31404 ), #57254, .F. ) ;
#40624 = VERTEX_POINT ( 'NONE', #51731 ) ;
#40623 = CARTESIAN_POINT ( 'NONE',  ( 5.860006189529234355, 9.426589201135499252, 47.30296539008827494 ) ) ;
#40625 = ORIENTED_EDGE ( 'NONE', *, *, #55343, .T. ) ;
#40626 = CARTESIAN_POINT ( 'NONE',  ( 0.9722240750034575330, 42.46141201102052776, -6.177112354444691533 ) ) ;
#40627 = VECTOR ( 'NONE', #50545, 1000.000000000000000 ) ;
#40628 = DIRECTION ( 'NONE',  ( 0.07906939808003035641, 0.8933371237230053330, -0.4423763258421154476 ) ) ;
#40629 = EDGE_CURVE ( 'NONE', #8248, #14950, #14373, .T. ) ;
#40630 = CARTESIAN_POINT ( 'NONE',  ( 2.526552050251864134, 41.18423939305565540, 12.29062829843992688 ) ) ;
#40631 = AXIS2_PLACEMENT_3D ( 'NONE', #32053, #61748, #41774 ) ;
#40632 = ORIENTED_EDGE ( 'NONE', *, *, #35856, .T. ) ;
#40633 = CARTESIAN_POINT ( 'NONE',  ( 5.958863334805807099, 5.311251202228577384, 19.82657410201445103 ) ) ;
#40634 = CARTESIAN_POINT ( 'NONE',  ( 0.6254087463353918963, 0.6881259009461112575, 48.10157520235527073 ) ) ;
#40635 = DIRECTION ( 'NONE',  ( 0.000000000000000000, 0.000000000000000000, 1.000000000000000000 ) ) ;
#40636 = ORIENTED_EDGE ( 'NONE', *, *, #57282, .F. ) ;
#40637 = VERTEX_POINT ( 'NONE', #12934 ) ;
#40638 = CARTESIAN_POINT ( 'NONE',  ( 4.975801465491694664, -47.10002938642148251, 8.787181743659342459 ) ) ;
#40639 =( BOUNDED_SURFACE ( )  B_SPLINE_SURFACE ( 3, 1, ( 
 ( #49886, #25447 ),
 ( #31088, #39900 ),
 ( #30146, #35807 ),
 ( #50191, #16072 ) ),
 .UNSPECIFIED., .F., .F., .F. ) 
 B_SPLINE_SURFACE_WITH_KNOTS ( ( 4, 4 ),
 ( 2, 2 ),
 ( 0.000000000000000000, 1.000000000000000000 ),
 ( 0.000000000000000000, 1.000000000000000000 ),
 .UNSPECIFIED. ) 
 GEOMETRIC_REPRESENTATION_ITEM ( )  RATIONAL_B_SPLINE_SURFACE ( (
 ( 1.000000000000000000, 1.000000000000000000),
 ( 0.9952954269826590483, 0.8620686068821307169),
 ( 0.9952954269826590483, 0.8620686068821307169),
 ( 1.000000000000000000, 1.000000000000000000) ) ) 
 REPRESENTATION_ITEM ( '' )  SURFACE ( )  );
#40640 = CIRCLE ( 'NONE', #21609, 42.92674063221959813 ) ;
#40641 = CARTESIAN_POINT ( 'NONE',  ( 3.270143674763207553, -13.68510027222513159, -0.2742231296311014588 ) ) ;
#40642 = CARTESIAN_POINT ( 'NONE',  ( 40.00000000000001421, -72.00000000000001421, 8.817456953860944867E-15 ) ) ;
#40643 = VERTEX_POINT ( 'NONE', #56118 ) ;
#40644 = ORIENTED_EDGE ( 'NONE', *, *, #15524, .T. ) ;
#40645 = CARTESIAN_POINT ( 'NONE',  ( -6.077587904424778920, 9.976910903713122281, -16.46988980574249695 ) ) ;
#40646 = CARTESIAN_POINT ( 'NONE',  ( 0.5998501479064708430, 0.5236536531314925913, -48.10473956285919428 ) ) ;
#40647 = ORIENTED_EDGE ( 'NONE', *, *, #36870, .F. ) ;
#40648 = B_SPLINE_CURVE_WITH_KNOTS ( 'NONE', 3,
 ( #50256, #40280, #30515, #34946 ),
 .UNSPECIFIED., .F., .F.,
 ( 4, 4 ),
 ( 5.057544569639794935E-18, 0.004566006591234646368 ),
 .UNSPECIFIED. ) ;
#40649 = CARTESIAN_POINT ( 'NONE',  ( 0.6000166863083090663, 28.52380356231368097, 39.97769518177598513 ) ) ;
#40650 = CARTESIAN_POINT ( 'NONE',  ( -31.74999999999995737, 0.000000000000000000, 2.500000000000000444 ) ) ;
#40651 = ORIENTED_EDGE ( 'NONE', *, *, #33947, .T. ) ;
#40652 = CARTESIAN_POINT ( 'NONE',  ( -6.010958268070873523, 18.68034667844849039, 2.473955915502278113 ) ) ;
#40653 = PLANE ( 'NONE',  #59536 ) ;
#40654 = ORIENTED_EDGE ( 'NONE', *, *, #53441, .F. ) ;
#40655 = CARTESIAN_POINT ( 'NONE',  ( 0.6067099128993207469, -41.82996792600761893, -23.33192673707576859 ) ) ;
#40656 = CARTESIAN_POINT ( 'NONE',  ( 0.5834584762367743815, -19.90520019176333477, 42.46197115465809446 ) ) ;
#40657 = DIRECTION ( 'NONE',  ( 0.1736481776669316079, -0.9848077530122079093, -5.551115123125822145E-17 ) ) ;
#40658 = CARTESIAN_POINT ( 'NONE',  ( 0.8760168074887090262, -41.20610493656926820, 24.81951362746006140 ) ) ;
#40659 = ORIENTED_EDGE ( 'NONE', *, *, #43745, .T. ) ;
#40660 = DIRECTION ( 'NONE',  ( -1.000000000000000000, -0.000000000000000000, -0.000000000000000000 ) ) ;
#40661 = CARTESIAN_POINT ( 'NONE',  ( 0.6023142530420679819, 44.34465601638699894, -18.65157113320505644 ) ) ;
#40662 = ORIENTED_EDGE ( 'NONE', *, *, #6547, .F. ) ;
#40663 = CARTESIAN_POINT ( 'NONE',  ( 5.895881250540457863, 8.470336106973904933, 18.24228844863481314 ) ) ;
#40664 = EDGE_CURVE ( 'NONE', #14433, #4518, #925, .T. ) ;
#40665 = B_SPLINE_CURVE_WITH_KNOTS ( 'NONE', 3,
 ( #57485, #48129, #30235, #6399, #58417, #10525 ),
 .UNSPECIFIED., .F., .F.,
 ( 4, 2, 4 ),
 ( 3.476216610979977084E-18, 0.0002291966416970807048, 0.0004583932833941579401 ),
 .UNSPECIFIED. ) ;
#40666 = ORIENTED_EDGE ( 'NONE', *, *, #44992, .F. ) ;
#40667 = CARTESIAN_POINT ( 'NONE',  ( 0.9722240741986376555, -36.86535088273189587, -21.95618662952224298 ) ) ;
#40668 = ORIENTED_EDGE ( 'NONE', *, *, #44729, .F. ) ;
#40669 = CARTESIAN_POINT ( 'NONE',  ( 0.2224561200757600998, 41.44719785461212780, 11.89200283918804679 ) ) ;
#40670 = CARTESIAN_POINT ( 'NONE',  ( 0.5997462898726536595, -48.76843890605300658, -5.761162800241320880 ) ) ;
#40671 = CIRCLE ( 'NONE', #52606, 1.000000000000000888 ) ;
#40672 = CARTESIAN_POINT ( 'NONE',  ( 0.1103744047535531458, -26.28322091066901578, 34.18931094754994859 ) ) ;
#40673 = ORIENTED_EDGE ( 'NONE', *, *, #9060, .F. ) ;
#40674 = CARTESIAN_POINT ( 'NONE',  ( 4.999999999999996447, 2.649999999999721023, 80.00000000000002842 ) ) ;
#40675 = AXIS2_PLACEMENT_3D ( 'NONE', #29233, #57405, #38060 ) ;
#40676 = CARTESIAN_POINT ( 'NONE',  ( 0.9762797500689124330, -0.8945891712305065191, 41.89897964629235361 ) ) ;
#40677 = CARTESIAN_POINT ( 'NONE',  ( 4.549368137175248350, 0.000000000000000000, 0.000000000000000000 ) ) ;
#40678 = EDGE_LOOP ( 'NONE', ( #8192, #30295 ) ) ;
#40679 = ORIENTED_EDGE ( 'NONE', *, *, #34078, .F. ) ;
#40680 = LINE ( 'NONE', #2418, #32517 ) ;
#40681 = CARTESIAN_POINT ( 'NONE',  ( 0.5786265663353196143, -46.45062944555901652, 11.69877690266638481 ) ) ;
#40682 = CARTESIAN_POINT ( 'NONE',  ( 0.6024113833632039894, 32.85349838899362851, 36.49917139751612893 ) ) ;
#40683 = CARTESIAN_POINT ( 'NONE',  ( 0.8744876279028306332, -14.81965677137948489, -46.80521149998148900 ) ) ;
#40684 = CARTESIAN_POINT ( 'NONE',  ( 0.8557997880470599172, -38.55640757422458620, 28.43566216844957140 ) ) ;
#40685 = CARTESIAN_POINT ( 'NONE',  ( 0.5988103622719991304, -37.79415722405575906, -29.76496569135148107 ) ) ;
#40686 = VERTEX_POINT ( 'NONE', #3490 ) ;
#40687 = VECTOR ( 'NONE', #60763, 1000.000000000000227 ) ;
#40688 = CARTESIAN_POINT ( 'NONE',  ( 5.981074661064941900, -2.670494474391857942, -20.35019299530687320 ) ) ;
#40689 = CARTESIAN_POINT ( 'NONE',  ( 1.227938101723756947, 39.32113113558990847, -17.20315230597801914 ) ) ;
#40690 = ORIENTED_EDGE ( 'NONE', *, *, #4241, .F. ) ;
#40691 = DIRECTION ( 'NONE',  ( 0.000000000000000000, 0.000000000000000000, 1.000000000000000000 ) ) ;
#40692 = CARTESIAN_POINT ( 'NONE',  ( 0.5835871038041856584, 36.71915229544869419, 29.17084687843575708 ) ) ;
#40693 = CARTESIAN_POINT ( 'NONE',  ( 5.896782393890504181, -2.019528367549316084, -20.01118667272572793 ) ) ;
#40694 = CARTESIAN_POINT ( 'NONE',  ( -6.675040713419566174, 8.977276343754100552, -2.131574760800940707E-15 ) ) ;
#40695 = CARTESIAN_POINT ( 'NONE',  ( 0.8551540677456715978, 23.16399837394545713, 41.94570365541211743 ) ) ;
#40696 = CARTESIAN_POINT ( 'NONE',  ( 4.956653778116975495, -20.77844580450591394, 43.37017594958047084 ) ) ;
#40697 = B_SPLINE_CURVE_WITH_KNOTS ( 'NONE', 3,
 ( #49726, #60339, #7095, #31237 ),
 .UNSPECIFIED., .F., .F.,
 ( 4, 4 ),
 ( 0.000000000000000000, 0.005004948556313814842 ),
 .UNSPECIFIED. ) ;
#40698 = CARTESIAN_POINT ( 'NONE',  ( 0.6029443449137436017, 4.672121757583973967, 48.88466851954346737 ) ) ;
#40700 = EDGE_CURVE ( 'NONE', #40643, #30048, #22670, .T. ) ;
#40699 = CARTESIAN_POINT ( 'NONE',  ( 0.1155031312995260795, -12.39291212668941355, -42.34805026860106381 ) ) ;
#40701 = CARTESIAN_POINT ( 'NONE',  ( 1.227938101723748288, -10.28900963485351205, -41.66816631169202623 ) ) ;
#40702 = EDGE_CURVE ( 'NONE', #48102, #20804, #1685, .T. ) ;
#40703 = CARTESIAN_POINT ( 'NONE',  ( 0.3676999524040366896, -28.14442808720893296, -33.96824621564622504 ) ) ;
#40704 = CARTESIAN_POINT ( 'NONE',  ( -6.015611763856276717, -17.40650793417848519, 7.216738110653220239 ) ) ;
#40705 = CARTESIAN_POINT ( 'NONE',  ( 5.965394784446458765, -10.27521535480974180, -17.76824826579351324 ) ) ;
#40706 = LINE ( 'NONE', #59779, #46249 ) ;
#40707 = EDGE_CURVE ( 'NONE', #15442, #25145, #60715, .T. ) ;
#40708 = CARTESIAN_POINT ( 'NONE',  ( 5.895596859100789899, -17.30333226730972385, -10.25294473112801619 ) ) ;
#40709 = CARTESIAN_POINT ( 'NONE',  ( 0.7948878604505658085, -45.82899947609774216, -17.61821370963155786 ) ) ;
#40710 = CARTESIAN_POINT ( 'NONE',  ( 4.549368137175248350, -23.67244292351665536, 35.80950303116058819 ) ) ;
#40711 = VERTEX_POINT ( 'NONE', #22941 ) ;
#40712 = VECTOR ( 'NONE', #48053, 1000.000000000000114 ) ;
#40713 = CARTESIAN_POINT ( 'NONE',  ( 0.1129192098497455998, 43.40062318508800843, -7.958498283668546947 ) ) ;
#40714 = EDGE_CURVE ( 'NONE', #31634, #44906, #35353, .T. ) ;
#40715 = CARTESIAN_POINT ( 'NONE',  ( 0.5835871038041854364, -19.61618793221725454, -42.59623955127298700 ) ) ;
#40716 = AXIS2_PLACEMENT_3D ( 'NONE', #21352, #26662, #11979 ) ;
#40717 = CARTESIAN_POINT ( 'NONE',  ( 0.1157506346131639274, -38.49163757259893259, -21.57161321696930401 ) ) ;
#40718 = CARTESIAN_POINT ( 'NONE',  ( 4.335381028904216727, 31.32980982056223951, -37.65899446708247211 ) ) ;
#40719 = B_SPLINE_CURVE_WITH_KNOTS ( 'NONE', 3,
 ( #40572, #49946, #35861, #11427, #49019, #59326 ),
 .UNSPECIFIED., .F., .F.,
 ( 4, 2, 4 ),
 ( 5.421010862427522170E-19, 0.0002293801035737090739, 0.0004587602071474176056 ),
 .UNSPECIFIED. ) ;
#40720 = CARTESIAN_POINT ( 'NONE',  ( 0.1103878639767399139, -41.64243544356636306, 11.20830530106120371 ) ) ;
#40721 = VECTOR ( 'NONE', #52860, 1000.000000000000000 ) ;
#40722 = ORIENTED_EDGE ( 'NONE', *, *, #6901, .F. ) ;
#40723 = EDGE_CURVE ( 'NONE', #26600, #24074, #46741, .T. ) ;
#40724 = CARTESIAN_POINT ( 'NONE',  ( 0.09136607875274982415, 9.539392014169456147, 3.000000000000000000 ) ) ;
#40725 = CARTESIAN_POINT ( 'NONE',  ( 0.6029443449137436017, -14.01413519038458055, 47.06531156647066183 ) ) ;
#40726 = ORIENTED_EDGE ( 'NONE', *, *, #24059, .T. ) ;
#40727 = CARTESIAN_POINT ( 'NONE',  ( 0.3622758884714600280, 43.10531414739104150, 0.8252992914329575491 ) ) ;
#40728 = ORIENTED_EDGE ( 'NONE', *, *, #38557, .F. ) ;
#40729 = AXIS2_PLACEMENT_3D ( 'NONE', #23887, #37384, #41788 ) ;
#40730 = DIRECTION ( 'NONE',  ( 0.09835009131224566048, 0.8656670924898616226, -0.4908642831975275067 ) ) ;
#40731 = DIRECTION ( 'NONE',  ( -1.000000000000000000, -1.836909530733573776E-16, 1.103352205049209901E-32 ) ) ;
#40732 = B_SPLINE_CURVE_WITH_KNOTS ( 'NONE', 3,
 ( #4894, #57504, #52207, #33751 ),
 .UNSPECIFIED., .F., .F.,
 ( 4, 4 ),
 ( 0.000000000000000000, 0.004447772540403782497 ),
 .UNSPECIFIED. ) ;
#40733 = ORIENTED_EDGE ( 'NONE', *, *, #9331, .T. ) ;
#40734 = CARTESIAN_POINT ( 'NONE',  ( -6.072942160501519027, 9.969886825815823528, 16.47438979050345864 ) ) ;
#40735 = ORIENTED_EDGE ( 'NONE', *, *, #33837, .T. ) ;
#40736 = CARTESIAN_POINT ( 'NONE',  ( 1.091591847532197956, 35.65871381344827995, 22.02759905496810333 ) ) ;
#40737 = CARTESIAN_POINT ( 'NONE',  ( 4.834790513006555379, 1.053669480798880009, -47.23853428663524312 ) ) ;
#40738 = AXIS2_PLACEMENT_3D ( 'NONE', #29042, #14961, #38772 ) ;
#40739 = VERTEX_POINT ( 'NONE', #327 ) ;
#40740 = B_SPLINE_CURVE_WITH_KNOTS ( 'NONE', 3,
 ( #37202, #8052, #32808, #7414, #56270, #8659 ),
 .UNSPECIFIED., .F., .F.,
 ( 4, 2, 4 ),
 ( 7.410741937918042371E-18, 0.0002291472222819936674, 0.0004582944445639799622 ),
 .UNSPECIFIED. ) ;
#40741 = CARTESIAN_POINT ( 'NONE',  ( 4.834790513006553603, 1.975078679466633957, -47.20898648704818612 ) ) ;
#40743 = VERTEX_POINT ( 'NONE', #5636 ) ;
#40742 =( BOUNDED_SURFACE ( )  B_SPLINE_SURFACE ( 3, 1, ( 
 ( #36578, #21231 ),
 ( #11529, #12780 ),
 ( #8051, #27165 ),
 ( #41589, #6788 ) ),
 .UNSPECIFIED., .F., .F., .F. ) 
 B_SPLINE_SURFACE_WITH_KNOTS ( ( 4, 4 ),
 ( 2, 2 ),
 ( 0.000000000000000000, 1.000000000000000000 ),
 ( 0.000000000000000000, 1.000000000000000000 ),
 .UNSPECIFIED. ) 
 GEOMETRIC_REPRESENTATION_ITEM ( )  RATIONAL_B_SPLINE_SURFACE ( (
 ( 1.000000000000000000, 1.000000000000000000),
 ( 0.7269869731126821222, 0.9931720237060910339),
 ( 0.7269869731126821222, 0.9931720237060910339),
 ( 1.000000000000000000, 1.000000000000000000) ) ) 
 REPRESENTATION_ITEM ( '' )  SURFACE ( )  );
#40744 = CARTESIAN_POINT ( 'NONE',  ( 0.5839254288179552832, -37.94310411505126268, -29.22920395911552305 ) ) ;
#40745 = EDGE_CURVE ( 'NONE', #58236, #42991, #54603, .T. ) ;
#40746 = VERTEX_POINT ( 'NONE', #647 ) ;
#40747 = VERTEX_POINT ( 'NONE', #48581 ) ;
#40748 = CARTESIAN_POINT ( 'NONE',  ( 4.549368137175248350, -42.14271863032838894, 8.166781970325002860 ) ) ;
#40749 = DIRECTION ( 'NONE',  ( -0.9848077530122079093, -0.1736481776669314414, 5.551115123125783935E-17 ) ) ;
#40750 = DIRECTION ( 'NONE',  ( -0.000000000000000000, 0.000000000000000000, 1.000000000000000000 ) ) ;
#40751 = CARTESIAN_POINT ( 'NONE',  ( 0.1098349054025746785, -16.69989664087480463, 39.75970464594237086 ) ) ;
#40752 = ORIENTED_EDGE ( 'NONE', *, *, #34200, .F. ) ;
#40753 = CARTESIAN_POINT ( 'NONE',  ( 0.9752570700956798566, 10.88256294660712697, 41.50550328400871081 ) ) ;
#40754 = CARTESIAN_POINT ( 'NONE',  ( -2.739355103387247858, -13.93362462427449167, 5.357394122222905786 ) ) ;
#40755 = CARTESIAN_POINT ( 'NONE',  ( -4.923482091946712380, -0.9563062221994939049, 3.000000000000061284 ) ) ;
#40756 = VERTEX_POINT ( 'NONE', #38286 ) ;
#40757 = ORIENTED_EDGE ( 'NONE', *, *, #18672, .T. ) ;
#40758 =( BOUNDED_SURFACE ( )  B_SPLINE_SURFACE ( 3, 1, ( 
 ( #57035, #5025 ),
 ( #51725, #14771 ),
 ( #42983, #29161 ),
 ( #23236, #43287 ) ),
 .UNSPECIFIED., .F., .F., .F. ) 
 B_SPLINE_SURFACE_WITH_KNOTS ( ( 4, 4 ),
 ( 2, 2 ),
 ( 0.000000000000000000, 1.000000000000000000 ),
 ( 0.000000000000000000, 1.000000000000000000 ),
 .UNSPECIFIED. ) 
 GEOMETRIC_REPRESENTATION_ITEM ( )  RATIONAL_B_SPLINE_SURFACE ( (
 ( 1.000000000000000000, 1.000000000000000000),
 ( 0.7282232189291693025, 0.9929344683865674037),
 ( 0.7282232189291693025, 0.9929344683865674037),
 ( 1.000000000000000000, 1.000000000000000000) ) ) 
 REPRESENTATION_ITEM ( '' )  SURFACE ( )  );
#40759 = CARTESIAN_POINT ( 'NONE',  ( 0.1073791018717578927, -33.91564619577789585, -26.63563652260155123 ) ) ;
#40760 = CARTESIAN_POINT ( 'NONE',  ( 4.975610109902397937, 7.237810502494091303, 48.37420290059321104 ) ) ;
#40761 = CARTESIAN_POINT ( 'NONE',  ( 1.231276596079887264, 40.19859528295904738, -11.88905834349085922 ) ) ;
#40762 = VERTEX_POINT ( 'NONE', #19475 ) ;
#40763 = CARTESIAN_POINT ( 'NONE',  ( 0.5988103564986355654, -34.44345003622227352, -33.58571500783047270 ) ) ;
#40764 = CARTESIAN_POINT ( 'NONE',  ( 2.706805983486680223, -34.25409726565154500, 27.63029015111926867 ) ) ;
#40765 = CARTESIAN_POINT ( 'NONE',  ( -18.24996621385825790, -12.32468876802673741, 2.086337228483194917 ) ) ;
#40766 = AXIS2_PLACEMENT_3D ( 'NONE', #22221, #12522, #31613 ) ;
#40767 = ORIENTED_EDGE ( 'NONE', *, *, #17206, .F. ) ;
#40768 = CARTESIAN_POINT ( 'NONE',  ( 2.643462169533613793, -32.97543604874699241, 34.93025802711668604 ) ) ;
#40769 = ORIENTED_EDGE ( 'NONE', *, *, #28775, .T. ) ;
#40770 = VECTOR ( 'NONE', #61944, 1000.000000000000000 ) ;
#40771 = CARTESIAN_POINT ( 'NONE',  ( 0.3622758884714730732, 31.06363466427686504, 29.89648521331642428 ) ) ;
#40772 = CARTESIAN_POINT ( 'NONE',  ( 4.956653778116990594, -20.77844580450529577, -43.37017594958076927 ) ) ;
#40773 = B_SPLINE_CURVE_WITH_KNOTS ( 'NONE', 3,
 ( #22627, #52042, #12939, #23860 ),
 .UNSPECIFIED., .F., .F.,
 ( 4, 4 ),
 ( 6.254634441385501517E-18, 0.004566006591234645501 ),
 .UNSPECIFIED. ) ;
#40774 = CARTESIAN_POINT ( 'NONE',  ( 2.299746137290199499, -18.66300477064106289, 45.34284497709828088 ) ) ;
#40775 = CARTESIAN_POINT ( 'NONE',  ( 0.5997462898726536595, -45.71211507932792273, 17.94308126043545215 ) ) ;
#40776 = ORIENTED_EDGE ( 'NONE', *, *, #54219, .T. ) ;
#40777 = CARTESIAN_POINT ( 'NONE',  ( 0.9749527285493307938, 21.70110358462093458, -37.01618455594552159 ) ) ;
#40778 = CARTESIAN_POINT ( 'NONE',  ( 5.901764892641288895, 1.526405342808391463, -48.94549574954905324 ) ) ;
#40779 = EDGE_CURVE ( 'NONE', #57626, #15681, #11726, .T. ) ;
#40780 = VECTOR ( 'NONE', #599, 1000.000000000000227 ) ;
#40781 = CARTESIAN_POINT ( 'NONE',  ( 0.1073791018717483448, -41.77800844988507123, -10.69234304550039383 ) ) ;
#40782 = CARTESIAN_POINT ( 'NONE',  ( 0.8753041380234465318, 3.828530797420660381, 48.95386276695825956 ) ) ;
#40783 = CARTESIAN_POINT ( 'NONE',  ( 0.9762797500689124330, 29.49606728235512776, 29.77090526101756751 ) ) ;
#40784 = EDGE_CURVE ( 'NONE', #48962, #44981, #33796, .T. ) ;
#40785 = CARTESIAN_POINT ( 'NONE',  ( 0.5998501479064699549, -44.24259072156099393, 18.89267974119588445 ) ) ;
#40786 = CARTESIAN_POINT ( 'NONE',  ( 0.5827357941260201679, 5.891356987508307164, -47.53228940613938391 ) ) ;
#40787 = CARTESIAN_POINT ( 'NONE',  ( 5.860006189529246790, 43.25137511473251095, 21.34829429597482076 ) ) ;
#40788 = FACE_OUTER_BOUND ( 'NONE', #42482, .T. ) ;
#40789 = EDGE_CURVE ( 'NONE', #37980, #44953, #40457, .T. ) ;
#40790 = CIRCLE ( 'NONE', #9868, 2.649999999999999467 ) ;
#40791 = DIRECTION ( 'NONE',  ( 0.000000000000000000, 0.000000000000000000, -1.000000000000000000 ) ) ;
#40792 = CARTESIAN_POINT ( 'NONE',  ( 0.8751705887134423323, 33.37254303619506857, 34.63284514348596588 ) ) ;
#40793 = VERTEX_POINT ( 'NONE', #24782 ) ;
#40794 = CARTESIAN_POINT ( 'NONE',  ( 0.7948884756798498818, -19.07805331891001188, -45.24076177697474321 ) ) ;
#40795 = CARTESIAN_POINT ( 'NONE',  ( 0.5786265663353153954, 43.97352617418643206, -18.99608782657985628 ) ) ;
#40796 = CARTESIAN_POINT ( 'NONE',  ( 2.359973842542475886, -42.17663974021382955, 12.62010122212638485 ) ) ;
#40797 = VERTEX_POINT ( 'NONE', #43925 ) ;
#40798 = EDGE_CURVE ( 'NONE', #23520, #41282, #42013, .T. ) ;
#40799 = CARTESIAN_POINT ( 'NONE',  ( 2.526464513654343769, -42.75268905308553258, -4.405490210168832910 ) ) ;
#40800 = CARTESIAN_POINT ( 'NONE',  ( 0.5997462898726536595, 44.46857747280041195, -20.83500054451300088 ) ) ;
#40801 =( LENGTH_UNIT ( ) NAMED_UNIT ( * ) SI_UNIT ( .MILLI., .METRE. ) );
#40802 = ORIENTED_EDGE ( 'NONE', *, *, #60921, .T. ) ;
#40803 = CARTESIAN_POINT ( 'NONE',  ( 0.5809828226811617480, -33.48000389720591841, -34.25055090842189287 ) ) ;
#40804 = DIRECTION ( 'NONE',  ( 0.000000000000000000, 0.000000000000000000, -1.000000000000000000 ) ) ;
#40805 = VECTOR ( 'NONE', #15219, 1000.000000000000000 ) ;
#40806 = ORIENTED_EDGE ( 'NONE', *, *, #12526, .T. ) ;
#40807 = CARTESIAN_POINT ( 'NONE',  ( 5.958863334805807099, 20.35021240744034898, -2.677925489610427867 ) ) ;
#40808 = CIRCLE ( 'NONE', #59776, 43.92652462719577500 ) ;
#40809 = CIRCLE ( 'NONE', #13791, 15.43999999999999240 ) ;
#40810 = VERTEX_POINT ( 'NONE', #20098 ) ;
#40811 = VERTEX_POINT ( 'NONE', #37988 ) ;
#40812 = CARTESIAN_POINT ( 'NONE',  ( 0.9749527285493301276, -5.883724875809405397, 42.50314808877159578 ) ) ;
#40813 = ORIENTED_EDGE ( 'NONE', *, *, #22758, .F. ) ;
#40814 = FACE_OUTER_BOUND ( 'NONE', #9336, .T. ) ;
#40815 = PRODUCT_DEFINITION_SHAPE ( 'NONE', 'NONE',  #61979 ) ;
#40816 = ORIENTED_EDGE ( 'NONE', *, *, #55075, .F. ) ;
#40817 = FACE_OUTER_BOUND ( 'NONE', #30673, .T. ) ;
#40818 = B_SPLINE_CURVE_WITH_KNOTS ( 'NONE', 3,
 ( #18632, #9519, #14250, #13947, #56818, #37760 ),
 .UNSPECIFIED., .F., .F.,
 ( 4, 2, 4 ),
 ( 1.870559545977334001E-17, 0.0002293319059085113364, 0.0004586638118170039704 ),
 .UNSPECIFIED. ) ;
#40819 = CARTESIAN_POINT ( 'NONE',  ( 0.6252788684277233999, 40.77687624000223821, -27.36221290906875225 ) ) ;
#40820 = VERTEX_POINT ( 'NONE', #14167 ) ;
#40821 = CARTESIAN_POINT ( 'NONE',  ( 0.1154773475650540532, 15.40762055515278384, 41.34669102690751430 ) ) ;
#40822 = DIRECTION ( 'NONE',  ( 0.07439287786467665975, 0.7830499462674470612, 0.6174937095821784183 ) ) ;
#40823 = CARTESIAN_POINT ( 'NONE',  ( 0.5806925824938502512, -44.47729014209954101, -14.86583411581937320 ) ) ;
#40824 = CARTESIAN_POINT ( 'NONE',  ( 0.5835871038041838821, -30.38152644921350998, 35.72390381127519277 ) ) ;
#40825 = ORIENTED_EDGE ( 'NONE', *, *, #25592, .F. ) ;
#40826 = ADVANCED_FACE ( 'NONE', ( #52036 ), #9132, .F. ) ;
#40827 = CARTESIAN_POINT ( 'NONE',  ( 0.6543461111163461075, 4.241015250120812929, -0.1391502195351438376 ) ) ;
#40828 = ORIENTED_EDGE ( 'NONE', *, *, #57434, .F. ) ;
#40829 = CARTESIAN_POINT ( 'NONE',  ( -6.078075953587585900, 17.84675544569240557, -7.231078364171170669 ) ) ;
#40830 = EDGE_CURVE ( 'NONE', #49095, #44905, #16678, .T. ) ;
#40831 = CARTESIAN_POINT ( 'NONE',  ( 0.1145239942831223490, -12.86729789440911986, 42.20637541416234484 ) ) ;
#40832 = CARTESIAN_POINT ( 'NONE',  ( 0.3676999524040366896, 14.45783756353458216, -41.67639039443420756 ) ) ;
#40833 = ORIENTED_EDGE ( 'NONE', *, *, #18596, .F. ) ;
#40834 = CARTESIAN_POINT ( 'NONE',  ( 0.5832367798473389042, -46.19266341874887871, -12.65931911325652415 ) ) ;
#40835 = FACE_BOUND ( 'NONE', #40124, .T. ) ;
#40836 = ADVANCED_FACE ( 'NONE', ( #33577 ), #7567, .F. ) ;
#40837 = CARTESIAN_POINT ( 'NONE',  ( 4.967162193818130511, 40.93989340068628024, -13.42934394584121094 ) ) ;
#40838 = CARTESIAN_POINT ( 'NONE',  ( 4.956653778116982600, -45.35992544608539845, 15.97476558431867844 ) ) ;
#40839 = AXIS2_PLACEMENT_3D ( 'NONE', #32139, #17115, #51217 ) ;
#40840 =( BOUNDED_SURFACE ( )  B_SPLINE_SURFACE ( 3, 1, ( 
 ( #24430, #57924 ),
 ( #6217, #19747 ),
 ( #25359, #19141 ),
 ( #38252, #57298 ) ),
 .UNSPECIFIED., .F., .F., .F. ) 
 B_SPLINE_SURFACE_WITH_KNOTS ( ( 4, 4 ),
 ( 2, 2 ),
 ( 0.000000000000000000, 1.000000000000000000 ),
 ( 0.000000000000000000, 1.000000000000000000 ),
 .UNSPECIFIED. ) 
 GEOMETRIC_REPRESENTATION_ITEM ( )  RATIONAL_B_SPLINE_SURFACE ( (
 ( 1.000000000000000000, 1.000000000000000000),
 ( 0.9952954269826590483, 0.8620686068821339365),
 ( 0.9952954269826590483, 0.8620686068821339365),
 ( 1.000000000000000000, 1.000000000000000000) ) ) 
 REPRESENTATION_ITEM ( '' )  SURFACE ( )  );
#40841 = ORIENTED_EDGE ( 'NONE', *, *, #38292, .F. ) ;
#40842 = ORIENTED_EDGE ( 'NONE', *, *, #39998, .T. ) ;
#40843 = CARTESIAN_POINT ( 'NONE',  ( 0.1092565886968785011, 34.40108480122215440, 26.00565248013064945 ) ) ;
#40844 = CARTESIAN_POINT ( 'NONE',  ( 0.9762797500689124330, -31.41867615533366376, -27.73430319715951242 ) ) ;
#40845 = CARTESIAN_POINT ( 'NONE',  ( 0.6031356755773454870, 6.279255973231343546, -47.69588082432150600 ) ) ;
#40846 = CARTESIAN_POINT ( 'NONE',  ( 1.227938101723748288, -11.92353943227977986, 41.23019537246705823 ) ) ;
#40847 = EDGE_CURVE ( 'NONE', #54373, #14724, #16581, .T. ) ;
#40848 = CARTESIAN_POINT ( 'NONE',  ( 0.5998501479064699549, 11.94461217097469685, -46.60114184914306179 ) ) ;
#40849 = CARTESIAN_POINT ( 'NONE',  ( 0.6254311100348644015, 38.58047947916330145, -28.73641524052532503 ) ) ;
#40850 = VECTOR ( 'NONE', #52267, 1000.000000000000114 ) ;
#40851 = CARTESIAN_POINT ( 'NONE',  ( 0.7056555295713289322, 0.8411712675128016903, 47.89404551051138981 ) ) ;
#40852 = CARTESIAN_POINT ( 'NONE',  ( 0.9785694773339252972, 32.75148539916909129, 26.14719124232438574 ) ) ;
#40853 = FACE_OUTER_BOUND ( 'NONE', #36539, .T. ) ;
#40854 = CARTESIAN_POINT ( 'NONE',  ( 4.390527457369401532, 40.84234994305386834, -16.18912560201280826 ) ) ;
#40855 = DIRECTION ( 'NONE',  ( 0.000000000000000000, 0.000000000000000000, 1.000000000000000000 ) ) ;
#40856 = CARTESIAN_POINT ( 'NONE',  ( 4.553261556744875094, 6.787618719203488915, 43.39893775135925580 ) ) ;
#40857 = CARTESIAN_POINT ( 'NONE',  ( 0.6027935024548038978, -6.106197519201156609, -47.71838037711331992 ) ) ;
#40858 = EDGE_CURVE ( 'NONE', #11409, #26359, #38748, .T. ) ;
#40859 = DIRECTION ( 'NONE',  ( 0.07500201931887537365, 0.9798016564750019475, -0.1853737065145253660 ) ) ;
#40860 = DIRECTION ( 'NONE',  ( 0.07906939808003032866, -0.9890184005629941710, 0.1248624588700636417 ) ) ;
#40861 = CARTESIAN_POINT ( 'NONE',  ( 4.549368137175248350, -23.67244292351665536, 35.80950303116058819 ) ) ;
#40863 = ORIENTED_EDGE ( 'NONE', *, *, #49575, .F. ) ;
#40862 = CARTESIAN_POINT ( 'NONE',  ( 5.965394784446460541, -16.27505370423073217, -12.50653125159001533 ) ) ;
#40864 = ORIENTED_EDGE ( 'NONE', *, *, #10963, .F. ) ;
#40865 = VECTOR ( 'NONE', #11453, 1000.000000000000000 ) ;
#40866 = CARTESIAN_POINT ( 'NONE',  ( 0.6026112563231247332, 17.12333019133003376, -46.02534690866429656 ) ) ;
#40867 = FACE_OUTER_BOUND ( 'NONE', #56491, .T. ) ;
#40868 = CARTESIAN_POINT ( 'NONE',  ( 1.088313998177379505, 6.373602917100794407, -42.43756598879020459 ) ) ;
#40869 = ORIENTED_EDGE ( 'NONE', *, *, #46693, .F. ) ;
#40870 = EDGE_CURVE ( 'NONE', #23080, #58704, #6880, .T. ) ;
#40871 = ORIENTED_EDGE ( 'NONE', *, *, #18296, .T. ) ;
#40872 = CARTESIAN_POINT ( 'NONE',  ( -2.601141883200662974, 14.55883463511898057, -3.291771792917696171 ) ) ;
#40873 = CARTESIAN_POINT ( 'NONE',  ( 0.1103310638050662013, -37.38800124003726211, 21.49083802119835696 ) ) ;
#40874 = MECHANICAL_DESIGN_GEOMETRIC_PRESENTATION_REPRESENTATION (  '', ( #46860 ), #29830 ) ;
#40875 = VERTEX_POINT ( 'NONE', #1258 ) ;
#40876 = ORIENTED_EDGE ( 'NONE', *, *, #21547, .F. ) ;
#40877 = CARTESIAN_POINT ( 'NONE',  ( 0.5839879882012670720, 47.89596766821092189, -3.018602154015963534E-05 ) ) ;
#40878 = AXIS2_PLACEMENT_3D ( 'NONE', #54338, #22950, #27637 ) ;
#40879 = CARTESIAN_POINT ( 'NONE',  ( -6.015611763856276717, 13.32857883366851937, -13.31979030221785365 ) ) ;
#40880 = CARTESIAN_POINT ( 'NONE',  ( 0.7056313189692662302, 17.64074258352390601, 43.45748318827730117 ) ) ;
#40881 = EDGE_LOOP ( 'NONE', ( #53870, #54080, #21827, #57564 ) ) ;
#40882 = CARTESIAN_POINT ( 'NONE',  ( 1.827119703190778432, 40.22835835992442810, 15.32887915442610272 ) ) ;
#40883 =( REPRESENTATION_RELATIONSHIP ('NONE','NONE', #44881, #8803 ) REPRESENTATION_RELATIONSHIP_WITH_TRANSFORMATION ( #27110 )SHAPE_REPRESENTATION_RELATIONSHIP( ) );
#40884 = FACE_OUTER_BOUND ( 'NONE', #44571, .T. ) ;
#40885 = B_SPLINE_CURVE_WITH_KNOTS ( 'NONE', 3,
 ( #49934, #60236, #6991, #41484 ),
 .UNSPECIFIED., .F., .F.,
 ( 4, 4 ),
 ( 4.046035655711835948E-17, 0.005004948556313840863 ),
 .UNSPECIFIED. ) ;
#40886 = CARTESIAN_POINT ( 'NONE',  ( 0.1102144999581333162, 0.1260305566212060746, -43.12427761225339395 ) ) ;
#40887 = ORIENTED_EDGE ( 'NONE', *, *, #61924, .T. ) ;
#40888 = ORIENTED_EDGE ( 'NONE', *, *, #59619, .T. ) ;
#40889 = CARTESIAN_POINT ( 'NONE',  ( 5.895596859100789899, 8.462961974658517406, 18.24572437114984780 ) ) ;
#40890 = CARTESIAN_POINT ( 'NONE',  ( 5.965394784446458765, 7.841344330024942799, -18.96850062921626900 ) ) ;
#40891 = AXIS2_PLACEMENT_3D ( 'NONE', #27561, #13171, #7506 ) ;
#40892 = ORIENTED_EDGE ( 'NONE', *, *, #3737, .T. ) ;
#40893 = CARTESIAN_POINT ( 'NONE',  ( 0.6026112563231248442, -48.72623651472557782, 6.106952596445339942 ) ) ;
#40894 = CARTESIAN_POINT ( 'NONE',  ( 4.000000000000003553, 2.309401076758524685, -5.242734410091827613 ) ) ;
#40895 = CARTESIAN_POINT ( 'NONE',  ( 0.5804410086790514622, 28.25755288515069807, 37.43034272883843983 ) ) ;
#40896 = CARTESIAN_POINT ( 'NONE',  ( 0.7948884756798504370, -8.691324955621483994, 48.32348823414908168 ) ) ;
#40897 = EDGE_CURVE ( 'NONE', #29351, #18593, #19589, .T. ) ;
#40898 = ORIENTED_EDGE ( 'NONE', *, *, #44863, .F. ) ;
#40899 = CARTESIAN_POINT ( 'NONE',  ( 0.5830081025819946472, -13.63296368238104250, 44.87064001791286216 ) ) ;
#40900 = CARTESIAN_POINT ( 'NONE',  ( 0.5998501479064699549, 18.89267974119604077, 44.24259072156093708 ) ) ;
#40901 = ADVANCED_FACE ( 'NONE', ( #6248 ), #25703, .T. ) ;
#40902 = CARTESIAN_POINT ( 'NONE',  ( 0.8751705887134423323, 29.98056538504960855, -37.60752970653798855 ) ) ;
#40903 = DIRECTION ( 'NONE',  ( 0.09722883295013592941, 0.2288279796715218528, 0.9685991481322931973 ) ) ;
#40904 = ORIENTED_EDGE ( 'NONE', *, *, #54630, .T. ) ;
#40905 = CARTESIAN_POINT ( 'NONE',  ( 0.5998501479064708430, -44.64337787626261189, 17.92509395669028649 ) ) ;
#40906 = CARTESIAN_POINT ( 'NONE',  ( 5.901463166500146684, 10.81005692193087420, -16.96055835417133295 ) ) ;
#40907 = EDGE_CURVE ( 'NONE', #45266, #61276, #21011, .T. ) ;
#40908 = CARTESIAN_POINT ( 'NONE',  ( 4.833616638992205949, -46.11947910922906146, -3.476827473557714931 ) ) ;
#40909 = ADVANCED_FACE ( 'NONE', ( #4599 ), #61675, .F. ) ;
#40910 = AXIS2_PLACEMENT_3D ( 'NONE', #21954, #36074, #41695 ) ;
#40911 = ORIENTED_EDGE ( 'NONE', *, *, #3103, .F. ) ;
#40912 = CARTESIAN_POINT ( 'NONE',  ( 5.981074661064941900, 10.25489689131105919, 17.77917279944636064 ) ) ;
#40913 = EDGE_CURVE ( 'NONE', #29096, #61317, #42875, .T. ) ;
#40914 = CARTESIAN_POINT ( 'NONE',  ( 4.549368137175248350, -19.17571786012351254, 38.40568845698243194 ) ) ;
#40915 = CARTESIAN_POINT ( 'NONE',  ( 4.962356264823608143, -14.71877352713578269, -39.42833123173278409 ) ) ;
#40916 = CARTESIAN_POINT ( 'NONE',  ( 5.960721111146673579, -19.82781442290501417, 5.306302591836237426 ) ) ;
#40917 = CARTESIAN_POINT ( 'NONE',  ( 0.5835226383429271690, -46.77883816727116795, 3.314026895820559204 ) ) ;
#40918 = EDGE_CURVE ( 'NONE', #12140, #54683, #11365, .T. ) ;
#40919 = DIRECTION ( 'NONE',  ( 0.000000000000000000, 0.000000000000000000, 1.000000000000000000 ) ) ;
#40920 = FACE_OUTER_BOUND ( 'NONE', #15135, .T. ) ;
#40921 = CARTESIAN_POINT ( 'NONE',  ( 0.1100053167205931048, -41.70112744323661502, -10.98799238780936527 ) ) ;
#40922 = EDGE_CURVE ( 'NONE', #31508, #39205, #35753, .T. ) ;
#40923 = CARTESIAN_POINT ( 'NONE',  ( 0.6026112563231247332, 41.25111472265821533, -26.64369585928908535 ) ) ;
#40924 = CARTESIAN_POINT ( 'NONE',  ( 0.8744876279028306332, -13.11369837310865805, 47.31153099782990523 ) ) ;
#40925 = ORIENTED_EDGE ( 'NONE', *, *, #2597, .T. ) ;
#40926 = CARTESIAN_POINT ( 'NONE',  ( 0.8760168074887090262, 47.80016357497242296, 5.394043284319671727 ) ) ;
#40927 = CARTESIAN_POINT ( 'NONE',  ( 0.9762797500689124330, -34.83496347773955648, 23.29914386174426255 ) ) ;
#40928 = CARTESIAN_POINT ( 'NONE',  ( 0.1140933569871965536, 44.05627166033247732, -2.448443888450706485 ) ) ;
#40929 = CARTESIAN_POINT ( 'NONE',  ( 5.959547316686252039, -17.77392908783941294, 10.26589671991332331 ) ) ;
#40930 = CARTESIAN_POINT ( 'NONE',  ( 0.9788927965476029724, -30.98642140960746616, 28.21663163557970222 ) ) ;
#40931 = APPLICATION_PROTOCOL_DEFINITION ( 'draft international standard', 'automotive_design', 1998, #48782 ) ;
#40932 = CARTESIAN_POINT ( 'NONE',  ( 0.1073791018717483448, -42.81622261970991161, -5.147744207006710759 ) ) ;
#40933 =( BOUNDED_SURFACE ( )  B_SPLINE_SURFACE ( 3, 1, ( 
 ( #19280, #3911 ),
 ( #38099, #51839 ),
 ( #38396, #52455 ),
 ( #57443, #14583 ) ),
 .UNSPECIFIED., .F., .F., .F. ) 
 B_SPLINE_SURFACE_WITH_KNOTS ( ( 4, 4 ),
 ( 2, 2 ),
 ( 0.000000000000000000, 1.000000000000000000 ),
 ( 0.000000000000000000, 1.000000000000000000 ),
 .UNSPECIFIED. ) 
 GEOMETRIC_REPRESENTATION_ITEM ( )  RATIONAL_B_SPLINE_SURFACE ( (
 ( 1.000000000000000000, 1.000000000000000000),
 ( 0.7211978278499970862, 0.9934217856018976445),
 ( 0.7211978278499970862, 0.9934217856018976445),
 ( 1.000000000000000000, 1.000000000000000000) ) ) 
 REPRESENTATION_ITEM ( '' )  SURFACE ( )  );
#40934 = CARTESIAN_POINT ( 'NONE',  ( 0.9789233960466705575, -7.100278355974616318, 41.30281799223896400 ) ) ;
#40935 = B_SPLINE_CURVE_WITH_KNOTS ( 'NONE', 3,
 ( #5289, #25041, #24417, #54134 ),
 .UNSPECIFIED., .F., .F.,
 ( 4, 4 ),
 ( 2.183987964099527011E-17, 0.004559932413162189405 ),
 .UNSPECIFIED. ) ;
#40936 = CIRCLE ( 'NONE', #21906, 2.649999999999997691 ) ;
#40937 = CARTESIAN_POINT ( 'NONE',  ( 0.6031356755852234075, 0.04363310494615044166, -48.10744332413860747 ) ) ;
#40939 = ORIENTED_EDGE ( 'NONE', *, *, #19968, .T. ) ;
#40938 = CARTESIAN_POINT ( 'NONE',  ( 4.975610109902397937, 24.86209007719020647, -42.12274782266053563 ) ) ;
#40940 = EDGE_LOOP ( 'NONE', ( #50226, #40158, #61424, #43448 ) ) ;
#40941 = CARTESIAN_POINT ( 'NONE',  ( 5.981074661064941900, 17.77917279944632512, -10.25489689131111959 ) ) ;
#40942 = AXIS2_PLACEMENT_3D ( 'NONE', #43367, #15460, #39910 ) ;
#40943 = CARTESIAN_POINT ( 'NONE',  ( 0.7413678028165012757, -18.69877339599409893, -39.93547251824506361 ) ) ;
#40944 = CARTESIAN_POINT ( 'NONE',  ( 0.5832655196449125778, -8.024559735822561990, 46.20434637585024262 ) ) ;
#40945 = CARTESIAN_POINT ( 'NONE',  ( 0.9762797500689124330, -1.905951756780080775, -41.86516610604251554 ) ) ;
#40946 = EDGE_CURVE ( 'NONE', #46145, #4231, #27006, .T. ) ;
#40947 = ORIENTED_EDGE ( 'NONE', *, *, #32084, .T. ) ;
#40948 = CARTESIAN_POINT ( 'NONE',  ( 40.00000000000000000, 0.000000000000000000, 0.000000000000000000 ) ) ;
#40949 = CARTESIAN_POINT ( 'NONE',  ( 2.618530812446111078, -35.79257080906894828, 30.47324505325918409 ) ) ;
#40950 = DIRECTION ( 'NONE',  ( 1.000000000000000000, 0.000000000000000000, 0.000000000000000000 ) ) ;
#40952 = EDGE_CURVE ( 'NONE', #23031, #21932, #18030, .T. ) ;
#40951 = VERTEX_POINT ( 'NONE', #10575 ) ;
#40953 = ORIENTED_EDGE ( 'NONE', *, *, #19477, .T. ) ;
#40954 = CARTESIAN_POINT ( 'NONE',  ( -4.908599999999999852, 0.000000000000000000, 0.000000000000000000 ) ) ;
#40955 = CONICAL_SURFACE ( 'NONE', #36929, 43.92652462719577500, 1.486293639869522343 ) ;
#40956 = DIRECTION ( 'NONE',  ( -0.1024043820194934507, -0.8679729669084614851, 0.4859385467930367741 ) ) ;
#40957 = ORIENTED_EDGE ( 'NONE', *, *, #4761, .T. ) ;
#40958 = B_SPLINE_CURVE_WITH_KNOTS ( 'NONE', 3,
 ( #44000, #58037, #38978, #24233, #11076, #34267 ),
 .UNSPECIFIED., .F., .F.,
 ( 4, 2, 4 ),
 ( 1.515731698875470022E-16, 0.0002445252820015211956, 0.0004890505640028908196 ),
 .UNSPECIFIED. ) ;
#40959 = CARTESIAN_POINT ( 'NONE',  ( 0.1154773475650540532, -42.72636521210627336, -11.01822788872314440 ) ) ;
#40960 = CARTESIAN_POINT ( 'NONE',  ( 5.895596859100789899, 10.81936814621394127, -16.95492424427719413 ) ) ;
#40961 = ORIENTED_EDGE ( 'NONE', *, *, #7778, .F. ) ;
#40962 = FACE_OUTER_BOUND ( 'NONE', #22067, .T. ) ;
#40963 = CARTESIAN_POINT ( 'NONE',  ( -6.079354080745853928, 5.479977851902066099, 18.45976159084468549 ) ) ;
#40964 = LINE ( 'NONE', #55008, #2974 ) ;
#40965 = ORIENTED_EDGE ( 'NONE', *, *, #12064, .T. ) ;
#40966 = CARTESIAN_POINT ( 'NONE',  ( 0.6000166863083090663, 10.41802958826996317, -47.99258423138293495 ) ) ;
#40967 = CARTESIAN_POINT ( 'NONE',  ( 0.6001305935487315502, 48.10757715638249010, -0.5236757026884391042 ) ) ;
#40968 = VERTEX_POINT ( 'NONE', #5532 ) ;
#40969 = CARTESIAN_POINT ( 'NONE',  ( 7.000000000000016875, -58.44237546506844438, 54.69470952477916370 ) ) ;
#40970 = CARTESIAN_POINT ( 'NONE',  ( 0.8744876279028263033, 11.79038800009220722, -47.65854384249244191 ) ) ;
#40971 = CARTESIAN_POINT ( 'NONE',  ( 0.6064515330803574855, 45.03781699277671180, -13.07399619711731731 ) ) ;
#40972 = CARTESIAN_POINT ( 'NONE',  ( 4.322998006666179727, -40.45864630878536161, 25.80712523194204877 ) ) ;
#40973 = VERTEX_POINT ( 'NONE', #43182 ) ;
#40974 = CARTESIAN_POINT ( 'NONE',  ( 0.8554163680231720024, 36.24698750680840931, -29.78861141095861598 ) ) ;
#40975 = CARTESIAN_POINT ( 'NONE',  ( 0.1154773475650540809, 39.67614629000453164, -19.30665806451962041 ) ) ;
#40976 = EDGE_CURVE ( 'NONE', #4099, #56285, #47988, .T. ) ;
#40977 = ORIENTED_EDGE ( 'NONE', *, *, #4413, .F. ) ;
#40978 = DIRECTION ( 'NONE',  ( -1.000000000000000000, -0.000000000000000000, -0.000000000000000000 ) ) ;
#40979 = AXIS2_PLACEMENT_3D ( 'NONE', #52000, #18503, #13821 ) ;
#40980 = EDGE_LOOP ( 'NONE', ( #50915, #24158, #29445, #37256 ) ) ;
#40981 = DIRECTION ( 'NONE',  ( 0.000000000000000000, 0.000000000000000000, -1.000000000000000000 ) ) ;
#40983 = ORIENTED_EDGE ( 'NONE', *, *, #58570, .T. ) ;
#40982 = ADVANCED_FACE ( 'NONE', ( #43812 ), #21680, .T. ) ;
#40984 = CARTESIAN_POINT ( 'NONE',  ( 5.959828726073459926, -0.004526594003520726349, 20.52560994243598813 ) ) ;
#40985 = CARTESIAN_POINT ( 'NONE',  ( 0.9790850452238870627, 24.90012728558320276, 33.70936059056818124 ) ) ;
#40986 = EDGE_CURVE ( 'NONE', #28137, #36643, #20707, .T. ) ;
#40987 = VECTOR ( 'NONE', #52970, 1000.000000000000227 ) ;
#40988 = CARTESIAN_POINT ( 'NONE',  ( 0.1152809850208376119, -43.78968008214310004, 5.423025059255664360 ) ) ;
#40989 = ORIENTED_EDGE ( 'NONE', *, *, #37744, .T. ) ;
#40990 = CARTESIAN_POINT ( 'NONE',  ( -6.016761891674565099, 17.41015286184812894, -7.207804629151121745 ) ) ;
#40991 = ADVANCED_FACE ( 'NONE', ( #24054 ), #34704, .F. ) ;
#40992 = DIRECTION ( 'NONE',  ( -0.07836865515943411409, 0.9649662368512218480, 0.2503967164834498549 ) ) ;
#40993 = CARTESIAN_POINT ( 'NONE',  ( -6.057079549204054558, 0.6257114429647351317, -19.24681054850079320 ) ) ;
#40995 = ORIENTED_EDGE ( 'NONE', *, *, #28272, .T. ) ;
#40994 = B_SPLINE_CURVE_WITH_KNOTS ( 'NONE', 3,
 ( #23260, #45, #42387, #61440 ),
 .UNSPECIFIED., .F., .F.,
 ( 4, 4 ),
 ( 0.000000000000000000, 0.004041751736740989073 ),
 .UNSPECIFIED. ) ;
#40996 = ORIENTED_EDGE ( 'NONE', *, *, #12365, .T. ) ;
#40997 = CARTESIAN_POINT ( 'NONE',  ( 0.1129192098497455998, 29.30421273086464140, 32.98810246148426728 ) ) ;
#40998 = DIRECTION ( 'NONE',  ( -0.07500201931887529039, -0.9939633762263326844, 0.08007186658771524301 ) ) ;
#40999 = CARTESIAN_POINT ( 'NONE',  ( 0.1073791018717578927, -16.05399293000789385, -40.02496097243051310 ) ) ;
#41000 = ADVANCED_FACE ( 'NONE', ( #25587 ), #5548, .F. ) ;
#41001 = CARTESIAN_POINT ( 'NONE',  ( 0.1087620492084206969, 30.23658359364778647, 30.74858804150697011 ) ) ;
#41002 = CARTESIAN_POINT ( 'NONE',  ( 0.7954196712028466232, -11.60747899261487071, -46.67728755034880805 ) ) ;
#41003 = ORIENTED_EDGE ( 'NONE', *, *, #34905, .F. ) ;
#41004 = CARTESIAN_POINT ( 'NONE',  ( 0.3622758884714730732, 11.95365414648439462, 41.42293301073630118 ) ) ;
#41005 = CARTESIAN_POINT ( 'NONE',  ( 5.910764540655177868, 5.943959005784828165, 19.21381247453801322 ) ) ;
#41006 = AXIS2_PLACEMENT_3D ( 'NONE', #51771, #18586, #18283 ) ;
#41007 = ORIENTED_EDGE ( 'NONE', *, *, #59781, .F. ) ;
#41008 = CARTESIAN_POINT ( 'NONE',  ( 0.9756008150404608115, -30.24019526051566586, 30.44122083654206179 ) ) ;
#41009 = CARTESIAN_POINT ( 'NONE',  ( 1.500000000000001332, 0.000000000000000000, 0.000000000000000000 ) ) ;
#41010 = CARTESIAN_POINT ( 'NONE',  ( 0.6029443199889047422, 44.24425750603113983, 21.30688432395522369 ) ) ;
#41011 = CARTESIAN_POINT ( 'NONE',  ( 0.1152809850208375841, -42.73668636166265600, 10.97820209846000772 ) ) ;
#41012 = CARTESIAN_POINT ( 'NONE',  ( 0.5807400328401574052, -6.791881299635267766, -47.41494605191449807 ) ) ;
#41013 = CARTESIAN_POINT ( 'NONE',  ( 4.335381028904216727, -23.55321997556169222, 42.95349434501397923 ) ) ;
#41014 = CARTESIAN_POINT ( 'NONE',  ( 4.956445790444035104, 38.51510088324747016, -27.09474218539284252 ) ) ;
#41015 = SURFACE_STYLE_USAGE ( .BOTH. , #21876 ) ;
#41016 = CARTESIAN_POINT ( 'NONE',  ( 7.000000000000005329, 2.650000000000838796, -79.99999999999998579 ) ) ;
#41017 = CARTESIAN_POINT ( 'NONE',  ( -6.057079549204054558, 3.065021114850542627, 19.01149327815305412 ) ) ;
#41018 = DIRECTION ( 'NONE',  ( -1.000000000000000000, -0.000000000000000000, -0.000000000000000000 ) ) ;
#41019 =( BOUNDED_SURFACE ( )  B_SPLINE_SURFACE ( 3, 1, ( 
 ( #47246, #20511 ),
 ( #778, #4295 ),
 ( #1371, #5757 ),
 ( #39636, #34933 ) ),
 .UNSPECIFIED., .F., .F., .F. ) 
 B_SPLINE_SURFACE_WITH_KNOTS ( ( 4, 4 ),
 ( 2, 2 ),
 ( 0.000000000000000000, 1.000000000000000000 ),
 ( 0.000000000000000000, 1.000000000000000000 ),
 .UNSPECIFIED. ) 
 GEOMETRIC_REPRESENTATION_ITEM ( )  RATIONAL_B_SPLINE_SURFACE ( (
 ( 1.000000000000000000, 1.000000000000000000),
 ( 0.9754377213608244057, 0.9999580625633939235),
 ( 0.9754377213608244057, 0.9999580625633939235),
 ( 1.000000000000000000, 1.000000000000000000) ) ) 
 REPRESENTATION_ITEM ( '' )  SURFACE ( )  );
#41020 = CARTESIAN_POINT ( 'NONE',  ( 0.7948884756798505480, 3.850400318513474751, 48.94765634825986211 ) ) ;
#41021 = CARTESIAN_POINT ( 'NONE',  ( 5.880360259849739535, 45.41096578730646627, -15.46489389606708542 ) ) ;
#41022 = CARTESIAN_POINT ( 'NONE',  ( -2.739355103387247858, -14.92576340101414800, -0.2629711922692861692 ) ) ;
#41023 = CARTESIAN_POINT ( 'NONE',  ( 0.2230388203127610658, 0.7599700551094308310, 43.11276071378622277 ) ) ;
#41024 = CARTESIAN_POINT ( 'NONE',  ( 0.5804410086790514622, -38.35366574782020876, 26.99103880105171882 ) ) ;
#41025 = CARTESIAN_POINT ( 'NONE',  ( 0.6067375320500707492, 37.56348932307263055, 29.71715680108748714 ) ) ;
#41026 = CARTESIAN_POINT ( 'NONE',  ( 0.5998501479064699549, 11.94461217097469685, -46.60114184914306179 ) ) ;
#41027 = EDGE_CURVE ( 'NONE', #41282, #12597, #8705, .T. ) ;
#41028 = EDGE_LOOP ( 'NONE', ( #45866, #12445, #20154, #27389 ) ) ;
#41029 = CARTESIAN_POINT ( 'NONE',  ( -5.995132425357893702, -11.46484027925377980, 14.95525565067270968 ) ) ;
#41030 = B_SPLINE_CURVE_WITH_KNOTS ( 'NONE', 3,
 ( #55820, #26705, #46763, #45844 ),
 .UNSPECIFIED., .F., .F.,
 ( 4, 4 ),
 ( 6.254634441385501517E-18, 0.004566006591234646368 ),
 .UNSPECIFIED. ) ;
#41031 = CARTESIAN_POINT ( 'NONE',  ( 0.1149546198390367091, -38.31111110369499784, -21.89075903260455647 ) ) ;
#41032 = FACE_OUTER_BOUND ( 'NONE', #25881, .T. ) ;
#41033 = ORIENTED_EDGE ( 'NONE', *, *, #21003, .T. ) ;
#41034 = CARTESIAN_POINT ( 'NONE',  ( 1.231276596079887264, -34.07446381689716475, 24.41736444846234733 ) ) ;
#41035 = LINE ( 'NONE', #60095, #13961 ) ;
#41036 = CARTESIAN_POINT ( 'NONE',  ( 4.956445790444027111, 14.46717203539434671, -44.81337951368921324 ) ) ;
#41037 = ORIENTED_EDGE ( 'NONE', *, *, #5580, .F. ) ;
#41038 = CARTESIAN_POINT ( 'NONE',  ( 3.376099380956838925, -10.78512648832971799, -7.961747940169664695 ) ) ;
#41039 = VERTEX_POINT ( 'NONE', #54690 ) ;
#41040 = LINE ( 'NONE', #56320, #9827 ) ;
#41041 = VECTOR ( 'NONE', #57428, 1000.000000000000114 ) ;
#41042 = CARTESIAN_POINT ( 'NONE',  ( 5.895596859100789899, 20.06821053248683029, 1.339816866691926567 ) ) ;
#41043 = ORIENTED_EDGE ( 'NONE', *, *, #36554, .T. ) ;
#41044 = CARTESIAN_POINT ( 'NONE',  ( 0.8551540677456715978, 28.44084013485173656, -38.56334384152401640 ) ) ;
#41045 = ORIENTED_EDGE ( 'NONE', *, *, #40276, .T. ) ;
#41046 = FACE_OUTER_BOUND ( 'NONE', #41961, .T. ) ;
#41047 = CARTESIAN_POINT ( 'NONE',  ( 0.1149546198390368618, 20.16591343492030930, 39.24643296350026134 ) ) ;
#41048 = EDGE_CURVE ( 'NONE', #600, #32441, #26685, .T. ) ;
#41049 = ORIENTED_EDGE ( 'NONE', *, *, #32042, .T. ) ;
#41050 = CARTESIAN_POINT ( 'NONE',  ( 0.6031356755852232965, 5.421189728766411748E-15, -48.10744332413860747 ) ) ;
#41051 = ADVANCED_FACE ( 'NONE', ( #21822 ), #12009, .F. ) ;
#41052 = ORIENTED_EDGE ( 'NONE', *, *, #21979, .F. ) ;
#41053 = CARTESIAN_POINT ( 'NONE',  ( 0.6845945791218023269, -38.17654861005544831, 27.25724962166981058 ) ) ;
#41054 = B_SPLINE_CURVE_WITH_KNOTS ( 'NONE', 3,
 ( #47086, #32362, #18568, #52062, #28262, #37693, #349, #43318, #9774, #8529, #56450, #18266, #18891, #13883, #37377, #28879 ),
 .UNSPECIFIED., .F., .F.,
 ( 4, 3, 3, 3, 3, 4 ),
 ( 6.939740885162003740E-18, 0.0002732102107931858796, 0.0004098135523333801787, 0.0005464168938824975159, 0.0008195847345945385647, 0.001092771384553108084 ),
 .UNSPECIFIED. ) ;
#41056 = EDGE_CURVE ( 'NONE', #21415, #2779, #49700, .T. ) ;
#41055 = ORIENTED_EDGE ( 'NONE', *, *, #23460, .T. ) ;
#41057 = VERTEX_POINT ( 'NONE', #53759 ) ;
#41058 = FACE_OUTER_BOUND ( 'NONE', #58773, .T. ) ;
#41060 = DIRECTION ( 'NONE',  ( -1.000000000000000000, -0.000000000000000000, -0.000000000000000000 ) ) ;
#41059 = B_SPLINE_CURVE_WITH_KNOTS ( 'NONE', 3,
 ( #15180, #48988, #39001, #25477, #58665, #53656, #5122, #44019, #10787, #10161, #428, #34284, #15483, #748, #52752, #20483 ),
 .UNSPECIFIED., .F., .F.,
 ( 4, 3, 3, 3, 3, 4 ),
 ( 1.962735358247463844E-17, 0.0002612764279487723496, 0.0003919131003184841782, 0.0005225497727000665569, 0.0007837925190632412343, 0.001045051706266714349 ),
 .UNSPECIFIED. ) ;
#41061 = DIRECTION ( 'NONE',  ( 1.000000000000000000, 0.000000000000000000, 0.000000000000000000 ) ) ;
#41062 = EDGE_CURVE ( 'NONE', #14203, #49966, #3792, .T. ) ;
#41063 = CARTESIAN_POINT ( 'NONE',  ( 5.896782393890504181, 19.00205529748295774, -6.591508275759957236 ) ) ;
#41064 = CARTESIAN_POINT ( 'NONE',  ( 0.6023142530420679819, 44.54505940664460439, 18.16775455049960541 ) ) ;
#41065 = ORIENTED_EDGE ( 'NONE', *, *, #6632, .F. ) ;
#41066 = CARTESIAN_POINT ( 'NONE',  ( 0.9756950546413938330, 11.19893879603448106, 41.42124338356081381 ) ) ;
#41067 = EDGE_CURVE ( 'NONE', #6072, #14441, #24789, .T. ) ;
#41068 = CARTESIAN_POINT ( 'NONE',  ( 4.975801465491695552, 0.000000000000000000, 0.000000000000000000 ) ) ;
#41069 = DIRECTION ( 'NONE',  ( 1.000000000000000000, 0.000000000000000000, 0.000000000000000000 ) ) ;
#41070 = ORIENTED_EDGE ( 'NONE', *, *, #34385, .F. ) ;
#41071 = ORIENTED_EDGE ( 'NONE', *, *, #20767, .T. ) ;
#41072 = CARTESIAN_POINT ( 'NONE',  ( 0.1084644655670282676, -21.90577137312966727, -37.14658555883725199 ) ) ;
#41073 = CARTESIAN_POINT ( 'NONE',  ( -6.001507490154110336, 2.444174634178409633, -18.68469198366094020 ) ) ;
#41074 = CARTESIAN_POINT ( 'NONE',  ( 0.5837157313716013762, -44.33100354085927819, 15.29703202070088253 ) ) ;
#41075 = ORIENTED_EDGE ( 'NONE', *, *, #36641, .T. ) ;
#41076 = CARTESIAN_POINT ( 'NONE',  ( 0.8557997880470599172, -44.60232077416698360, 17.48760788519201981 ) ) ;
#41077 = CARTESIAN_POINT ( 'NONE',  ( 0.9762797500689124330, 9.222352665238926051, -40.88120590813907285 ) ) ;
#41078 = EDGE_CURVE ( 'NONE', #51621, #33107, #8349, .T. ) ;
#41079 = ORIENTED_EDGE ( 'NONE', *, *, #36870, .T. ) ;
#41080 = CARTESIAN_POINT ( 'NONE',  ( -16.98648177666931858, 7.159091074317976755, -1.550344604434408250E-15 ) ) ;
#41081 = ORIENTED_EDGE ( 'NONE', *, *, #57480, .T. ) ;
#41082 = EDGE_CURVE ( 'NONE', #3613, #11994, #15037, .T. ) ;
#41083 = DIRECTION ( 'NONE',  ( 0.09722883295013598492, -0.7930735330831429897, -0.6013159944373470678 ) ) ;
#41084 = CARTESIAN_POINT ( 'NONE',  ( 0.5797568665920724840, -44.09074206032379806, 15.97597487391192850 ) ) ;
#41085 = CARTESIAN_POINT ( 'NONE',  ( 0.9790320750461918298, 9.798880805960621387, -40.74701298859544352 ) ) ;
#41086 = CARTESIAN_POINT ( 'NONE',  ( -2.601141883200665639, 11.65089574274779949, -9.330169122851405206 ) ) ;
#41087 = AXIS2_PLACEMENT_3D ( 'NONE', #60552, #31137, #3538 ) ;
#41088 = ORIENTED_EDGE ( 'NONE', *, *, #53441, .T. ) ;
#41089 = CARTESIAN_POINT ( 'NONE',  ( 0.9754292589017206083, 41.60825678442307662, 5.008036966395961187 ) ) ;
#41090 = CARTESIAN_POINT ( 'NONE',  ( 0.1313383488274094957, -25.74310646082176035, 34.59671037481825806 ) ) ;
#41091 = CARTESIAN_POINT ( 'NONE',  ( 0.3676999524040366896, 33.04872056100262512, -29.21870381457057775 ) ) ;
#41092 = AXIS2_PLACEMENT_3D ( 'NONE', #44244, #48910, #49521 ) ;
#41093 = CARTESIAN_POINT ( 'NONE',  ( 0.5807400328401574052, 29.58941477093070205, -37.66660715020834971 ) ) ;
#41094 = CARTESIAN_POINT ( 'NONE',  ( 1.511340767998295531, -0.4710343482720885655, 46.93530765796581505 ) ) ;
#41095 = CARTESIAN_POINT ( 'NONE',  ( 0.5817216825391109403, 32.92749829871815592, 33.39183744562994605 ) ) ;
#41096 = CARTESIAN_POINT ( 'NONE',  ( 2.299746137290199055, 33.90759634673861456, 35.41971552218871722 ) ) ;
#41097 = B_SPLINE_CURVE_WITH_KNOTS ( 'NONE', 3,
 ( #60675, #50666, #22181, #31577 ),
 .UNSPECIFIED., .F., .F.,
 ( 4, 4 ),
 ( 1.084202172485504434E-19, 0.004446298630425057213 ),
 .UNSPECIFIED. ) ;
#41098 = CARTESIAN_POINT ( 'NONE',  ( 4.553261556744875094, 0.000000000000000000, 0.000000000000000000 ) ) ;
#41099 = EDGE_CURVE ( 'NONE', #53021, #26015, #55687, .T. ) ;
#41100 = CARTESIAN_POINT ( 'NONE',  ( 4.960386119450151732, 42.78128882304991976, 9.175935446107084559 ) ) ;
#41101 = EDGE_LOOP ( 'NONE', ( #14611, #56177, #60490, #52784 ) ) ;
#41102 = CARTESIAN_POINT ( 'NONE',  ( 4.956653778116949738, -36.51451553856396970, -31.29546495791881000 ) ) ;
#41103 = CARTESIAN_POINT ( 'NONE',  ( 0.6845945791218023269, 10.02997083121021582, -45.82364243312635921 ) ) ;
#41104 = CARTESIAN_POINT ( 'NONE',  ( 0.7762777257811891429, 44.59086130178278040, -17.50713318242589622 ) ) ;
#41105 = ORIENTED_EDGE ( 'NONE', *, *, #60165, .F. ) ;
#41106 = CARTESIAN_POINT ( 'NONE',  ( 0.8753041380234530822, 48.36002538446245325, 8.511537621788884067 ) ) ;
#41107 =( BOUNDED_SURFACE ( )  B_SPLINE_SURFACE ( 3, 1, ( 
 ( #31209, #60013 ),
 ( #1755, #16497 ),
 ( #35310, #7375 ),
 ( #59389, #35929 ) ),
 .UNSPECIFIED., .F., .F., .F. ) 
 B_SPLINE_SURFACE_WITH_KNOTS ( ( 4, 4 ),
 ( 2, 2 ),
 ( 0.000000000000000000, 1.000000000000000000 ),
 ( 0.000000000000000000, 1.000000000000000000 ),
 .UNSPECIFIED. ) 
 GEOMETRIC_REPRESENTATION_ITEM ( )  RATIONAL_B_SPLINE_SURFACE ( (
 ( 1.000000000000000000, 1.000000000000000000),
 ( 0.9953040768229013402, 0.8617119497784988535),
 ( 0.9953040768229013402, 0.8617119497784988535),
 ( 1.000000000000000000, 1.000000000000000000) ) ) 
 REPRESENTATION_ITEM ( '' )  SURFACE ( )  );
#41108 = DIRECTION ( 'NONE',  ( 0.09835009131224566048, -0.1375559175655364230, 0.9855991218957007582 ) ) ;
#41109 = ORIENTED_EDGE ( 'NONE', *, *, #29408, .F. ) ;
#41110 = DIRECTION ( 'NONE',  ( -1.000000000000000000, -0.000000000000000000, -0.000000000000000000 ) ) ;
#41111 = CARTESIAN_POINT ( 'NONE',  ( 0.9756354156337461170, -41.41248945940454718, -11.23134828980320066 ) ) ;
#41112 = DIRECTION ( 'NONE',  ( 0.07439287786467665975, 0.9868880006907381208, 0.1432402660415323659 ) ) ;
#41113 = ORIENTED_EDGE ( 'NONE', *, *, #38057, .T. ) ;
#41114 = CARTESIAN_POINT ( 'NONE',  ( 4.967162193818129623, -18.65818244221285127, 38.83676580803761169 ) ) ;
#41115 = VERTEX_POINT ( 'NONE', #35939 ) ;
#41116 = VERTEX_POINT ( 'NONE', #54072 ) ;
#41117 = CARTESIAN_POINT ( 'NONE',  ( 0.1149546198390368201, 44.01516278036778829, 3.100324247711259584 ) ) ;
#41118 = EDGE_LOOP ( 'NONE', ( #32939, #8463, #48014, #32761 ) ) ;
#41119 = CARTESIAN_POINT ( 'NONE',  ( 0.5807400328401574052, 0.5448834511089933885, 47.89582301953903709 ) ) ;
#41120 = EDGE_LOOP ( 'NONE', ( #49813, #21111, #3421, #33264 ) ) ;
#41121 =( BOUNDED_SURFACE ( )  B_SPLINE_SURFACE ( 3, 1, ( 
 ( #27349, #6980 ),
 ( #12656, #7290 ),
 ( #60229, #22344 ),
 ( #2915, #45552 ) ),
 .UNSPECIFIED., .F., .F., .F. ) 
 B_SPLINE_SURFACE_WITH_KNOTS ( ( 4, 4 ),
 ( 2, 2 ),
 ( 0.000000000000000000, 1.000000000000000000 ),
 ( 0.000000000000000000, 1.000000000000000000 ),
 .UNSPECIFIED. ) 
 GEOMETRIC_REPRESENTATION_ITEM ( )  RATIONAL_B_SPLINE_SURFACE ( (
 ( 1.000000000000000000, 1.000000000000000000),
 ( 0.7223157951917476005, 0.9931996967497186413),
 ( 0.7223157951917476005, 0.9931996967497186413),
 ( 1.000000000000000000, 1.000000000000000000) ) ) 
 REPRESENTATION_ITEM ( '' )  SURFACE ( )  );
#41122 = AXIS2_PLACEMENT_3D ( 'NONE', #12911, #36717, #31381 ) ;
#41123 = CARTESIAN_POINT ( 'NONE',  ( 3.680882792899938138, 16.63701193713989568, -44.99870212802625247 ) ) ;
#41124 = EDGE_CURVE ( 'NONE', #37598, #1001, #51615, .T. ) ;
#41125 = ORIENTED_EDGE ( 'NONE', *, *, #35694, .F. ) ;
#41126 = CARTESIAN_POINT ( 'NONE',  ( 4.000000000000003553, 0.3904826640788068293, -5.599999999999999645 ) ) ;
#41127 = CARTESIAN_POINT ( 'NONE',  ( 47.98570199392409563, 12.47176666825323288, -0.8548734444802772448 ) ) ;
#41128 = CARTESIAN_POINT ( 'NONE',  ( 4.226256110419178924, -37.05036947536322600, 23.62408456906341669 ) ) ;
#41129 = CARTESIAN_POINT ( 'NONE',  ( 0.5800708057587377064, 18.90714313908718580, -44.00606528161367237 ) ) ;
#41130 = VERTEX_POINT ( 'NONE', #49091 ) ;
#41131 = EDGE_CURVE ( 'NONE', #38091, #10566, #13907, .T. ) ;
#41132 = CARTESIAN_POINT ( 'NONE',  ( 0.8744876279028263033, 3.827863332834932297, 48.94586308039354350 ) ) ;
#41133 = ORIENTED_EDGE ( 'NONE', *, *, #17076, .F. ) ;
#41134 = CARTESIAN_POINT ( 'NONE',  ( -5.719999999999997087, -15.99999999999999645, 1.959434878635764737E-15 ) ) ;
#41135 = CARTESIAN_POINT ( 'NONE',  ( 0.9749527285493300166, 25.89384247702570008, 34.21468599366719587 ) ) ;
#41136 = ORIENTED_EDGE ( 'NONE', *, *, #9060, .T. ) ;
#41137 = CARTESIAN_POINT ( 'NONE',  ( 11.40403086437694569, 0.6959691356230525150, 0.000000000000000000 ) ) ;
#41138 = CARTESIAN_POINT ( 'NONE',  ( 0.8760168074886965917, 46.68716261866176609, -11.58706983520276879 ) ) ;
#41139 = DIRECTION ( 'NONE',  ( -0.07439287786467652097, -0.5965490341031320920, 0.7991213610169807247 ) ) ;
#41140 = ORIENTED_EDGE ( 'NONE', *, *, #33638, .T. ) ;
#41141 = VERTEX_POINT ( 'NONE', #42714 ) ;
#41142 = CARTESIAN_POINT ( 'NONE',  ( 4.967162193818130511, 23.56777426397228936, -36.06913038482774425 ) ) ;
#41143 = CARTESIAN_POINT ( 'NONE',  ( 2.185380717157383135, 42.21983218090981183, 12.50222274969580383 ) ) ;
#41144 = DIRECTION ( 'NONE',  ( 1.000000000000000000, 0.000000000000000000, 0.000000000000000000 ) ) ;
#41145 = B_SPLINE_CURVE_WITH_KNOTS ( 'NONE', 3,
 ( #223, #28141, #37567, #37257, #32553, #33169 ),
 .UNSPECIFIED., .F., .F.,
 ( 4, 2, 4 ),
 ( 1.951563910473907981E-18, 0.0002447193893791718765, 0.0004894387787583418014 ),
 .UNSPECIFIED. ) ;
#41146 = ADVANCED_FACE ( 'NONE', ( #4447 ), #16726, .F. ) ;
#41147 = CARTESIAN_POINT ( 'NONE',  ( 0.5824935313925958535, 4.331522541955116878, -46.69556820001628950 ) ) ;
#41148 = DIRECTION ( 'NONE',  ( 0.000000000000000000, 0.000000000000000000, 1.000000000000000000 ) ) ;
#41149 = CARTESIAN_POINT ( 'NONE',  ( 0.6031357023905875581, 12.49325238079538103, -46.45693331047446861 ) ) ;
#41150 = CARTESIAN_POINT ( 'NONE',  ( 2.618530812446115519, 36.00211569111162646, -30.22539420689188105 ) ) ;
#41151 = LINE ( 'NONE', #2587, #57201 ) ;
#41152 = CARTESIAN_POINT ( 'NONE',  ( 3.238741278300273585, -14.74792908357277099, -40.38334873621877819 ) ) ;
#41153 = CARTESIAN_POINT ( 'NONE',  ( 0.6846871229502932144, -11.56285438919599606, -46.49193983736603286 ) ) ;
#41154 = CARTESIAN_POINT ( 'NONE',  ( 4.060580049360325461, 40.92264867182483812, -16.02512152969835668 ) ) ;
#41156 = B_SPLINE_CURVE_WITH_KNOTS ( 'NONE', 3,
 ( #52079, #4443, #8869, #32689 ),
 .UNSPECIFIED., .F., .F.,
 ( 4, 4 ),
 ( 0.000000000000000000, 0.005013413432710147645 ),
 .UNSPECIFIED. ) ;
#41155 = CARTESIAN_POINT ( 'NONE',  ( 0.5998501479064699549, -34.38546660123274989, -33.64490850298832925 ) ) ;
#41157 = CARTESIAN_POINT ( 'NONE',  ( 0.9790724872846766624, -22.58437671703066130, 35.30270723733094940 ) ) ;
#41158 = VECTOR ( 'NONE', #37932, 1000.000000000000114 ) ;
#41159 = CARTESIAN_POINT ( 'NONE',  ( 0.6252788684277231779, -38.93999277421796279, 29.91857773888190053 ) ) ;
#41160 = B_SPLINE_CURVE_WITH_KNOTS ( 'NONE', 3,
 ( #4724, #28870, #32663, #3504 ),
 .UNSPECIFIED., .F., .F.,
 ( 4, 4 ),
 ( 2.276824562219559311E-18, 0.004446298630425058948 ),
 .UNSPECIFIED. ) ;
#41161 = CARTESIAN_POINT ( 'NONE',  ( 0.6026112563231247332, 16.79644620207902861, 46.14564323839112348 ) ) ;
#41162 = CARTESIAN_POINT ( 'NONE',  ( 0.6028777368367060907, -47.52337658901180362, 12.37208579383598206 ) ) ;
#41163 = B_SPLINE_CURVE_WITH_KNOTS ( 'NONE', 3,
 ( #49579, #6634, #28827, #15057, #53241, #9404 ),
 .UNSPECIFIED., .F., .F.,
 ( 4, 2, 4 ),
 ( 1.541099475799976578E-16, 0.0002445252820015208703, 0.0004890505640028875670 ),
 .UNSPECIFIED. ) ;
#41165 = ORIENTED_EDGE ( 'NONE', *, *, #22290, .F. ) ;
#41164 = CARTESIAN_POINT ( 'NONE',  ( 0.6041374136657476912, 47.67304777898699086, -6.452348380035426878 ) ) ;
#41166 = VERTEX_POINT ( 'NONE', #23587 ) ;
#41167 = CARTESIAN_POINT ( 'NONE',  ( 0.9754292589017249382, -11.85895077972789124, 40.19568077914918547 ) ) ;
#41168 = CARTESIAN_POINT ( 'NONE',  ( 0.7245667037590761694, -48.09508190954919371, 0.8205429720402956928 ) ) ;
#41169 = CARTESIAN_POINT ( 'NONE',  ( 0.8744876279028306332, 44.61213666265828692, 20.49651952824657286 ) ) ;
#41170 = ORIENTED_EDGE ( 'NONE', *, *, #851, .F. ) ;
#41171 = VERTEX_POINT ( 'NONE', #52388 ) ;
#41172 = CARTESIAN_POINT ( 'NONE',  ( 4.553261556744875094, 27.21079963941838997, 34.48350256002230196 ) ) ;
#41173 = EDGE_CURVE ( 'NONE', #59625, #17743, #18912, .T. ) ;
#41174 = UNCERTAINTY_MEASURE_WITH_UNIT (LENGTH_MEASURE( 1.000000000000000082E-05 ), #17423, 'distance_accuracy_value', 'NONE');
#41175 = VERTEX_POINT ( 'NONE', #50616 ) ;
#41176 = ORIENTED_EDGE ( 'NONE', *, *, #56476, .F. ) ;
#41177 = CARTESIAN_POINT ( 'NONE',  ( 0.1073791018717578927, 30.83464511437137645, -30.14884492832358731 ) ) ;
#41178 = ADVANCED_FACE ( 'NONE', ( #33011 ), #7951, .F. ) ;
#41179 = DIRECTION ( 'NONE',  ( 0.000000000000000000, 0.000000000000000000, 1.000000000000000000 ) ) ;
#41180 = CARTESIAN_POINT ( 'NONE',  ( 0.5837800005270554760, -38.66303329572635761, -26.54063139820414108 ) ) ;
#41181 = ORIENTED_EDGE ( 'NONE', *, *, #6062, .T. ) ;
#41182 = CARTESIAN_POINT ( 'NONE',  ( 4.967162193818130511, -40.65506779172153529, -14.26841313271325795 ) ) ;
#41183 = CARTESIAN_POINT ( 'NONE',  ( 4.962356264823608143, 1.841560470688809792, -42.04574000888963781 ) ) ;
#41184 = CARTESIAN_POINT ( 'NONE',  ( 0.1098349054025746507, 21.37724154645449914, 37.45309339978490470 ) ) ;
#41185 = ORIENTED_EDGE ( 'NONE', *, *, #41485, .F. ) ;
#41186 = EDGE_CURVE ( 'NONE', #5328, #51700, #19217, .T. ) ;
#41187 = ORIENTED_EDGE ( 'NONE', *, *, #36217, .T. ) ;
#41188 = CARTESIAN_POINT ( 'NONE',  ( 0.6064782688330881966, 10.17905733607075724, 45.77904802601024414 ) ) ;
#41189 = ORIENTED_EDGE ( 'NONE', *, *, #42951, .F. ) ;
#41190 = CARTESIAN_POINT ( 'NONE',  ( 0.000000000000000000, 0.000000000000000000, 0.000000000000000000 ) ) ;
#41191 = DIRECTION ( 'NONE',  ( 0.07906939808003035641, 0.1578407582592837588, 0.9842938206244089550 ) ) ;
#41192 = DIRECTION ( 'NONE',  ( 0.1024043820194936449, -0.9573600124648778964, 0.2701391291102688275 ) ) ;
#41193 = CARTESIAN_POINT ( 'NONE',  ( 0.7242003506639999033, 16.18715005828274300, -46.35717686741356403 ) ) ;
#41194 = CARTESIAN_POINT ( 'NONE',  ( 0.5809828226811617480, 12.92184523170268839, -46.11980934799325382 ) ) ;
#41195 = ADVANCED_FACE ( 'NONE', ( #5071 ), #48689, .F. ) ;
#41196 = B_SPLINE_CURVE_WITH_KNOTS ( 'NONE', 3,
 ( #8211, #36440, #12636, #50817, #7910, #27330, #3500, #1503, #35062, #10944, #1203, #11239, #40089, #43537, #20335, #30025, #49137, #48518, #30329, #39152, #20636, #29103, #54117, #49441, #39455 ),
 .UNSPECIFIED., .F., .F.,
 ( 4, 3, 3, 3, 3, 3, 3, 3, 4 ),
 ( 4.670885906470169154E-18, 0.0005656085177311393148, 0.001131215744874498755, 0.001696821861372766567, 0.002262427090022498151, 0.002828031679238745925, 0.003393635864401605730, 0.003977030878808132490, 0.004561030005651159000 ),
 .UNSPECIFIED. ) ;
#41197 = ORIENTED_EDGE ( 'NONE', *, *, #34182, .T. ) ;
#41198 = DIRECTION ( 'NONE',  ( 0.09722883295013594329, 0.3508110149947525902, 0.9313850899609172895 ) ) ;
#41199 = VECTOR ( 'NONE', #25222, 1000.000000000000000 ) ;
#41200 = DIRECTION ( 'NONE',  ( 1.000000000000000000, 1.836970198721027715E-16, 2.280301054154487250E-31 ) ) ;
#41201 = EDGE_CURVE ( 'NONE', #38564, #19953, #36731, .T. ) ;
#41202 = CARTESIAN_POINT ( 'NONE',  ( 0.8753041380234471980, -8.714053517584197550, 48.32394436680080219 ) ) ;
#41203 = ORIENTED_EDGE ( 'NONE', *, *, #60948, .F. ) ;
#41204 = CARTESIAN_POINT ( 'NONE',  ( 0.1081432562775998668, 42.80885385101081653, -5.208748643066250850 ) ) ;
#41205 = FACE_OUTER_BOUND ( 'NONE', #19832, .T. ) ;
#41206 = CARTESIAN_POINT ( 'NONE',  ( 0.9747592971366234593, 30.56898208368274084, 30.11108831501845629 ) ) ;
#41207 = CARTESIAN_POINT ( 'NONE',  ( 0.2230388203127576796, 29.94794547692447395, -31.02270543585797213 ) ) ;
#41208 = ORIENTED_EDGE ( 'NONE', *, *, #45036, .F. ) ;
#41209 = CARTESIAN_POINT ( 'NONE',  ( 4.962356264823608143, 0.000000000000000000, 0.000000000000000000 ) ) ;
#41210 = CARTESIAN_POINT ( 'NONE',  ( 0.9754292580325127915, 20.64935461952654805, -36.46822755085641177 ) ) ;
#41211 = CARTESIAN_POINT ( 'NONE',  ( 0.5850706913938534814, 24.10530971368288178, 41.38834827854216769 ) ) ;
#41212 = EDGE_CURVE ( 'NONE', #5378, #59500, #44235, .T. ) ;
#41213 = B_SPLINE_CURVE_WITH_KNOTS ( 'NONE', 3,
 ( #58602, #53296, #48608, #16037, #29501, #15111 ),
 .UNSPECIFIED., .F., .F.,
 ( 4, 2, 4 ),
 ( 1.261467247513764704E-16, 0.0002450741128632345106, 0.0004901482257263428200 ),
 .UNSPECIFIED. ) ;
#41214 = CARTESIAN_POINT ( 'NONE',  ( 0.6009452777970412107, -41.44251326863946616, 24.43074291040833756 ) ) ;
#41215 = CARTESIAN_POINT ( 'NONE',  ( 0.5824935313925933000, -46.76557014396445311, 3.495658187492202362 ) ) ;
#41216 =( REPRESENTATION_RELATIONSHIP ('NONE','NONE', #44881, #13 ) REPRESENTATION_RELATIONSHIP_WITH_TRANSFORMATION ( #24253 )SHAPE_REPRESENTATION_RELATIONSHIP( ) );
#41217 = CARTESIAN_POINT ( 'NONE',  ( 4.967162193818130511, -36.06913038482816347, 23.56777426397165698 ) ) ;
#41218 =( BOUNDED_SURFACE ( )  B_SPLINE_SURFACE ( 3, 1, ( 
 ( #54840, #45793 ),
 ( #2839, #6584 ),
 ( #25730, #21037 ),
 ( #59857, #21971 ) ),
 .UNSPECIFIED., .F., .F., .F. ) 
 B_SPLINE_SURFACE_WITH_KNOTS ( ( 4, 4 ),
 ( 2, 2 ),
 ( 0.000000000000000000, 1.000000000000000000 ),
 ( 0.000000000000000000, 1.000000000000000000 ),
 .UNSPECIFIED. ) 
 GEOMETRIC_REPRESENTATION_ITEM ( )  RATIONAL_B_SPLINE_SURFACE ( (
 ( 1.000000000000000000, 1.000000000000000000),
 ( 0.9953040768229005630, 0.8617119497784937465),
 ( 0.9953040768229005630, 0.8617119497784937465),
 ( 1.000000000000000000, 1.000000000000000000) ) ) 
 REPRESENTATION_ITEM ( '' )  SURFACE ( )  );
#41219 = FACE_OUTER_BOUND ( 'NONE', #9668, .T. ) ;
#41220 = CARTESIAN_POINT ( 'NONE',  ( 5.959828726073459926, -5.316791119500952512, -19.82504517499711127 ) ) ;
#41221 = CARTESIAN_POINT ( 'NONE',  ( 0.6016118706126977189, 41.34544472431174711, -26.49726882780209891 ) ) ;
#41222 = CARTESIAN_POINT ( 'NONE',  ( 4.833616638992208614, -46.17873762321151787, -2.572717262757827861 ) ) ;
#41223 = VERTEX_POINT ( 'NONE', #17130 ) ;
#41224 = CARTESIAN_POINT ( 'NONE',  ( -16.30394644734282394, -12.43472632814719070, -1.280860982936265380 ) ) ;
#41225 = CARTESIAN_POINT ( 'NONE',  ( 4.956653778116959508, -15.97476558431919180, 45.35992544608522792 ) ) ;
#41226 = CARTESIAN_POINT ( 'NONE',  ( 0.5809828226811553087, -0.5448590168529036104, -47.89273459658654275 ) ) ;
#41227 = CARTESIAN_POINT ( 'NONE',  ( 0.5806925824938494740, -35.14454992382308518, -31.04968555389040219 ) ) ;
#41228 = CARTESIAN_POINT ( 'NONE',  ( 0.6846871229502899947, -46.49193983736581970, -11.56285438919680963 ) ) ;
#41229 = CARTESIAN_POINT ( 'NONE',  ( 0.9762797500689124330, -31.41867615533404390, 27.73430319715907544 ) ) ;
#41230 = SHAPE_DEFINITION_REPRESENTATION ( #21778, #40484 ) ;
#41231 = CARTESIAN_POINT ( 'NONE',  ( 0.5804410086790514622, -42.10186154173687356, 20.66284362269178132 ) ) ;
#41232 = CARTESIAN_POINT ( 'NONE',  ( 3.376099380956842921, -10.78512648832982634, 7.961747940169504822 ) ) ;
#41233 = CARTESIAN_POINT ( 'NONE',  ( -2.569797478183790229, -14.44232325624825108, -2.353985772484699979 ) ) ;
#41234 = ADVANCED_FACE ( 'NONE', ( #47711 ), #38328, .F. ) ;
#41236 = VERTEX_POINT ( 'NONE', #57081 ) ;
#41235 = CARTESIAN_POINT ( 'NONE',  ( 3.782542959838396168, -14.09167658397165468, 39.60634424494784156 ) ) ;
#41237 = ORIENTED_EDGE ( 'NONE', *, *, #9809, .F. ) ;
#41238 = CARTESIAN_POINT ( 'NONE',  ( 0.5987334363312691865, 27.59677704409741139, 40.61995572684014633 ) ) ;
#41239 = CARTESIAN_POINT ( 'NONE',  ( -6.001507490154110336, 7.225628667346580158, 17.40350523682697670 ) ) ;
#41240 = CARTESIAN_POINT ( 'NONE',  ( 3.238018933889920792, -11.19612451184702273, 7.352162150202567581 ) ) ;
#41241 = ADVANCED_FACE ( 'NONE', ( #68 ), #29674, .T. ) ;
#41242 = ORIENTED_EDGE ( 'NONE', *, *, #54946, .T. ) ;
#41243 = LINE ( 'NONE', #60303, #38540 ) ;
#41244 = CARTESIAN_POINT ( 'NONE',  ( 0.7762783648524410607, -23.17763242108785349, 41.92424098267934340 ) ) ;
#41245 = CARTESIAN_POINT ( 'NONE',  ( 0.1087620492084206830, 41.74735017127130732, -10.81135549499737003 ) ) ;
#41246 = VECTOR ( 'NONE', #31278, 1000.000000000000114 ) ;
#41247 = EDGE_CURVE ( 'NONE', #51225, #23152, #2356, .T. ) ;
#41248 = ORIENTED_EDGE ( 'NONE', *, *, #52038, .F. ) ;
#41249 = ORIENTED_EDGE ( 'NONE', *, *, #59461, .T. ) ;
#41250 = CARTESIAN_POINT ( 'NONE',  ( 0.7762783648524383961, -43.90991295203431832, 19.15108798908297416 ) ) ;
#41251 = ADVANCED_FACE ( 'NONE', ( #53315 ), #50755, .F. ) ;
#41252 = DIRECTION ( 'NONE',  ( 0.000000000000000000, 0.000000000000000000, 1.000000000000000000 ) ) ;
#41253 = B_SPLINE_CURVE_WITH_KNOTS ( 'NONE', 3,
 ( #33642, #390, #33033, #88 ),
 .UNSPECIFIED., .F., .F.,
 ( 4, 4 ),
 ( 5.485677294651096434E-18, 0.004042984057420971958 ),
 .UNSPECIFIED. ) ;
#41254 = FACE_OUTER_BOUND ( 'NONE', #7103, .T. ) ;
#41255 = ORIENTED_EDGE ( 'NONE', *, *, #2970, .F. ) ;
#41256 = CARTESIAN_POINT ( 'NONE',  ( 0.8744876279028306332, 43.84003649649945089, -22.09980204357244560 ) ) ;
#41257 = CARTESIAN_POINT ( 'NONE',  ( 0.1135584504625007513, -42.56957105991563139, -11.60963702748914628 ) ) ;
#41258 = CARTESIAN_POINT ( 'NONE',  ( -6.078726893082806448, 5.482141236671949969, 18.45914864585853721 ) ) ;
#41259 = CARTESIAN_POINT ( 'NONE',  ( 0.5980894510889457338, 17.76188940524948023, -44.71414919659888199 ) ) ;
#41260 = VERTEX_POINT ( 'NONE', #24512 ) ;
#41261 = EDGE_CURVE ( 'NONE', #473, #29981, #58009, .T. ) ;
#41262 = CARTESIAN_POINT ( 'NONE',  ( -6.078075953587585900, -4.290048539733580135, 18.77207121693995973 ) ) ;
#41263 = SURFACE_STYLE_FILL_AREA ( #46571 ) ;
#41264 = VERTEX_POINT ( 'NONE', #43654 ) ;
#41265 = CARTESIAN_POINT ( 'NONE',  ( 4.967162193818130511, -28.07411493385318124, 32.68434214048159703 ) ) ;
#41266 = ADVANCED_FACE ( 'NONE', ( #17740 ), #18699, .T. ) ;
#41267 = CARTESIAN_POINT ( 'NONE',  ( 5.901463166500145796, -9.678444301826402807, 17.63081354439098547 ) ) ;
#41268 = CARTESIAN_POINT ( 'NONE',  ( 0.7413678028165009426, 39.31562913345087651, -19.96916116443533440 ) ) ;
#41269 = CARTESIAN_POINT ( 'NONE',  ( 5.880360259849752858, -21.17507050419485637, -43.04573319267437626 ) ) ;
#41270 = ORIENTED_EDGE ( 'NONE', *, *, #14237, .F. ) ;
#41271 = ORIENTED_EDGE ( 'NONE', *, *, #7259, .T. ) ;
#41272 = LINE ( 'NONE', #4547, #48017 ) ;
#41273 = ORIENTED_EDGE ( 'NONE', *, *, #49277, .F. ) ;
#41274 = ADVANCED_FACE ( 'NONE', ( #23593 ), #5388, .T. ) ;
#41275 = CARTESIAN_POINT ( 'NONE',  ( 0.5804410086790514622, 17.36461428077125291, 43.56592731407689456 ) ) ;
#41276 = ORIENTED_EDGE ( 'NONE', *, *, #2168, .T. ) ;
#41277 = CARTESIAN_POINT ( 'NONE',  ( 3.678834586032788234, -40.32777138951392715, 27.78998424582957227 ) ) ;
#41278 = ORIENTED_EDGE ( 'NONE', *, *, #42801, .T. ) ;
#41279 = CARTESIAN_POINT ( 'NONE',  ( -2.708315649062910779, 7.087851317223793579, 12.80362818457447638 ) ) ;
#41280 = B_SPLINE_CURVE_WITH_KNOTS ( 'NONE', 3,
 ( #58892, #20393, #35432, #39522 ),
 .UNSPECIFIED., .F., .F.,
 ( 4, 4 ),
 ( 2.054184040232706591E-17, 0.004444306975806115896 ),
 .UNSPECIFIED. ) ;
#41281 = CARTESIAN_POINT ( 'NONE',  ( 0.1087620492084206414, -26.53886348603028367, 33.99140154262259017 ) ) ;
#41282 = VERTEX_POINT ( 'NONE', #43038 ) ;
#41283 = CARTESIAN_POINT ( 'NONE',  ( 0.1156495703730067437, -27.61742026461291744, -34.41251300266834079 ) ) ;
#41284 = CARTESIAN_POINT ( 'NONE',  ( 0.5809828226811560858, -41.74875432577632495, -23.47450554821754309 ) ) ;
#41285 = CARTESIAN_POINT ( 'NONE',  ( 5.894904586330512508, -18.51647496758820921, -7.852997315440910064 ) ) ;
#41287 = ORIENTED_EDGE ( 'NONE', *, *, #46232, .T. ) ;
#41286 = EDGE_CURVE ( 'NONE', #21723, #52990, #35230, .T. ) ;
#41288 = AXIS2_PLACEMENT_3D ( 'NONE', #37304, #56071, #37618 ) ;
#41289 = EDGE_LOOP ( 'NONE', ( #40288, #30286, #44090, #32307 ) ) ;
#41290 =( BOUNDED_SURFACE ( )  B_SPLINE_SURFACE ( 3, 1, ( 
 ( #268, #19415 ),
 ( #47605, #33211 ),
 ( #47922, #38532 ),
 ( #29109, #42926 ) ),
 .UNSPECIFIED., .F., .F., .F. ) 
 B_SPLINE_SURFACE_WITH_KNOTS ( ( 4, 4 ),
 ( 2, 2 ),
 ( 0.000000000000000000, 1.000000000000000000 ),
 ( 0.000000000000000000, 1.000000000000000000 ),
 .UNSPECIFIED. ) 
 GEOMETRIC_REPRESENTATION_ITEM ( )  RATIONAL_B_SPLINE_SURFACE ( (
 ( 1.000000000000000000, 1.000000000000000000),
 ( 0.7211978278499970862, 0.9934217856018976445),
 ( 0.7211978278499970862, 0.9934217856018976445),
 ( 1.000000000000000000, 1.000000000000000000) ) ) 
 REPRESENTATION_ITEM ( '' )  SURFACE ( )  );
#41291 = CIRCLE ( 'NONE', #19284, 42.08604991992415023 ) ;
#41292 = PLANE ( 'NONE',  #59491 ) ;
#41293 = CARTESIAN_POINT ( 'NONE',  ( 1.000433927950261204, -26.55171663538948224, 32.42568459364935762 ) ) ;
#41295 = EDGE_CURVE ( 'NONE', #40053, #23307, #699, .T. ) ;
#41294 = DIRECTION ( 'NONE',  ( -1.000000000000000000, -1.558861125776144859E-16, 3.851859888774471706E-32 ) ) ;
#41296 = CARTESIAN_POINT ( 'NONE',  ( 0.1098349054025746507, 26.42143025179989380, -34.08267426123933319 ) ) ;
#41297 = DIRECTION ( 'NONE',  ( -0.000000000000000000, 1.000000000000000000, 1.224646799147353207E-16 ) ) ;
#41298 = ORIENTED_EDGE ( 'NONE', *, *, #56856, .F. ) ;
#41299 = CARTESIAN_POINT ( 'NONE',  ( 0.1100053167205930771, 37.25683392728333132, -21.71746606919068512 ) ) ;
#41300 = CARTESIAN_POINT ( 'NONE',  ( 0.7056759521545006297, 39.91793999877379662, 24.62329984732515697 ) ) ;
#41301 = VERTEX_POINT ( 'NONE', #19839 ) ;
#41302 = CARTESIAN_POINT ( 'NONE',  ( 0.9754642270333686582, -30.46484943293178205, 30.21634823122154145 ) ) ;
#41303 = DIRECTION ( 'NONE',  ( 0.000000000000000000, 1.000000000000000000, 0.000000000000000000 ) ) ;
#41304 = CARTESIAN_POINT ( 'NONE',  ( 0.8560838555295223751, -42.27062166135446120, -20.33635607586480631 ) ) ;
#41305 = CARTESIAN_POINT ( 'NONE',  ( 5.960721111146673579, -10.25731071096595137, 17.77882586010649391 ) ) ;
#41306 = B_SPLINE_CURVE_WITH_KNOTS ( 'NONE', 3,
 ( #39238, #10715, #21341, #24804 ),
 .UNSPECIFIED., .F., .F.,
 ( 4, 4 ),
 ( 0.000000000000000000, 0.005004948556313794893 ),
 .UNSPECIFIED. ) ;
#41307 = CARTESIAN_POINT ( 'NONE',  ( 0.5786265663353196143, 23.32245830379028106, 41.83999636203328265 ) ) ;
#41308 = CARTESIAN_POINT ( 'NONE',  ( 0.5997462898726536595, 32.62638226927682439, 36.70246327105753892 ) ) ;
#41309 = CARTESIAN_POINT ( 'NONE',  ( 3.661933894777896104, 38.05324307217590274, -27.65107333615731378 ) ) ;
#41310 = CARTESIAN_POINT ( 'NONE',  ( 5.960721111146673579, 5.318514366754933498, -19.82454228767740645 ) ) ;
#41311 = CARTESIAN_POINT ( 'NONE',  ( -6.017396004339686577, -18.84316306185412415, 0.001173774848916064005 ) ) ;
#41312 = CARTESIAN_POINT ( 'NONE',  ( 4.967162193818130511, -42.34252806656598977, 7.970725651239652265 ) ) ;
#41313 = CARTESIAN_POINT ( 'NONE',  ( 0.7242486021783841599, 3.898994070056987393, 48.94700509342359851 ) ) ;
#41314 = CARTESIAN_POINT ( 'NONE',  ( 1.830465331921977468, 43.86281037434080332, 4.053384011293614364 ) ) ;
#41315 = DIRECTION ( 'NONE',  ( 1.000000000000000000, 0.000000000000000000, 0.000000000000000000 ) ) ;
#41316 = FACE_OUTER_BOUND ( 'NONE', #29529, .T. ) ;
#41317 = CARTESIAN_POINT ( 'NONE',  ( -99.50001199999974233, 2.999999999999994671, 1.500000000000001554 ) ) ;
#41318 = EDGE_CURVE ( 'NONE', #25300, #29382, #10588, .T. ) ;
#41319 = PRODUCT_DEFINITION_SHAPE ( 'NONE', 'NONE',  #61985 ) ;
#41320 = CARTESIAN_POINT ( 'NONE',  ( 0.8744876279028306332, -45.83369275826206746, -17.59609782084448071 ) ) ;
#41321 = CARTESIAN_POINT ( 'NONE',  ( 1.000110580585052311, -41.19582803197042864, 7.702028014245381193 ) ) ;
#41322 = B_SPLINE_CURVE_WITH_KNOTS ( 'NONE', 3,
 ( #29901, #53683, #15820, #34935, #1374, #49621 ),
 .UNSPECIFIED., .F., .F.,
 ( 4, 2, 4 ),
 ( 3.496446946337351263E-18, 0.0002450742804987333088, 0.0004901485609974631482 ),
 .UNSPECIFIED. ) ;
#41323 = ADVANCED_FACE ( 'NONE', ( #15133 ), #1641, .F. ) ;
#41324 = ORIENTED_EDGE ( 'NONE', *, *, #38917, .F. ) ;
#41325 = CARTESIAN_POINT ( 'NONE',  ( 1.088908134280554219, 37.54826033999260915, 20.77739698351946984 ) ) ;
#41326 = EDGE_CURVE ( 'NONE', #15399, #49037, #7665, .T. ) ;
#41327 = EDGE_CURVE ( 'NONE', #21984, #49864, #18810, .T. ) ;
#41328 = LINE ( 'NONE', #56309, #60923 ) ;
#41329 = CARTESIAN_POINT ( 'NONE',  ( 3.782542959838389063, 30.43994881966847288, -28.99391952207450274 ) ) ;
#41330 = DIRECTION ( 'NONE',  ( 0.000000000000000000, 0.000000000000000000, 1.000000000000000000 ) ) ;
#41331 = EDGE_CURVE ( 'NONE', #42964, #36881, #52395, .T. ) ;
#41332 = ORIENTED_EDGE ( 'NONE', *, *, #2633, .F. ) ;
#41333 = CARTESIAN_POINT ( 'NONE',  ( 1.296416391601052265, -40.42071545795151621, 17.56340331323853476 ) ) ;
#41334 = CARTESIAN_POINT ( 'NONE',  ( 1.157643937452369487, -41.23316700651808020, -7.538448992156369322 ) ) ;
#41335 = AXIS2_PLACEMENT_3D ( 'NONE', #9630, #57846, #29661 ) ;
#41336 = CARTESIAN_POINT ( 'NONE',  ( 5.895596859100789899, -19.39920506799825262, -5.310275505304632659 ) ) ;
#41337 = B_SPLINE_CURVE_WITH_KNOTS ( 'NONE', 3,
 ( #52681, #39545, #38935, #53906, #57987, #9779 ),
 .UNSPECIFIED., .F., .F.,
 ( 4, 2, 4 ),
 ( 1.910620358896493634E-17, 0.0002293755540694311830, 0.0004587511081388432298 ),
 .UNSPECIFIED. ) ;
#41338 = ORIENTED_EDGE ( 'NONE', *, *, #55714, .T. ) ;
#41339 = EDGE_CURVE ( 'NONE', #54484, #17218, #49406, .T. ) ;
#41340 = DIRECTION ( 'NONE',  ( -1.000000000000000000, -1.836909530733580185E-16, 1.836909530733574022E-16 ) ) ;
#41341 = ORIENTED_EDGE ( 'NONE', *, *, #52556, .T. ) ;
#41342 = CARTESIAN_POINT ( 'NONE',  ( 0.5839879882012661838, -3.018602103822392988E-05, -47.89596766821095031 ) ) ;
#41343 = ORIENTED_EDGE ( 'NONE', *, *, #43766, .T. ) ;
#41344 = CARTESIAN_POINT ( 'NONE',  ( 0.6041374136657476912, 18.57118264377476535, 44.37863742124674360 ) ) ;
#41345 = CARTESIAN_POINT ( 'NONE',  ( 2.648799415243708655, 38.22150636650994926, 30.71862487749798731 ) ) ;
#41346 = ORIENTED_EDGE ( 'NONE', *, *, #19085, .F. ) ;
#41347 = CARTESIAN_POINT ( 'NONE',  ( 0.5806925824938499181, -46.82446035038572063, 2.586943222941027631 ) ) ;
#41348 = CARTESIAN_POINT ( 'NONE',  ( 0.1073791018717578927, -25.86618856530687793, -34.50606437925538472 ) ) ;
#41349 = CIRCLE ( 'NONE', #47361, 43.08621763946400307 ) ;
#41350 = ORIENTED_EDGE ( 'NONE', *, *, #59562, .F. ) ;
#41351 = CARTESIAN_POINT ( 'NONE',  ( 0.8753041380234524160, -34.64850320773157222, 34.79395857525835822 ) ) ;
#41352 = VERTEX_POINT ( 'NONE', #11053 ) ;
#41353 = CARTESIAN_POINT ( 'NONE',  ( 0.1158516988532803799, -1.365047127049809239, 44.10304757240399454 ) ) ;
#41354 = EDGE_LOOP ( 'NONE', ( #35396, #9830, #15427, #28909 ) ) ;
#41355 = ORIENTED_EDGE ( 'NONE', *, *, #14045, .F. ) ;
#41356 = DIRECTION ( 'NONE',  ( 0.000000000000000000, 0.000000000000000000, 1.000000000000000000 ) ) ;
#41357 = PLANE ( 'NONE',  #32458 ) ;
#41358 = CARTESIAN_POINT ( 'NONE',  ( 4.960156602257181468, -41.85906677498973494, 20.07163247083132873 ) ) ;
#41359 = CARTESIAN_POINT ( 'NONE',  ( 1.227938101723756947, -41.66816631169184859, -10.28900963485423858 ) ) ;
#41360 = ORIENTED_EDGE ( 'NONE', *, *, #4928, .F. ) ;
#41361 = CARTESIAN_POINT ( 'NONE',  ( 4.553261556744875094, 6.787618719203488915, 43.39893775135925580 ) ) ;
#41362 = CARTESIAN_POINT ( 'NONE',  ( 0.9791128995231621612, -17.63619210405237681, 38.01712985372675746 ) ) ;
#41363 = CARTESIAN_POINT ( 'NONE',  ( 2.879087469061463178, 0.3214110636685244549, 43.99998149671804271 ) ) ;
#41364 = ORIENTED_EDGE ( 'NONE', *, *, #37099, .T. ) ;
#41365 = ORIENTED_EDGE ( 'NONE', *, *, #9528, .F. ) ;
#41366 = CARTESIAN_POINT ( 'NONE',  ( -6.077587904424778920, -17.34643006009198274, 8.360465630828690209 ) ) ;
#41368 = EDGE_CURVE ( 'NONE', #38729, #3122, #30646, .T. ) ;
#41367 = CARTESIAN_POINT ( 'NONE',  ( 0.8744876279028306332, 5.599149760997630842, 48.77498920895230583 ) ) ;
#41369 = CARTESIAN_POINT ( 'NONE',  ( 0.9730545539215883499, 41.31259007387247095, -11.59290486963463351 ) ) ;
#41370 = VERTEX_POINT ( 'NONE', #54859 ) ;
#41371 = CARTESIAN_POINT ( 'NONE',  ( 4.553261556744875094, 0.000000000000000000, 0.000000000000000000 ) ) ;
#41372 = FACE_OUTER_BOUND ( 'NONE', #17500, .T. ) ;
#41373 =( BOUNDED_SURFACE ( )  B_SPLINE_SURFACE ( 3, 1, ( 
 ( #37968, #2313 ),
 ( #56100, #31142 ),
 ( #46733, #21440 ),
 ( #40889, #23220 ) ),
 .UNSPECIFIED., .F., .F., .F. ) 
 B_SPLINE_SURFACE_WITH_KNOTS ( ( 4, 4 ),
 ( 2, 2 ),
 ( 0.000000000000000000, 1.000000000000000000 ),
 ( 0.000000000000000000, 1.000000000000000000 ),
 .UNSPECIFIED. ) 
 GEOMETRIC_REPRESENTATION_ITEM ( )  RATIONAL_B_SPLINE_SURFACE ( (
 ( 1.000000000000000000, 1.000000000000000000),
 ( 0.9952954269826590483, 0.8620686068821307169),
 ( 0.9952954269826590483, 0.8620686068821307169),
 ( 1.000000000000000000, 1.000000000000000000) ) ) 
 REPRESENTATION_ITEM ( '' )  SURFACE ( )  );
#41374 = VERTEX_POINT ( 'NONE', #16057 ) ;
#41375 = LINE ( 'NONE', #27255, #39955 ) ;
#41376 = ORIENTED_EDGE ( 'NONE', *, *, #23484, .T. ) ;
#41377 = CARTESIAN_POINT ( 'NONE',  ( 0.8744876279028263033, 32.34273794994744833, 36.93639603806145288 ) ) ;
#41378 = CARTESIAN_POINT ( 'NONE',  ( 0.9736507210033059634, -34.31386771842680616, 25.76216842460683765 ) ) ;
#41379 = CARTESIAN_POINT ( 'NONE',  ( 0.9772918015221174759, 9.311194862264514427, -40.86121028539926670 ) ) ;
#41380 = VECTOR ( 'NONE', #42232, 1000.000000000000227 ) ;
#41381 = CARTESIAN_POINT ( 'NONE',  ( 3.894904216938897878, -43.25473375298778933, 7.819996191453038037 ) ) ;
#41382 = PRESENTATION_STYLE_ASSIGNMENT (( #51355 ) ) ;
#41383 = VERTEX_POINT ( 'NONE', #54230 ) ;
#41384 = CARTESIAN_POINT ( 'NONE',  ( -4.915099999999998914, 0.000000000000000000, 0.000000000000000000 ) ) ;
#41385 = DIRECTION ( 'NONE',  ( 1.000000000000000000, -0.000000000000000000, -0.000000000000000000 ) ) ;
#41386 = CARTESIAN_POINT ( 'NONE',  ( 0.7245667037590750592, 46.24390958543276753, -13.24050682223045783 ) ) ;
#41387 =( BOUNDED_SURFACE ( )  B_SPLINE_SURFACE ( 3, 1, ( 
 ( #7023, #17382 ),
 ( #21768, #46211 ),
 ( #31473, #36501 ),
 ( #26154, #2331 ) ),
 .UNSPECIFIED., .F., .F., .F. ) 
 B_SPLINE_SURFACE_WITH_KNOTS ( ( 4, 4 ),
 ( 2, 2 ),
 ( 0.000000000000000000, 1.000000000000000000 ),
 ( 0.000000000000000000, 1.000000000000000000 ),
 .UNSPECIFIED. ) 
 GEOMETRIC_REPRESENTATION_ITEM ( )  RATIONAL_B_SPLINE_SURFACE ( (
 ( 1.000000000000000000, 1.000000000000000000),
 ( 0.9953040768229005630, 0.8617119497784937465),
 ( 0.9953040768229005630, 0.8617119497784937465),
 ( 1.000000000000000000, 1.000000000000000000) ) ) 
 REPRESENTATION_ITEM ( '' )  SURFACE ( )  );
#41388 = CARTESIAN_POINT ( 'NONE',  ( 0.3622758884714730732, -0.8252992914325094631, -43.10531414739105571 ) ) ;
#41389 = CARTESIAN_POINT ( 'NONE',  ( 50.50000000000024869, 1.836970198721029747E-14, -7.703719777548943412E-31 ) ) ;
#41390 = CARTESIAN_POINT ( 'NONE',  ( 5.895881250540457863, -18.51513737938366333, -7.856040314996530327 ) ) ;
#41391 =( BOUNDED_SURFACE ( )  B_SPLINE_SURFACE ( 3, 1, ( 
 ( #887, #20027 ),
 ( #48817, #44462 ),
 ( #5871, #1189 ),
 ( #20323, #58812 ) ),
 .UNSPECIFIED., .F., .F., .F. ) 
 B_SPLINE_SURFACE_WITH_KNOTS ( ( 4, 4 ),
 ( 2, 2 ),
 ( 0.000000000000000000, 1.000000000000000000 ),
 ( 0.000000000000000000, 1.000000000000000000 ),
 .UNSPECIFIED. ) 
 GEOMETRIC_REPRESENTATION_ITEM ( )  RATIONAL_B_SPLINE_SURFACE ( (
 ( 1.000000000000000000, 1.000000000000000000),
 ( 0.9953485035131437453, 0.8621029689291523912),
 ( 0.9953485035131437453, 0.8621029689291523912),
 ( 1.000000000000000000, 1.000000000000000000) ) ) 
 REPRESENTATION_ITEM ( '' )  SURFACE ( )  );
#41392 = CARTESIAN_POINT ( 'NONE',  ( 0.7056759521544971880, -38.18414334534395493, -27.23453737626569549 ) ) ;
#41393 = CIRCLE ( 'NONE', #14417, 43.08621763946400307 ) ;
#41394 = CARTESIAN_POINT ( 'NONE',  ( 5.960721111146673579, 5.318514366754933498, -19.82454228767740645 ) ) ;
#41395 = EDGE_CURVE ( 'NONE', #44899, #41864, #49246, .T. ) ;
#41396 = EDGE_CURVE ( 'NONE', #29523, #55039, #54539, .T. ) ;
#41397 = CARTESIAN_POINT ( 'NONE',  ( -6.077587904424778920, -4.290907484552072049, -18.77189746277518623 ) ) ;
#41398 = CARTESIAN_POINT ( 'NONE',  ( 0.5827359174754817017, -28.86822142608426134, -38.21848266111700099 ) ) ;
#41399 = VERTEX_POINT ( 'NONE', #10740 ) ;
#41401 = EDGE_CURVE ( 'NONE', #59818, #59625, #5989, .T. ) ;
#41400 = B_SPLINE_CURVE_WITH_KNOTS ( 'NONE', 3,
 ( #53619, #25760, #34247, #20758, #20446, #30138 ),
 .UNSPECIFIED., .F., .F.,
 ( 4, 2, 4 ),
 ( 1.738108305489988542E-18, 0.0002291459268755712919, 0.0004582918537511408491 ),
 .UNSPECIFIED. ) ;
#41402 = DIRECTION ( 'NONE',  ( 0.000000000000000000, 0.7071067811865540120, -0.7071067811865409114 ) ) ;
#41403 = CARTESIAN_POINT ( 'NONE',  ( 5.959828726073459926, -18.96492317065699851, 7.850628836606516003 ) ) ;
#41404 = DIRECTION ( 'NONE',  ( -1.000000000000000000, -0.000000000000000000, -0.000000000000000000 ) ) ;
#41405 = CARTESIAN_POINT ( 'NONE',  ( 4.975801465491695552, 0.000000000000000000, 0.000000000000000000 ) ) ;
#41406 = EDGE_CURVE ( 'NONE', #27511, #58301, #44578, .T. ) ;
#41407 = ORIENTED_EDGE ( 'NONE', *, *, #815, .T. ) ;
#41408 = CARTESIAN_POINT ( 'NONE',  ( 0.6026777506516368677, 44.16847194355625561, -21.46374796741015345 ) ) ;
#41409 =( NAMED_UNIT ( * ) SI_UNIT ( $, .STERADIAN. ) SOLID_ANGLE_UNIT ( ) );
#41410 = EDGE_LOOP ( 'NONE', ( #58425, #53444, #59947, #39951 ) ) ;
#41411 = CARTESIAN_POINT ( 'NONE',  ( 0.8557997880470599172, -23.15977007032294210, -41.93815086860281127 ) ) ;
#41412 = CARTESIAN_POINT ( 'NONE',  ( 0.9730545539215883499, -41.57420493492377744, -10.61654491617608009 ) ) ;
#41413 = CARTESIAN_POINT ( 'NONE',  ( 0.5817216825391117174, 16.42910366609513417, -43.92401968099184018 ) ) ;
#41414 = VERTEX_POINT ( 'NONE', #26064 ) ;
#41415 = EDGE_CURVE ( 'NONE', #27238, #49921, #23697, .T. ) ;
#41416 = CARTESIAN_POINT ( 'NONE',  ( -4.062725214796418349, -12.40828859588279798, -1.199999999999999956 ) ) ;
#41417 = VERTEX_POINT ( 'NONE', #49549 ) ;
#41418 = ORIENTED_EDGE ( 'NONE', *, *, #49649, .T. ) ;
#41419 = CARTESIAN_POINT ( 'NONE',  ( 4.335381028904216727, -21.75407475222698750, -43.89210725562018922 ) ) ;
#41421 = ORIENTED_EDGE ( 'NONE', *, *, #25203, .T. ) ;
#41420 = EDGE_CURVE ( 'NONE', #37050, #9776, #2231, .T. ) ;
#41422 = FACE_OUTER_BOUND ( 'NONE', #6679, .T. ) ;
#41423 = B_SPLINE_CURVE_WITH_KNOTS ( 'NONE', 3,
 ( #13507, #56697, #51078, #42034, #47632, #41721 ),
 .UNSPECIFIED., .F., .F.,
 ( 4, 2, 4 ),
 ( 7.007167689862070887E-18, 0.0002450742804987350435, 0.0004901485609974631482 ),
 .UNSPECIFIED. ) ;
#41424 = AXIS2_PLACEMENT_3D ( 'NONE', #57513, #9942, #34071 ) ;
#41425 = ORIENTED_EDGE ( 'NONE', *, *, #17929, .T. ) ;
#41426 = CARTESIAN_POINT ( 'NONE',  ( 4.975801465491694664, 27.09127437476381317, -39.51822597168466444 ) ) ;
#41427 = CARTESIAN_POINT ( 'NONE',  ( 1.112077966505211624, -0.3630408210682974923, 44.07832263699236108 ) ) ;
#41428 = ORIENTED_EDGE ( 'NONE', *, *, #38994, .T. ) ;
#41429 = CARTESIAN_POINT ( 'NONE',  ( 0.1129192098497455998, 43.40062318508800843, -7.958498283668546947 ) ) ;
#41430 = FACE_OUTER_BOUND ( 'NONE', #36667, .T. ) ;
#41431 = CARTESIAN_POINT ( 'NONE',  ( 1.479689385636123067, -37.80276034141566299, 22.63923929457843087 ) ) ;
#41432 = CARTESIAN_POINT ( 'NONE',  ( 0.7246131072078531021, -41.24126838495085678, -24.75818606403435851 ) ) ;
#41433 = ORIENTED_EDGE ( 'NONE', *, *, #24314, .F. ) ;
#41434 = CARTESIAN_POINT ( 'NONE',  ( 0.5839880159502358614, 44.23273844814462308, 18.37091806000251282 ) ) ;
#41435 = VECTOR ( 'NONE', #47194, 1000.000000000000000 ) ;
#41436 = ORIENTED_EDGE ( 'NONE', *, *, #48926, .T. ) ;
#41437 = CARTESIAN_POINT ( 'NONE',  ( 0.9757892942422815574, -42.90845395884348079, 0.05132855327719211547 ) ) ;
#41438 = ORIENTED_EDGE ( 'NONE', *, *, #30491, .F. ) ;
#41439 = CARTESIAN_POINT ( 'NONE',  ( 0.9752132459055852243, 26.30543738863344672, 33.89922943039187686 ) ) ;
#41440 = EDGE_CURVE ( 'NONE', #25211, #4627, #20439, .T. ) ;
#41442 = CARTESIAN_POINT ( 'NONE',  ( 1.657374760986086271, 14.04758338772360915, -41.75590794387299809 ) ) ;
#41441 = B_SPLINE_CURVE_WITH_KNOTS ( 'NONE', 3,
 ( #60344, #3641, #56584, #23091 ),
 .UNSPECIFIED., .F., .F.,
 ( 4, 4 ),
 ( 5.057544569639794935E-18, 0.004050076154993004218 ),
 .UNSPECIFIED. ) ;
#41443 = VERTEX_POINT ( 'NONE', #1613 ) ;
#41444 = LINE ( 'NONE', #37054, #52575 ) ;
#41445 = CARTESIAN_POINT ( 'NONE',  ( 0.5980894510889448457, 11.77356634613253306, 46.65000524237092350 ) ) ;
#41446 = CARTESIAN_POINT ( 'NONE',  ( 3.661933894777873455, -36.12137754761139519, 30.13100146053178108 ) ) ;
#41447 = LINE ( 'NONE', #61731, #61412 ) ;
#41448 = VERTEX_POINT ( 'NONE', #44895 ) ;
#41449 = EDGE_LOOP ( 'NONE', ( #60774, #37706, #1864, #13455 ) ) ;
#41450 = DIRECTION ( 'NONE',  ( -0.1024043820194934368, 0.7811075516170080668, 0.6159418278945573144 ) ) ;
#41451 = CARTESIAN_POINT ( 'NONE',  ( 5.981074661064941900, 18.96560215432016960, -7.846517100474624584 ) ) ;
#41452 = CARTESIAN_POINT ( 'NONE',  ( 0.9756950546413942771, -16.33093981194350164, 39.67916378221933371 ) ) ;
#41453 = CARTESIAN_POINT ( 'NONE',  ( 0.6023143664670691511, 6.538774821499189649, -47.66103278671584320 ) ) ;
#41454 = CARTESIAN_POINT ( 'NONE',  ( 0.5809828226811617480, 6.791453954331010401, -47.41188724015871969 ) ) ;
#41455 = DIRECTION ( 'NONE',  ( 0.000000000000000000, -0.7071067811865461294, -0.7071067811865487940 ) ) ;
#41456 = CARTESIAN_POINT ( 'NONE',  ( 4.956653778116966613, 0.000000000000000000, 0.000000000000000000 ) ) ;
#41457 = CARTESIAN_POINT ( 'NONE',  ( 0.7948884756798504370, 43.85325300242502067, 22.08145932010500800 ) ) ;
#41458 = CARTESIAN_POINT ( 'NONE',  ( -6.063463321072278589, 13.82218400051372598, 13.40774708649489355 ) ) ;
#41459 = FACE_OUTER_BOUND ( 'NONE', #3297, .T. ) ;
#41460 = CARTESIAN_POINT ( 'NONE',  ( 0.1084644655670284064, -21.21700107124074819, 37.54424727804264705 ) ) ;
#41461 = CONICAL_SURFACE ( 'NONE', #14446, 41.88877248453276536, 0.04450589592585735277 ) ;
#41462 = CARTESIAN_POINT ( 'NONE',  ( 0.6017666602106489515, -34.26316403931537025, -33.76944145963963706 ) ) ;
#41463 = CARTESIAN_POINT ( 'NONE',  ( 0.7245667037590773907, -19.16327388244031837, -44.12005358974296598 ) ) ;
#41464 = DIRECTION ( 'NONE',  ( -1.000000000000000000, -0.000000000000000000, -0.000000000000000000 ) ) ;
#41465 =( BOUNDED_SURFACE ( )  B_SPLINE_SURFACE ( 3, 1, ( 
 ( #55066, #21262 ),
 ( #40393, #59455 ),
 ( #16563, #54754 ),
 ( #12193, #55994 ) ),
 .UNSPECIFIED., .F., .F., .F. ) 
 B_SPLINE_SURFACE_WITH_KNOTS ( ( 4, 4 ),
 ( 2, 2 ),
 ( 0.000000000000000000, 1.000000000000000000 ),
 ( 0.000000000000000000, 1.000000000000000000 ),
 .UNSPECIFIED. ) 
 GEOMETRIC_REPRESENTATION_ITEM ( )  RATIONAL_B_SPLINE_SURFACE ( (
 ( 1.000000000000000000, 1.000000000000000000),
 ( 0.7282232189291694135, 0.9929344683865672927),
 ( 0.7282232189291694135, 0.9929344683865672927),
 ( 1.000000000000000000, 1.000000000000000000) ) ) 
 REPRESENTATION_ITEM ( '' )  SURFACE ( )  );
#41466 = CARTESIAN_POINT ( 'NONE',  ( 0.5786265663353153954, -23.32245830379058660, 41.83999636203313344 ) ) ;
#41467 = VECTOR ( 'NONE', #55106, 1000.000000000000114 ) ;
#41468 = EDGE_CURVE ( 'NONE', #60467, #53953, #42658, .T. ) ;
#41469 = LINE ( 'NONE', #2598, #58273 ) ;
#41470 = CARTESIAN_POINT ( 'NONE',  ( 4.691466044806104740, -24.49380602310839805, 37.25818859570263442 ) ) ;
#41472 = VERTEX_POINT ( 'NONE', #35794 ) ;
#41471 = FACE_OUTER_BOUND ( 'NONE', #38196, .T. ) ;
#41473 = ORIENTED_EDGE ( 'NONE', *, *, #19728, .F. ) ;
#41474 = CARTESIAN_POINT ( 'NONE',  ( 3.727782113643637096, 2.088457279502629493, -43.91373500509456562 ) ) ;
#41475 = CARTESIAN_POINT ( 'NONE',  ( 0.9968887458511638267, 6.251925120322047391, -42.45154664631701280 ) ) ;
#41476 = EDGE_CURVE ( 'NONE', #40143, #8823, #7445, .T. ) ;
#41477 = ORIENTED_EDGE ( 'NONE', *, *, #23563, .T. ) ;
#41478 = ORIENTED_EDGE ( 'NONE', *, *, #44797, .F. ) ;
#41479 = DIRECTION ( 'NONE',  ( 0.1011922191286468292, 0.9739806266819530656, -0.2027852894961811869 ) ) ;
#41480 = AXIS2_PLACEMENT_3D ( 'NONE', #53338, #1028, #19550 ) ;
#41481 = CARTESIAN_POINT ( 'NONE',  ( 4.226256110419178924, 27.07260893061330620, 34.61070781820654929 ) ) ;
#41482 = ORIENTED_EDGE ( 'NONE', *, *, #32514, .F. ) ;
#41483 = ORIENTED_EDGE ( 'NONE', *, *, #49552, .T. ) ;
#41484 = CARTESIAN_POINT ( 'NONE',  ( 4.962356264823609031, -35.98698831890617100, -21.82137185415387037 ) ) ;
#41485 = EDGE_CURVE ( 'NONE', #20243, #19512, #58622, .T. ) ;
#41486 = LINE ( 'NONE', #49938, #21969 ) ;
#41487 = CARTESIAN_POINT ( 'NONE',  ( 0.5987334363312694085, 48.96426925486512971, 3.750099039911617194 ) ) ;
#41488 = VERTEX_POINT ( 'NONE', #30132 ) ;
#41489 = EDGE_CURVE ( 'NONE', #41383, #40152, #6300, .T. ) ;
#41490 = FACE_OUTER_BOUND ( 'NONE', #42332, .T. ) ;
#41491 = CARTESIAN_POINT ( 'NONE',  ( 3.680882792899937250, -47.77138407787919760, -4.423598386734230559 ) ) ;
#41492 = CARTESIAN_POINT ( 'NONE',  ( 0.1098349054025746091, 0.2133124578264728455, -43.12395110775227636 ) ) ;
#41493 = ORIENTED_EDGE ( 'NONE', *, *, #50546, .F. ) ;
#41494 = VERTEX_POINT ( 'NONE', #55172 ) ;
#41495 = FACE_OUTER_BOUND ( 'NONE', #26060, .T. ) ;
#41496 = B_SPLINE_CURVE_WITH_KNOTS ( 'NONE', 3,
 ( #48740, #16165, #58424, #24633, #10227, #15244 ),
 .UNSPECIFIED., .F., .F.,
 ( 4, 2, 4 ),
 ( 1.517598411722886997E-16, 0.0002445252820015207619, 0.0004890505640028898439 ),
 .UNSPECIFIED. ) ;
#41497 = VERTEX_POINT ( 'NONE', #45501 ) ;
#41498 = CARTESIAN_POINT ( 'NONE',  ( 0.5832366564991509073, 44.14509737861672534, -18.58038995918305503 ) ) ;
#41499 = CARTESIAN_POINT ( 'NONE',  ( 1.227938101723756947, 17.20315230597844192, 39.32113113558972373 ) ) ;
#41500 = CARTESIAN_POINT ( 'NONE',  ( 3.238018933889920792, 2.836920992588588764, 13.09043053720782268 ) ) ;
#41501 = CARTESIAN_POINT ( 'NONE',  ( 0.5830082357119545922, -38.81693288260808572, 26.31497209813148785 ) ) ;
#41502 = CARTESIAN_POINT ( 'NONE',  ( 0.8557997880470690211, 41.02602466100812961, -24.73961900479208609 ) ) ;
#41503 = ORIENTED_EDGE ( 'NONE', *, *, #51062, .F. ) ;
#41504 = CARTESIAN_POINT ( 'NONE',  ( -6.077587904424778920, 19.09718056542708453, -2.468545289316033120 ) ) ;
#41505 = CARTESIAN_POINT ( 'NONE',  ( 6.999999999999991118, 80.00000000000001421, -7.414830285890871171E-32 ) ) ;
#41506 = ADVANCED_FACE ( 'NONE', ( #31384 ), #54396, .F. ) ;
#41507 = B_SPLINE_CURVE_WITH_KNOTS ( 'NONE', 3,
 ( #54671, #59999, #11800, #49995 ),
 .UNSPECIFIED., .F., .F.,
 ( 4, 4 ),
 ( 0.000000000000000000, 0.005004948556313800097 ),
 .UNSPECIFIED. ) ;
#41508 = VECTOR ( 'NONE', #31008, 1000.000000000000114 ) ;
#41509 = ORIENTED_EDGE ( 'NONE', *, *, #4494, .T. ) ;
#41510 = CARTESIAN_POINT ( 'NONE',  ( 0.1092355843206037486, 42.79374386763046090, -5.330717085612877604 ) ) ;
#41511 = CARTESIAN_POINT ( 'NONE',  ( 3.270143674763207553, -13.28976595685391082, -3.277085381513258788 ) ) ;
#41512 = CARTESIAN_POINT ( 'NONE',  ( 4.553261556744873317, -36.69060082144796553, 24.15241969627054530 ) ) ;
#41513 = CARTESIAN_POINT ( 'NONE',  ( 0.1064266379913940547, 30.09411261783690605, -30.88821943652580515 ) ) ;
#41514 = B_SPLINE_CURVE_WITH_KNOTS ( 'NONE', 3,
 ( #51940, #42886, #18759, #9030 ),
 .UNSPECIFIED., .F., .F.,
 ( 4, 4 ),
 ( 1.734723475976807094E-18, 0.004050076154993002484 ),
 .UNSPECIFIED. ) ;
#41516 = ORIENTED_EDGE ( 'NONE', *, *, #38552, .F. ) ;
#41515 = CIRCLE ( 'NONE', #38522, 48.09070567114147110 ) ;
#41517 = CARTESIAN_POINT ( 'NONE',  ( 2.624215991343620935, -25.21574086439677487, -40.85210347989558244 ) ) ;
#41518 = CARTESIAN_POINT ( 'NONE',  ( 6.999999999999995559, 54.69470952478017978, -58.44237546506749226 ) ) ;
#41519 = CARTESIAN_POINT ( 'NONE',  ( 0.8760168074887076939, -0.8912768426702952773, -48.09529047980637273 ) ) ;
#41520 = VECTOR ( 'NONE', #38368, 1000.000000000000000 ) ;
#41521 = CARTESIAN_POINT ( 'NONE',  ( 0.6028618097248862329, -41.57478760529421180, 24.20479143424818247 ) ) ;
#41522 = CARTESIAN_POINT ( 'NONE',  ( 0.8760168074886960365, 41.20610493656875661, 24.81951362746092116 ) ) ;
#41523 = CARTESIAN_POINT ( 'NONE',  ( 4.975610109902397937, 20.32389311291233724, -44.49032227207044343 ) ) ;
#41524 = DIRECTION ( 'NONE',  ( -1.000000000000000000, -0.000000000000000000, -0.000000000000000000 ) ) ;
#41525 = CARTESIAN_POINT ( 'NONE',  ( 0.5832366564991503521, 38.16363840618255665, 28.94058080282794876 ) ) ;
#41526 = CARTESIAN_POINT ( 'NONE',  ( 5.896782393890504181, -4.668739246792056541, -19.56345983519980081 ) ) ;
#41527 = ORIENTED_EDGE ( 'NONE', *, *, #32461, .F. ) ;
#41528 = CARTESIAN_POINT ( 'NONE',  ( -17.04253418815309118, -12.35682012055057299, -1.887283050050494015 ) ) ;
#41529 = CARTESIAN_POINT ( 'NONE',  ( 2.281448460670559175, -17.13756432392869300, 44.80776276180765905 ) ) ;
#41530 = CARTESIAN_POINT ( 'NONE',  ( 4.975801465491695552, 0.000000000000000000, 0.000000000000000000 ) ) ;
#41531 = CARTESIAN_POINT ( 'NONE',  ( 4.553261556744873317, 12.28162544311275006, -42.17465165592624032 ) ) ;
#41532 = B_SPLINE_CURVE_WITH_KNOTS ( 'NONE', 3,
 ( #55313, #45643, #22130, #36555, #26202, #35635 ),
 .UNSPECIFIED., .F., .F.,
 ( 4, 2, 4 ),
 ( 7.047314121155778821E-19, 0.0002293801035737096431, 0.0004587602071474185814 ),
 .UNSPECIFIED. ) ;
#41533 = CARTESIAN_POINT ( 'NONE',  ( -6.079354080745853928, 7.795569227099167442, -17.60744318956237464 ) ) ;
#41534 = CARTESIAN_POINT ( 'NONE',  ( 0.8554163680231816613, -46.15020320557298561, -8.447734441620468715 ) ) ;
#41535 = APPLICATION_PROTOCOL_DEFINITION ( 'draft international standard', 'automotive_design', 1998, #4407 ) ;
#41536 = CARTESIAN_POINT ( 'NONE',  ( 0.6017667736363750963, -44.57803721604164338, 18.08696174077311625 ) ) ;
#41537 = B_SPLINE_CURVE_WITH_KNOTS ( 'NONE', 3,
 ( #16505, #58461, #25280, #15587, #44426, #1452 ),
 .UNSPECIFIED., .F., .F.,
 ( 4, 2, 4 ),
 ( 8.833954287279779637E-17, 0.0002293366620881460689, 0.0004586733241762038296 ),
 .UNSPECIFIED. ) ;
#41538 = AXIS2_PLACEMENT_3D ( 'NONE', #40948, #17117, #7686 ) ;
#41539 = CARTESIAN_POINT ( 'NONE',  ( 0.5998501479064708430, 41.92175333043619645, -23.59887241503310307 ) ) ;
#41540 = EDGE_CURVE ( 'NONE', #20535, #49864, #36108, .T. ) ;
#41541 = DIRECTION ( 'NONE',  ( -0.1024043820194934645, 0.9844298967354725427, 0.1428674944016040949 ) ) ;
#41543 = VERTEX_POINT ( 'NONE', #8181 ) ;
#41542 = CARTESIAN_POINT ( 'NONE',  ( 4.303969348037246512, 10.35452842635843673, 46.98258166031693861 ) ) ;
#41544 = ORIENTED_EDGE ( 'NONE', *, *, #8623, .T. ) ;
#41545 = CARTESIAN_POINT ( 'NONE',  ( 4.967162193818130511, 42.34252806656594004, 7.970725651239941811 ) ) ;
#41546 = CARTESIAN_POINT ( 'NONE',  ( 2.624215991343620935, -42.26352390376081303, -22.77108897942180477 ) ) ;
#41547 = LINE ( 'NONE', #45948, #42793 ) ;
#41548 = ADVANCED_FACE ( 'NONE', ( #60793 ), #50392, .F. ) ;
#41549 = ORIENTED_EDGE ( 'NONE', *, *, #59468, .F. ) ;
#41550 = CARTESIAN_POINT ( 'NONE',  ( 0.8744876279028263033, -47.25615711918255357, -13.31186180466976587 ) ) ;
#41551 = CARTESIAN_POINT ( 'NONE',  ( -6.078075953587585900, 3.068021059656498295, 19.01006104736752889 ) ) ;
#41552 = CARTESIAN_POINT ( 'NONE',  ( 0.1097557419366048670, 5.407604117549707823, -42.78407272074152701 ) ) ;
#41553 = EDGE_CURVE ( 'NONE', #15459, #39035, #3470, .T. ) ;
#41554 = ORIENTED_EDGE ( 'NONE', *, *, #60765, .F. ) ;
#41555 = EDGE_LOOP ( 'NONE', ( #27701, #46758, #59200, #29543 ) ) ;
#41556 = CARTESIAN_POINT ( 'NONE',  ( 0.9762797500689124330, 25.26481495167912783, -33.43671500974812716 ) ) ;
#41558 = CARTESIAN_POINT ( 'NONE',  ( 2.359973842542476330, 37.69777570118016996, 22.73793310342894358 ) ) ;
#41557 = CONICAL_SURFACE ( 'NONE', #30512, 42.88844316795388778, 0.04450589592585932341 ) ;
#41559 = CYLINDRICAL_SURFACE ( 'NONE', #47933, 2.649999999999992806 ) ;
#41560 = ADVANCED_FACE ( 'NONE', ( #40817 ), #60809, .F. ) ;
#41561 = CARTESIAN_POINT ( 'NONE',  ( 3.407937589446178528, -5.663729899984980776, -12.47329436636634981 ) ) ;
#41562 = CARTESIAN_POINT ( 'NONE',  ( 0.6029443449137436017, 49.00372439284071646, 3.189754475479290363 ) ) ;
#41563 = CARTESIAN_POINT ( 'NONE',  ( -6.078726893082806448, -11.01948708261720178, -15.79129335123480971 ) ) ;
#41564 = CARTESIAN_POINT ( 'NONE',  ( 0.1155031312995260795, 33.48869165808871173, 28.73063110273194454 ) ) ;
#41565 = ORIENTED_EDGE ( 'NONE', *, *, #9528, .T. ) ;
#41566 = CARTESIAN_POINT ( 'NONE',  ( 0.8744876279028306332, 21.91587810745098963, -43.93226988397984911 ) ) ;
#41567 = CARTESIAN_POINT ( 'NONE',  ( 5.960221823109900008, 20.35070456576731246, 2.673723662181406002 ) ) ;
#41568 = ORIENTED_EDGE ( 'NONE', *, *, #21557, .F. ) ;
#41569 = CARTESIAN_POINT ( 'NONE',  ( 0.6030672727741701600, -47.68443224372866496, -6.365785297724608327 ) ) ;
#41570 = CARTESIAN_POINT ( 'NONE',  ( 5.838029081930955932, 19.90064824094183749, -42.83724148148685629 ) ) ;
#41571 = CARTESIAN_POINT ( 'NONE',  ( 1.657374760986086493, 39.13992893817287211, -20.22267069323491029 ) ) ;
#41572 = CARTESIAN_POINT ( 'NONE',  ( 0.7948884756798516582, 23.47568016441766758, -43.12297630519164215 ) ) ;
#41573 = ORIENTED_EDGE ( 'NONE', *, *, #48810, .F. ) ;
#41574 = VERTEX_POINT ( 'NONE', #26366 ) ;
#41575 = CARTESIAN_POINT ( 'NONE',  ( 4.963659409799331179, -24.46566636552851293, 37.47512675766687806 ) ) ;
#41576 = CARTESIAN_POINT ( 'NONE',  ( 2.301430502907644726, -38.87758534782525999, 28.20897229937338224 ) ) ;
#41577 = VERTEX_POINT ( 'NONE', #36412 ) ;
#41578 = CARTESIAN_POINT ( 'NONE',  ( 0.6039202388192953519, 17.12343321804663177, 46.02555537607436520 ) ) ;
#41579 =( BOUNDED_SURFACE ( )  B_SPLINE_SURFACE ( 3, 1, ( 
 ( #17402, #21796 ),
 ( #7356, #26482 ),
 ( #40313, #7047 ),
 ( #2980, #41534 ) ),
 .UNSPECIFIED., .F., .F., .F. ) 
 B_SPLINE_SURFACE_WITH_KNOTS ( ( 4, 4 ),
 ( 2, 2 ),
 ( 0.000000000000000000, 1.000000000000000000 ),
 ( 0.000000000000000000, 1.000000000000000000 ),
 .UNSPECIFIED. ) 
 GEOMETRIC_REPRESENTATION_ITEM ( )  RATIONAL_B_SPLINE_SURFACE ( (
 ( 1.000000000000000000, 1.000000000000000000),
 ( 0.7282232189291693025, 0.9929344683865674037),
 ( 0.7282232189291693025, 0.9929344683865674037),
 ( 1.000000000000000000, 1.000000000000000000) ) ) 
 REPRESENTATION_ITEM ( '' )  SURFACE ( )  );
#41580 = ORIENTED_EDGE ( 'NONE', *, *, #33779, .T. ) ;
#41581 = CARTESIAN_POINT ( 'NONE',  ( 0.6001305935487422083, -18.89378601236034427, -44.24520387813821287 ) ) ;
#41582 = VERTEX_POINT ( 'NONE', #55479 ) ;
#41583 = CARTESIAN_POINT ( 'NONE',  ( 4.060580049360325461, 43.52047761765033584, 6.118473853078531199 ) ) ;
#41584 = CARTESIAN_POINT ( 'NONE',  ( 0.9789233960466692253, 24.75338403626521355, 33.81725455422888871 ) ) ;
#41585 = CARTESIAN_POINT ( 'NONE',  ( -4.214292481396491930, -11.25702090725073035, 0.000000000000000000 ) ) ;
#41586 = ORIENTED_EDGE ( 'NONE', *, *, #56427, .T. ) ;
#41587 = CARTESIAN_POINT ( 'NONE',  ( 0.1155031312995260795, -27.37902390932426755, -34.60246641938199019 ) ) ;
#41588 = EDGE_CURVE ( 'NONE', #46515, #33349, #20248, .T. ) ;
#41589 = CARTESIAN_POINT ( 'NONE',  ( 5.981074661064941900, -20.52466374824937034, 0.008585178657547546527 ) ) ;
#41590 = CARTESIAN_POINT ( 'NONE',  ( 1.157644175074339365, 29.72797329618415318, -29.55080166730750335 ) ) ;
#41591 = EDGE_CURVE ( 'NONE', #20061, #19329, #16457, .T. ) ;
#41592 = ORIENTED_EDGE ( 'NONE', *, *, #58612, .T. ) ;
#41593 = DIRECTION ( 'NONE',  ( 0.000000000000000000, -0.5000000000000009992, -0.8660254037844380415 ) ) ;
#41594 = CARTESIAN_POINT ( 'NONE',  ( 4.958415959904820092, 7.056061540672502908, 44.87110372340845288 ) ) ;
#41595 = CARTESIAN_POINT ( 'NONE',  ( 3.680882792899939471, 42.44216617524785562, 22.36818923730784903 ) ) ;
#41596 = CARTESIAN_POINT ( 'NONE',  ( 0.3676999524040366896, 41.59822836379080968, -14.68121181363270367 ) ) ;
#41597 = ORIENTED_EDGE ( 'NONE', *, *, #51852, .T. ) ;
#41598 = EDGE_CURVE ( 'NONE', #45197, #23651, #8479, .T. ) ;
#41599 = CARTESIAN_POINT ( 'NONE',  ( 0.1098349054025746507, 37.45309339978484076, -21.37724154645462704 ) ) ;
#41600 = CARTESIAN_POINT ( 'NONE',  ( -6.015611763856276717, 18.68284711750061788, -2.453375430803879986 ) ) ;
#41601 = ORIENTED_EDGE ( 'NONE', *, *, #46559, .T. ) ;
#41602 = AXIS2_PLACEMENT_3D ( 'NONE', #2621, #51461, #45886 ) ;
#41603 = CARTESIAN_POINT ( 'NONE',  ( 0.5980271706414734822, -43.13192993667226460, -23.48799401353080540 ) ) ;
#41604 = CARTESIAN_POINT ( 'NONE',  ( -6.057079549204054558, -18.27862279149374203, 6.059965341982067599 ) ) ;
#41605 = CARTESIAN_POINT ( 'NONE',  ( 0.6016118706126977189, 44.09211895607887755, 21.62027059837412679 ) ) ;
#41606 = VECTOR ( 'NONE', #12013, 1000.000000000000000 ) ;
#41607 = CARTESIAN_POINT ( 'NONE',  ( 0.9730545539215883499, 6.101350888305258735, -42.47233286818610054 ) ) ;
#41608 = CARTESIAN_POINT ( 'NONE',  ( -6.016104459813371719, 18.68131780085935034, -2.464823636987256261 ) ) ;
#41609 = CARTESIAN_POINT ( 'NONE',  ( 0.8557997880470606944, -19.17299735372040459, 43.90420959842174398 ) ) ;
#41610 = PLANE ( 'NONE',  #12633 ) ;
#41611 = CARTESIAN_POINT ( 'NONE',  ( 0.1158516988532803521, -12.60172690908452076, -42.28638832699774497 ) ) ;
#41612 = CARTESIAN_POINT ( 'NONE',  ( -6.016761891674565099, -18.84319130225482297, -0.003433883959981760738 ) ) ;
#41613 = CARTESIAN_POINT ( 'NONE',  ( -6.079354080745853928, 13.83171223607736167, 13.39689112691858419 ) ) ;
#41614 = EDGE_CURVE ( 'NONE', #15708, #50474, #28430, .T. ) ;
#41615 = DIRECTION ( 'NONE',  ( 0.07836865515943411409, 0.3887811538706197889, -0.9179910502197345945 ) ) ;
#41616 = CARTESIAN_POINT ( 'NONE',  ( -5.995132425357893702, -17.40647075750121431, 7.219211173946431082 ) ) ;
#41617 = CARTESIAN_POINT ( 'NONE',  ( -6.203732170862584994, -1.182048853166489222, 5.744326400484686099E-14 ) ) ;
#41618 = CARTESIAN_POINT ( 'NONE',  ( 5.960221823109900008, 18.96108896995703930, 7.859839668735279616 ) ) ;
#41619 = FACE_OUTER_BOUND ( 'NONE', #47696, .T. ) ;
#41620 = CARTESIAN_POINT ( 'NONE',  ( 0.7762777257811898091, 37.45705273431007498, 29.86325207275890747 ) ) ;
#41621 = CARTESIAN_POINT ( 'NONE',  ( 0.5806925824938490299, 46.40146083665128174, 6.791670970260652140 ) ) ;
#41622 = CARTESIAN_POINT ( 'NONE',  ( 2.359973842542475442, 32.52418265237010786, -29.67007646481159711 ) ) ;
#41623 = EDGE_CURVE ( 'NONE', #21629, #45591, #14264, .T. ) ;
#41624 = ORIENTED_EDGE ( 'NONE', *, *, #20400, .F. ) ;
#41625 = CARTESIAN_POINT ( 'NONE',  ( 0.3676999524040323597, 39.37931578712994707, 19.88014264185084912 ) ) ;
#41626 = B_SPLINE_CURVE_WITH_KNOTS ( 'NONE', 3,
 ( #28624, #33356, #14249, #4799, #46840, #4183, #23939, #47142, #103, #8585, #57116, #56816, #4489, #38069, #52736, #43063, #13316, #41835, #37439 ),
 .UNSPECIFIED., .F., .F.,
 ( 4, 3, 3, 3, 3, 3, 4 ),
 ( 3.469446951953614189E-18, 0.0002724573126191750507, 0.0004086839781548493988, 0.0005449106435901834378, 0.0006811373090491472295, 0.0008459866663933670976, 0.001010840725717212715 ),
 .UNSPECIFIED. ) ;
#41627 = CARTESIAN_POINT ( 'NONE',  ( 3.221118495291108719, -32.88209193446716938, -29.21522633277039560 ) ) ;
#41628 = CARTESIAN_POINT ( 'NONE',  ( 3.727782113643637540, 27.93898545223054697, -33.94393712883089620 ) ) ;
#41629 = CARTESIAN_POINT ( 'NONE',  ( 0.6008122571543325074, -45.68025335892497907, -18.02412282275449584 ) ) ;
#41630 = VERTEX_POINT ( 'NONE', #57938 ) ;
#41631 = CARTESIAN_POINT ( 'NONE',  ( 4.967162193818129623, -43.02067033766018511, 2.375726030842427061 ) ) ;
#41633 = EDGE_CURVE ( 'NONE', #21594, #24966, #30744, .T. ) ;
#41632 = B_SPLINE_CURVE_WITH_KNOTS ( 'NONE', 3,
 ( #59077, #54062, #1439, #49380 ),
 .UNSPECIFIED., .F., .F.,
 ( 4, 4 ),
 ( 3.878959614448864246E-18, 0.004050076154992999014 ),
 .UNSPECIFIED. ) ;
#41634 =( BOUNDED_SURFACE ( )  B_SPLINE_SURFACE ( 3, 1, ( 
 ( #16916, #45124 ),
 ( #35721, #59484 ),
 ( #46050, #11275 ),
 ( #59174, #54463 ) ),
 .UNSPECIFIED., .F., .F., .F. ) 
 B_SPLINE_SURFACE_WITH_KNOTS ( ( 4, 4 ),
 ( 2, 2 ),
 ( 0.000000000000000000, 1.000000000000000000 ),
 ( 0.000000000000000000, 1.000000000000000000 ),
 .UNSPECIFIED. ) 
 GEOMETRIC_REPRESENTATION_ITEM ( )  RATIONAL_B_SPLINE_SURFACE ( (
 ( 1.000000000000000000, 1.000000000000000000),
 ( 0.7269869731126821222, 0.9931720237060910339),
 ( 0.7269869731126821222, 0.9931720237060910339),
 ( 1.000000000000000000, 1.000000000000000000) ) ) 
 REPRESENTATION_ITEM ( '' )  SURFACE ( )  );
#41635 = CARTESIAN_POINT ( 'NONE',  ( 4.967162193818130511, -28.07411493385318124, 32.68434214048159703 ) ) ;
#41636 = ORIENTED_EDGE ( 'NONE', *, *, #6746, .F. ) ;
#41637 = CARTESIAN_POINT ( 'NONE',  ( 4.226256110419179812, -25.47726887332619583, 35.80134104671822115 ) ) ;
#41638 = ORIENTED_EDGE ( 'NONE', *, *, #48931, .T. ) ;
#41639 = CARTESIAN_POINT ( 'NONE',  ( -6.063463321072276813, 12.01854346922034722, 15.04576569530214059 ) ) ;
#41640 = CARTESIAN_POINT ( 'NONE',  ( -6.016104459813374383, 18.19977249352310267, 4.882138007282813774 ) ) ;
#41641 = VERTEX_POINT ( 'NONE', #52632 ) ;
#41642 = CARTESIAN_POINT ( 'NONE',  ( 4.062725214796417461, -12.40828859588279798, -1.199999999999999956 ) ) ;
#41643 = CARTESIAN_POINT ( 'NONE',  ( 0.1092565886968783900, 26.49813811968539312, 34.02318727879972471 ) ) ;
#41644 = EDGE_LOOP ( 'NONE', ( #37700, #41276, #1145, #58333 ) ) ;
#41645 = CARTESIAN_POINT ( 'NONE',  ( 0.5806925824938499181, -7.260877859416734026, -46.33035738103254175 ) ) ;
#41646 = CARTESIAN_POINT ( 'NONE',  ( 0.1087620492084205720, -25.96440931622107229, -34.43219573047424120 ) ) ;
#41647 = B_SPLINE_CURVE_WITH_KNOTS ( 'NONE', 3,
 ( #14935, #5486, #24625, #808 ),
 .UNSPECIFIED., .F., .F.,
 ( 4, 4 ),
 ( 5.553824967135426632E-18, 0.004566006591234645501 ),
 .UNSPECIFIED. ) ;
#41648 = ORIENTED_EDGE ( 'NONE', *, *, #2163, .F. ) ;
#41649 = CARTESIAN_POINT ( 'NONE',  ( -5.999999999999999112, -15.71999999999999353, 1.942289823447701879E-15 ) ) ;
#41650 = ORIENTED_EDGE ( 'NONE', *, *, #27341, .F. ) ;
#41651 = CARTESIAN_POINT ( 'NONE',  ( -5.995132425357893702, -0.008513469642939168122, 18.84415457712583475 ) ) ;
#41652 =( BOUNDED_SURFACE ( )  B_SPLINE_SURFACE ( 3, 1, ( 
 ( #2819, #41691 ),
 ( #21952, #60146 ),
 ( #17255, #36376 ),
 ( #22260, #7834 ) ),
 .UNSPECIFIED., .F., .F., .F. ) 
 B_SPLINE_SURFACE_WITH_KNOTS ( ( 4, 4 ),
 ( 2, 2 ),
 ( 0.000000000000000000, 1.000000000000000000 ),
 ( 0.000000000000000000, 1.000000000000000000 ),
 .UNSPECIFIED. ) 
 GEOMETRIC_REPRESENTATION_ITEM ( )  RATIONAL_B_SPLINE_SURFACE ( (
 ( 1.000000000000000000, 1.000000000000000000),
 ( 0.9952954269826590483, 0.8620686068821307169),
 ( 0.9952954269826590483, 0.8620686068821307169),
 ( 1.000000000000000000, 1.000000000000000000) ) ) 
 REPRESENTATION_ITEM ( '' )  SURFACE ( )  );
#41653 = ORIENTED_EDGE ( 'NONE', *, *, #52076, .T. ) ;
#41654 = VERTEX_POINT ( 'NONE', #38886 ) ;
#41655 = CARTESIAN_POINT ( 'NONE',  ( 4.956445790443989807, 44.30493387627029733, 15.95653108789479191 ) ) ;
#41657 = AXIS2_PLACEMENT_3D ( 'NONE', #32834, #51913, #51287 ) ;
#41656 = CARTESIAN_POINT ( 'NONE',  ( 0.5998501479064699549, -11.94461217097501837, 46.60114184914296942 ) ) ;
#41658 = CARTESIAN_POINT ( 'NONE',  ( 2.282803330402959574, 39.73060135428402617, 25.05945377465257451 ) ) ;
#41659 = CARTESIAN_POINT ( 'NONE',  ( 0.1084644655670282676, -16.13497904887329426, 39.99242539812087216 ) ) ;
#41660 = FACE_OUTER_BOUND ( 'NONE', #26807, .T. ) ;
#41661 = ORIENTED_EDGE ( 'NONE', *, *, #11978, .T. ) ;
#41662 = CARTESIAN_POINT ( 'NONE',  ( 4.226256110419178924, 6.604788716987348707, 43.44196146574351758 ) ) ;
#41663 = EDGE_CURVE ( 'NONE', #27614, #16034, #48263, .T. ) ;
#41664 = DIRECTION ( 'NONE',  ( 0.000000000000000000, 0.000000000000000000, 1.000000000000000000 ) ) ;
#41665 = CARTESIAN_POINT ( 'NONE',  ( 4.967162193818130511, 3.259922920618364639, -42.96271701169381885 ) ) ;
#41666 = B_SPLINE_CURVE_WITH_KNOTS ( 'NONE', 3,
 ( #20994, #34485, #58561, #15691, #40141, #6864 ),
 .UNSPECIFIED., .F., .F.,
 ( 4, 2, 4 ),
 ( 1.246832498358330099E-18, 0.0002293801035737093178, 0.0004587602071474173888 ),
 .UNSPECIFIED. ) ;
#41667 = VERTEX_POINT ( 'NONE', #38571 ) ;
#41668 = ADVANCED_FACE ( 'NONE', ( #4078 ), #14485, .F. ) ;
#41669 = ORIENTED_EDGE ( 'NONE', *, *, #52039, .F. ) ;
#41670 = CARTESIAN_POINT ( 'NONE',  ( 0.9730545539215883499, 34.34678117142591702, -25.71816799638743944 ) ) ;
#41671 = CARTESIAN_POINT ( 'NONE',  ( 2.299746137290199943, 5.989104756252149997, 48.66633294079981198 ) ) ;
#41672 = CARTESIAN_POINT ( 'NONE',  ( 0.1064266379913943877, -42.67882137217595329, 6.185137063632299537 ) ) ;
#41673 = ORIENTED_EDGE ( 'NONE', *, *, #51541, .T. ) ;
#41674 = CARTESIAN_POINT ( 'NONE',  ( 30.00000000000001421, -15.99999999999999289, 1.959434878635763159E-15 ) ) ;
#41675 = CARTESIAN_POINT ( 'NONE',  ( 5.895596859100789899, -2.009647457886758914, -20.01223376606161963 ) ) ;
#41676 = ADVANCED_FACE ( 'NONE', ( #52320 ), #42764, .T. ) ;
#41677 = ADVANCED_FACE ( 'NONE', ( #29145 ), #57147, .F. ) ;
#41678 = B_SPLINE_CURVE_WITH_KNOTS ( 'NONE', 3,
 ( #28103, #8674, #42534, #47222 ),
 .UNSPECIFIED., .F., .F.,
 ( 4, 4 ),
 ( 2.964296775167216948E-17, 0.005004741218457446628 ),
 .UNSPECIFIED. ) ;
#41679 = ORIENTED_EDGE ( 'NONE', *, *, #43275, .T. ) ;
#41680 = CARTESIAN_POINT ( 'NONE',  ( 0.5819845079324650339, 47.54334065046006685, 5.801222053075247409 ) ) ;
#41681 = EDGE_CURVE ( 'NONE', #21596, #23436, #57623, .T. ) ;
#41682 = B_SPLINE_CURVE_WITH_KNOTS ( 'NONE', 3,
 ( #483, #48727, #38745, #29312, #1400, #49340, #14933, #20847, #48421, #6393, #29010, #39986, #53414, #25229, #48124, #5177, #34339, #57800, #34040 ),
 .UNSPECIFIED., .F., .F.,
 ( 4, 3, 3, 3, 3, 3, 4 ),
 ( 1.734776414728241573E-18, 0.0002612768053151712754, 0.0003919133833142901665, 0.0005225499612322610787, 0.0006531865391693348743, 0.0008112755173415197489, 0.0009693688056799721394 ),
 .UNSPECIFIED. ) ;
#41683 = CARTESIAN_POINT ( 'NONE',  ( 1.092182651088186462, -16.93161368780761578, 38.34164370979851100 ) ) ;
#41684 = CARTESIAN_POINT ( 'NONE',  ( 0.9756950546413952763, -33.98259063592739437, 26.19769393035354810 ) ) ;
#41685 = CARTESIAN_POINT ( 'NONE',  ( 0.5824936645240087474, -41.69005659875550407, -21.47504039187983693 ) ) ;
#41686 = CARTESIAN_POINT ( 'NONE',  ( 1.155036213957052500E-14, 4.618802153517020059, -5.599999999999999645 ) ) ;
#41687 = FILL_AREA_STYLE_COLOUR ( '', #59718 ) ;
#41688 = DIRECTION ( 'NONE',  ( 0.000000000000000000, -1.000000000000000000, 0.000000000000000000 ) ) ;
#41689 = EDGE_CURVE ( 'NONE', #5387, #54885, #58259, .T. ) ;
#41690 = VERTEX_POINT ( 'NONE', #42645 ) ;
#41691 = CARTESIAN_POINT ( 'NONE',  ( 0.8554163680231720024, -44.01281378489805007, 16.25046755781837504 ) ) ;
#41692 = CARTESIAN_POINT ( 'NONE',  ( 0.5797568599927140909, 28.32170417884941926, -37.37788625747514715 ) ) ;
#41693 = VECTOR ( 'NONE', #26464, 1000.000000000000114 ) ;
#41694 = EDGE_CURVE ( 'NONE', #54562, #4022, #52013, .T. ) ;
#41695 = DIRECTION ( 'NONE',  ( 0.000000000000000000, 0.000000000000000000, 1.000000000000000000 ) ) ;
#41696 = CARTESIAN_POINT ( 'NONE',  ( 4.999999999999996447, 2.650000000000838352, -79.99999999999998579 ) ) ;
#41697 = CIRCLE ( 'NONE', #45670, 8.000000000000000000 ) ;
#41698 = CARTESIAN_POINT ( 'NONE',  ( 0.9789889208857700531, 29.20362932482186480, 30.05799281889552788 ) ) ;
#41699 = CARTESIAN_POINT ( 'NONE',  ( 0.2285344041767085055, 43.15390724259560074, -9.178314659724513547 ) ) ;
#41700 = CARTESIAN_POINT ( 'NONE',  ( 0.5997462898726536595, -49.10477184366966696, -0.5225058138009923692 ) ) ;
#41701 = B_SPLINE_CURVE_WITH_KNOTS ( 'NONE', 3,
 ( #43153, #39379, #5807, #57503 ),
 .UNSPECIFIED., .F., .F.,
 ( 4, 4 ),
 ( 0.000000000000000000, 0.005013413432710150247 ),
 .UNSPECIFIED. ) ;
#41702 = CARTESIAN_POINT ( 'NONE',  ( 3.376099380956842921, 3.553490516825148049, 12.92598502161057006 ) ) ;
#41703 = B_SPLINE_CURVE_WITH_KNOTS ( 'NONE', 3,
 ( #16647, #55759, #41100, #35769 ),
 .UNSPECIFIED., .F., .F.,
 ( 4, 4 ),
 ( 7.152448122690996019E-18, 0.005004948556313816577 ),
 .UNSPECIFIED. ) ;
#41704 = CARTESIAN_POINT ( 'NONE',  ( 0.8554163680231738898, 31.95314001164559770, 34.35407277904604229 ) ) ;
#41705 = CARTESIAN_POINT ( 'NONE',  ( 0.5838002273316426072, -29.04904228829587254, -38.08117724016836547 ) ) ;
#41706 = AXIS2_PLACEMENT_3D ( 'NONE', #30038, #42933, #43868 ) ;
#41707 = ORIENTED_EDGE ( 'NONE', *, *, #40170, .T. ) ;
#41708 = CARTESIAN_POINT ( 'NONE',  ( -6.057079549204054558, 19.25697688790420159, -0.008499321259853864774 ) ) ;
#41709 = CARTESIAN_POINT ( 'NONE',  ( 5.958863334805807099, 17.77634700750914476, 10.26176968287951397 ) ) ;
#41710 = CARTESIAN_POINT ( 'NONE',  ( 2.301529144917016989, 38.87759814529778879, 28.20894756932154834 ) ) ;
#41711 = CARTESIAN_POINT ( 'NONE',  ( 2.500000000000000000, 1.178949249685217415, 2.041999999999998483 ) ) ;
#41712 = ORIENTED_EDGE ( 'NONE', *, *, #6711, .F. ) ;
#41713 = CARTESIAN_POINT ( 'NONE',  ( 4.975801465491695552, 47.10002938642130488, 8.787181743660319455 ) ) ;
#41714 = CARTESIAN_POINT ( 'NONE',  ( 0.8557997880470697982, -19.17299735371977221, -43.90420959842202109 ) ) ;
#41715 = EDGE_CURVE ( 'NONE', #2075, #44883, #19466, .T. ) ;
#41716 = VECTOR ( 'NONE', #52595, 1000.000000000000114 ) ;
#41717 = EDGE_LOOP ( 'NONE', ( #15143, #14913, #32221, #42637 ) ) ;
#41718 = CARTESIAN_POINT ( 'NONE',  ( 4.962356264823603702, -4.645793755590432283, -41.82884409403234116 ) ) ;
#41719 = EDGE_CURVE ( 'NONE', #58860, #11856, #44122, .T. ) ;
#41720 = CARTESIAN_POINT ( 'NONE',  ( 4.967162193818132288, -24.30453456948087521, -35.57684288742000689 ) ) ;
#41721 = CARTESIAN_POINT ( 'NONE',  ( 0.8751705887134553219, 24.81530984069150136, 41.19904111682516401 ) ) ;
#41722 = ORIENTED_EDGE ( 'NONE', *, *, #46027, .F. ) ;
#41723 = CARTESIAN_POINT ( 'NONE',  ( 0.3622758884714730732, 39.50828911766998175, -17.25816669464953534 ) ) ;
#41724 = VERTEX_POINT ( 'NONE', #33558 ) ;
#41725 = ORIENTED_EDGE ( 'NONE', *, *, #7489, .T. ) ;
#41726 = CARTESIAN_POINT ( 'NONE',  ( 0.3622758884714730732, -42.84426538328728640, -4.808133778521729518 ) ) ;
#41727 = ORIENTED_EDGE ( 'NONE', *, *, #24008, .F. ) ;
#41728 = CARTESIAN_POINT ( 'NONE',  ( 0.7048096507298635682, -13.26491767067483707, -46.24547838151364942 ) ) ;
#41729 = VERTEX_POINT ( 'NONE', #43274 ) ;
#41730 = CARTESIAN_POINT ( 'NONE',  ( 3.598860563414087554, 0.2887493804703922251, 48.97398519332762845 ) ) ;
#41731 = CARTESIAN_POINT ( 'NONE',  ( 0.9730545539215883499, 16.88610103448558064, 39.44597740938066721 ) ) ;
#41732 = AXIS2_PLACEMENT_3D ( 'NONE', #57191, #33433, #23401 ) ;
#41733 =( BOUNDED_SURFACE ( )  B_SPLINE_SURFACE ( 3, 1, ( 
 ( #15725, #34831 ),
 ( #35766, #1584 ),
 ( #40468, #53897 ),
 ( #59218, #7520 ) ),
 .UNSPECIFIED., .F., .F., .F. ) 
 B_SPLINE_SURFACE_WITH_KNOTS ( ( 4, 4 ),
 ( 2, 2 ),
 ( 0.000000000000000000, 1.000000000000000000 ),
 ( 0.000000000000000000, 1.000000000000000000 ),
 .UNSPECIFIED. ) 
 GEOMETRIC_REPRESENTATION_ITEM ( )  RATIONAL_B_SPLINE_SURFACE ( (
 ( 1.000000000000000000, 1.000000000000000000),
 ( 0.9953390228620291325, 0.8624445117760984880),
 ( 0.9953390228620291325, 0.8624445117760984880),
 ( 1.000000000000000000, 1.000000000000000000) ) ) 
 REPRESENTATION_ITEM ( '' )  SURFACE ( )  );
#41734 = EDGE_LOOP ( 'NONE', ( #38626, #3910, #37584, #466 ) ) ;
#41735 = CARTESIAN_POINT ( 'NONE',  ( 0.1157991065609915854, 15.16251859759399778, 41.43718614137927858 ) ) ;
#41736 =( GEOMETRIC_REPRESENTATION_CONTEXT ( 3 ) GLOBAL_UNCERTAINTY_ASSIGNED_CONTEXT ( ( #8541 ) ) GLOBAL_UNIT_ASSIGNED_CONTEXT ( ( #57006, #13197, #3453 ) ) REPRESENTATION_CONTEXT ( 'NONE', 'WORKASPACE' ) );
#41737 = CARTESIAN_POINT ( 'NONE',  ( 0.8744876279028263033, 28.81338721758142896, -39.75095932715596092 ) ) ;
#41738 = CARTESIAN_POINT ( 'NONE',  ( 0.5824936645240096356, -44.18041932528780080, -15.72668837619807825 ) ) ;
#41739 = VECTOR ( 'NONE', #4454, 1000.000000000000000 ) ;
#41740 = CARTESIAN_POINT ( 'NONE',  ( -2.708315649062916552, 13.61924161399626421, 5.356004933109508315 ) ) ;
#41741 = ORIENTED_EDGE ( 'NONE', *, *, #26409, .F. ) ;
#41742 = DIRECTION ( 'NONE',  ( -0.07500201931887529039, -0.6334382584229031332, 0.7701497710603116831 ) ) ;
#41743 = EDGE_LOOP ( 'NONE', ( #57689, #46099, #55978, #18815 ) ) ;
#41744 = DIRECTION ( 'NONE',  ( -1.000000000000000000, -0.000000000000000000, -0.000000000000000000 ) ) ;
#41745 = ADVANCED_FACE ( 'NONE', ( #20075 ), #14016, .F. ) ;
#41746 = ORIENTED_EDGE ( 'NONE', *, *, #26678, .T. ) ;
#41747 = DIRECTION ( 'NONE',  ( -1.000000000000000000, -0.000000000000000000, -0.000000000000000000 ) ) ;
#41748 = CARTESIAN_POINT ( 'NONE',  ( 0.3622758884714600280, -41.42293301073617329, -11.95365414648482627 ) ) ;
#41749 = EDGE_LOOP ( 'NONE', ( #2936, #35734, #36342, #48280 ) ) ;
#41750 = CARTESIAN_POINT ( 'NONE',  ( 43.00000000000000000, 2.549224068967256441E-30, 75.00000000000001421 ) ) ;
#41751 = DIRECTION ( 'NONE',  ( -1.850371707708593823E-16, 1.000000000000000000, 0.000000000000000000 ) ) ;
#41752 = CARTESIAN_POINT ( 'NONE',  ( -6.079354080745853928, -18.90111140843025694, -3.679802002047057652 ) ) ;
#41753 = CARTESIAN_POINT ( 'NONE',  ( -6.078726893082806448, -18.27395335922926378, 6.070969436048390122 ) ) ;
#41754 = VECTOR ( 'NONE', #52683, 1000.000000000000114 ) ;
#41755 = EDGE_CURVE ( 'NONE', #21932, #51356, #54160, .T. ) ;
#41756 =( BOUNDED_SURFACE ( )  B_SPLINE_SURFACE ( 3, 1, ( 
 ( #23717, #9298 ),
 ( #19038, #52515 ),
 ( #27483, #46613 ),
 ( #38152, #46931 ) ),
 .UNSPECIFIED., .F., .F., .F. ) 
 B_SPLINE_SURFACE_WITH_KNOTS ( ( 4, 4 ),
 ( 2, 2 ),
 ( 0.000000000000000000, 1.000000000000000000 ),
 ( 0.000000000000000000, 1.000000000000000000 ),
 .UNSPECIFIED. ) 
 GEOMETRIC_REPRESENTATION_ITEM ( )  RATIONAL_B_SPLINE_SURFACE ( (
 ( 1.000000000000000000, 1.000000000000000000),
 ( 0.7282232189291694135, 0.9929344683865672927),
 ( 0.7282232189291694135, 0.9929344683865672927),
 ( 1.000000000000000000, 1.000000000000000000) ) ) 
 REPRESENTATION_ITEM ( '' )  SURFACE ( )  );
#41757 = ORIENTED_EDGE ( 'NONE', *, *, #21299, .F. ) ;
#41758 = DIRECTION ( 'NONE',  ( 1.000000000000000000, 0.000000000000000000, 0.000000000000000000 ) ) ;
#41759 = EDGE_CURVE ( 'NONE', #19838, #10899, #32741, .T. ) ;
#41760 = CARTESIAN_POINT ( 'NONE',  ( 5.960721111146673579, -16.28018152803684515, -12.50019045452732591 ) ) ;
#41761 =( BOUNDED_SURFACE ( )  B_SPLINE_SURFACE ( 3, 1, ( 
 ( #58022, #34870 ),
 ( #14839, #53027 ),
 ( #20451, #10128 ),
 ( #39581, #29842 ) ),
 .UNSPECIFIED., .F., .F., .F. ) 
 B_SPLINE_SURFACE_WITH_KNOTS ( ( 4, 4 ),
 ( 2, 2 ),
 ( 0.000000000000000000, 1.000000000000000000 ),
 ( 0.000000000000000000, 1.000000000000000000 ),
 .UNSPECIFIED. ) 
 GEOMETRIC_REPRESENTATION_ITEM ( )  RATIONAL_B_SPLINE_SURFACE ( (
 ( 1.000000000000000000, 1.000000000000000000),
 ( 0.9754377213608244057, 0.9999580625633939235),
 ( 0.9754377213608244057, 0.9999580625633939235),
 ( 1.000000000000000000, 1.000000000000000000) ) ) 
 REPRESENTATION_ITEM ( '' )  SURFACE ( )  );
#41762 = FACE_OUTER_BOUND ( 'NONE', #3283, .T. ) ;
#41763 = CARTESIAN_POINT ( 'NONE',  ( 0.3676999524040366896, -18.60775935196311082, -39.99627326667158655 ) ) ;
#41764 = VECTOR ( 'NONE', #46678, 1000.000000000000227 ) ;
#41765 = DIRECTION ( 'NONE',  ( -1.000000000000000000, 0.000000000000000000, 0.000000000000000000 ) ) ;
#41766 = DIRECTION ( 'NONE',  ( -1.836909530733573776E-16, 1.000000000000000000, 0.000000000000000000 ) ) ;
#41767 = CARTESIAN_POINT ( 'NONE',  ( 0.5817216825391114954, 4.240840028299648345, -46.70385667224744708 ) ) ;
#41768 = DIRECTION ( 'NONE',  ( 0.000000000000000000, -0.7071067811865487940, 0.7071067811865461294 ) ) ;
#41769 = CARTESIAN_POINT ( 'NONE',  ( 0.7044674535452954967, 48.94804745615587649, 3.986398505019110416 ) ) ;
#41770 = CARTESIAN_POINT ( 'NONE',  ( 0.5817216825391126056, 40.11545677781317920, -24.28960847183133609 ) ) ;
#41771 = CARTESIAN_POINT ( 'NONE',  ( 0.1313383488274104394, -15.91164383651771885, 40.08066228784235108 ) ) ;
#41772 = CARTESIAN_POINT ( 'NONE',  ( 4.962356264823602814, -36.43094049105359744, -21.07183363638911189 ) ) ;
#41773 = CARTESIAN_POINT ( 'NONE',  ( 0.8554163680231720024, 42.82911630180360163, -19.15391004255791430 ) ) ;
#41774 = DIRECTION ( 'NONE',  ( 0.000000000000000000, 0.000000000000000000, 1.000000000000000000 ) ) ;
#41775 = CARTESIAN_POINT ( 'NONE',  ( 0.9758171775293923433, 37.16279804060133074, 21.44911662810663344 ) ) ;
#41776 = LINE ( 'NONE', #23877, #11748 ) ;
#41777 = B_SPLINE_CURVE_WITH_KNOTS ( 'NONE', 3,
 ( #53690, #10819, #48710, #1382 ),
 .UNSPECIFIED., .F., .F.,
 ( 4, 4 ),
 ( 1.301042606982605321E-18, 0.004041751736740996012 ),
 .UNSPECIFIED. ) ;
#41778 = B_SPLINE_CURVE_WITH_KNOTS ( 'NONE', 3,
 ( #27810, #37859, #46942, #51921, #3977, #56920 ),
 .UNSPECIFIED., .F., .F.,
 ( 4, 2, 4 ),
 ( 2.196947838360372653E-17, 0.0002293755540694311017, 0.0004587511081388401940 ),
 .UNSPECIFIED. ) ;
#41779 = LINE ( 'NONE', #60842, #13491 ) ;
#41780 = CIRCLE ( 'NONE', #29719, 10.00000000000000000 ) ;
#41781 = CARTESIAN_POINT ( 'NONE',  ( 4.000000000000003553, -0.3902508023145557225, -5.599999999999998757 ) ) ;
#41782 = CARTESIAN_POINT ( 'NONE',  ( 0.6029442701453590070, -47.47924998016712550, 12.54057600268335548 ) ) ;
#41784 = VERTEX_POINT ( 'NONE', #39817 ) ;
#41783 = CARTESIAN_POINT ( 'NONE',  ( 0.9741495583595179975, 39.48917442789120003, 16.78504838919898745 ) ) ;
#41785 = EDGE_LOOP ( 'NONE', ( #28741, #14282, #55537, #59375 ) ) ;
#41786 = CARTESIAN_POINT ( 'NONE',  ( 4.963659409799330291, 20.22157859941785674, -39.92545197189527784 ) ) ;
#41787 = AXIS2_PLACEMENT_3D ( 'NONE', #19933, #474, #15528 ) ;
#41788 = DIRECTION ( 'NONE',  ( 0.000000000000000000, 0.000000000000000000, -1.000000000000000000 ) ) ;
#41789 = ORIENTED_EDGE ( 'NONE', *, *, #48935, .F. ) ;
#41790 = ORIENTED_EDGE ( 'NONE', *, *, #40316, .T. ) ;
#41791 = CARTESIAN_POINT ( 'NONE',  ( 0.7413678028165008316, -31.02027698649011711, 31.34052500280865772 ) ) ;
#41792 = CARTESIAN_POINT ( 'NONE',  ( 0.6009452777970415438, 6.711700115492909013, 47.63713033690756049 ) ) ;
#41793 = B_SPLINE_CURVE_WITH_KNOTS ( 'NONE', 3,
 ( #2609, #17046, #50845, #11410, #7936, #21113 ),
 .UNSPECIFIED., .F., .F.,
 ( 4, 2, 4 ),
 ( 0.000000000000000000, 0.0002447195606305737161, 0.0004894391212611474322 ),
 .UNSPECIFIED. ) ;
#41794 = UNCERTAINTY_MEASURE_WITH_UNIT (LENGTH_MEASURE( 1.000000000000000082E-05 ), #42001, 'distance_accuracy_value', 'NONE');
#41795 = EDGE_LOOP ( 'NONE', ( #9565, #20079, #38217, #28439 ) ) ;
#41796 = ORIENTED_EDGE ( 'NONE', *, *, #18549, .T. ) ;
#41797 = EDGE_CURVE ( 'NONE', #8563, #219, #19773, .T. ) ;
#41798 = CARTESIAN_POINT ( 'NONE',  ( 5.895596859100789899, -19.39731145114843613, -5.317188324634858354 ) ) ;
#41799 = FACE_OUTER_BOUND ( 'NONE', #27350, .T. ) ;
#41800 = CARTESIAN_POINT ( 'NONE',  ( 2.299746137290199055, 48.99837783518191259, 1.854806514677992624 ) ) ;
#41801 = ORIENTED_EDGE ( 'NONE', *, *, #38219, .T. ) ;
#41802 = ORIENTED_EDGE ( 'NONE', *, *, #24644, .T. ) ;
#41803 = B_SPLINE_CURVE_WITH_KNOTS ( 'NONE', 3,
 ( #9352, #32878, #27847, #37270, #51952, #24076, #57248, #9044, #38503, #46980, #37900, #4015, #28150, #57555, #14692, #4318 ),
 .UNSPECIFIED., .F., .F.,
 ( 4, 3, 3, 3, 3, 4 ),
 ( 1.962735358247464152E-17, 0.0002618515315864422478, 0.0003927756766341962565, 0.0005236998216950601668, 0.0007855159896329981387, 0.001047349442285927870 ),
 .UNSPECIFIED. ) ;
#41804 = FACE_OUTER_BOUND ( 'NONE', #52348, .T. ) ;
#41805 = AXIS2_PLACEMENT_3D ( 'NONE', #52895, #42297, #56663 ) ;
#41806 = DIRECTION ( 'NONE',  ( -1.000000000000000000, -0.000000000000000000, -0.000000000000000000 ) ) ;
#41807 = CARTESIAN_POINT ( 'NONE',  ( 0.5998501479064708430, -48.10473956285919428, -0.5236536531313246146 ) ) ;
#41808 = VERTEX_POINT ( 'NONE', #44821 ) ;
#41809 = ORIENTED_EDGE ( 'NONE', *, *, #22218, .F. ) ;
#41810 = CARTESIAN_POINT ( 'NONE',  ( 0.7764139734771244861, 10.00418665513137384, 45.82528472662399111 ) ) ;
#41811 = ORIENTED_EDGE ( 'NONE', *, *, #52338, .F. ) ;
#41812 = CARTESIAN_POINT ( 'NONE',  ( -6.016761891674565099, 4.880293656735219088, -18.20023637398594119 ) ) ;
#41813 = CARTESIAN_POINT ( 'NONE',  ( 4.962356264823608143, 23.01169039590672938, -35.23773124060741679 ) ) ;
#41814 = CARTESIAN_POINT ( 'NONE',  ( 0.8557997880470697982, 38.55640757422439435, 28.43566216844983074 ) ) ;
#41815 = CARTESIAN_POINT ( 'NONE',  ( -6.016761891674565099, 11.46828378093559131, 14.95139917749708758 ) ) ;
#41816 = CARTESIAN_POINT ( 'NONE',  ( 2.643462169533613793, -7.637863311827277180, -47.42536612906426541 ) ) ;
#41817 = ORIENTED_EDGE ( 'NONE', *, *, #41694, .T. ) ;
#41818 = CARTESIAN_POINT ( 'NONE',  ( 0.6041374136657476912, -23.90252055111350415, 41.74951251761532234 ) ) ;
#41819 = CARTESIAN_POINT ( 'NONE',  ( -6.057079549204054558, 18.62501892953343585, -4.892841809650052554 ) ) ;
#41820 = EDGE_CURVE ( 'NONE', #30940, #6137, #55267, .T. ) ;
#41821 = CARTESIAN_POINT ( 'NONE',  ( 0.9745511491811735816, -21.15859207114723972, -37.32887948083622121 ) ) ;
#41822 = VERTEX_POINT ( 'NONE', #15990 ) ;
#41823 = CARTESIAN_POINT ( 'NONE',  ( 5.960721111146673579, 7.848955554238242982, 18.96557324978290282 ) ) ;
#41824 = EDGE_CURVE ( 'NONE', #50613, #52183, #41891, .T. ) ;
#41825 = CARTESIAN_POINT ( 'NONE',  ( 0.9730545539215883499, -26.52009130076794108, 33.73144377768549163 ) ) ;
#41826 = CARTESIAN_POINT ( 'NONE',  ( -6.057079549204054558, 12.01317374117834902, -15.05041154799434011 ) ) ;
#41827 = DIRECTION ( 'NONE',  ( -0.07906939808003032866, -0.9752531043637164831, 0.2064689146486601845 ) ) ;
#41828 = VECTOR ( 'NONE', #38213, 1000.000000000000114 ) ;
#41829 = EDGE_LOOP ( 'NONE', ( #20462, #48492, #33717, #45815 ) ) ;
#41830 = CARTESIAN_POINT ( 'NONE',  ( 0.1073791018717483448, 39.65380858626214433, -16.95003405440273525 ) ) ;
#41831 = EDGE_CURVE ( 'NONE', #35339, #43120, #2158, .T. ) ;
#41832 = FACE_OUTER_BOUND ( 'NONE', #12210, .T. ) ;
#41833 = CARTESIAN_POINT ( 'NONE',  ( -6.078457390727109555, 0.6128065477899394820, -19.24627182527810021 ) ) ;
#41834 = CARTESIAN_POINT ( 'NONE',  ( 2.500000000000002220, 3.061616997868386099E-16, -5.574599999999999334 ) ) ;
#41835 = CARTESIAN_POINT ( 'NONE',  ( 0.9736507210033070736, -42.59776535855980484, 5.153758453069401391 ) ) ;
#41836 =( BOUNDED_SURFACE ( )  B_SPLINE_SURFACE ( 3, 1, ( 
 ( #13801, #14413 ),
 ( #9691, #57583 ),
 ( #61068, #32591 ),
 ( #52284, #47009 ) ),
 .UNSPECIFIED., .F., .F., .F. ) 
 B_SPLINE_SURFACE_WITH_KNOTS ( ( 4, 4 ),
 ( 2, 2 ),
 ( 0.000000000000000000, 1.000000000000000000 ),
 ( 0.000000000000000000, 1.000000000000000000 ),
 .UNSPECIFIED. ) 
 GEOMETRIC_REPRESENTATION_ITEM ( )  RATIONAL_B_SPLINE_SURFACE ( (
 ( 1.000000000000000000, 1.000000000000000000),
 ( 0.9952954269826590483, 0.8620686068821307169),
 ( 0.9952954269826590483, 0.8620686068821307169),
 ( 1.000000000000000000, 1.000000000000000000) ) ) 
 REPRESENTATION_ITEM ( '' )  SURFACE ( )  );
#41837 = CARTESIAN_POINT ( 'NONE',  ( 0.5830081025819910945, -46.77220438400303237, 3.404839415199392150 ) ) ;
#41838 = CARTESIAN_POINT ( 'NONE',  ( 5.959547316686252039, -5.315863417546468739, 19.82530672674353056 ) ) ;
#41839 = FACE_OUTER_BOUND ( 'NONE', #45631, .T. ) ;
#41840 = CARTESIAN_POINT ( 'NONE',  ( 4.956445790443991584, 38.51510088324707226, 27.09474218539341450 ) ) ;
#41841 = CARTESIAN_POINT ( 'NONE',  ( 0.9775691876210983455, 41.90693278755279749, 0.3777477061777904099 ) ) ;
#41842 = FACE_OUTER_BOUND ( 'NONE', #14015, .T. ) ;
#41844 = ORIENTED_EDGE ( 'NONE', *, *, #5838, .F. ) ;
#41843 = ADVANCED_FACE ( 'NONE', ( #15064 ), #3729, .F. ) ;
#41845 = CARTESIAN_POINT ( 'NONE',  ( 0.5797568599927122035, -25.76189090885626598, 39.18609811490797767 ) ) ;
#41847 = ADVANCED_FACE ( 'NONE', ( #59179 ), #27761, .T. ) ;
#41846 = CARTESIAN_POINT ( 'NONE',  ( 0.1140933569871964426, -35.13362084938451346, -26.69416857846670865 ) ) ;
#41848 = CYLINDRICAL_SURFACE ( 'NONE', #14026, 2.649999999999992806 ) ;
#41849 = B_SPLINE_CURVE_WITH_KNOTS ( 'NONE', 3,
 ( #160, #58711, #19618, #34333 ),
 .UNSPECIFIED., .F., .F.,
 ( 4, 4 ),
 ( 6.582812753581314488E-17, 0.005004948556313859077 ),
 .UNSPECIFIED. ) ;
#41850 = LINE ( 'NONE', #22718, #60129 ) ;
#41851 = AXIS2_PLACEMENT_3D ( 'NONE', #14712, #29406, #19111 ) ;
#41852 = CARTESIAN_POINT ( 'NONE',  ( 0.9730545539215883499, -39.44597740938072405, 16.88610103448544209 ) ) ;
#41853 = SHAPE_DEFINITION_REPRESENTATION ( #37327, #2385 ) ;
#41854 = CARTESIAN_POINT ( 'NONE',  ( 0.5830082357119559244, -25.46372197616247490, 39.38059037214954827 ) ) ;
#41855 = CARTESIAN_POINT ( 'NONE',  ( 5.838029081930955932, -40.63013578422354755, -24.08852681897500503 ) ) ;
#41856 = CONICAL_SURFACE ( 'NONE', #48842, 43.92652462719577500, 1.486293639869522343 ) ;
#41857 = CARTESIAN_POINT ( 'NONE',  ( 0.8557997880470599172, 34.51495345639595058, -33.22501220301865033 ) ) ;
#41859 = ORIENTED_EDGE ( 'NONE', *, *, #10253, .T. ) ;
#41858 = CARTESIAN_POINT ( 'NONE',  ( 0.6031356219577717059, -46.49081620741446841, -12.36679943215644961 ) ) ;
#41860 = VERTEX_POINT ( 'NONE', #24758 ) ;
#41861 = CARTESIAN_POINT ( 'NONE',  ( 0.5804410086790514622, -25.69437916690351642, -39.23415261073943583 ) ) ;
#41862 = LINE ( 'NONE', #26494, #1497 ) ;
#41863 = CARTESIAN_POINT ( 'NONE',  ( 4.962356264823608143, 0.000000000000000000, 0.000000000000000000 ) ) ;
#41864 = VERTEX_POINT ( 'NONE', #29756 ) ;
#41865 = CARTESIAN_POINT ( 'NONE',  ( 0.5824936645240086364, 22.21727860259796472, 41.29928220362735658 ) ) ;
#41866 = CARTESIAN_POINT ( 'NONE',  ( 2.500000000000000000, -1.768423874527823569, 1.021000000000002350 ) ) ;
#41867 = CARTESIAN_POINT ( 'NONE',  ( 0.1095718737110177449, 5.883530294870134902, -42.72125633542928824 ) ) ;
#41868 = ORIENTED_EDGE ( 'NONE', *, *, #49935, .F. ) ;
#41869 = ORIENTED_EDGE ( 'NONE', *, *, #36166, .T. ) ;
#41870 = EDGE_CURVE ( 'NONE', #54056, #2081, #38900, .T. ) ;
#41871 = CARTESIAN_POINT ( 'NONE',  ( 0.9789889208857696090, 24.78187179627650139, -33.79635673138873386 ) ) ;
#41872 = VECTOR ( 'NONE', #859, 1000.000000000000114 ) ;
#41873 = VECTOR ( 'NONE', #31572, 1000.000000000000000 ) ;
#41874 = CARTESIAN_POINT ( 'NONE',  ( 0.7048096507298579061, 46.24547838151348600, 13.26491767067531136 ) ) ;
#41875 = CARTESIAN_POINT ( 'NONE',  ( 0.9769922540276034795, 33.16186414041638386, -25.62464286226623145 ) ) ;
#41876 = CARTESIAN_POINT ( 'NONE',  ( 1.112077966505211624, -44.06731193995874918, 1.049925480652556198 ) ) ;
#41877 = B_SPLINE_CURVE_WITH_KNOTS ( 'NONE', 3,
 ( #23867, #29481, #48291, #19486 ),
 .UNSPECIFIED., .F., .F.,
 ( 4, 4 ),
 ( 4.336808689942017736E-19, 0.004446298630425048540 ),
 .UNSPECIFIED. ) ;
#41878 = CARTESIAN_POINT ( 'NONE',  ( 0.6027444965799114707, 48.99797994875344642, 3.276656348932040164 ) ) ;
#41879 = B_SPLINE_CURVE_WITH_KNOTS ( 'NONE', 3,
 ( #4137, #60233, #13271, #23276 ),
 .UNSPECIFIED., .F., .F.,
 ( 4, 4 ),
 ( 1.179611963664228824E-16, 0.005004741218457495200 ),
 .UNSPECIFIED. ) ;
#41880 = CARTESIAN_POINT ( 'NONE',  ( 0.1129192098497447394, 33.91039995638862337, 28.23183597612653983 ) ) ;
#41881 = VERTEX_POINT ( 'NONE', #41649 ) ;
#41882 = CARTESIAN_POINT ( 'NONE',  ( 4.694002226626921015, 44.18338616738627422, -11.23001149731177328 ) ) ;
#41883 = CARTESIAN_POINT ( 'NONE',  ( -6.072942160501519915, -6.636811946999699785, 18.07641804863957091 ) ) ;
#41884 = VECTOR ( 'NONE', #8766, 1000.000000000000000 ) ;
#41885 = ORIENTED_EDGE ( 'NONE', *, *, #34900, .F. ) ;
#41886 = CARTESIAN_POINT ( 'NONE',  ( 0.5987334363312690755, -20.42989704442242171, 44.65626734542841803 ) ) ;
#41887 = CARTESIAN_POINT ( 'NONE',  ( 5.974727161628367256, 20.52494643607030156, -0.01551142186628274786 ) ) ;
#41888 = CARTESIAN_POINT ( 'NONE',  ( 2.879087469061462734, 38.86168815156121781, -20.63663903822967427 ) ) ;
#41889 = CARTESIAN_POINT ( 'NONE',  ( 0.5997462898726536595, 23.17609050332929854, -43.29457771044543080 ) ) ;
#41890 = ORIENTED_EDGE ( 'NONE', *, *, #7431, .T. ) ;
#41891 = B_SPLINE_CURVE_WITH_KNOTS ( 'NONE', 3,
 ( #49481, #6536, #25994, #34788 ),
 .UNSPECIFIED., .F., .F.,
 ( 4, 4 ),
 ( 0.000000000000000000, 0.005004741218457366830 ),
 .UNSPECIFIED. ) ;
#41892 = VERTEX_POINT ( 'NONE', #26601 ) ;
#41893 = CARTESIAN_POINT ( 'NONE',  ( 1.231276596079881047, -31.65135013586901991, 27.48579279545509380 ) ) ;
#41894 = CARTESIAN_POINT ( 'NONE',  ( 0.7044674535452954967, -47.28336972574645358, -13.26972758534514618 ) ) ;
#41895 = CARTESIAN_POINT ( 'NONE',  ( 0.1310142868023716212, 25.74368468368890106, 34.59629828998422596 ) ) ;
#41896 = ORIENTED_EDGE ( 'NONE', *, *, #9148, .T. ) ;
#41897 = DIRECTION ( 'NONE',  ( -1.000000000000000000, -3.673819061467147552E-16, 1.925929944387234758E-32 ) ) ;
#41898 = EDGE_CURVE ( 'NONE', #53021, #11949, #50082, .T. ) ;
#41899 = ORIENTED_EDGE ( 'NONE', *, *, #59954, .T. ) ;
#41900 = DIRECTION ( 'NONE',  ( -1.685288351013738396E-16, 1.000000000000000000, 0.000000000000000000 ) ) ;
#41901 = CARTESIAN_POINT ( 'NONE',  ( 0.6029443449137436017, -25.49413300155796591, 41.97128447500987392 ) ) ;
#41902 = CARTESIAN_POINT ( 'NONE',  ( 4.975801465491694664, 32.01766832630313075, -35.64402118370923489 ) ) ;
#41903 = ORIENTED_EDGE ( 'NONE', *, *, #51493, .F. ) ;
#41905 = VECTOR ( 'NONE', #6039, 1000.000000000000114 ) ;
#41904 = CARTESIAN_POINT ( 'NONE',  ( 0.7948878604505664747, -8.691324790642898535, -48.32348829174041072 ) ) ;
#41906 = EDGE_CURVE ( 'NONE', #2801, #36534, #24665, .T. ) ;
#41907 = CARTESIAN_POINT ( 'NONE',  ( 5.910764540655178756, 0.6565643306764937792, -20.10149650520693143 ) ) ;
#41908 = CARTESIAN_POINT ( 'NONE',  ( 0.9730545539215892381, 25.71816799638828499, -34.34678117142529175 ) ) ;
#41909 = VERTEX_POINT ( 'NONE', #41050 ) ;
#41910 = CARTESIAN_POINT ( 'NONE',  ( -19.55613784151982060, -12.42316071588242110, 1.387283936007070562 ) ) ;
#41911 = CARTESIAN_POINT ( 'NONE',  ( 0.2285344041767085332, -43.65329955122442129, 6.394576497824234984 ) ) ;
#41912 = CARTESIAN_POINT ( 'NONE',  ( 2.618530812446115519, -26.46994001812951680, -38.84673814665556080 ) ) ;
#41913 = CARTESIAN_POINT ( 'NONE',  ( 4.975801465491694664, 42.71626295676232843, 21.70134120755216145 ) ) ;
#41914 = CARTESIAN_POINT ( 'NONE',  ( 5.959547316686252039, -19.82715097195166010, 5.308980600728112620 ) ) ;
#41915 = EDGE_LOOP ( 'NONE', ( #4354, #36327, #4242, #17611 ) ) ;
#41916 = CARTESIAN_POINT ( 'NONE',  ( -5.995132425357893702, -9.429450169547841654, -16.31525984181043043 ) ) ;
#41917 = AXIS2_PLACEMENT_3D ( 'NONE', #3750, #42020, #41402 ) ;
#41918 = CARTESIAN_POINT ( 'NONE',  ( 4.975801465491695552, 40.15204426031497320, 26.14269827151694514 ) ) ;
#41919 = ORIENTED_EDGE ( 'NONE', *, *, #12680, .T. ) ;
#41920 = CARTESIAN_POINT ( 'NONE',  ( 0.6000166863083090663, -43.04473087057990455, -23.64264422580097502 ) ) ;
#41921 = CARTESIAN_POINT ( 'NONE',  ( 0.9790320750461900534, -27.12300087535202309, 31.94808219686815676 ) ) ;
#41923 = EDGE_CURVE ( 'NONE', #60001, #27320, #50408, .T. ) ;
#41922 = FACE_OUTER_BOUND ( 'NONE', #58381, .T. ) ;
#41924 = CARTESIAN_POINT ( 'NONE',  ( 1.227938101723748288, 41.66816631169206886, -10.28900963485336995 ) ) ;
#41925 = CARTESIAN_POINT ( 'NONE',  ( 0.8760168074886960365, 48.09529047980636562, 0.8912768426707899927 ) ) ;
#41926 = CARTESIAN_POINT ( 'NONE',  ( 0.6001305935487315502, -11.94532529598410875, 46.60388846085702141 ) ) ;
#41927 =( NAMED_UNIT ( * ) PLANE_ANGLE_UNIT ( ) SI_UNIT ( $, .RADIAN. ) );
#41928 = CARTESIAN_POINT ( 'NONE',  ( 0.6029303876144825880, 38.08638053211497976, 29.38970229176916860 ) ) ;
#41929 = CARTESIAN_POINT ( 'NONE',  ( 5.960721111146673579, -17.77882586010674260, 10.25731071096551794 ) ) ;
#41930 = CARTESIAN_POINT ( 'NONE',  ( 4.833616638992208614, -45.27110352095254342, 9.466882727841344547 ) ) ;
#41931 = CARTESIAN_POINT ( 'NONE',  ( -6.015611763856276717, -9.427003116184289766, 16.31561949997072958 ) ) ;
#41932 = ORIENTED_EDGE ( 'NONE', *, *, #49273, .F. ) ;
#41933 = VECTOR ( 'NONE', #38581, 999.9999999999998863 ) ;
#41934 = CARTESIAN_POINT ( 'NONE',  ( 1.227938101723756947, 11.92353943227949387, 41.23019537246713639 ) ) ;
#41935 = CARTESIAN_POINT ( 'NONE',  ( 4.975610109902397937, 24.86209007718959185, 42.12274782266089801 ) ) ;
#41936 = CARTESIAN_POINT ( 'NONE',  ( 5.894904586330512508, -17.30581086051407169, -10.24882054295791001 ) ) ;
#41937 = CARTESIAN_POINT ( 'NONE',  ( 4.553261556744875094, 0.000000000000000000, 0.000000000000000000 ) ) ;
#41938 = CARTESIAN_POINT ( 'NONE',  ( 0.1310142868023661811, 26.75450212504321001, -33.82067078731319043 ) ) ;
#41939 = CARTESIAN_POINT ( 'NONE',  ( 0.6023142530420679819, -38.00626667377541423, 29.49327578399123695 ) ) ;
#41940 = B_SPLINE_CURVE_WITH_KNOTS ( 'NONE', 3,
 ( #47906, #10302, #5262, #4958 ),
 .UNSPECIFIED., .F., .F.,
 ( 4, 4 ),
 ( 1.551583845779545699E-17, 0.005004948556313822648 ),
 .UNSPECIFIED. ) ;
#41941 = AXIS2_PLACEMENT_3D ( 'NONE', #57507, #52520, #38156 ) ;
#41942 = EDGE_LOOP ( 'NONE', ( #52636, #33387, #31610, #54410, #18675, #31035, #34305, #53561, #36477, #20031, #47427, #33663, #22466, #5213, #32013, #36125, #15767, #1185, #60185, #21294, #55974, #45630, #36473, #20662, #6477, #21130, #37392, #15994, #3398, #47352, #4446, #48433, #27916, #28069, #3296, #18378, #10369, #53762, #41088, #8095, #37432, #54520, #33789, #9897, #22748, #11481, #40871, #36486, #28597, #21664, #56775, #47034, #58933, #11990, #11175, #4379, #60298, #7889, #52491, #28298, #21916, #56569, #56983, #52571, #8786, #20287, #39039, #30131, #5746, #33113, #33854, #47235, #51517, #37785, #5558, #37961, #45451, #11403, #8180, #39120, #25134, #27682, #33942, #10205, #16697, #48020, #11522, #50925, #19899, #41661, #1570, #25574, #56029, #53179, #18902, #40363, #18975, #12864, #36748, #17451, #60934, #47103, #52693, #20361, #42870, #19176, #29236, #53184, #48929, #46971, #12511, #48120, #34319, #9349, #60541, #34251, #12342, #30650, #20986, #15848, #53480, #24416, #9717, #35739, #18289, #38811, #60430, #51145, #32327, #12431, #4770, #54737, #26533, #27837, #15527, #51476, #29541, #15079, #27455, #4334, #37897, #43173, #57302, #45123, #30904, #61501, #61115, #40596, #16972, #1284, #7152, #22340 ) ) ;
#41943 = CARTESIAN_POINT ( 'NONE',  ( 0.9730545539215883499, 10.61654491617622398, -41.57420493492374192 ) ) ;
#41944 = B_SPLINE_CURVE_WITH_KNOTS ( 'NONE', 3,
 ( #43218, #47284, #56970, #33196, #28468, #4635 ),
 .UNSPECIFIED., .F., .F.,
 ( 4, 2, 4 ),
 ( 1.823789517034659149E-17, 0.0002293319059085100083, 0.0004586638118170017478 ),
 .UNSPECIFIED. ) ;
#41945 = CARTESIAN_POINT ( 'NONE',  ( -6.015611763856276717, -18.68284711750056815, -2.453375430804263235 ) ) ;
#41946 = CARTESIAN_POINT ( 'NONE',  ( 2.533389852662419894, 28.40184444967290034, -33.62715812539327231 ) ) ;
#41947 = CARTESIAN_POINT ( 'NONE',  ( -18.24846456548969797, -7.719455939378113030, -2.099999999999997868 ) ) ;
#41948 = ORIENTED_EDGE ( 'NONE', *, *, #46090, .F. ) ;
#41949 = EDGE_CURVE ( 'NONE', #29740, #6434, #16919, .T. ) ;
#41950 = CARTESIAN_POINT ( 'NONE',  ( 2.618530812446115519, -2.977833924573772606, -46.91331681213615923 ) ) ;
#41951 = EDGE_CURVE ( 'NONE', #52969, #23152, #17835, .T. ) ;
#41952 = CARTESIAN_POINT ( 'NONE',  ( 0.6025881611877910160, 24.24244696985808289, -41.55278713510058708 ) ) ;
#41953 = VERTEX_POINT ( 'NONE', #7474 ) ;
#41954 =( BOUNDED_SURFACE ( )  B_SPLINE_SURFACE ( 3, 1, ( 
 ( #1015, #58629 ),
 ( #21063, #16065 ),
 ( #6304, #43663 ),
 ( #48634, #6001 ) ),
 .UNSPECIFIED., .F., .F., .F. ) 
 B_SPLINE_SURFACE_WITH_KNOTS ( ( 4, 4 ),
 ( 2, 2 ),
 ( 0.000000000000000000, 1.000000000000000000 ),
 ( 0.000000000000000000, 1.000000000000000000 ),
 .UNSPECIFIED. ) 
 GEOMETRIC_REPRESENTATION_ITEM ( )  RATIONAL_B_SPLINE_SURFACE ( (
 ( 1.000000000000000000, 1.000000000000000000),
 ( 0.9952954269826590483, 0.8620686068821339365),
 ( 0.9952954269826590483, 0.8620686068821339365),
 ( 1.000000000000000000, 1.000000000000000000) ) ) 
 REPRESENTATION_ITEM ( '' )  SURFACE ( )  );
#41955 = ADVANCED_FACE ( 'NONE', ( #27530 ), #1525, .F. ) ;
#41956 = CARTESIAN_POINT ( 'NONE',  ( 1.296416391601052487, -26.60065513383224456, 35.13847635466117936 ) ) ;
#41957 = ORIENTED_EDGE ( 'NONE', *, *, #35677, .F. ) ;
#41958 = CARTESIAN_POINT ( 'NONE',  ( 5.880360259849752858, 47.87242051977165858, -3.090325311464368507 ) ) ;
#41960 = CARTESIAN_POINT ( 'NONE',  ( 0.6252788684277220677, 17.60247651936639102, 45.84317998959954110 ) ) ;
#41959 = VECTOR ( 'NONE', #30205, 1000.000000000000114 ) ;
#41961 = EDGE_LOOP ( 'NONE', ( #38283, #10678, #41298, #48157 ) ) ;
#41962 = CARTESIAN_POINT ( 'NONE',  ( -6.016761891674565099, -7.207804629151182141, -17.41015286184810407 ) ) ;
#41963 = CARTESIAN_POINT ( 'NONE',  ( 0.8560838555295223751, 43.53454501559562573, 17.46757637357886850 ) ) ;
#41964 = ORIENTED_EDGE ( 'NONE', *, *, #33677, .F. ) ;
#41965 = CARTESIAN_POINT ( 'NONE',  ( 0.9758171775293923433, 21.45936886481795014, 37.15687890897625323 ) ) ;
#41966 = CARTESIAN_POINT ( 'NONE',  ( 5.896782393890504181, 12.98055409426303441, 15.36331026452057813 ) ) ;
#41967 = VERTEX_POINT ( 'NONE', #31932 ) ;
#41968 = CARTESIAN_POINT ( 'NONE',  ( 0.6021448801613057400, -7.579532981145714388, -48.51898410328343658 ) ) ;
#41969 = ORIENTED_EDGE ( 'NONE', *, *, #30518, .F. ) ;
#41970 = CARTESIAN_POINT ( 'NONE',  ( -6.072942160501519915, 17.84350912780789500, -7.239706091745485850 ) ) ;
#41971 = ORIENTED_EDGE ( 'NONE', *, *, #34929, .T. ) ;
#41972 = EDGE_CURVE ( 'NONE', #17539, #19838, #4437, .T. ) ;
#41973 = ORIENTED_EDGE ( 'NONE', *, *, #45155, .F. ) ;
#41974 = CARTESIAN_POINT ( 'NONE',  ( 0.6026777506516366456, -42.87348921357890674, -23.94598741523000740 ) ) ;
#41975 = CARTESIAN_POINT ( 'NONE',  ( 0.5786265663353196143, 44.52624106864168141, -17.66171603226031550 ) ) ;
#41976 = DIRECTION ( 'NONE',  ( 1.000000000000000000, 1.836909530733573776E-16, 0.000000000000000000 ) ) ;
#41977 = CIRCLE ( 'NONE', #39971, 43.92652462719577500 ) ;
#41978 = CARTESIAN_POINT ( 'NONE',  ( 4.956653778116982600, -43.37017594958069111, 20.77844580450546985 ) ) ;
#41979 = CARTESIAN_POINT ( 'NONE',  ( 3.390910168358337806, -28.93279679135903848, -33.12084549590425553 ) ) ;
#41980 = EDGE_LOOP ( 'NONE', ( #9367, #26048 ) ) ;
#41981 = CARTESIAN_POINT ( 'NONE',  ( 3.050102900204245682, 6.022580839601601177, 43.57928142143379802 ) ) ;
#41982 = ADVANCED_FACE ( 'NONE', ( #21915 ), #27167, .F. ) ;
#41983 = CARTESIAN_POINT ( 'NONE',  ( 5.896782393890504181, 12.98055409426324580, -15.36331026452040049 ) ) ;
#41984 = CARTESIAN_POINT ( 'NONE',  ( 2.254628338793795983, 0.05544974030731342207, 44.02889495774882533 ) ) ;
#41985 = ORIENTED_EDGE ( 'NONE', *, *, #40471, .T. ) ;
#41986 = EDGE_CURVE ( 'NONE', #18352, #12599, #26922, .T. ) ;
#41987 = VERTEX_POINT ( 'NONE', #12841 ) ;
#41988 = CARTESIAN_POINT ( 'NONE',  ( 0.7948878604505678069, 11.76956405680572892, 47.66734741110693108 ) ) ;
#41989 = FACE_OUTER_BOUND ( 'NONE', #36209, .T. ) ;
#41990 = CARTESIAN_POINT ( 'NONE',  ( 4.335381028904216727, 29.74326630871418331, 38.92422069808531404 ) ) ;
#41991 = CARTESIAN_POINT ( 'NONE',  ( -6.017396004339687465, -16.31924478664281963, 9.420565012089369361 ) ) ;
#41992 = B_SPLINE_CURVE_WITH_KNOTS ( 'NONE', 3,
 ( #31321, #7177, #45443, #44527, #26617, #45747, #2798, #15695, #34800, #1558, #50063, #57346, #24791, #34506, #44236, #10391 ),
 .UNSPECIFIED., .F., .F.,
 ( 4, 3, 3, 3, 3, 4 ),
 ( 6.939740885162003740E-18, 0.0002724568934985503971, 0.0004086836638483758643, 0.0005449104342063602240, 0.0008173270854453667817, 0.001089761613562689226 ),
 .UNSPECIFIED. ) ;
#41993 = ORIENTED_EDGE ( 'NONE', *, *, #10680, .F. ) ;
#41994 = CARTESIAN_POINT ( 'NONE',  ( 0.5832366564991512403, 47.52097076201152248, 5.981458972433913779 ) ) ;
#41995 = CARTESIAN_POINT ( 'NONE',  ( 4.956653778116992370, 3.690426056930664611, -47.94889704119048446 ) ) ;
#41997 = EDGE_CURVE ( 'NONE', #11842, #9433, #35117, .T. ) ;
#41996 = CARTESIAN_POINT ( 'NONE',  ( 0.5549461598389361372, 43.11493157709418966, -9.290875662137066726 ) ) ;
#41998 = CYLINDRICAL_SURFACE ( 'NONE', #51993, 75.00000000000001421 ) ;
#41999 = B_SPLINE_CURVE_WITH_KNOTS ( 'NONE', 3,
 ( #12276, #26047, #31671, #3151, #60461, #21655 ),
 .UNSPECIFIED., .F., .F.,
 ( 4, 2, 4 ),
 ( 1.870761316369714769E-17, 0.0002293755540694314540, 0.0004587511081388442056 ),
 .UNSPECIFIED. ) ;
#42000 = CARTESIAN_POINT ( 'NONE',  ( 0.9268187852002115479, -43.58820572414531114, 6.619868175289538748 ) ) ;
#42001 =( LENGTH_UNIT ( ) NAMED_UNIT ( * ) SI_UNIT ( .MILLI., .METRE. ) );
#42002 = CIRCLE ( 'NONE', #11996, 48.91267123290010943 ) ;
#42003 = VERTEX_POINT ( 'NONE', #60403 ) ;
#42004 = CARTESIAN_POINT ( 'NONE',  ( 0.2279481005628782586, 21.07700012148384516, -38.75904478895067484 ) ) ;
#42005 = CARTESIAN_POINT ( 'NONE',  ( 0.1064266379913939298, 5.071708164747061431, -42.82540706760017457 ) ) ;
#42006 = CARTESIAN_POINT ( 'NONE',  ( 4.967162193818131399, -3.259922920618036901, 42.96271701169384016 ) ) ;
#42007 = CARTESIAN_POINT ( 'NONE',  ( 4.691466044806102076, -20.01963481131688027, 39.84135254923101144 ) ) ;
#42008 = AXIS2_PLACEMENT_3D ( 'NONE', #50548, #55547, #27368 ) ;
#42009 = CARTESIAN_POINT ( 'NONE',  ( 0.5807400328401574052, 17.82553128098469131, -44.45848844984423920 ) ) ;
#42010 = CARTESIAN_POINT ( 'NONE',  ( 0.5832367798473389042, 6.521664418777854522, -47.44985149964043103 ) ) ;
#42011 = CARTESIAN_POINT ( 'NONE',  ( 0.6026777506516367566, -49.10718938754244789, 0.1741869491615331278 ) ) ;
#42012 = DIRECTION ( 'NONE',  ( 0.07906939808003035641, -0.6871887087747612366, -0.7221632148065547652 ) ) ;
#42013 = B_SPLINE_CURVE_WITH_KNOTS ( 'NONE', 3,
 ( #962, #5030, #39215, #57336 ),
 .UNSPECIFIED., .F., .F.,
 ( 4, 4 ),
 ( 6.736447455048116623E-17, 0.005004741218457475251 ),
 .UNSPECIFIED. ) ;
#42014 =( BOUNDED_SURFACE ( )  B_SPLINE_SURFACE ( 3, 1, ( 
 ( #26000, #7802 ),
 ( #3100, #26929 ),
 ( #59813, #45740 ),
 ( #7481, #49801 ) ),
 .UNSPECIFIED., .F., .F., .F. ) 
 B_SPLINE_SURFACE_WITH_KNOTS ( ( 4, 4 ),
 ( 2, 2 ),
 ( 0.000000000000000000, 1.000000000000000000 ),
 ( 0.000000000000000000, 1.000000000000000000 ),
 .UNSPECIFIED. ) 
 GEOMETRIC_REPRESENTATION_ITEM ( )  RATIONAL_B_SPLINE_SURFACE ( (
 ( 1.000000000000000000, 1.000000000000000000),
 ( 0.9751682680413298332, 0.9999560080971552356),
 ( 0.9751682680413298332, 0.9999560080971552356),
 ( 1.000000000000000000, 1.000000000000000000) ) ) 
 REPRESENTATION_ITEM ( '' )  SURFACE ( )  );
#42015 = B_SPLINE_CURVE_WITH_KNOTS ( 'NONE', 3,
 ( #834, #197, #53442, #10551, #15566, #29648, #44102, #39388, #58439, #52215, #9310, #28411, #58748, #59688, #59998, #11799, #30876, #35611, #54979 ),
 .UNSPECIFIED., .F., .F.,
 ( 4, 3, 3, 3, 3, 3, 4 ),
 ( 9.813676791237319219E-18, 0.0002732106629380591793, 0.0004098138914053713121, 0.0005464171197651385582, 0.0006830203481512525134, 0.0008196235766963584288, 0.001011968216111141378 ),
 .UNSPECIFIED. ) ;
#42016 = CARTESIAN_POINT ( 'NONE',  ( -2.569797478183790229, 13.68441171582016125, -5.182550149005160200 ) ) ;
#42017 = ORIENTED_EDGE ( 'NONE', *, *, #12680, .F. ) ;
#42018 = ADVANCED_FACE ( 'NONE', ( #8112 ), #20403, .F. ) ;
#42019 = AXIS2_PLACEMENT_3D ( 'NONE', #15557, #34063, #43463 ) ;
#42020 = DIRECTION ( 'NONE',  ( -1.000000000000000000, -3.135800716341471541E-16, -1.298891185607920445E-16 ) ) ;
#42021 = CARTESIAN_POINT ( 'NONE',  ( 0.5827357941260206120, 46.35666768646135694, 12.04516435546818087 ) ) ;
#42022 = CARTESIAN_POINT ( 'NONE',  ( 4.962356264823608143, 0.000000000000000000, 0.000000000000000000 ) ) ;
#42023 = FACE_BOUND ( 'NONE', #43597, .T. ) ;
#42024 = EDGE_LOOP ( 'NONE', ( #3703, #54073, #11581, #50701 ) ) ;
#42025 = EDGE_CURVE ( 'NONE', #49335, #39339, #23233, .T. ) ;
#42026 = CARTESIAN_POINT ( 'NONE',  ( 0.8557997880470690211, 46.03118133706043835, -13.27832040216591380 ) ) ;
#42027 = FACE_OUTER_BOUND ( 'NONE', #47195, .T. ) ;
#42028 = EDGE_CURVE ( 'NONE', #45745, #44200, #28744, .T. ) ;
#42029 =( BOUNDED_SURFACE ( )  B_SPLINE_SURFACE ( 3, 1, ( 
 ( #45896, #27690 ),
 ( #46821, #61185 ),
 ( #51791, #22683 ),
 ( #27998, #47120 ) ),
 .UNSPECIFIED., .F., .F., .F. ) 
 B_SPLINE_SURFACE_WITH_KNOTS ( ( 4, 4 ),
 ( 2, 2 ),
 ( 0.000000000000000000, 1.000000000000000000 ),
 ( 0.000000000000000000, 1.000000000000000000 ),
 .UNSPECIFIED. ) 
 GEOMETRIC_REPRESENTATION_ITEM ( )  RATIONAL_B_SPLINE_SURFACE ( (
 ( 1.000000000000000000, 1.000000000000000000),
 ( 0.9751682680413298332, 0.9999560080971552356),
 ( 0.9751682680413298332, 0.9999560080971552356),
 ( 1.000000000000000000, 1.000000000000000000) ) ) 
 REPRESENTATION_ITEM ( '' )  SURFACE ( )  );
#42030 = VERTEX_POINT ( 'NONE', #47573 ) ;
#42031 = LINE ( 'NONE', #18205, #21022 ) ;
#42032 = CARTESIAN_POINT ( 'NONE',  ( 0.5806925824938506953, -46.06186276235258958, -8.804950948515241294 ) ) ;
#42033 = EDGE_CURVE ( 'NONE', #37323, #10433, #14072, .T. ) ;
#42034 = CARTESIAN_POINT ( 'NONE',  ( 0.7245667037590770576, 24.75815201345788807, 41.24129124474305286 ) ) ;
#42035 = EDGE_LOOP ( 'NONE', ( #6982, #61348, #18930, #34018 ) ) ;
#42036 = CARTESIAN_POINT ( 'NONE',  ( 5.880360259849739535, -39.86101557989688615, 26.69116321728503394 ) ) ;
#42037 = B_SPLINE_CURVE_WITH_KNOTS ( 'NONE', 3,
 ( #18613, #13005, #12691, #37743, #51478, #46506 ),
 .UNSPECIFIED., .F., .F.,
 ( 4, 2, 4 ),
 ( 1.275615807185303638E-16, 0.0002450741128632364621, 0.0004901482257263454221 ),
 .UNSPECIFIED. ) ;
#42038 = ORIENTED_EDGE ( 'NONE', *, *, #60436, .T. ) ;
#42039 = VERTEX_POINT ( 'NONE', #13442 ) ;
#42040 = CARTESIAN_POINT ( 'NONE',  ( 0.5834872094924171693, -6.026535573893806230, -47.51530820063773319 ) ) ;
#42041 = CARTESIAN_POINT ( 'NONE',  ( -4.915099999999999802, 0.000000000000000000, -3.000000000000000000 ) ) ;
#42042 = VERTEX_POINT ( 'NONE', #14686 ) ;
#42043 = CARTESIAN_POINT ( 'NONE',  ( 1.000433927950262758, 24.32662655438078048, -34.12673318875604878 ) ) ;
#42044 = VERTEX_POINT ( 'NONE', #47884 ) ;
#42045 = CARTESIAN_POINT ( 'NONE',  ( -2.569797478183783568, -13.68441171582012750, -5.182550149005254347 ) ) ;
#42046 = CARTESIAN_POINT ( 'NONE',  ( 1.227938101723748288, 15.63977281655842511, 39.96870412324341260 ) ) ;
#42047 = CARTESIAN_POINT ( 'NONE',  ( 4.975801465491694664, 47.84403947906843513, -2.564218696446985302 ) ) ;
#42048 = ADVANCED_FACE ( 'NONE', ( #23448 ), #24768, .F. ) ;
#42049 = ORIENTED_EDGE ( 'NONE', *, *, #3098, .F. ) ;
#42050 = FACE_OUTER_BOUND ( 'NONE', #56030, .T. ) ;
#42051 = CARTESIAN_POINT ( 'NONE',  ( -6.057079549204054558, -11.01026639367740501, 15.79890075416629713 ) ) ;
#42052 = CARTESIAN_POINT ( 'NONE',  ( 0.5837800005270546988, -44.30121660599532873, -15.38302525092088224 ) ) ;
#42053 = DIRECTION ( 'NONE',  ( -3.273063162220399693E-16, 1.000000000000000000, 1.047380211910527902E-14 ) ) ;
#42054 = EDGE_LOOP ( 'NONE', ( #8202, #19746, #17220, #27777, #16600, #60338 ) ) ;
#42055 = EDGE_CURVE ( 'NONE', #28087, #43207, #56707, .T. ) ;
#42056 = DIRECTION ( 'NONE',  ( 0.000000000000000000, 0.000000000000000000, 1.000000000000000000 ) ) ;
#42057 = CARTESIAN_POINT ( 'NONE',  ( 4.963659409799330291, 20.22157859941729896, 39.92545197189556916 ) ) ;
#42058 = ORIENTED_EDGE ( 'NONE', *, *, #5312, .F. ) ;
#42059 = CARTESIAN_POINT ( 'NONE',  ( 0.9757787079277449038, -42.90844198810271592, -0.03949005143946147239 ) ) ;
#42060 = EDGE_CURVE ( 'NONE', #50622, #31128, #2116, .T. ) ;
#42061 = EDGE_LOOP ( 'NONE', ( #28849, #29235, #43570, #51369 ) ) ;
#42062 = AXIS2_PLACEMENT_3D ( 'NONE', #22283, #60169, #54527 ) ;
#42063 = CARTESIAN_POINT ( 'NONE',  ( 0.1129192098497447394, -12.08918212651769686, 42.43587472053614817 ) ) ;
#42064 = CARTESIAN_POINT ( 'NONE',  ( 0.5997462898726536595, 46.76781179977627545, -14.97743000668059210 ) ) ;
#42065 = VERTEX_POINT ( 'NONE', #23757 ) ;
#42066 = CARTESIAN_POINT ( 'NONE',  ( 0.5824935313925946323, 5.056376536285211110, 46.62264721545897572 ) ) ;
#42067 = CARTESIAN_POINT ( 'NONE',  ( 0.3676999524040323597, 34.11874447325018167, -27.96179284115914854 ) ) ;
#42068 = CARTESIAN_POINT ( 'NONE',  ( 0.6029442701453591180, 28.16660832611681542, 40.22670009535214319 ) ) ;
#42069 = CARTESIAN_POINT ( 'NONE',  ( 0.5817217712918332229, -1.111903975787065235, -46.88281799931615268 ) ) ;
#42070 = B_SPLINE_CURVE_WITH_KNOTS ( 'NONE', 3,
 ( #7644, #3561, #54951, #51484, #36193, #8575, #3871, #50879, #59970, #26772, #55258, #31158, #45906, #50266, #27702, #41510, #2952, #41204, #37125 ),
 .UNSPECIFIED., .F., .F.,
 ( 4, 3, 3, 3, 3, 3, 4 ),
 ( 1.161956753697875813E-16, 0.0002618519381806248868, 0.0003927759815485977100, 0.0005237000248299422374, 0.0006546240681324978251, 0.0007855481115631330344, 0.0009699050456655102914 ),
 .UNSPECIFIED. ) ;
#42071 = CIRCLE ( 'NONE', #47068, 6.728125000000022560 ) ;
#42072 = VERTEX_POINT ( 'NONE', #51633 ) ;
#42073 = FACE_BOUND ( 'NONE', #56395, .T. ) ;
#42074 = CARTESIAN_POINT ( 'NONE',  ( 4.303969348037258058, -43.57722561725972099, 20.38638383586104652 ) ) ;
#42075 = CARTESIAN_POINT ( 'NONE',  ( 6.890143360408123030, -11.60930335864404306, -1.199999999999999956 ) ) ;
#42077 = EDGE_CURVE ( 'NONE', #331, #51504, #59777, .T. ) ;
#42076 = CARTESIAN_POINT ( 'NONE',  ( 3.270143674763207553, 7.080034332678258657, 11.71453292426881987 ) ) ;
#42078 = PLANE ( 'NONE',  #59313 ) ;
#42079 = CARTESIAN_POINT ( 'NONE',  ( 0.5263152470540294336, 0.000000000000000000, 8.000000000000000000 ) ) ;
#42080 = ADVANCED_FACE ( 'NONE', ( #42275 ), #14375, .F. ) ;
#42081 = CARTESIAN_POINT ( 'NONE',  ( 0.9722240741986377666, 39.86121768686908240, -15.88116971565344393 ) ) ;
#42082 = CARTESIAN_POINT ( 'NONE',  ( 0.8751705887134423323, 44.08562551107055327, 19.22545746485676688 ) ) ;
#42083 = CARTESIAN_POINT ( 'NONE',  ( 0.9784957157296367836, -12.19398871309499022, 40.09538248049621245 ) ) ;
#42084 = CARTESIAN_POINT ( 'NONE',  ( -2.601141883200662974, -11.02917173973125919, -10.05747474294128985 ) ) ;
#42085 = CARTESIAN_POINT ( 'NONE',  ( -6.063463321072278589, 5.494009911919311762, -18.45633516078428826 ) ) ;
#42086 = CARTESIAN_POINT ( 'NONE',  ( 0.8560838555295158248, 33.26091945577399400, -33.07694168205770069 ) ) ;
#42087 = CARTESIAN_POINT ( 'NONE',  ( 0.5997462898726536595, 17.44942740672471260, -45.90282249842328355 ) ) ;
#42088 = CARTESIAN_POINT ( 'NONE',  ( 0.9756008150404594792, 37.23069985082546651, 21.33101788548744082 ) ) ;
#42089 = CARTESIAN_POINT ( 'NONE',  ( 0.1365634738349401633, -31.24960441609707829, -31.15003761571876950 ) ) ;
#42090 = CARTESIAN_POINT ( 'NONE',  ( 0.5980894510889448457, -41.31170365136871681, -24.66136644716806359 ) ) ;
#42091 =( LENGTH_UNIT ( ) NAMED_UNIT ( * ) SI_UNIT ( .MILLI., .METRE. ) );
#42092 = CARTESIAN_POINT ( 'NONE',  ( 0.6025881611877910160, 46.52425620537270134, -12.24025891548874512 ) ) ;
#42094 = ORIENTED_EDGE ( 'NONE', *, *, #30280, .F. ) ;
#42093 = DIRECTION ( 'NONE',  ( 1.000000000000000000, 0.000000000000000000, 0.000000000000000000 ) ) ;
#42095 = ORIENTED_EDGE ( 'NONE', *, *, #22912, .F. ) ;
#42096 = DIRECTION ( 'NONE',  ( 1.836766033387207149E-16, -1.000000000000000000, 0.000000000000000000 ) ) ;
#42097 = CARTESIAN_POINT ( 'NONE',  ( 0.8560838555295158248, -39.18289055412748922, 25.78902716088759206 ) ) ;
#42098 = CARTESIAN_POINT ( 'NONE',  ( -2.739355103387248747, 9.839932234830028435, -11.22601000199848365 ) ) ;
#42099 = ORIENTED_EDGE ( 'NONE', *, *, #26726, .F. ) ;
#42100 = ADVANCED_FACE ( 'NONE', ( #57866 ), #52772, .F. ) ;
#42101 = ORIENTED_EDGE ( 'NONE', *, *, #59546, .T. ) ;
#42102 = DIRECTION ( 'NONE',  ( 0.09835009131224566048, -0.9876177374393984021, 0.1222230102474844704 ) ) ;
#42103 = CARTESIAN_POINT ( 'NONE',  ( 0.7044674535453004927, -39.85538961151615212, -28.69408722585818339 ) ) ;
#42104 = EDGE_CURVE ( 'NONE', #34503, #61620, #17915, .T. ) ;
#42106 = ORIENTED_EDGE ( 'NONE', *, *, #685, .T. ) ;
#42105 = VECTOR ( 'NONE', #58619, 1000.000000000000000 ) ;
#42107 = ORIENTED_EDGE ( 'NONE', *, *, #10409, .T. ) ;
#42108 = CARTESIAN_POINT ( 'NONE',  ( 0.9747592971366226822, -11.41797089479104521, -41.36145845824421485 ) ) ;
#42109 = EDGE_CURVE ( 'NONE', #9554, #26349, #25328, .T. ) ;
#42110 =( BOUNDED_SURFACE ( )  B_SPLINE_SURFACE ( 3, 1, ( 
 ( #24897, #57764 ),
 ( #44038, #1071 ),
 ( #20207, #43409 ),
 ( #52770, #445 ) ),
 .UNSPECIFIED., .F., .F., .F. ) 
 B_SPLINE_SURFACE_WITH_KNOTS ( ( 4, 4 ),
 ( 2, 2 ),
 ( 0.000000000000000000, 1.000000000000000000 ),
 ( 0.000000000000000000, 1.000000000000000000 ),
 .UNSPECIFIED. ) 
 GEOMETRIC_REPRESENTATION_ITEM ( )  RATIONAL_B_SPLINE_SURFACE ( (
 ( 1.000000000000000000, 1.000000000000000000),
 ( 0.7269869731126821222, 0.9931720237060910339),
 ( 0.7269869731126821222, 0.9931720237060910339),
 ( 1.000000000000000000, 1.000000000000000000) ) ) 
 REPRESENTATION_ITEM ( '' )  SURFACE ( )  );
#42111 = EDGE_CURVE ( 'NONE', #31002, #22293, #47759, .T. ) ;
#42112 = CARTESIAN_POINT ( 'NONE',  ( 0.5326698147273788431, 0.000000000000000000, 0.000000000000000000 ) ) ;
#42113 = CARTESIAN_POINT ( 'NONE',  ( 2.282803330402973785, 28.91046258521398116, -37.02272357034160422 ) ) ;
#42114 = B_SPLINE_CURVE_WITH_KNOTS ( 'NONE', 3,
 ( #21639, #59845, #35760, #7205 ),
 .UNSPECIFIED., .F., .F.,
 ( 4, 4 ),
 ( 0.000000000000000000, 0.005014147105413702989 ),
 .UNSPECIFIED. ) ;
#42115 = EDGE_CURVE ( 'NONE', #3613, #30211, #49106, .T. ) ;
#42116 = ORIENTED_EDGE ( 'NONE', *, *, #55151, .F. ) ;
#42117 = ORIENTED_EDGE ( 'NONE', *, *, #30370, .T. ) ;
#42118 = CARTESIAN_POINT ( 'NONE',  ( 0.5838002273316417190, -12.26477999444036548, -46.29900743592993706 ) ) ;
#42119 = VERTEX_POINT ( 'NONE', #53774 ) ;
#42120 = CARTESIAN_POINT ( 'NONE',  ( 4.553261556744875094, 22.57774691820428714, 37.68003330573307608 ) ) ;
#42121 = LINE ( 'NONE', #27679, #17092 ) ;
#42122 = CARTESIAN_POINT ( 'NONE',  ( 0.8751705887134423323, -46.21789262997747727, -13.30665218149346529 ) ) ;
#42123 = ORIENTED_EDGE ( 'NONE', *, *, #42109, .T. ) ;
#42124 = EDGE_CURVE ( 'NONE', #2726, #40574, #15606, .T. ) ;
#42125 = DIRECTION ( 'NONE',  ( -1.836909530733573776E-16, 1.000000000000000000, 0.000000000000000000 ) ) ;
#42126 = ORIENTED_EDGE ( 'NONE', *, *, #35502, .F. ) ;
#42127 = ORIENTED_EDGE ( 'NONE', *, *, #43872, .F. ) ;
#42128 = CARTESIAN_POINT ( 'NONE',  ( 0.9730545539215883499, -29.98130006528883129, 30.69604515769640329 ) ) ;
#42129 = EDGE_LOOP ( 'NONE', ( #44952, #55109, #46891, #31537 ) ) ;
#42130 = CARTESIAN_POINT ( 'NONE',  ( 2.185380717157382691, 34.44259825520901330, 27.43222973980556390 ) ) ;
#42131 = CARTESIAN_POINT ( 'NONE',  ( 3.238018933889920792, -1.956241471237834872, -13.25068344176488822 ) ) ;
#42132 = CARTESIAN_POINT ( 'NONE',  ( 3.660087539127315992, 39.22752134874918539, 27.72868323267822532 ) ) ;
#42133 = CARTESIAN_POINT ( 'NONE',  ( -6.078457390727109555, 12.00250936636376231, 15.05769836156436092 ) ) ;
#42134 = CARTESIAN_POINT ( 'NONE',  ( 1.834102595619085507, -43.83354038710950817, -4.338027430679048280 ) ) ;
#42135 =( BOUNDED_SURFACE ( )  B_SPLINE_SURFACE ( 3, 1, ( 
 ( #12306, #37049 ),
 ( #46747, #27005 ),
 ( #22004, #51723 ),
 ( #47057, #22616 ) ),
 .UNSPECIFIED., .F., .F., .F. ) 
 B_SPLINE_SURFACE_WITH_KNOTS ( ( 4, 4 ),
 ( 2, 2 ),
 ( 0.000000000000000000, 1.000000000000000000 ),
 ( 0.000000000000000000, 1.000000000000000000 ),
 .UNSPECIFIED. ) 
 GEOMETRIC_REPRESENTATION_ITEM ( )  RATIONAL_B_SPLINE_SURFACE ( (
 ( 1.000000000000000000, 1.000000000000000000),
 ( 0.7269869731126817891, 0.9931720237060910339),
 ( 0.7269869731126817891, 0.9931720237060910339),
 ( 1.000000000000000000, 1.000000000000000000) ) ) 
 REPRESENTATION_ITEM ( '' )  SURFACE ( )  );
#42136 = ORIENTED_EDGE ( 'NONE', *, *, #58185, .F. ) ;
#42137 = CARTESIAN_POINT ( 'NONE',  ( 4.960386119450151732, -40.46376651419630832, 16.64692356433904052 ) ) ;
#42138 = CARTESIAN_POINT ( 'NONE',  ( 4.967162193818130511, 23.56777426397228936, -36.06913038482774425 ) ) ;
#42139 = B_SPLINE_CURVE_WITH_KNOTS ( 'NONE', 3,
 ( #34412, #58795, #39743, #58183 ),
 .UNSPECIFIED., .F., .F.,
 ( 4, 4 ),
 ( 0.000000000000000000, 0.004446090762761313944 ),
 .UNSPECIFIED. ) ;
#42140 = CARTESIAN_POINT ( 'NONE',  ( 0.1100053167205930216, 39.77279469894213548, -16.66867746965606045 ) ) ;
#42141 = B_SPLINE_CURVE_WITH_KNOTS ( 'NONE', 3,
 ( #33590, #52980, #5354, #41, #4117, #61436 ),
 .UNSPECIFIED., .F., .F.,
 ( 4, 2, 4 ),
 ( 8.541065402288461036E-17, 0.0002293366620881447679, 0.0004586733241762041549 ),
 .UNSPECIFIED. ) ;
#42142 = ORIENTED_EDGE ( 'NONE', *, *, #41951, .T. ) ;
#42143 = CARTESIAN_POINT ( 'NONE',  ( 0.2279481005628774537, 15.94756160462533501, -41.13610051936851164 ) ) ;
#42144 = CARTESIAN_POINT ( 'NONE',  ( -5.995132425357893702, 13.31880955509727293, 13.33084941932912137 ) ) ;
#42145 = CARTESIAN_POINT ( 'NONE',  ( 0.9736507210033066295, 30.02062799605199572, 30.65767007549924372 ) ) ;
#42146 = ORIENTED_EDGE ( 'NONE', *, *, #14704, .F. ) ;
#42147 = CARTESIAN_POINT ( 'NONE',  ( 0.1365634738349410515, 19.84198381844869274, 39.41012938029597024 ) ) ;
#42148 = CARTESIAN_POINT ( 'NONE',  ( 4.956653778116970166, 39.67974989265038488, 27.17045123668485829 ) ) ;
#42149 = CARTESIAN_POINT ( 'NONE',  ( 4.956445790444006683, -23.10347171912805564, -41.03373788315033721 ) ) ;
#42150 = CARTESIAN_POINT ( 'NONE',  ( 3.407937589446174087, 8.699069120706923286, -10.58239600294629668 ) ) ;
#42151 = CARTESIAN_POINT ( 'NONE',  ( 0.1156867017252034557, -17.74639720403204990, -40.39812116363717820 ) ) ;
#42152 = CARTESIAN_POINT ( 'NONE',  ( 0.6021447746440204973, -42.65942225007028554, 24.32518925679092092 ) ) ;
#42153 = CIRCLE ( 'NONE', #104, 0.02570000000000176310 ) ;
#42154 = CARTESIAN_POINT ( 'NONE',  ( 0.9756950546413931669, 42.90834738653779823, -0.09673755062811521810 ) ) ;
#42155 = EDGE_CURVE ( 'NONE', #42953, #6465, #45765, .T. ) ;
#42156 = CARTESIAN_POINT ( 'NONE',  ( -6.079354080745853928, -8.905595498587096870, -17.07288271100423316 ) ) ;
#42157 = CARTESIAN_POINT ( 'NONE',  ( 0.5998501479064708430, -46.33007877220729398, -12.95623334615486222 ) ) ;
#42158 = CARTESIAN_POINT ( 'NONE',  ( 0.9790320750461913857, -1.314454984195479570, -41.88805725546019687 ) ) ;
#42159 = CARTESIAN_POINT ( 'NONE',  ( 4.975801465491695552, -47.84403947906842092, -2.564218696447329027 ) ) ;
#42160 = ORIENTED_EDGE ( 'NONE', *, *, #35886, .T. ) ;
#42161 = B_SPLINE_CURVE_WITH_KNOTS ( 'NONE', 3,
 ( #41880, #32778, #47184, #4230, #50930, #37805, #12434, #31527, #7704, #37176, #3306, #22439, #41564, #146, #57157, #47486, #4534, #19293, #48401 ),
 .UNSPECIFIED., .F., .F.,
 ( 4, 3, 3, 3, 3, 3, 4 ),
 ( 1.355252715606880543E-20, 0.0002612768053151737690, 0.0003919133833142954791, 0.0005225499612322595609, 0.0006531865391693357416, 0.0008112755173415181226, 0.0009693688056799743078 ),
 .UNSPECIFIED. ) ;
#42162 = CARTESIAN_POINT ( 'NONE',  ( -3.319141568766058814, -12.31039395171775830, -1.199999999999999956 ) ) ;
#42163 = CARTESIAN_POINT ( 'NONE',  ( 0.8751705887134553219, -11.58504748649232496, 46.67919521768867241 ) ) ;
#42164 = CARTESIAN_POINT ( 'NONE',  ( 0.1149546198390367924, -35.19724927890863597, -26.61015235246850352 ) ) ;
#42165 = CARTESIAN_POINT ( 'NONE',  ( -6.016761891674564211, 14.95139917749704495, 11.46828378093564460 ) ) ;
#42166 = CARTESIAN_POINT ( 'NONE',  ( 3.661933894777866350, 20.93652954769201813, 42.12235624285840885 ) ) ;
#42167 = CARTESIAN_POINT ( 'NONE',  ( 0.1087620492084205859, 42.70684898916388761, 5.987629195157958328 ) ) ;
#42168 = CARTESIAN_POINT ( 'NONE',  ( 0.5806925824938502512, -24.77160101449099727, 39.81946942793729249 ) ) ;
#42169 = CARTESIAN_POINT ( 'NONE',  ( 0.8751705887134423323, -34.63284514348608667, 33.37254303619495488 ) ) ;
#42170 = CARTESIAN_POINT ( 'NONE',  ( -6.078726893082806448, 16.77980020642716141, -9.446287434813061878 ) ) ;
#42172 = ORIENTED_EDGE ( 'NONE', *, *, #60209, .T. ) ;
#42171 = LINE ( 'NONE', #122, #11320 ) ;
#42173 = ORIENTED_EDGE ( 'NONE', *, *, #52815, .F. ) ;
#42174 = CARTESIAN_POINT ( 'NONE',  ( -2.099999999999999645, 2.571758278209440971E-16, -5.599999999999999645 ) ) ;
#42175 = CARTESIAN_POINT ( 'NONE',  ( -6.078075953587585900, 3.078503442539607615, -19.00836633699508482 ) ) ;
#42176 = CARTESIAN_POINT ( 'NONE',  ( 0.8557997880470599172, 17.48760788519217257, 44.60232077416692675 ) ) ;
#42177 = ORIENTED_EDGE ( 'NONE', *, *, #505, .F. ) ;
#42178 = CARTESIAN_POINT ( 'NONE',  ( 0.6026112563231247332, 11.09715715893446841, -47.83716231021774234 ) ) ;
#42179 = CARTESIAN_POINT ( 'NONE',  ( 0.6000166863083090663, -8.353387137038088994, -48.39467331274403961 ) ) ;
#42180 = CARTESIAN_POINT ( 'NONE',  ( 0.6029303876144825880, -44.39523326884624765, -18.53079182983329432 ) ) ;
#42181 = EDGE_CURVE ( 'NONE', #42423, #17824, #16338, .T. ) ;
#42182 = EDGE_LOOP ( 'NONE', ( #57376, #11992, #43849, #1384 ) ) ;
#42183 = ORIENTED_EDGE ( 'NONE', *, *, #27732, .T. ) ;
#42184 = ADVANCED_FACE ( 'NONE', ( #34104 ), #39629, .F. ) ;
#42185 = DIRECTION ( 'NONE',  ( 0.07439287786467665975, 0.9161872986448671430, 0.3937848822959463813 ) ) ;
#42186 = ADVANCED_FACE ( 'NONE', ( #25001 ), #46038, .F. ) ;
#42187 = DIRECTION ( 'NONE',  ( -1.000000000000000000, -1.836909530733580185E-16, 1.836909530733574022E-16 ) ) ;
#42188 = CARTESIAN_POINT ( 'NONE',  ( 0.9789889208857682767, 32.83019349609273974, -26.04828771822593936 ) ) ;
#42189 = EDGE_CURVE ( 'NONE', #48274, #8195, #27549, .T. ) ;
#42190 = CARTESIAN_POINT ( 'NONE',  ( -6.015611763856276717, 13.31979030221799398, 13.32857883366838081 ) ) ;
#42191 = CARTESIAN_POINT ( 'NONE',  ( 0.8751705887134423323, -23.27176129838396790, -42.09020928323367627 ) ) ;
#42192 = CIRCLE ( 'NONE', #49180, 48.09070567114147110 ) ;
#42193 = AXIS2_PLACEMENT_3D ( 'NONE', #28805, #29113, #47301 ) ;
#42194 = CARTESIAN_POINT ( 'NONE',  ( 0.7242003506640006805, -24.75021972573795992, 42.40799803873931495 ) ) ;
#42195 = ORIENTED_EDGE ( 'NONE', *, *, #15052, .T. ) ;
#42196 = CARTESIAN_POINT ( 'NONE',  ( 2.282803330402968012, -33.94297585900464043, -32.47108401781518694 ) ) ;
#42197 = EDGE_CURVE ( 'NONE', #40188, #25455, #10356, .T. ) ;
#42198 = VERTEX_POINT ( 'NONE', #39736 ) ;
#42199 = CARTESIAN_POINT ( 'NONE',  ( 0.6039202388192952409, -7.665580222076482819, -48.50569649750325851 ) ) ;
#42200 = CARTESIAN_POINT ( 'NONE',  ( 4.962356264823608143, 23.01169039590672938, -35.23773124060741679 ) ) ;
#42201 = CARTESIAN_POINT ( 'NONE',  ( 0.3676999524040323597, -34.85286720109652947, -27.04123205746306979 ) ) ;
#42202 = ADVANCED_FACE ( 'NONE', ( #36260 ), #36567, .T. ) ;
#42203 = B_SPLINE_CURVE_WITH_KNOTS ( 'NONE', 3,
 ( #19748, #15053, #34159, #49165, #44499, #25054 ),
 .UNSPECIFIED., .F., .F.,
 ( 4, 2, 4 ),
 ( 1.738108305489988542E-18, 0.0002291966416970788616, 0.0004583932833941559886 ),
 .UNSPECIFIED. ) ;
#42204 = ORIENTED_EDGE ( 'NONE', *, *, #38809, .T. ) ;
#42205 = ORIENTED_EDGE ( 'NONE', *, *, #10072, .F. ) ;
#42206 = CARTESIAN_POINT ( 'NONE',  ( 0.1129192098497455998, -44.12161472487017733, -0.4846667466135657909 ) ) ;
#42207 = DIRECTION ( 'NONE',  ( 0.000000000000000000, 0.000000000000000000, 1.000000000000000000 ) ) ;
#42208 = CARTESIAN_POINT ( 'NONE',  ( 0.6000166863083106206, 17.45040302316584757, 45.90541270958728148 ) ) ;
#42209 =( BOUNDED_SURFACE ( )  B_SPLINE_SURFACE ( 3, 1, ( 
 ( #26710, #51123 ),
 ( #8516, #12640 ),
 ( #50820, #13248 ),
 ( #32352, #31417 ) ),
 .UNSPECIFIED., .F., .F., .F. ) 
 B_SPLINE_SURFACE_WITH_KNOTS ( ( 4, 4 ),
 ( 2, 2 ),
 ( 0.000000000000000000, 1.000000000000000000 ),
 ( 0.000000000000000000, 1.000000000000000000 ),
 .UNSPECIFIED. ) 
 GEOMETRIC_REPRESENTATION_ITEM ( )  RATIONAL_B_SPLINE_SURFACE ( (
 ( 1.000000000000000000, 1.000000000000000000),
 ( 0.7223157951917480446, 0.9931996967497186413),
 ( 0.7223157951917480446, 0.9931996967497186413),
 ( 1.000000000000000000, 1.000000000000000000) ) ) 
 REPRESENTATION_ITEM ( '' )  SURFACE ( )  );
#42210 = VERTEX_POINT ( 'NONE', #21215 ) ;
#42211 = CARTESIAN_POINT ( 'NONE',  ( 2.624215991343608501, 30.33228621715088380, -37.21129343241572229 ) ) ;
#42212 = ORIENTED_EDGE ( 'NONE', *, *, #16443, .F. ) ;
#42213 = CARTESIAN_POINT ( 'NONE',  ( 2.706805983486679779, 43.48315593847570426, 6.781685848663358662 ) ) ;
#42214 = CARTESIAN_POINT ( 'NONE',  ( 4.960386119450151732, -43.29863790797077883, -6.297969513007882547 ) ) ;
#42215 = CARTESIAN_POINT ( 'NONE',  ( 0.5987334308729320709, 33.46066835468740663, 35.94365840906223752 ) ) ;
#42216 = VERTEX_POINT ( 'NONE', #21837 ) ;
#42217 = DIRECTION ( 'NONE',  ( -0.000000000000000000, -1.000000000000000000, -0.000000000000000000 ) ) ;
#42218 = CARTESIAN_POINT ( 'NONE',  ( 0.1135584504625007374, -27.84745193548719655, 34.22676544513054608 ) ) ;
#42219 = CARTESIAN_POINT ( 'NONE',  ( 1.231276596079881047, -26.41281459480337546, -32.55211200826465756 ) ) ;
#42220 = VERTEX_POINT ( 'NONE', #50329 ) ;
#42221 = CARTESIAN_POINT ( 'NONE',  ( 0.2285344041767061740, 24.61438786917755905, -36.61465662984072367 ) ) ;
#42222 = CARTESIAN_POINT ( 'NONE',  ( 5.000000000000012434, -80.00000000000001421, -1.569632904675596344E-31 ) ) ;
#42223 = CARTESIAN_POINT ( 'NONE',  ( 0.6023143664670691511, 47.72938193173972365, -6.019611522082831456 ) ) ;
#42224 = EDGE_CURVE ( 'NONE', #12597, #22992, #51495, .T. ) ;
#42225 = DIRECTION ( 'NONE',  ( 1.000000000000000000, 0.000000000000000000, 0.000000000000000000 ) ) ;
#42226 = ORIENTED_EDGE ( 'NONE', *, *, #20397, .T. ) ;
#42227 = FACE_OUTER_BOUND ( 'NONE', #61398, .T. ) ;
#42228 = CARTESIAN_POINT ( 'NONE',  ( 6.189768672337906175, 1.091423221261470733, -2.362915713819767774E-16 ) ) ;
#42229 = ORIENTED_EDGE ( 'NONE', *, *, #44103, .T. ) ;
#42230 = B_SPLINE_CURVE_WITH_KNOTS ( 'NONE', 3,
 ( #3164, #22292, #11991, #11661 ),
 .UNSPECIFIED., .F., .F.,
 ( 4, 4 ),
 ( 0.000000000000000000, 0.004445488388166994251 ),
 .UNSPECIFIED. ) ;
#42231 = FACE_OUTER_BOUND ( 'NONE', #38578, .T. ) ;
#42232 = DIRECTION ( 'NONE',  ( 0.1024043820194936449, 0.7811075516170125077, -0.6159418278945518743 ) ) ;
#42233 = CARTESIAN_POINT ( 'NONE',  ( 0.8744876279028263033, -26.20733431478184983, 41.51536677536103070 ) ) ;
#42234 = CARTESIAN_POINT ( 'NONE',  ( 5.894904586330512508, -17.30581086051421025, 10.24882054295766842 ) ) ;
#42235 = CARTESIAN_POINT ( 'NONE',  ( 4.549368137175248350, 3.018832571116558672, -42.82045902618769873 ) ) ;
#42236 = CARTESIAN_POINT ( 'NONE',  ( 0.5998501479064708430, -11.94461217097437000, -46.60114184914313995 ) ) ;
#42237 = AXIS2_PLACEMENT_3D ( 'NONE', #31863, #7723, #35338 ) ;
#42238 = CARTESIAN_POINT ( 'NONE',  ( 5.959547316686252039, 18.96456592444100053, -7.851524054666214170 ) ) ;
#42239 = CARTESIAN_POINT ( 'NONE',  ( 0.9722240741986377666, -41.59310805473376860, 10.54237114526869412 ) ) ;
#42240 = CIRCLE ( 'NONE', #9202, 47.09074272231896430 ) ;
#42241 = CARTESIAN_POINT ( 'NONE',  ( 4.967162193818130511, 0.000000000000000000, 0.000000000000000000 ) ) ;
#42242 = CARTESIAN_POINT ( 'NONE',  ( 3.270143674763207553, -10.69018354892893718, 8.548517033725214986 ) ) ;
#42243 = CARTESIAN_POINT ( 'NONE',  ( 0.8760168074887076939, 23.27577685234598093, -42.09738177923931346 ) ) ;
#42244 = ORIENTED_EDGE ( 'NONE', *, *, #1677, .T. ) ;
#42245 = CARTESIAN_POINT ( 'NONE',  ( 0.9730545539215892381, -15.95224156741857691, 39.83279466599033469 ) ) ;
#42246 = CARTESIAN_POINT ( 'NONE',  ( 47.85000000000000853, 15.50000000000000711, -0.1749776157412613053 ) ) ;
#42247 = B_SPLINE_CURVE_WITH_KNOTS ( 'NONE', 3,
 ( #27622, #37984, #52342, #32025, #9432, #41748 ),
 .UNSPECIFIED., .F., .F.,
 ( 4, 2, 4 ),
 ( 1.710438460654249876E-17, 0.0002293319059085089241, 0.0004586638118170007720 ),
 .UNSPECIFIED. ) ;
#42248 = DIRECTION ( 'NONE',  ( -1.000000000000000000, -0.000000000000000000, -0.000000000000000000 ) ) ;
#42249 = CARTESIAN_POINT ( 'NONE',  ( 0.5824935313925957425, 46.52475397494940523, 5.889435000427824640 ) ) ;
#42250 = CARTESIAN_POINT ( 'NONE',  ( 3.894904216938898323, 31.98519698887119489, -30.15081269318135782 ) ) ;
#42251 = B_SPLINE_CURVE_WITH_KNOTS ( 'NONE', 3,
 ( #25079, #10376, #44225, #40444 ),
 .UNSPECIFIED., .F., .F.,
 ( 4, 4 ),
 ( 2.043828937333572736E-17, 0.004444306975806115029 ),
 .UNSPECIFIED. ) ;
#42252 = EDGE_LOOP ( 'NONE', ( #3547, #53673, #44823, #30156, #20130, #39886 ) ) ;
#42253 = B_SPLINE_CURVE_WITH_KNOTS ( 'NONE', 3,
 ( #31481, #50577, #26784, #60275, #22391, #13019, #47440, #52121, #23940, #32732, #5109, #43064, #42152, #19252, #42450, #8913 ),
 .UNSPECIFIED., .F., .F.,
 ( 4, 3, 3, 3, 3, 4 ),
 ( 1.868480190406682863E-17, 0.0002612764279487752770, 0.0003919131003184815219, 0.0005225497727000692674, 0.0007837925190632515342, 0.001045051706266716084 ),
 .UNSPECIFIED. ) ;
#42254 = EDGE_CURVE ( 'NONE', #50038, #30020, #5675, .T. ) ;
#42255 = CARTESIAN_POINT ( 'NONE',  ( 1.088313998177385278, -29.78798111128807236, -30.89087247895961852 ) ) ;
#42256 = CARTESIAN_POINT ( 'NONE',  ( 2.643462169533600914, 30.32726672320799821, -37.25264019563384466 ) ) ;
#42257 = CARTESIAN_POINT ( 'NONE',  ( 1.834102595619085507, 28.63582846592697351, -33.46919588110372956 ) ) ;
#42258 = CARTESIAN_POINT ( 'NONE',  ( -18.52588630790603474, -7.735090112546274099, -2.044527905409440294 ) ) ;
#42259 = ORIENTED_EDGE ( 'NONE', *, *, #58693, .F. ) ;
#42260 = EDGE_CURVE ( 'NONE', #21937, #26819, #55325, .T. ) ;
#42261 = CARTESIAN_POINT ( 'NONE',  ( 4.967162193818129623, -18.65818244221285127, 38.83676580803761169 ) ) ;
#42262 = CARTESIAN_POINT ( 'NONE',  ( 1.227938101723748288, 42.65467462194924764, -4.762198645644009076 ) ) ;
#42263 = EDGE_LOOP ( 'NONE', ( #39592, #13008, #16683, #42322, #2811 ) ) ;
#42264 = CARTESIAN_POINT ( 'NONE',  ( 3.050102900204245682, -25.99102862069139519, 35.49495288652262559 ) ) ;
#42265 = EDGE_LOOP ( 'NONE', ( #59023, #18431, #20129, #402 ) ) ;
#42266 = CARTESIAN_POINT ( 'NONE',  ( -6.016761891674565099, -11.46828378093549361, -14.95139917749716041 ) ) ;
#42267 = CARTESIAN_POINT ( 'NONE',  ( 0.5809828226811617480, 6.791453954331010401, -47.41188724015871969 ) ) ;
#42268 = ORIENTED_EDGE ( 'NONE', *, *, #1626, .F. ) ;
#42269 = CARTESIAN_POINT ( 'NONE',  ( 0.8753041380234524160, 3.828530797421371812, -48.95386276695819561 ) ) ;
#42270 = CARTESIAN_POINT ( 'NONE',  ( 0.1100247026804066219, 26.11768802553199365, 34.31594964380191470 ) ) ;
#42271 = ORIENTED_EDGE ( 'NONE', *, *, #33136, .F. ) ;
#42272 = CARTESIAN_POINT ( 'NONE',  ( 0.5837800005270550319, -7.800213544018094858, -46.24274999726447533 ) ) ;
#42273 = EDGE_CURVE ( 'NONE', #37705, #20429, #47748, .T. ) ;
#42274 = EDGE_LOOP ( 'NONE', ( #29963, #57699, #5440, #58577 ) ) ;
#42275 = FACE_OUTER_BOUND ( 'NONE', #57721, .T. ) ;
#42276 = VERTEX_POINT ( 'NONE', #26528 ) ;
#42277 = CARTESIAN_POINT ( 'NONE',  ( 0.8753041380234471980, -45.84117188851855929, 17.59901382919725066 ) ) ;
#42278 = B_SPLINE_CURVE_WITH_KNOTS ( 'NONE', 3,
 ( #27895, #8781, #23813, #27582, #8162, #57001 ),
 .UNSPECIFIED., .F., .F.,
 ( 4, 2, 4 ),
 ( 1.843143693225357538E-18, 0.0002447193893791693828, 0.0004894387787583369225 ),
 .UNSPECIFIED. ) ;
#42279 = ORIENTED_EDGE ( 'NONE', *, *, #46624, .T. ) ;
#42280 = ORIENTED_EDGE ( 'NONE', *, *, #45139, .T. ) ;
#42281 = CARTESIAN_POINT ( 'NONE',  ( 0.9762797500689124330, 28.76866969768027715, -30.47438972336406238 ) ) ;
#42282 = CARTESIAN_POINT ( 'NONE',  ( 0.5807400328401637335, 47.55718917606851193, -5.711437504335475701 ) ) ;
#42283 = CARTESIAN_POINT ( 'NONE',  ( 0.000000000000000000, 0.000000000000000000, 0.000000000000000000 ) ) ;
#42284 = CARTESIAN_POINT ( 'NONE',  ( 2.528100132419516033, 41.42605997219556002, -6.792299596759092672 ) ) ;
#42285 = ORIENTED_EDGE ( 'NONE', *, *, #59321, .F. ) ;
#42286 = CARTESIAN_POINT ( 'NONE',  ( 0.9757898596046642448, 0.02632670903343587582, -42.90845459940354090 ) ) ;
#42287 = CARTESIAN_POINT ( 'NONE',  ( 5.894904586330512508, -19.39796360309183498, 5.314924281188501354 ) ) ;
#42288 = CARTESIAN_POINT ( 'NONE',  ( 4.553261556744875094, 1.182159483579356074, 43.91061448874314976 ) ) ;
#42289 = ORIENTED_EDGE ( 'NONE', *, *, #59918, .T. ) ;
#42290 = ORIENTED_EDGE ( 'NONE', *, *, #5069, .F. ) ;
#42291 = CARTESIAN_POINT ( 'NONE',  ( -6.016761891674564211, -2.462934516563682230, -18.68153697670644320 ) ) ;
#42292 = CARTESIAN_POINT ( 'NONE',  ( 20.55500000000001748, 0.000000000000000000, 0.000000000000000000 ) ) ;
#42293 = CARTESIAN_POINT ( 'NONE',  ( 5.965394784446458765, -5.298374383010773236, 19.82972329408676515 ) ) ;
#42294 = EDGE_CURVE ( 'NONE', #44566, #51524, #18743, .T. ) ;
#42295 = CARTESIAN_POINT ( 'NONE',  ( 0.1081432562775999084, -34.46918062033768138, 25.91533557232832408 ) ) ;
#42296 = B_SPLINE_CURVE_WITH_KNOTS ( 'NONE', 3,
 ( #41226, #17398, #2977, #60286, #36521, #55587 ),
 .UNSPECIFIED., .F., .F.,
 ( 4, 2, 4 ),
 ( 6.149443329761889321E-18, 0.0002445244328975372940, 0.0004890488657950685164 ),
 .UNSPECIFIED. ) ;
#42297 = DIRECTION ( 'NONE',  ( -1.000000000000000000, -5.380183451256491399E-17, -1.298891185607892835E-16 ) ) ;
#42298 = B_SPLINE_CURVE_WITH_KNOTS ( 'NONE', 3,
 ( #60324, #12145, #50936, #41265 ),
 .UNSPECIFIED., .F., .F.,
 ( 4, 4 ),
 ( 8.673617379884035472E-19, 0.004048833967417089091 ),
 .UNSPECIFIED. ) ;
#42299 = ORIENTED_EDGE ( 'NONE', *, *, #21660, .T. ) ;
#42300 = FACE_OUTER_BOUND ( 'NONE', #59881, .T. ) ;
#42301 = CARTESIAN_POINT ( 'NONE',  ( 0.9790320750461924959, -41.08593480789065211, 8.263358488166169025 ) ) ;
#42302 = CARTESIAN_POINT ( 'NONE',  ( 3.894904216938897878, -39.34215491042563428, -19.60406028046930516 ) ) ;
#42303 = CARTESIAN_POINT ( 'NONE',  ( 2.185380717157383135, -41.33206684581055157, -15.18156952757675349 ) ) ;
#42304 = ADVANCED_FACE ( 'NONE', ( #11843, #45655 ), #26213, .F. ) ;
#42305 = FILL_AREA_STYLE ('',( #41687 ) ) ;
#42306 = LINE ( 'NONE', #24099, #52823 ) ;
#42307 = ORIENTED_EDGE ( 'NONE', *, *, #35553, .F. ) ;
#42308 = CARTESIAN_POINT ( 'NONE',  ( 0.6000166863083106206, 48.97316450298206547, 3.667784109283283911 ) ) ;
#42309 = CARTESIAN_POINT ( 'NONE',  ( 3.376099380956842921, 11.29282810595550934, -7.223601387217343905 ) ) ;
#42310 = ADVANCED_FACE ( 'NONE', ( #2402 ), #52397, .F. ) ;
#42311 = CARTESIAN_POINT ( 'NONE',  ( -6.079354080745853928, 3.072100940895990284, -19.00934378291655236 ) ) ;
#42312 = DIRECTION ( 'NONE',  ( 0.000000000000000000, -0.5000000000000009992, -0.8660254037844380415 ) ) ;
#42313 = CARTESIAN_POINT ( 'NONE',  ( 0.5850706913938534814, 18.16120156791940943, -44.31965802246087094 ) ) ;
#42314 = CARTESIAN_POINT ( 'NONE',  ( 2.301529144917014769, -43.86846428170474610, 19.56451384728966403 ) ) ;
#42315 = CARTESIAN_POINT ( 'NONE',  ( 0.6029443449137434907, -49.10740925637109200, -0.04352138108543880668 ) ) ;
#42316 = CARTESIAN_POINT ( 'NONE',  ( 0.5837157313716024865, 22.61716662562863789, -41.08163625527314622 ) ) ;
#42317 = B_SPLINE_CURVE_WITH_KNOTS ( 'NONE', 3,
 ( #37271, #24616, #800, #43127, #29307, #52800, #5780, #18153, #29005, #38740, #32563, #48119, #8415, #44069, #5172, #51641 ),
 .UNSPECIFIED., .F., .F.,
 ( 4, 3, 3, 3, 3, 4 ),
 ( 1.250973872328959318E-17, 0.0002724568934985619980, 0.0004086836638483865437, 0.0005449104342063674881, 0.0008173270854453680827, 0.001089761613562689659 ),
 .UNSPECIFIED. ) ;
#42318 = AXIS2_PLACEMENT_3D ( 'NONE', #6317, #15769, #44597 ) ;
#42319 =( BOUNDED_SURFACE ( )  B_SPLINE_SURFACE ( 3, 1, ( 
 ( #14152, #25005 ),
 ( #44144, #42650 ),
 ( #29686, #22925 ),
 ( #58181, #18526 ) ),
 .UNSPECIFIED., .F., .F., .F. ) 
 B_SPLINE_SURFACE_WITH_KNOTS ( ( 4, 4 ),
 ( 2, 2 ),
 ( 0.000000000000000000, 1.000000000000000000 ),
 ( 0.000000000000000000, 1.000000000000000000 ),
 .UNSPECIFIED. ) 
 GEOMETRIC_REPRESENTATION_ITEM ( )  RATIONAL_B_SPLINE_SURFACE ( (
 ( 1.000000000000000000, 1.000000000000000000),
 ( 0.7211978278499968642, 0.9934217856018975334),
 ( 0.7211978278499968642, 0.9934217856018975334),
 ( 1.000000000000000000, 1.000000000000000000) ) ) 
 REPRESENTATION_ITEM ( '' )  SURFACE ( )  );
#42320 = EDGE_CURVE ( 'NONE', #1177, #47186, #35957, .T. ) ;
#42321 = CARTESIAN_POINT ( 'NONE',  ( 4.553261556744873317, -41.75933753256789771, -13.62707946203816967 ) ) ;
#42322 = ORIENTED_EDGE ( 'NONE', *, *, #48978, .T. ) ;
#42323 = CARTESIAN_POINT ( 'NONE',  ( 0.000000000000000000, -1.178949249685218748, -2.041999999999998039 ) ) ;
#42324 = CARTESIAN_POINT ( 'NONE',  ( 0.9790320750461907195, 20.06511352880068344, 36.79304759894904464 ) ) ;
#42325 = CARTESIAN_POINT ( 'NONE',  ( 0.8751705887134553219, 5.393078191592700854, -47.79200036674274088 ) ) ;
#42326 = DIRECTION ( 'NONE',  ( 0.000000000000000000, -0.000000000000000000, 1.000000000000000000 ) ) ;
#42327 = ORIENTED_EDGE ( 'NONE', *, *, #53867, .F. ) ;
#42328 = ADVANCED_FACE ( 'NONE', ( #60638 ), #3182, .F. ) ;
#42329 = CARTESIAN_POINT ( 'NONE',  ( 0.8760168074886960365, -11.58706983520293754, -46.68716261866172346 ) ) ;
#42330 = CARTESIAN_POINT ( 'NONE',  ( 0.6027444965799114707, 44.30076917591773622, -21.18915680978122751 ) ) ;
#42331 = EDGE_CURVE ( 'NONE', #9726, #20133, #17749, .T. ) ;
#42332 = EDGE_LOOP ( 'NONE', ( #23608, #49252, #33770, #30363 ) ) ;
#42333 = DIRECTION ( 'NONE',  ( -1.000000000000000000, -0.000000000000000000, -0.000000000000000000 ) ) ;
#42334 = AXIS2_PLACEMENT_3D ( 'NONE', #51148, #8233, #60854 ) ;
#42335 = CARTESIAN_POINT ( 'NONE',  ( 4.975610109902397937, 35.53430708602537891, 33.61193875773635398 ) ) ;
#42336 = DIRECTION ( 'NONE',  ( 0.000000000000000000, 0.000000000000000000, 1.000000000000000000 ) ) ;
#42337 = ORIENTED_EDGE ( 'NONE', *, *, #50283, .T. ) ;
#42338 = FACE_OUTER_BOUND ( 'NONE', #49816, .T. ) ;
#42339 = ORIENTED_EDGE ( 'NONE', *, *, #33765, .T. ) ;
#42340 = ORIENTED_EDGE ( 'NONE', *, *, #55612, .F. ) ;
#42341 = CARTESIAN_POINT ( 'NONE',  ( 4.553261556744873317, 22.96401893593727550, 37.44587293859699173 ) ) ;
#42342 = CARTESIAN_POINT ( 'NONE',  ( 1.227938101723748288, -15.63977281655813023, -39.96870412324352628 ) ) ;
#42343 = ORIENTED_EDGE ( 'NONE', *, *, #15164, .F. ) ;
#42344 = CARTESIAN_POINT ( 'NONE',  ( 0.5807400328401574052, -0.5448834511093306743, 47.89582301953903709 ) ) ;
#42345 = EDGE_CURVE ( 'NONE', #36881, #46133, #19352, .T. ) ;
#42346 = ORIENTED_EDGE ( 'NONE', *, *, #13686, .F. ) ;
#42347 = CARTESIAN_POINT ( 'NONE',  ( 5.965394784446458765, 16.27505370423081388, -12.50653125158990697 ) ) ;
#42348 = DIRECTION ( 'NONE',  ( 0.1011922191286468153, 0.8267003359790527917, -0.5534678755627476798 ) ) ;
#42349 = CARTESIAN_POINT ( 'NONE',  ( 0.6031356755852232965, -8.546889681428286551E-06, -48.10744332413860747 ) ) ;
#42350 = VERTEX_POINT ( 'NONE', #42506 ) ;
#42351 = CARTESIAN_POINT ( 'NONE',  ( 8.000000000000007105, -58.44237546506844438, 54.69470952477916370 ) ) ;
#42352 = CARTESIAN_POINT ( 'NONE',  ( -6.078726893082806448, -14.66019907464893635, -12.48489504803234418 ) ) ;
#42353 = CARTESIAN_POINT ( 'NONE',  ( 1.231276596079887264, 15.85305549123172320, 38.80666698661448777 ) ) ;
#42354 = CARTESIAN_POINT ( 'NONE',  ( 0.5987334308729319599, 27.59677667583599714, -40.61995597823517556 ) ) ;
#42355 = ORIENTED_EDGE ( 'NONE', *, *, #16014, .T. ) ;
#42356 = LINE ( 'NONE', #4700, #53755 ) ;
#42357 = B_SPLINE_CURVE_WITH_KNOTS ( 'NONE', 3,
 ( #29797, #1276, #35763, #40169 ),
 .UNSPECIFIED., .F., .F.,
 ( 4, 4 ),
 ( 0.000000000000000000, 0.005014147105413700387 ),
 .UNSPECIFIED. ) ;
#42358 = ORIENTED_EDGE ( 'NONE', *, *, #48030, .F. ) ;
#42359 = AXIS2_PLACEMENT_3D ( 'NONE', #1835, #21893, #45103 ) ;
#42360 = CARTESIAN_POINT ( 'NONE',  ( 0.5835871038041853254, 43.22792673488614668, -18.18188117618243282 ) ) ;
#42361 = ORIENTED_EDGE ( 'NONE', *, *, #39888, .F. ) ;
#42362 = CARTESIAN_POINT ( 'NONE',  ( 0.7057020205115028810, -47.59410670607640270, 5.417413437617410565 ) ) ;
#42363 = CARTESIAN_POINT ( 'NONE',  ( 0.6024113833632039894, 46.67385196666943159, -15.26739701764171997 ) ) ;
#42364 = ORIENTED_EDGE ( 'NONE', *, *, #32121, .T. ) ;
#42365 = CARTESIAN_POINT ( 'NONE',  ( 5.960721111146673579, 2.672857320903303968, -20.35079619394243267 ) ) ;
#42366 = CARTESIAN_POINT ( 'NONE',  ( 0.8753041380234524160, -19.05925361776951021, 45.25354328012912219 ) ) ;
#42367 = FACE_OUTER_BOUND ( 'NONE', #25504, .T. ) ;
#42368 = FACE_OUTER_BOUND ( 'NONE', #42720, .T. ) ;
#42369 = ORIENTED_EDGE ( 'NONE', *, *, #46693, .T. ) ;
#42370 = CARTESIAN_POINT ( 'NONE',  ( 0.1152339509894530906, -40.81507403732233286, 16.76521463576112225 ) ) ;
#42371 = CARTESIAN_POINT ( 'NONE',  ( 5.959547316686252039, 17.77749189599217416, -10.25972575517511487 ) ) ;
#42372 = EDGE_CURVE ( 'NONE', #30901, #49479, #6646, .T. ) ;
#42373 = CARTESIAN_POINT ( 'NONE',  ( 2.528190830796658961, -41.78722795036133419, -4.010201538270607990 ) ) ;
#42374 = CARTESIAN_POINT ( 'NONE',  ( 0.5809828226811617480, -44.03860873105681151, -18.83114015454746237 ) ) ;
#42375 = EDGE_CURVE ( 'NONE', #32617, #38098, #43328, .T. ) ;
#42377 = CARTESIAN_POINT ( 'NONE',  ( 0.7762777257811892540, -29.86325207275904248, 37.45705273430995419 ) ) ;
#42376 =( BOUNDED_SURFACE ( )  B_SPLINE_SURFACE ( 3, 1, ( 
 ( #56758, #57667 ),
 ( #52989, #43628 ),
 ( #19199, #9157 ),
 ( #5052, #671 ) ),
 .UNSPECIFIED., .F., .F., .F. ) 
 B_SPLINE_SURFACE_WITH_KNOTS ( ( 4, 4 ),
 ( 2, 2 ),
 ( 0.000000000000000000, 1.000000000000000000 ),
 ( 0.000000000000000000, 1.000000000000000000 ),
 .UNSPECIFIED. ) 
 GEOMETRIC_REPRESENTATION_ITEM ( )  RATIONAL_B_SPLINE_SURFACE ( (
 ( 1.000000000000000000, 1.000000000000000000),
 ( 0.9754377213608244057, 0.9999580625633939235),
 ( 0.9754377213608244057, 0.9999580625633939235),
 ( 1.000000000000000000, 1.000000000000000000) ) ) 
 REPRESENTATION_ITEM ( '' )  SURFACE ( )  );
#42378 = DIRECTION ( 'NONE',  ( -0.07439287786467650709, -0.4871392060438084481, 0.8701500408883626747 ) ) ;
#42379 = FACE_OUTER_BOUND ( 'NONE', #60331, .T. ) ;
#42380 = ADVANCED_FACE ( 'NONE', ( #9269 ), #16020, .F. ) ;
#42381 = LINE ( 'NONE', #52053, #55843 ) ;
#42382 = CARTESIAN_POINT ( 'NONE',  ( 0.5824936645240085253, 40.53382933285173095, -23.58488623367848191 ) ) ;
#42383 = CYLINDRICAL_SURFACE ( 'NONE', #57369, 10.00000000000000711 ) ;
#42384 = CARTESIAN_POINT ( 'NONE',  ( 2.648799415243708655, -12.61806922346209348, 47.38461556625227189 ) ) ;
#42385 = CARTESIAN_POINT ( 'NONE',  ( 3.660176727303400934, -1.881607889988088367, 48.00143922595155033 ) ) ;
#42386 = CARTESIAN_POINT ( 'NONE',  ( 4.975801465491694664, 9.906103548668228953, -46.87746200127445206 ) ) ;
#42387 = CARTESIAN_POINT ( 'NONE',  ( 3.782542959838393948, -24.05480172452273635, 34.47614200270191986 ) ) ;
#42388 = DIRECTION ( 'NONE',  ( 1.000000000000000000, 0.000000000000000000, 0.000000000000000000 ) ) ;
#42389 =( BOUNDED_SURFACE ( )  B_SPLINE_SURFACE ( 3, 1, ( 
 ( #32287, #36691 ),
 ( #46393, #3437 ),
 ( #15654, #47929 ),
 ( #28806, #43243 ) ),
 .UNSPECIFIED., .F., .F., .F. ) 
 B_SPLINE_SURFACE_WITH_KNOTS ( ( 4, 4 ),
 ( 2, 2 ),
 ( 0.000000000000000000, 1.000000000000000000 ),
 ( 0.000000000000000000, 1.000000000000000000 ),
 .UNSPECIFIED. ) 
 GEOMETRIC_REPRESENTATION_ITEM ( )  RATIONAL_B_SPLINE_SURFACE ( (
 ( 1.000000000000000000, 1.000000000000000000),
 ( 0.9952954269826590483, 0.8620686068821339365),
 ( 0.9952954269826590483, 0.8620686068821339365),
 ( 1.000000000000000000, 1.000000000000000000) ) ) 
 REPRESENTATION_ITEM ( '' )  SURFACE ( )  );
#42390 = ADVANCED_FACE ( 'NONE', ( #60960 ), #46502, .F. ) ;
#42391 = CARTESIAN_POINT ( 'NONE',  ( 0.5804410086790514622, 11.40290849443536025, -45.49168638029294698 ) ) ;
#42392 = CARTESIAN_POINT ( 'NONE',  ( 0.7948878604505672518, -39.86121510370232102, -28.66674341034903861 ) ) ;
#42394 = ORIENTED_EDGE ( 'NONE', *, *, #49623, .T. ) ;
#42393 = CARTESIAN_POINT ( 'NONE',  ( 0.9752570700956808558, 39.55341424149108320, 16.63323182627884478 ) ) ;
#42395 = CARTESIAN_POINT ( 'NONE',  ( 4.549368137175248350, -40.58005590356700765, 13.99871866169291579 ) ) ;
#42396 = CARTESIAN_POINT ( 'NONE',  ( -5.995132425357893702, 18.20425902871274459, -4.869002713216382006 ) ) ;
#42398 = EDGE_CURVE ( 'NONE', #36654, #39909, #54483, .T. ) ;
#42397 = CARTESIAN_POINT ( 'NONE',  ( 3.680974057930774812, -32.59081219554006736, -35.20670187740648061 ) ) ;
#42399 = VERTEX_POINT ( 'NONE', #37495 ) ;
#42400 = VERTEX_POINT ( 'NONE', #13684 ) ;
#42401 = CARTESIAN_POINT ( 'NONE',  ( 0.5549461598389366923, -31.06561436148498956, 31.30727231507564312 ) ) ;
#42402 = DIRECTION ( 'NONE',  ( 0.000000000000000000, -1.000000000000000000, 1.287488025362403787E-15 ) ) ;
#42403 = AXIS2_PLACEMENT_3D ( 'NONE', #8755, #27871, #47000 ) ;
#42404 = EDGE_CURVE ( 'NONE', #57082, #57756, #59705, .T. ) ;
#42405 = ORIENTED_EDGE ( 'NONE', *, *, #6674, .F. ) ;
#42406 =( REPRESENTATION_RELATIONSHIP ('NONE','NONE', #44881, #40484 ) REPRESENTATION_RELATIONSHIP_WITH_TRANSFORMATION ( #57747 )SHAPE_REPRESENTATION_RELATIONSHIP( ) );
#42407 = ORIENTED_EDGE ( 'NONE', *, *, #32998, .F. ) ;
#42408 = CARTESIAN_POINT ( 'NONE',  ( 0.5998501479064699549, -38.48283596222010061, -28.86886762351111457 ) ) ;
#42409 = EDGE_LOOP ( 'NONE', ( #8231, #3768, #4872, #32551, #12515, #7230 ) ) ;
#42410 = DIRECTION ( 'NONE',  ( 0.000000000000000000, 0.000000000000000000, 1.000000000000000000 ) ) ;
#42411 = CARTESIAN_POINT ( 'NONE',  ( 0.9754642270333684362, -41.49150764699765404, 10.93570046136892948 ) ) ;
#42412 = ORIENTED_EDGE ( 'NONE', *, *, #54240, .F. ) ;
#42413 = ORIENTED_EDGE ( 'NONE', *, *, #28577, .T. ) ;
#42414 = CARTESIAN_POINT ( 'NONE',  ( 4.553261556744875094, 0.000000000000000000, 0.000000000000000000 ) ) ;
#42415 = ORIENTED_EDGE ( 'NONE', *, *, #48091, .F. ) ;
#42416 = CARTESIAN_POINT ( 'NONE',  ( 5.910764540655178756, -4.677486889029723649, -19.56073502893278260 ) ) ;
#42417 = ADVANCED_FACE ( 'NONE', ( #44661 ), #60932, .F. ) ;
#42418 = VECTOR ( 'NONE', #29678, 1000.000000000000000 ) ;
#42419 = CARTESIAN_POINT ( 'NONE',  ( -2.569797478183790229, -3.352038560005818457, -14.24379821351256226 ) ) ;
#42420 = ORIENTED_EDGE ( 'NONE', *, *, #13321, .T. ) ;
#42421 = CARTESIAN_POINT ( 'NONE',  ( 0.9790724872846782167, -39.60305385475923856, 13.70887797591368340 ) ) ;
#42422 = ORIENTED_EDGE ( 'NONE', *, *, #35797, .T. ) ;
#42423 = VERTEX_POINT ( 'NONE', #53405 ) ;
#42424 = LINE ( 'NONE', #23598, #16585 ) ;
#42425 = ORIENTED_EDGE ( 'NONE', *, *, #55588, .T. ) ;
#42426 = FACE_OUTER_BOUND ( 'NONE', #11198, .T. ) ;
#42427 = CARTESIAN_POINT ( 'NONE',  ( 0.9757898596046643558, -0.02632670903323431136, 42.90845459940352669 ) ) ;
#42428 = CARTESIAN_POINT ( 'NONE',  ( 0.7948878604505656975, 16.14027002511539877, -46.37014482201644938 ) ) ;
#42429 = CARTESIAN_POINT ( 'NONE',  ( 0.5804410086790514622, -38.97211966759145696, -26.09010809617946336 ) ) ;
#42430 = VERTEX_POINT ( 'NONE', #29607 ) ;
#42431 = CARTESIAN_POINT ( 'NONE',  ( 0.5806925824938511393, -45.84420715090610798, 9.875780123533177246 ) ) ;
#42432 = CARTESIAN_POINT ( 'NONE',  ( 4.962356264823608143, 34.94214251265138671, -23.45809613945485950 ) ) ;
#42433 = B_SPLINE_CURVE_WITH_KNOTS ( 'NONE', 3,
 ( #14349, #27501, #47240, #3366, #13119, #60690 ),
 .UNSPECIFIED., .F., .F.,
 ( 4, 2, 4 ),
 ( 0.000000000000000000, 0.0002450742804987322246, 0.0004901485609974644492 ),
 .UNSPECIFIED. ) ;
#42434 = DIRECTION ( 'NONE',  ( -1.000000000000000000, -0.000000000000000000, 1.925929944387235853E-32 ) ) ;
#42435 = VERTEX_POINT ( 'NONE', #54014 ) ;
#42436 = CARTESIAN_POINT ( 'NONE',  ( 0.7242003506639983490, 41.59292590893083030, 26.09674670261058438 ) ) ;
#42437 = CARTESIAN_POINT ( 'NONE',  ( 0.8753041380234524160, -29.91468680897855492, 38.93905290314216927 ) ) ;
#42438 = CARTESIAN_POINT ( 'NONE',  ( 2.879087469061463178, -5.307820464692313500, 43.67984339140849670 ) ) ;
#42439 = VERTEX_POINT ( 'NONE', #10513 ) ;
#42440 = VERTEX_POINT ( 'NONE', #30220 ) ;
#42441 = CARTESIAN_POINT ( 'NONE',  ( 2.299746137290199055, -47.08665685429843251, 13.67947674334394392 ) ) ;
#42442 = CARTESIAN_POINT ( 'NONE',  ( 4.960156602257181468, 43.79161740034472672, 15.40604254112658644 ) ) ;
#42443 = EDGE_CURVE ( 'NONE', #17526, #10258, #29101, .T. ) ;
#42444 = CARTESIAN_POINT ( 'NONE',  ( -2.601141883200662974, 1.878577531911864718, 14.80764579283231619 ) ) ;
#42445 = CARTESIAN_POINT ( 'NONE',  ( 4.962356264823602814, 22.27740539909316198, -35.70648129607287302 ) ) ;
#42446 = CIRCLE ( 'NONE', #7380, 43.92652462719577500 ) ;
#42447 = CARTESIAN_POINT ( 'NONE',  ( -2.708315649062916552, -11.76894112707806883, -8.698422600177076802 ) ) ;
#42448 = ADVANCED_FACE ( 'NONE', ( #796 ), #43749, .F. ) ;
#42449 = DIRECTION ( 'NONE',  ( 0.1024043820194936172, 0.3684880688409203353, -0.9239750460186112457 ) ) ;
#42450 = CARTESIAN_POINT ( 'NONE',  ( 0.6008122571543325074, -42.57299878231319212, 24.47640343568631494 ) ) ;
#42451 = CARTESIAN_POINT ( 'NONE',  ( 5.917102823773431552, 12.99138957749402401, 15.35296436840526368 ) ) ;
#42452 = CARTESIAN_POINT ( 'NONE',  ( 0.8560838555295167129, -41.44626783305055540, -21.96769712083564841 ) ) ;
#42453 = EDGE_CURVE ( 'NONE', #18686, #1320, #34753, .T. ) ;
#42454 = CARTESIAN_POINT ( 'NONE',  ( -6.063463321072276813, -4.300220425534933888, -18.77041706439369761 ) ) ;
#42455 = EDGE_CURVE ( 'NONE', #17384, #41864, #8127, .T. ) ;
#42456 = CARTESIAN_POINT ( 'NONE',  ( -6.016489644550736315, 17.41053539857199439, 7.206912786933354020 ) ) ;
#42457 = ORIENTED_EDGE ( 'NONE', *, *, #14332, .F. ) ;
#42458 = ADVANCED_FACE ( 'NONE', ( #1700 ), #50737, .F. ) ;
#42459 = CARTESIAN_POINT ( 'NONE',  ( -6.016104459813371719, -9.426230926598529791, -16.31603998697579527 ) ) ;
#42460 = CARTESIAN_POINT ( 'NONE',  ( 0.1103744047535531458, -34.18931094755022571, -26.28322091066863564 ) ) ;
#42461 = B_SPLINE_CURVE_WITH_KNOTS ( 'NONE', 3,
 ( #25847, #54638, #45909, #2956, #59345, #7973 ),
 .UNSPECIFIED., .F., .F.,
 ( 4, 2, 4 ),
 ( 1.168977108780794757E-16, 0.0002448718616795901690, 0.0004897437233590634610 ),
 .UNSPECIFIED. ) ;
#42462 = CARTESIAN_POINT ( 'NONE',  ( 0.5998501479064699549, -24.50586714782575726, -41.39809967730479201 ) ) ;
#42463 = CARTESIAN_POINT ( 'NONE',  ( 3.678748215320119197, 9.087549784784737739, -48.12514159156878435 ) ) ;
#42464 = AXIS2_PLACEMENT_3D ( 'NONE', #6016, #34881, #38974 ) ;
#42465 = CARTESIAN_POINT ( 'NONE',  ( 0.5549461598389364703, -23.60958411260055456, -37.25325802526328545 ) ) ;
#42466 = CARTESIAN_POINT ( 'NONE',  ( -17.97369999999976642, -7.719455939378112141, -2.099999999999997424 ) ) ;
#42467 = CARTESIAN_POINT ( 'NONE',  ( 4.956653778116966613, 0.000000000000000000, 0.000000000000000000 ) ) ;
#42468 = EDGE_CURVE ( 'NONE', #25211, #35968, #44773, .T. ) ;
#42469 = CARTESIAN_POINT ( 'NONE',  ( 4.962356264823608143, -4.645793755591040686, 41.82884409403227011 ) ) ;
#42470 = EDGE_CURVE ( 'NONE', #49719, #13205, #34327, .T. ) ;
#42471 = CARTESIAN_POINT ( 'NONE',  ( 3.660176727303414701, 35.27264088192925584, -32.61164548483928627 ) ) ;
#42473 = VERTEX_POINT ( 'NONE', #26766 ) ;
#42472 = CARTESIAN_POINT ( 'NONE',  ( 0.6017666602106488405, -46.55749120190036905, -12.11361215600163632 ) ) ;
#42474 = ORIENTED_EDGE ( 'NONE', *, *, #47624, .T. ) ;
#42475 = CARTESIAN_POINT ( 'NONE',  ( 0.9722240750034564227, -42.90442369954360657, 0.5819398758578646635 ) ) ;
#42476 = CARTESIAN_POINT ( 'NONE',  ( 5.917102823773431552, 5.950457534746081301, -19.21150106521938383 ) ) ;
#42477 = DIRECTION ( 'NONE',  ( 0.000000000000000000, 0.000000000000000000, -1.000000000000000000 ) ) ;
#42478 = ORIENTED_EDGE ( 'NONE', *, *, #6944, .F. ) ;
#42479 = CARTESIAN_POINT ( 'NONE',  ( 0.6027444965799114707, 11.05472791484353579, -47.84695922016592107 ) ) ;
#42480 = CARTESIAN_POINT ( 'NONE',  ( 0.1310142868023675966, -30.03916697317195883, -30.94009702668463646 ) ) ;
#42481 = CARTESIAN_POINT ( 'NONE',  ( -6.015611763856276717, -13.32857883366824048, -13.31979030221813254 ) ) ;
#42482 = EDGE_LOOP ( 'NONE', ( #11272, #23662, #9177, #8190, #9887, #34380, #27578, #45764, #1019, #22216, #22198, #33221, #22045, #51236, #61181, #15137, #24617, #50950, #25056, #44794, #50873, #61614, #9025, #55664, #16446, #40329, #24710, #38410, #29685, #46115, #27684, #15351, #837, #45748, #33611, #16467, #26238, #23442, #59894, #20022, #43072, #54170, #16118, #31447, #60345, #41802, #7735, #20769, #58687, #23163, #7777, #16861, #15547, #44654, #42790, #50711, #21438, #58296, #4174, #53380, #58778, #32560, #44517, #26996, #13413, #324, #25880, #38776, #16674, #51956, #29123, #35545, #39814, #13272, #59019, #20506, #52941, #18281, #31057, #60439, #50795, #34802, #61283, #8798, #5156, #18854, #59406, #53688, #48065, #19171, #23984, #22544, #5985, #13426, #7072, #58402, #11344, #36965, #38265, #2544, #57240, #53757, #43713, #59331, #57755, #43833, #36022, #14620, #4372, #44816, #28045, #44195, #42670, #11111, #5395, #43335, #24838, #46551, #607, #24927, #2233, #39185, #52908, #46911, #25809, #59381, #11041, #14623, #59343, #20753, #30089, #61177, #15586, #46898, #21106, #61388, #40223, #21044, #55100, #24583, #37112, #51213, #31872, #24110, #57722, #49108, #42578, #31826, #31118, #53549, #12386, #11215 ) ) ;
#42483 = ORIENTED_EDGE ( 'NONE', *, *, #35159, .F. ) ;
#42484 = B_SPLINE_CURVE_WITH_KNOTS ( 'NONE', 3,
 ( #41943, #46326, #27818, #37867, #51606, #37239, #9016, #61009, #28423, #23428, #27203, #42554, #18117, #13422, #46950, #56926, #3985, #4592, #13737 ),
 .UNSPECIFIED., .F., .F.,
 ( 4, 3, 3, 3, 3, 3, 4 ),
 ( 3.469446951953614189E-18, 0.0002724573126191766771, 0.0004086839781548514045, 0.0005449106435901833294, 0.0006811373090491508074, 0.0008459866663933649292, 0.001010840725717214233 ),
 .UNSPECIFIED. ) ;
#42485 = CARTESIAN_POINT ( 'NONE',  ( -2.569797478183783568, 4.218948559326054948, 14.01151037928424437 ) ) ;
#42486 = CARTESIAN_POINT ( 'NONE',  ( 3.390910168358336918, -39.98406868784916668, 18.31314794618874942 ) ) ;
#42487 = CARTESIAN_POINT ( 'NONE',  ( 1.154321485836933281, -34.54400167111882780, -25.46626718279344104 ) ) ;
#42488 = CARTESIAN_POINT ( 'NONE',  ( 0.7048096507298635682, -34.61049487267037250, -33.41730025321742659 ) ) ;
#42489 = ADVANCED_FACE ( 'NONE', ( #50874 ), #49761, .T. ) ;
#42490 = CARTESIAN_POINT ( 'NONE',  ( 4.962356264823608143, -4.645793755591040686, 41.82884409403227011 ) ) ;
#42491 = SHAPE_REPRESENTATION ( 'straight bevel gear(output)_iso_ISO - Straight bevel gear 2M 47GT 48PT 20PA 5FW ---47O25H120MD16.0N', ( #14677 ), #18740 ) ;
#42492 = EDGE_CURVE ( 'NONE', #27686, #30599, #22074, .T. ) ;
#42493 = CARTESIAN_POINT ( 'NONE',  ( 5.917102823773431552, 5.966888710896498083, 19.20640406644403342 ) ) ;
#42494 = ORIENTED_EDGE ( 'NONE', *, *, #7195, .F. ) ;
#42495 = CARTESIAN_POINT ( 'NONE',  ( 4.322998006666179727, 22.13465289016626514, -42.57894920390106108 ) ) ;
#42496 = CARTESIAN_POINT ( 'NONE',  ( -6.057079549204054558, -6.642710526269747007, 18.07500008198958952 ) ) ;
#42497 = EDGE_LOOP ( 'NONE', ( #8727, #26198, #30356, #58373 ) ) ;
#42498 = CARTESIAN_POINT ( 'NONE',  ( 0.9785694773339252972, -37.30335551955128182, -19.09960922889875690 ) ) ;
#42499 = CARTESIAN_POINT ( 'NONE',  ( 0.6000166863083090663, -43.04473087058024561, 23.64264422580035330 ) ) ;
#42500 = CARTESIAN_POINT ( 'NONE',  ( 1.479689385636123067, 39.17559155776038438, -20.17069337844452903 ) ) ;
#42501 = CARTESIAN_POINT ( 'NONE',  ( 0.5809828226811556418, 44.03860873105722362, -18.83114015454650314 ) ) ;
#42502 = CONICAL_SURFACE ( 'NONE', #19463, 42.08604991992415023, 1.569615340895231137 ) ;
#42503 = B_SPLINE_CURVE_WITH_KNOTS ( 'NONE', 3,
 ( #20317, #10605, #562, #24699, #58489, #35348 ),
 .UNSPECIFIED., .F., .F.,
 ( 4, 2, 4 ),
 ( 1.497599948434059756E-16, 0.0002445252820015213040, 0.0004890505640028927712 ),
 .UNSPECIFIED. ) ;
#42504 = EDGE_LOOP ( 'NONE', ( #61909, #23400, #35809, #50717 ) ) ;
#42505 = ORIENTED_EDGE ( 'NONE', *, *, #18489, .F. ) ;
#42506 = CARTESIAN_POINT ( 'NONE',  ( 0.5997462898726536595, -31.02483596213004091, -38.06587952047387091 ) ) ;
#42507 = CARTESIAN_POINT ( 'NONE',  ( 0.5836750258453371476, 41.38803015412003816, 24.10509086647765287 ) ) ;
#42508 = CARTESIAN_POINT ( 'NONE',  ( 0.6001305935487422083, 6.798494447611586722, 47.62765676940946236 ) ) ;
#42509 = ORIENTED_EDGE ( 'NONE', *, *, #20579, .F. ) ;
#42510 = CARTESIAN_POINT ( 'NONE',  ( 0.8560838555295223751, 11.76118766017263972, 45.40977096290989579 ) ) ;
#42511 = ORIENTED_EDGE ( 'NONE', *, *, #34032, .F. ) ;
#42512 = CARTESIAN_POINT ( 'NONE',  ( 0.9722240741986373225, -5.023189681690476860, -42.61332881199392375 ) ) ;
#42513 = CARTESIAN_POINT ( 'NONE',  ( 0.5824935313925941882, 28.11019129984335763, 37.53738565936699700 ) ) ;
#42514 = ORIENTED_EDGE ( 'NONE', *, *, #25117, .T. ) ;
#42515 = CARTESIAN_POINT ( 'NONE',  ( 0.5839879882104922482, -0.04539914087004336823, 47.89596766822081264 ) ) ;
#42516 = FACE_OUTER_BOUND ( 'NONE', #18073, .T. ) ;
#42517 = DIRECTION ( 'NONE',  ( 0.000000000000000000, 0.000000000000000000, 1.000000000000000000 ) ) ;
#42518 = EDGE_CURVE ( 'NONE', #14833, #9944, #17890, .T. ) ;
#42519 = CARTESIAN_POINT ( 'NONE',  ( 4.967162193818129623, -13.42934394584134949, -40.93989340068622340 ) ) ;
#42520 = DIRECTION ( 'NONE',  ( -0.07500201931887529039, -0.04681388819014925540, -0.9960839106072396643 ) ) ;
#42521 = CARTESIAN_POINT ( 'NONE',  ( 0.5809828226811544205, 17.82437196699742188, -44.45562576850583270 ) ) ;
#42522 = VECTOR ( 'NONE', #22196, 1000.000000000000227 ) ;
#42523 = CARTESIAN_POINT ( 'NONE',  ( 0.5998501479064699549, 47.62484632993687939, -6.798102206413639159 ) ) ;
#42524 = CARTESIAN_POINT ( 'NONE',  ( 5.880360259849752858, 9.312491912827496776, 47.05949693022710534 ) ) ;
#42525 = VERTEX_POINT ( 'NONE', #16760 ) ;
#42526 = EDGE_CURVE ( 'NONE', #47205, #4749, #2635, .T. ) ;
#42527 = CARTESIAN_POINT ( 'NONE',  ( 0.5806925824938499181, -42.09901922557445175, 20.66143612114793626 ) ) ;
#42528 = EDGE_CURVE ( 'NONE', #1527, #3705, #44976, .T. ) ;
#42529 = DIRECTION ( 'NONE',  ( 0.000000000000000000, 0.000000000000000000, -1.000000000000000000 ) ) ;
#42530 = ORIENTED_EDGE ( 'NONE', *, *, #20453, .T. ) ;
#42531 = ADVANCED_FACE ( 'NONE', ( #11759 ), #27076, .F. ) ;
#42532 = CARTESIAN_POINT ( 'NONE',  ( 0.8554163680231708922, -24.47000373826151787, -40.03029340588557972 ) ) ;
#42533 = DIRECTION ( 'NONE',  ( 1.000000000000000000, 0.000000000000000000, 0.000000000000000000 ) ) ;
#42534 = CARTESIAN_POINT ( 'NONE',  ( 4.963659409799328515, 19.36487359954699272, 40.34793212403975105 ) ) ;
#42535 = CARTESIAN_POINT ( 'NONE',  ( 0.9754642270333672149, 5.774842730422650838, -42.51806607596982701 ) ) ;
#42536 = CARTESIAN_POINT ( 'NONE',  ( -5.995132425357893702, -18.84415457712583475, 0.008513469642740825044 ) ) ;
#42537 = CARTESIAN_POINT ( 'NONE',  ( 0.5839879327111937579, -47.89596760851021173, 0.09083573661695024115 ) ) ;
#42538 = CARTESIAN_POINT ( 'NONE',  ( -21.49998475294620448, 1.965116437629976787E-15, 4.109229525913649238E-20 ) ) ;
#42539 = CARTESIAN_POINT ( 'NONE',  ( 0.6027935024548038978, 47.67281620606623704, 6.452291758824889811 ) ) ;
#42540 = CARTESIAN_POINT ( 'NONE',  ( 4.694002226626921015, 13.30107597157399368, -43.60465742835910419 ) ) ;
#42541 = CIRCLE ( 'NONE', #28504, 43.08621763946400307 ) ;
#42542 = CARTESIAN_POINT ( 'NONE',  ( 0.5806925824938499181, 32.20670061096218006, 34.08739940358331921 ) ) ;
#42543 = CARTESIAN_POINT ( 'NONE',  ( 0.1092355843206037486, -5.926758618548289448, 42.71527351115368987 ) ) ;
#42544 = ORIENTED_EDGE ( 'NONE', *, *, #26324, .T. ) ;
#42545 = VECTOR ( 'NONE', #12275, 1000.000000000000227 ) ;
#42546 = CARTESIAN_POINT ( 'NONE',  ( 5.960721111146673579, -10.26825948882938278, 17.77250458025974567 ) ) ;
#42547 = CARTESIAN_POINT ( 'NONE',  ( 7.000000000000007105, -2.649999999999161027, -80.00000000000004263 ) ) ;
#42548 = CIRCLE ( 'NONE', #35522, 43.08621763946400307 ) ;
#42549 = CARTESIAN_POINT ( 'NONE',  ( 0.1073791018717483448, 37.58707531572176919, 21.14095454447572564 ) ) ;
#42550 = CARTESIAN_POINT ( 'NONE',  ( 0.5800708119828337228, -47.89175345941821149, 0.6275298934113306970 ) ) ;
#42552 = CARTESIAN_POINT ( 'NONE',  ( 4.975610109902397937, 0.000000000000000000, 0.000000000000000000 ) ) ;
#42551 = B_SPLINE_CURVE_WITH_KNOTS ( 'NONE', 3,
 ( #18612, #46505, #60884, #52409, #18310, #47126 ),
 .UNSPECIFIED., .F., .F.,
 ( 4, 2, 4 ),
 ( 1.222726755474739050E-16, 0.0002448718616795939637, 0.0004897437233590656294 ),
 .UNSPECIFIED. ) ;
#42553 = ORIENTED_EDGE ( 'NONE', *, *, #42871, .F. ) ;
#42554 = CARTESIAN_POINT ( 'NONE',  ( 0.9756354156337464500, 11.23134828980333211, -41.41248945940449033 ) ) ;
#42555 = CYLINDRICAL_SURFACE ( 'NONE', #2160, 2.649999999999992806 ) ;
#42556 = ORIENTED_EDGE ( 'NONE', *, *, #28282, .T. ) ;
#42557 = CARTESIAN_POINT ( 'NONE',  ( 1.000433927950263424, -41.19597236030789134, -7.701333582022964919 ) ) ;
#42558 = B_SPLINE_CURVE_WITH_KNOTS ( 'NONE', 3,
 ( #32681, #47698, #61456, #22974, #32999, #14199, #18577, #33304, #61762, #55851, #52373, #9469, #13270, #9164, #18899, #56158 ),
 .UNSPECIFIED., .F., .F.,
 ( 4, 3, 3, 3, 3, 4 ),
 ( 9.813676791237319219E-18, 0.0002724568934985570107, 0.0004086836638483730996, 0.0005449104342063434189, 0.0008173270854453667817, 0.001089761613562694430 ),
 .UNSPECIFIED. ) ;
#42559 = CARTESIAN_POINT ( 'NONE',  ( 0.5837157313716024865, 43.13919761750232595, 18.39148423863895587 ) ) ;
#42560 =( BOUNDED_SURFACE ( )  B_SPLINE_SURFACE ( 3, 1, ( 
 ( #50388, #45719 ),
 ( #6515, #30353 ),
 ( #21899, #2138 ),
 ( #26583, #49465 ) ),
 .UNSPECIFIED., .F., .F., .F. ) 
 B_SPLINE_SURFACE_WITH_KNOTS ( ( 4, 4 ),
 ( 2, 2 ),
 ( 0.000000000000000000, 1.000000000000000000 ),
 ( 0.000000000000000000, 1.000000000000000000 ),
 .UNSPECIFIED. ) 
 GEOMETRIC_REPRESENTATION_ITEM ( )  RATIONAL_B_SPLINE_SURFACE ( (
 ( 1.000000000000000000, 1.000000000000000000),
 ( 0.7269869731126817891, 0.9931720237060910339),
 ( 0.7269869731126817891, 0.9931720237060910339),
 ( 1.000000000000000000, 1.000000000000000000) ) ) 
 REPRESENTATION_ITEM ( '' )  SURFACE ( )  );
#42561 = ORIENTED_EDGE ( 'NONE', *, *, #14683, .T. ) ;
#42562 = ADVANCED_FACE ( 'NONE', ( #45582 ), #52149, .F. ) ;
#42563 = CARTESIAN_POINT ( 'NONE',  ( 1.399999999999999023, 0.000000000000000000, 0.000000000000000000 ) ) ;
#42564 = ORIENTED_EDGE ( 'NONE', *, *, #4560, .F. ) ;
#42565 = FACE_OUTER_BOUND ( 'NONE', #43432, .T. ) ;
#42566 = CARTESIAN_POINT ( 'NONE',  ( 5.960721111146673579, 14.51823969584079599, 14.50930005615021656 ) ) ;
#42567 = B_SPLINE_CURVE_WITH_KNOTS ( 'NONE', 3,
 ( #48357, #33968, #43686, #15162 ),
 .UNSPECIFIED., .F., .F.,
 ( 4, 4 ),
 ( 2.178848519881467304E-17, 0.004559932413162187670 ),
 .UNSPECIFIED. ) ;
#42568 = VERTEX_POINT ( 'NONE', #25839 ) ;
#42569 = DIRECTION ( 'NONE',  ( 1.000000000000000000, 0.000000000000000000, 0.000000000000000000 ) ) ;
#42570 = FACE_OUTER_BOUND ( 'NONE', #25449, .T. ) ;
#42571 = CARTESIAN_POINT ( 'NONE',  ( 4.967162193818130511, -42.16965968614200477, 8.839793687085075291 ) ) ;
#42572 = CARTESIAN_POINT ( 'NONE',  ( 0.5834872094924173913, -38.13619618345230577, 28.97678700412168951 ) ) ;
#42573 = ORIENTED_EDGE ( 'NONE', *, *, #526, .F. ) ;
#42574 = CARTESIAN_POINT ( 'NONE',  ( 4.553261556744875094, 0.000000000000000000, 0.000000000000000000 ) ) ;
#42575 = VERTEX_POINT ( 'NONE', #36186 ) ;
#42576 = CARTESIAN_POINT ( 'NONE',  ( 0.5807400328401574052, 47.55718917606850482, -5.711437504335486359 ) ) ;
#42577 = VECTOR ( 'NONE', #39970, 1000.000000000000114 ) ;
#42578 = ORIENTED_EDGE ( 'NONE', *, *, #51454, .T. ) ;
#42579 = VERTEX_POINT ( 'NONE', #35259 ) ;
#42580 = CARTESIAN_POINT ( 'NONE',  ( 1.000433927950262980, 28.65822030437768575, -30.57981501969232951 ) ) ;
#42581 = CARTESIAN_POINT ( 'NONE',  ( 0.9762797500689124330, -37.17323042682988188, 19.35137526946117958 ) ) ;
#42582 = CONICAL_SURFACE ( 'NONE', #36592, 4.000000000000000000, 1.047197551196595855 ) ;
#42583 = CARTESIAN_POINT ( 'NONE',  ( 5.896782393890504181, 10.82771479451295349, -16.94953330350713117 ) ) ;
#42584 = CARTESIAN_POINT ( 'NONE',  ( 0.5807400328401637335, -5.711437504335642679, -47.55718917606849061 ) ) ;
#42585 = ORIENTED_EDGE ( 'NONE', *, *, #196, .F. ) ;
#42586 = CARTESIAN_POINT ( 'NONE',  ( -6.015611763856276717, -7.205255340944484388, -17.41126425312545223 ) ) ;
#42587 = CARTESIAN_POINT ( 'NONE',  ( 0.7056313189692701160, -46.12214899551614877, -8.514459230800694556 ) ) ;
#42588 = FACE_OUTER_BOUND ( 'NONE', #14528, .T. ) ;
#42589 = VECTOR ( 'NONE', #9214, 1000.000000000000114 ) ;
#42590 = ORIENTED_EDGE ( 'NONE', *, *, #51619, .T. ) ;
#42591 = B_SPLINE_CURVE_WITH_KNOTS ( 'NONE', 3,
 ( #55270, #36828, #46842, #41523 ),
 .UNSPECIFIED., .F., .F.,
 ( 4, 4 ),
 ( 0.000000000000000000, 0.004442905043737213101 ),
 .UNSPECIFIED. ) ;
#42592 = EDGE_CURVE ( 'NONE', #44953, #41472, #20127, .T. ) ;
#42593 = ORIENTED_EDGE ( 'NONE', *, *, #44332, .T. ) ;
#42594 = CARTESIAN_POINT ( 'NONE',  ( 0.1103878639767399694, -21.60424693647530958, -37.32258098927759704 ) ) ;
#42595 = CARTESIAN_POINT ( 'NONE',  ( -1.500000000000001110, 0.000000000000000000, -5.100000000000000533 ) ) ;
#42596 = DIRECTION ( 'NONE',  ( 0.000000000000000000, 0.000000000000000000, -1.000000000000000000 ) ) ;
#42597 = CARTESIAN_POINT ( 'NONE',  ( 4.834790513006555379, 46.80118606150062277, -6.499101796493102157 ) ) ;
#42598 = CARTESIAN_POINT ( 'NONE',  ( -2.739355103387248747, -7.512526911499135096, 12.89998086645938535 ) ) ;
#42599 = ORIENTED_EDGE ( 'NONE', *, *, #15513, .F. ) ;
#42600 = EDGE_CURVE ( 'NONE', #50265, #36264, #24551, .T. ) ;
#42601 = ORIENTED_EDGE ( 'NONE', *, *, #38543, .T. ) ;
#42602 = EDGE_CURVE ( 'NONE', #8164, #30005, #21908, .T. ) ;
#42603 = CARTESIAN_POINT ( 'NONE',  ( 3.407937589446178528, -12.47329436636632494, 5.663729899985029625 ) ) ;
#42604 = CARTESIAN_POINT ( 'NONE',  ( 2.533389852662419894, 42.87438241343366485, -9.961820335674985927 ) ) ;
#42605 = CARTESIAN_POINT ( 'NONE',  ( 0.5834584762367748256, -41.77312704313945346, -21.31295019585331829 ) ) ;
#42606 = CARTESIAN_POINT ( 'NONE',  ( 0.9756354156337437855, -21.56699035436967193, 37.09450626018208652 ) ) ;
#42607 = SHAPE_REPRESENTATION_RELATIONSHIP ( 'NONE' , 'NONE' ,  #10831, #24273 ) ;
#42608 = CARTESIAN_POINT ( 'NONE',  ( 0.6031356755773454870, 2.564066871919272342E-05, 48.10744332413212021 ) ) ;
#42609 = EDGE_LOOP ( 'NONE', ( #33763, #29894, #40562, #51530 ) ) ;
#42610 = CARTESIAN_POINT ( 'NONE',  ( 4.303969348037258058, 2.158280495710214630, 48.06163817123226778 ) ) ;
#42611 = CARTESIAN_POINT ( 'NONE',  ( 0.5809828226811553087, 12.92184523170202937, 46.11980934799343856 ) ) ;
#42612 = CARTESIAN_POINT ( 'NONE',  ( -6.015611763856276717, -9.416239407363420355, 16.32183393015593609 ) ) ;
#42614 = EDGE_CURVE ( 'NONE', #30244, #42659, #8910, .T. ) ;
#42613 = CARTESIAN_POINT ( 'NONE',  ( -6.079354080745853928, -8.907665152502962869, 17.07180297388200074 ) ) ;
#42615 = CARTESIAN_POINT ( 'NONE',  ( 0.5804410086790514622, -45.84731009780852418, -9.876437042313485293 ) ) ;
#42616 = EDGE_CURVE ( 'NONE', #59254, #22938, #18931, .T. ) ;
#42617 = CARTESIAN_POINT ( 'NONE',  ( -6.203732170862584994, -1.182048853166489222, 5.744326400484686099E-14 ) ) ;
#42618 = CARTESIAN_POINT ( 'NONE',  ( 0.5837799406558221715, 22.45748484441089943, -41.16922301963273867 ) ) ;
#42619 = CARTESIAN_POINT ( 'NONE',  ( 2.526552050251864134, -39.22765360404638102, -17.56110221699869101 ) ) ;
#42620 = VERTEX_POINT ( 'NONE', #8260 ) ;
#42621 = CARTESIAN_POINT ( 'NONE',  ( 1.154321485836932837, -39.95809831208268292, -15.65787964449906511 ) ) ;
#42622 = CONICAL_SURFACE ( 'NONE', #2573, 43.08621763946400307, 1.568696531533066763 ) ;
#42623 = CARTESIAN_POINT ( 'NONE',  ( 4.553261556744875094, 22.96401893593780841, -37.44587293859667199 ) ) ;
#42624 = CARTESIAN_POINT ( 'NONE',  ( -6.016761891674565099, -4.873659902332239113, -18.20201388312100477 ) ) ;
#42625 = CARTESIAN_POINT ( 'NONE',  ( 5.960721111146673579, -17.77250458025999080, 10.26825948882894934 ) ) ;
#42626 = ORIENTED_EDGE ( 'NONE', *, *, #30106, .F. ) ;
#42627 = CARTESIAN_POINT ( 'NONE',  ( 5.896278296736517710, 19.71091930359941102, -4.000829891581988207 ) ) ;
#42628 = CIRCLE ( 'NONE', #15621, 48.91267123290010943 ) ;
#42629 = SURFACE_SIDE_STYLE ('',( #60777 ) ) ;
#42630 = ORIENTED_EDGE ( 'NONE', *, *, #21466, .T. ) ;
#42631 = CARTESIAN_POINT ( 'NONE',  ( 4.963659409799330291, -2.450325214228084025, -44.68724496494576925 ) ) ;
#42632 = ADVANCED_FACE ( 'NONE', ( #61192 ), #50508, .F. ) ;
#42633 = CARTESIAN_POINT ( 'NONE',  ( 0.5824936645240084143, -45.88238142230681404, -9.697693233870870344 ) ) ;
#42634 = EDGE_LOOP ( 'NONE', ( #61866, #8318, #16239, #78 ) ) ;
#42635 = CONICAL_SURFACE ( 'NONE', #30626, 42.08604991992415023, 1.569615340895231137 ) ;
#42636 = CARTESIAN_POINT ( 'NONE',  ( 0.1119899015040011075, 41.69625326363821927, 14.43550386952412268 ) ) ;
#42637 = ORIENTED_EDGE ( 'NONE', *, *, #32284, .F. ) ;
#42638 = FACE_BOUND ( 'NONE', #41980, .T. ) ;
#42639 = ORIENTED_EDGE ( 'NONE', *, *, #27933, .F. ) ;
#42640 = CARTESIAN_POINT ( 'NONE',  ( 1.000110580585050757, -6.321169275951049826, -41.43018587644367301 ) ) ;
#42641 = CARTESIAN_POINT ( 'NONE',  ( -6.077587904424778920, 19.09876248768971152, -2.456276212632990674 ) ) ;
#42642 = ORIENTED_EDGE ( 'NONE', *, *, #38205, .F. ) ;
#42643 = B_SPLINE_CURVE_WITH_KNOTS ( 'NONE', 3,
 ( #20659, #2456, #35081, #49463, #59156, #54139, #16265, #40720, #30657, #6513, #35389, #54448, #11575, #6834, #49774, #50091, #59466, #25975, #39799 ),
 .UNSPECIFIED., .F., .F.,
 ( 4, 3, 3, 3, 3, 3, 4 ),
 ( 1.144439277862597989E-16, 0.0002618519381806271636, 0.0003927759815485981436, 0.0005237000248299445142, 0.0006546240681324981504, 0.0007855481115631322755, 0.0009699050456655115924 ),
 .UNSPECIFIED. ) ;
#42644 = ORIENTED_EDGE ( 'NONE', *, *, #51969, .T. ) ;
#42645 = CARTESIAN_POINT ( 'NONE',  ( 0.8560838555295158248, 43.53454501559585310, -17.46757637357826454 ) ) ;
#42646 = CARTESIAN_POINT ( 'NONE',  ( 0.7762783648524377300, 13.25585403815120245, 46.03397615175189372 ) ) ;
#42647 = FACE_OUTER_BOUND ( 'NONE', #60709, .T. ) ;
#42648 = VERTEX_POINT ( 'NONE', #27380 ) ;
#42649 = CARTESIAN_POINT ( 'NONE',  ( -90.00000000000000000, 6.123233995736767268E-16, 5.000000000000000888 ) ) ;
#42650 = CARTESIAN_POINT ( 'NONE',  ( 4.335381028904216727, -47.87967504119340134, -10.35826074271485275 ) ) ;
#42651 = LINE ( 'NONE', #14153, #50247 ) ;
#42652 = CARTESIAN_POINT ( 'NONE',  ( 0.1145239942831223490, -22.59375522573645867, -37.90076127868911016 ) ) ;
#42653 = ORIENTED_EDGE ( 'NONE', *, *, #22567, .F. ) ;
#42654 = FACE_OUTER_BOUND ( 'NONE', #35490, .T. ) ;
#42655 = CARTESIAN_POINT ( 'NONE',  ( 0.1157506346131639274, -31.76102471912784608, -30.62969096471239894 ) ) ;
#42656 = ORIENTED_EDGE ( 'NONE', *, *, #33289, .F. ) ;
#42657 = CARTESIAN_POINT ( 'NONE',  ( 0.7056555295713301534, 47.59410019435330241, 5.417452459789892316 ) ) ;
#42658 = B_SPLINE_CURVE_WITH_KNOTS ( 'NONE', 3,
 ( #1932, #35171, #21058, #39568, #31076, #16671 ),
 .UNSPECIFIED., .F., .F.,
 ( 4, 2, 4 ),
 ( 4.770489558936219510E-18, 0.0002291472222819929626, 0.0004582944445639811548 ),
 .UNSPECIFIED. ) ;
#42659 = VERTEX_POINT ( 'NONE', #32715 ) ;
#42660 = CARTESIAN_POINT ( 'NONE',  ( -6.016104459813371719, 18.20253432612966904, 4.871830707673121097 ) ) ;
#42661 = CARTESIAN_POINT ( 'NONE',  ( 0.6041374136657475802, -29.42442150067225981, 38.05989626241380819 ) ) ;
#42662 = ORIENTED_EDGE ( 'NONE', *, *, #37756, .T. ) ;
#42663 = CARTESIAN_POINT ( 'NONE',  ( 0.9775691876210967912, -34.33603183980574869, -24.02853775172010486 ) ) ;
#42664 = FACE_OUTER_BOUND ( 'NONE', #58140, .T. ) ;
#42665 = CARTESIAN_POINT ( 'NONE',  ( 4.962356264823603702, 12.05238263218972072, -40.32338863178092225 ) ) ;
#42666 = DIRECTION ( 'NONE',  ( -1.000000000000000000, -0.000000000000000000, -0.000000000000000000 ) ) ;
#42667 = EDGE_CURVE ( 'NONE', #45332, #61929, #42551, .T. ) ;
#42668 = VECTOR ( 'NONE', #49809, 1000.000000000000341 ) ;
#42669 = AXIS2_PLACEMENT_3D ( 'NONE', #4610, #38806, #5239 ) ;
#42670 = ORIENTED_EDGE ( 'NONE', *, *, #32612, .T. ) ;
#42671 = CARTESIAN_POINT ( 'NONE',  ( 3.660176727303400934, 4.399934609596583002, 47.83637937224826686 ) ) ;
#42672 = AXIS2_PLACEMENT_3D ( 'NONE', #59037, #50569, #16450 ) ;
#42673 = CARTESIAN_POINT ( 'NONE',  ( 0.6846871229502899947, -41.05093867799203622, 24.69859318104474255 ) ) ;
#42674 = EDGE_CURVE ( 'NONE', #30112, #21310, #56899, .T. ) ;
#42675 = DIRECTION ( 'NONE',  ( 0.000000000000000000, 0.000000000000000000, 1.000000000000000000 ) ) ;
#42676 = CARTESIAN_POINT ( 'NONE',  ( 0.5832366564991507962, -44.35361744978924037, -18.07697797533135642 ) ) ;
#42677 = ADVANCED_FACE ( 'NONE', ( #4469 ), #52512, .F. ) ;
#42678 = DIRECTION ( 'NONE',  ( -1.655270492344281801E-16, 1.000000000000000000, 0.000000000000000000 ) ) ;
#42679 = DIRECTION ( 'NONE',  ( 1.000000000000000000, 0.000000000000000000, 0.000000000000000000 ) ) ;
#42680 = CARTESIAN_POINT ( 'NONE',  ( 0.5809828226811617480, -46.40184912890847357, 11.86925843957150128 ) ) ;
#42681 = VECTOR ( 'NONE', #39235, 1000.000000000000114 ) ;
#42682 = CARTESIAN_POINT ( 'NONE',  ( 0.8744876279028306332, 46.86690837902563089, 14.62336997314605469 ) ) ;
#42683 = B_SPLINE_CURVE_WITH_KNOTS ( 'NONE', 3,
 ( #37343, #59891, #27932, #60493 ),
 .UNSPECIFIED., .F., .F.,
 ( 4, 4 ),
 ( 0.000000000000000000, 0.004445488388166994251 ),
 .UNSPECIFIED. ) ;
#42684 = CARTESIAN_POINT ( 'NONE',  ( 0.5837799406558231707, 40.30297663972491762, -23.97735647553728455 ) ) ;
#42685 = DIRECTION ( 'NONE',  ( 1.000000000000000000, 0.000000000000000000, 0.000000000000000000 ) ) ;
#42686 = FACE_OUTER_BOUND ( 'NONE', #22565, .T. ) ;
#42687 = ADVANCED_FACE ( 'NONE', ( #32405 ), #53843, .T. ) ;
#42688 = CARTESIAN_POINT ( 'NONE',  ( -6.010958268070873523, -7.224487401384422469, 17.40352239307055271 ) ) ;
#42689 = CARTESIAN_POINT ( 'NONE',  ( 0.9757787079277449038, 37.14005577278821590, 21.48842038179446590 ) ) ;
#42690 = CARTESIAN_POINT ( 'NONE',  ( 0.5804410086790514622, 16.34485605153991017, -43.95867983128970735 ) ) ;
#42691 = DIRECTION ( 'NONE',  ( 0.000000000000000000, 0.000000000000000000, 1.000000000000000000 ) ) ;
#42692 = CARTESIAN_POINT ( 'NONE',  ( 0.1147471544378675656, 37.14850691661145277, 23.81051495326627077 ) ) ;
#42694 = ORIENTED_EDGE ( 'NONE', *, *, #35595, .F. ) ;
#42693 = LINE ( 'NONE', #61754, #14334 ) ;
#42695 = CARTESIAN_POINT ( 'NONE',  ( 0.8753041380234530822, -34.64850320773157932, 34.79395857525835822 ) ) ;
#42696 = CARTESIAN_POINT ( 'NONE',  ( 0.8744876279028263033, 5.599149760998344050, -48.77498920895221346 ) ) ;
#42697 = CARTESIAN_POINT ( 'NONE',  ( 0.6067375320500704161, -34.36594163291733395, 33.36326114377807528 ) ) ;
#42698 = ORIENTED_EDGE ( 'NONE', *, *, #21351, .T. ) ;
#42699 = CARTESIAN_POINT ( 'NONE',  ( 2.706805983486679779, -30.43958851955885692, 31.78376258531540799 ) ) ;
#42700 = CARTESIAN_POINT ( 'NONE',  ( 0.5782707292762442330, 36.35509350284729635, 29.63179930592889733 ) ) ;
#42701 = ORIENTED_EDGE ( 'NONE', *, *, #17018, .T. ) ;
#42702 = VERTEX_POINT ( 'NONE', #42431 ) ;
#42703 = B_SPLINE_CURVE_WITH_KNOTS ( 'NONE', 3,
 ( #51505, #3892, #18639, #4500, #8922, #28950 ),
 .UNSPECIFIED., .F., .F.,
 ( 4, 2, 4 ),
 ( 8.787390050835121380E-18, 0.0002448709889506569398, 0.0004897419779013041218 ),
 .UNSPECIFIED. ) ;
#42704 = CARTESIAN_POINT ( 'NONE',  ( 4.956445790443988031, 0.000000000000000000, 0.000000000000000000 ) ) ;
#42705 = AXIS2_PLACEMENT_3D ( 'NONE', #45295, #2647, #30538 ) ;
#42706 = ORIENTED_EDGE ( 'NONE', *, *, #53515, .F. ) ;
#42707 = CARTESIAN_POINT ( 'NONE',  ( 4.975801465491695552, 43.22084481528192157, 20.67815041659156705 ) ) ;
#42708 = AXIS2_PLACEMENT_3D ( 'NONE', #60166, #2217, #31679 ) ;
#42709 = CARTESIAN_POINT ( 'NONE',  ( 0.9756950546413949432, -41.42124338356082802, 11.19893879603432296 ) ) ;
#42710 = AXIS2_PLACEMENT_3D ( 'NONE', #14218, #18918, #33936 ) ;
#42711 = ORIENTED_EDGE ( 'NONE', *, *, #18837, .F. ) ;
#42712 = ADVANCED_FACE ( 'NONE', ( #55880 ), #31305, .F. ) ;
#42713 = EDGE_LOOP ( 'NONE', ( #41376, #25923, #52180 ) ) ;
#42714 = CARTESIAN_POINT ( 'NONE',  ( 4.962356264823603702, -10.17958088187380739, -40.83640203215431086 ) ) ;
#42715 = ORIENTED_EDGE ( 'NONE', *, *, #27977, .T. ) ;
#42716 = CARTESIAN_POINT ( 'NONE',  ( -6.078726893082806448, -12.94330610022648820, 14.25709887966552003 ) ) ;
#42717 = CARTESIAN_POINT ( 'NONE',  ( 4.549368137175248350, 0.000000000000000000, 0.000000000000000000 ) ) ;
#42718 = EDGE_CURVE ( 'NONE', #12140, #2858, #23609, .T. ) ;
#42719 = CARTESIAN_POINT ( 'NONE',  ( 0.1081432562775999084, -30.19275717928102409, -30.79166192943834801 ) ) ;
#42720 = EDGE_LOOP ( 'NONE', ( #29391, #47497, #1769, #14164 ) ) ;
#42721 = CARTESIAN_POINT ( 'NONE',  ( 0.1129192098497447394, -7.520259262076021578, -43.47870154933693243 ) ) ;
#42722 = CARTESIAN_POINT ( 'NONE',  ( 0.9780106845699496620, -39.69153635952322645, 13.45039731294514773 ) ) ;
#42723 = ORIENTED_EDGE ( 'NONE', *, *, #27468, .F. ) ;
#42724 = EDGE_CURVE ( 'NONE', #43333, #51621, #2900, .T. ) ;
#42725 = VERTEX_POINT ( 'NONE', #15763 ) ;
#42726 = DIRECTION ( 'NONE',  ( 0.07500201931887538753, -0.3709639164044654658, 0.9256135639801049697 ) ) ;
#42727 = ORIENTED_EDGE ( 'NONE', *, *, #39942, .F. ) ;
#42728 = CARTESIAN_POINT ( 'NONE',  ( 0.8560838555295158248, -8.701885300216421371, 46.09392613244839509 ) ) ;
#42729 = CARTESIAN_POINT ( 'NONE',  ( -6.016489644550737204, -2.463898142942892555, 18.68142234211823549 ) ) ;
#42730 = CARTESIAN_POINT ( 'NONE',  ( 4.694002226626921015, 28.69237940071545268, 35.42643272715351799 ) ) ;
#42731 = DIRECTION ( 'NONE',  ( -0.000000000000000000, -0.000000000000000000, 1.000000000000000000 ) ) ;
#42732 = CARTESIAN_POINT ( 'NONE',  ( -5.995132425357893702, 2.451215106828342982, 18.68405145320025085 ) ) ;
#42733 = VERTEX_POINT ( 'NONE', #19851 ) ;
#42734 = CARTESIAN_POINT ( 'NONE',  ( 0.9745511491811756910, -30.09905547141332605, -30.58068216140363660 ) ) ;
#42735 = CIRCLE ( 'NONE', #50704, 8.000000000000000000 ) ;
#42736 = DIRECTION ( 'NONE',  ( -1.000000000000000000, -0.000000000000000000, -0.000000000000000000 ) ) ;
#42737 =( BOUNDED_SURFACE ( )  B_SPLINE_SURFACE ( 3, 1, ( 
 ( #4792, #53636 ),
 ( #10769, #53954 ),
 ( #38669, #29238 ),
 ( #23934, #48971 ) ),
 .UNSPECIFIED., .F., .F., .F. ) 
 B_SPLINE_SURFACE_WITH_KNOTS ( ( 4, 4 ),
 ( 2, 2 ),
 ( 0.000000000000000000, 1.000000000000000000 ),
 ( 0.000000000000000000, 1.000000000000000000 ),
 .UNSPECIFIED. ) 
 GEOMETRIC_REPRESENTATION_ITEM ( )  RATIONAL_B_SPLINE_SURFACE ( (
 ( 1.000000000000000000, 1.000000000000000000),
 ( 0.9953040768229013402, 0.8617119497784988535),
 ( 0.9953040768229013402, 0.8617119497784988535),
 ( 1.000000000000000000, 1.000000000000000000) ) ) 
 REPRESENTATION_ITEM ( '' )  SURFACE ( )  );
#42738 = LINE ( 'NONE', #23924, #27437 ) ;
#42739 = VERTEX_POINT ( 'NONE', #29530 ) ;
#42740 = CARTESIAN_POINT ( 'NONE',  ( 0.8554163680231738898, 46.36773742900842166, 7.158100224665124856 ) ) ;
#42741 = CARTESIAN_POINT ( 'NONE',  ( -6.015611763856276717, 18.19956619163665223, -4.882992715191109667 ) ) ;
#42742 = CARTESIAN_POINT ( 'NONE',  ( 0.1129192098497447394, -41.07894348801345075, -16.10814047907924973 ) ) ;
#42743 = EDGE_CURVE ( 'NONE', #60753, #46133, #36913, .T. ) ;
#42744 = EDGE_LOOP ( 'NONE', ( #32941, #11671, #895, #49599 ) ) ;
#42745 = VERTEX_POINT ( 'NONE', #10751 ) ;
#42746 = CARTESIAN_POINT ( 'NONE',  ( 0.1129192098497455998, 19.97823103613628248, 39.34236993944205807 ) ) ;
#42747 = CARTESIAN_POINT ( 'NONE',  ( 4.975610109902397937, 30.94437158899580353, 37.88001153774800400 ) ) ;
#42748 = ADVANCED_FACE ( 'NONE', ( #34252 ), #10875, .F. ) ;
#42749 = CARTESIAN_POINT ( 'NONE',  ( 5.896782393890504181, -9.671431223050909409, -17.63489452692610371 ) ) ;
#42750 = CARTESIAN_POINT ( 'NONE',  ( 4.553261556744873317, 43.59419396814051595, 5.393126930805304475 ) ) ;
#42751 = CARTESIAN_POINT ( 'NONE',  ( 0.8557997880470690211, -44.60232077416674201, -17.48760788519264153 ) ) ;
#42752 = ADVANCED_FACE ( 'NONE', ( #33949 ), #41761, .F. ) ;
#42753 = CARTESIAN_POINT ( 'NONE',  ( 4.975610109902397937, 19.27143522741721426, -44.95621415792522413 ) ) ;
#42754 = CARTESIAN_POINT ( 'NONE',  ( 1.154321485836932837, -22.16897757994451013, -36.74718014677589650 ) ) ;
#42755 =( BOUNDED_SURFACE ( )  B_SPLINE_SURFACE ( 3, 1, ( 
 ( #37164, #17118 ),
 ( #60613, #17418 ),
 ( #51221, #56233 ),
 ( #32447, #23357 ) ),
 .UNSPECIFIED., .F., .F., .F. ) 
 B_SPLINE_SURFACE_WITH_KNOTS ( ( 4, 4 ),
 ( 2, 2 ),
 ( 0.000000000000000000, 1.000000000000000000 ),
 ( 0.000000000000000000, 1.000000000000000000 ),
 .UNSPECIFIED. ) 
 GEOMETRIC_REPRESENTATION_ITEM ( )  RATIONAL_B_SPLINE_SURFACE ( (
 ( 1.000000000000000000, 1.000000000000000000),
 ( 0.7211978278499968642, 0.9934217856018975334),
 ( 0.7211978278499968642, 0.9934217856018975334),
 ( 1.000000000000000000, 1.000000000000000000) ) ) 
 REPRESENTATION_ITEM ( '' )  SURFACE ( )  );
#42756 = DIRECTION ( 'NONE',  ( 0.000000000000000000, 0.000000000000000000, 1.000000000000000000 ) ) ;
#42757 = CARTESIAN_POINT ( 'NONE',  ( 0.2885697896453111033, 42.84523253470161563, -4.828949182955488695 ) ) ;
#42758 = CARTESIAN_POINT ( 'NONE',  ( 0.6254087463353913412, 29.82831063981281972, 37.74264085326067431 ) ) ;
#42759 = CIRCLE ( 'NONE', #39776, 2.649999999999999467 ) ;
#42760 = CARTESIAN_POINT ( 'NONE',  ( 0.1368894036331286812, -22.32560810002344809, 38.05822577167124621 ) ) ;
#42761 = CARTESIAN_POINT ( 'NONE',  ( 5.959547316686252039, -5.308980600728319565, -19.82715097195160325 ) ) ;
#42762 = ORIENTED_EDGE ( 'NONE', *, *, #15650, .T. ) ;
#42763 = AXIS2_PLACEMENT_3D ( 'NONE', #20839, #44363, #1392 ) ;
#42764 = CONICAL_SURFACE ( 'NONE', #29723, 42.08604991992415023, 1.569615340895231137 ) ;
#42765 = CARTESIAN_POINT ( 'NONE',  ( 1.830465331921978134, 19.27193292033265237, 39.61020900465671701 ) ) ;
#42766 = CARTESIAN_POINT ( 'NONE',  ( 5.860006189529234355, -15.48781697582079531, 45.67886430272027098 ) ) ;
#42767 = CARTESIAN_POINT ( 'NONE',  ( 1.227938101723756947, -36.73927144310528092, 22.18841447410706635 ) ) ;
#42768 = EDGE_CURVE ( 'NONE', #49434, #47393, #6534, .T. ) ;
#42769 = CARTESIAN_POINT ( 'NONE',  ( 4.975610109902397937, -27.50982196586548412, -40.44328253918266824 ) ) ;
#42770 = CARTESIAN_POINT ( 'NONE',  ( 1.227938101723756947, -39.32113113558978057, 17.20315230597830336 ) ) ;
#42771 = CONTEXT_DEPENDENT_SHAPE_REPRESENTATION ( #38024, #17292 ) ;
#42772 = DIRECTION ( 'NONE',  ( 0.000000000000000000, 0.000000000000000000, 1.000000000000000000 ) ) ;
#42773 = B_SPLINE_CURVE_WITH_KNOTS ( 'NONE', 3,
 ( #27580, #31987, #8160, #56381, #46398, #60458 ),
 .UNSPECIFIED., .F., .F.,
 ( 4, 2, 4 ),
 ( 0.000000000000000000, 0.0002447195606305738787, 0.0004894391212611477575 ),
 .UNSPECIFIED. ) ;
#42774 = CARTESIAN_POINT ( 'NONE',  ( 4.956445790444005794, -36.61936279692559992, -29.60676136437043127 ) ) ;
#42775 = CARTESIAN_POINT ( 'NONE',  ( 0.5832367798473397924, 12.13303976268060858, 46.33367954572886305 ) ) ;
#42776 = CARTESIAN_POINT ( 'NONE',  ( 9.999999999999989342, 85.00000000000001421, 1.040949779275250495E-14 ) ) ;
#42778 = EDGE_LOOP ( 'NONE', ( #52679, #32242, #37878, #50032 ) ) ;
#42777 = CARTESIAN_POINT ( 'NONE',  ( 0.6009453534118439633, -46.35353704332102609, -12.87216801774528996 ) ) ;
#42779 = ORIENTED_EDGE ( 'NONE', *, *, #29655, .T. ) ;
#42780 = CARTESIAN_POINT ( 'NONE',  ( 0.5848930533535030563, -25.38746244141776387, -39.43031616882066714 ) ) ;
#42781 = CARTESIAN_POINT ( 'NONE',  ( 3.238018933889920792, -8.855909537851550439, 10.04889837868026703 ) ) ;
#42782 = CARTESIAN_POINT ( 'NONE',  ( 2.643462169533613793, 37.25264019563415729, -30.32726672320761097 ) ) ;
#42783 = ORIENTED_EDGE ( 'NONE', *, *, #24738, .T. ) ;
#42784 = CARTESIAN_POINT ( 'NONE',  ( -4.908599999999999852, 12.80000000000000071, 0.000000000000000000 ) ) ;
#42785 = CARTESIAN_POINT ( 'NONE',  ( 0.6252788684277219566, -47.32158689167658849, 13.11913660372399093 ) ) ;
#42786 = CARTESIAN_POINT ( 'NONE',  ( 0.5827357941260202789, -41.65958460246757511, -23.63272379758836195 ) ) ;
#42787 = B_SPLINE_CURVE_WITH_KNOTS ( 'NONE', 3,
 ( #11766, #40908, #16152, #54022 ),
 .UNSPECIFIED., .F., .F.,
 ( 4, 4 ),
 ( 4.336808689942017736E-19, 0.005014147105413698652 ),
 .UNSPECIFIED. ) ;
#42788 = B_SPLINE_CURVE_WITH_KNOTS ( 'NONE', 3,
 ( #27186, #3354, #55987, #35686, #13105, #50668 ),
 .UNSPECIFIED., .F., .F.,
 ( 4, 2, 4 ),
 ( 9.745765416140531346E-18, 0.0002291978881530158619, 0.0004583957763060219660 ),
 .UNSPECIFIED. ) ;
#42789 = ORIENTED_EDGE ( 'NONE', *, *, #18882, .T. ) ;
#42790 = ORIENTED_EDGE ( 'NONE', *, *, #36113, .T. ) ;
#42791 = B_SPLINE_CURVE_WITH_KNOTS ( 'NONE', 3,
 ( #45172, #6896, #36078, #26644 ),
 .UNSPECIFIED., .F., .F.,
 ( 4, 4 ),
 ( 0.000000000000000000, 0.005013413432710150247 ),
 .UNSPECIFIED. ) ;
#42792 = CARTESIAN_POINT ( 'NONE',  ( 0.8760168074886960365, -29.98565522133374373, 37.61398439004481986 ) ) ;
#42793 = VECTOR ( 'NONE', #31195, 1000.000000000000114 ) ;
#42794 = CARTESIAN_POINT ( 'NONE',  ( 2.359973842542475442, -40.21654738650805427, 17.90991934491199444 ) ) ;
#42795 = CARTESIAN_POINT ( 'NONE',  ( 4.694002226626921015, 28.15356303305684804, 35.85612444185553471 ) ) ;
#42796 = EDGE_CURVE ( 'NONE', #29310, #46130, #566, .T. ) ;
#42797 = EDGE_CURVE ( 'NONE', #56636, #15927, #50121, .T. ) ;
#42798 = CARTESIAN_POINT ( 'NONE',  ( 4.967162193818130511, 40.65506779172185503, -14.26841313271238221 ) ) ;
#42799 = FACE_OUTER_BOUND ( 'NONE', #36460, .T. ) ;
#42800 = ORIENTED_EDGE ( 'NONE', *, *, #51261, .F. ) ;
#42801 = EDGE_CURVE ( 'NONE', #24263, #24670, #52161, .T. ) ;
#42802 = ADVANCED_FACE ( 'NONE', ( #19235 ), #34884, .F. ) ;
#42803 = DIRECTION ( 'NONE',  ( 0.000000000000000000, 0.000000000000000000, 1.000000000000000000 ) ) ;
#42804 = CARTESIAN_POINT ( 'NONE',  ( 4.335381028904201628, 18.89720170524701004, -45.19571456870170323 ) ) ;
#42805 = AXIS2_PLACEMENT_3D ( 'NONE', #40227, #40526, #34891 ) ;
#42806 = ORIENTED_EDGE ( 'NONE', *, *, #4999, .T. ) ;
#42807 = AXIS2_PLACEMENT_3D ( 'NONE', #60805, #3178, #51401 ) ;
#42808 = CARTESIAN_POINT ( 'NONE',  ( 0.8751705887134423323, 17.57879340691479797, 44.76769609654243709 ) ) ;
#42809 = EDGE_CURVE ( 'NONE', #22425, #19824, #31994, .T. ) ;
#42810 = CARTESIAN_POINT ( 'NONE',  ( 0.5800708057587384836, -47.89175345272234807, -0.6275304576135395385 ) ) ;
#42811 = CARTESIAN_POINT ( 'NONE',  ( 4.960156602257179692, -38.88108289790847039, -25.36362146861427647 ) ) ;
#42812 = CARTESIAN_POINT ( 'NONE',  ( 2.526552050251863690, -17.56110221699855245, 39.22765360404644497 ) ) ;
#42813 = ORIENTED_EDGE ( 'NONE', *, *, #43626, .T. ) ;
#42814 = ORIENTED_EDGE ( 'NONE', *, *, #2917, .F. ) ;
#42815 = CARTESIAN_POINT ( 'NONE',  ( 0.1152809850208376119, -44.12364846630579507, -0.2211979014933812271 ) ) ;
#42816 = CARTESIAN_POINT ( 'NONE',  ( 0.9757787079277436826, -42.53619983261573623, -5.639827755377083029 ) ) ;
#42817 = CARTESIAN_POINT ( 'NONE',  ( 0.3622758884714600280, 25.58609868863721459, 34.70015533914837391 ) ) ;
#42818 = EDGE_CURVE ( 'NONE', #14283, #26948, #26764, .T. ) ;
#42819 = ORIENTED_EDGE ( 'NONE', *, *, #41339, .T. ) ;
#42820 = LINE ( 'NONE', #38742, #7492 ) ;
#42821 = ORIENTED_EDGE ( 'NONE', *, *, #43305, .F. ) ;
#42822 = CARTESIAN_POINT ( 'NONE',  ( -6.017396004339686577, 0.001173774848981854477, 18.84316306185412415 ) ) ;
#42823 = CARTESIAN_POINT ( 'NONE',  ( 0.6021448801613057400, -25.67997845241691834, 41.85785285117177779 ) ) ;
#42824 = EDGE_CURVE ( 'NONE', #20977, #60, #44003, .T. ) ;
#42825 = VECTOR ( 'NONE', #34, 1000.000000000000227 ) ;
#42826 = ORIENTED_EDGE ( 'NONE', *, *, #36168, .T. ) ;
#42827 = CARTESIAN_POINT ( 'NONE',  ( 0.5827359174754830340, -0.3632382226754043431, 47.89462060834303259 ) ) ;
#42828 = CARTESIAN_POINT ( 'NONE',  ( 0.6000166863083090663, -49.10753961887881758, 0.5225268306041207511 ) ) ;
#42829 = CARTESIAN_POINT ( 'NONE',  ( 0.1073791018717578927, 34.50606437925546999, -25.86618856530675714 ) ) ;
#42830 = VECTOR ( 'NONE', #53643, 999.9999999999998863 ) ;
#42831 = VERTEX_POINT ( 'NONE', #50718 ) ;
#42832 = CARTESIAN_POINT ( 'NONE',  ( 0.5800708119828336118, -18.90714262039440996, -44.00606550371082193 ) ) ;
#42833 = DIRECTION ( 'NONE',  ( -1.000000000000000000, -0.000000000000000000, -0.000000000000000000 ) ) ;
#42834 = CARTESIAN_POINT ( 'NONE',  ( 5.910764540655178756, -19.40170003828495027, -5.298610581423855770 ) ) ;
#42835 = CARTESIAN_POINT ( 'NONE',  ( -6.063463321072276813, 13.82218400051391960, -13.40774708649469105 ) ) ;
#42836 = CARTESIAN_POINT ( 'NONE',  ( 0.2279481005628835044, -38.80879475857510386, 20.98525521550088513 ) ) ;
#42837 = ORIENTED_EDGE ( 'NONE', *, *, #51165, .T. ) ;
#42838 = CARTESIAN_POINT ( 'NONE',  ( -2.569797478183783568, -7.701637110048594970, -12.44213550320650619 ) ) ;
#42839 = B_SPLINE_CURVE_WITH_KNOTS ( 'NONE', 3,
 ( #43992, #15454, #39587, #34566, #39902, #30453, #21073, #25771, #15768, #1632, #11068, #35498, #1948, #1025, #34259, #6013, #30150, #48963, #25146, #58029, #44292, #59268, #30770, #49889, #6947 ),
 .UNSPECIFIED., .F., .F.,
 ( 4, 3, 3, 3, 3, 3, 3, 3, 4 ),
 ( 4.670885906470169154E-18, 0.0005656085177311397484, 0.001131215744874499406, 0.001696821861372765266, 0.002262427090022498151, 0.002828031679238745925, 0.003393635864401604862, 0.003977030878808131623, 0.004561030005651158133 ),
 .UNSPECIFIED. ) ;
#42840 = CARTESIAN_POINT ( 'NONE',  ( 0.7057020205115064337, -24.67553336431215172, 41.05685587925830760 ) ) ;
#42841 = ORIENTED_EDGE ( 'NONE', *, *, #39557, .F. ) ;
#42842 = CARTESIAN_POINT ( 'NONE',  ( 0.9762797500689124330, 24.45014227843030596, -34.03697001423921620 ) ) ;
#42843 = CARTESIAN_POINT ( 'NONE',  ( 0.5836750258453355933, 0.1816059738423085046, -47.89563095930317616 ) ) ;
#42844 = CARTESIAN_POINT ( 'NONE',  ( 0.2285344041767131407, -34.89800547056871238, 26.99315440017360146 ) ) ;
#42845 = CARTESIAN_POINT ( 'NONE',  ( -5.439999999999997726, -15.14599999999999014, 1.854850041988580438E-15 ) ) ;
#42846 = ADVANCED_FACE ( 'NONE', ( #31630 ), #16489, .F. ) ;
#42847 = CARTESIAN_POINT ( 'NONE',  ( 4.975610109902397937, 48.90928568712962488, -0.5754830253892166958 ) ) ;
#42848 = DIRECTION ( 'NONE',  ( -1.000000000000000000, -0.000000000000000000, -0.000000000000000000 ) ) ;
#42849 = CARTESIAN_POINT ( 'NONE',  ( 0.5834872094924159480, -47.89542889285422689, -0.2270145249678201249 ) ) ;
#42850 = DIRECTION ( 'NONE',  ( 1.038697898353729756E-16, -0.8294993580478376982, 0.5585076678061146049 ) ) ;
#42851 = CARTESIAN_POINT ( 'NONE',  ( 0.6009453534118438522, 47.63713118507418187, 6.711694149738390180 ) ) ;
#42852 = EDGE_CURVE ( 'NONE', #50622, #50432, #61649, .T. ) ;
#42853 = CARTESIAN_POINT ( 'NONE',  ( 0.7044674535453004927, -29.95677278048795600, 38.91522179545072646 ) ) ;
#42854 = AXIS2_PLACEMENT_3D ( 'NONE', #21907, #60104, #13433 ) ;
#42855 = LINE ( 'NONE', #29341, #28416 ) ;
#42856 = CARTESIAN_POINT ( 'NONE',  ( 4.967162193818130511, 0.000000000000000000, 0.000000000000000000 ) ) ;
#42857 = ORIENTED_EDGE ( 'NONE', *, *, #43789, .T. ) ;
#42858 = VECTOR ( 'NONE', #39464, 1000.000000000000114 ) ;
#42859 = CARTESIAN_POINT ( 'NONE',  ( 0.3676999524040366896, -28.14442808720893296, -33.96824621564622504 ) ) ;
#42860 = CARTESIAN_POINT ( 'NONE',  ( 48.11856151137951088, 15.45621073281055402, -1.175286366004017813 ) ) ;
#42861 = CARTESIAN_POINT ( 'NONE',  ( 0.6254311100348668440, -48.10157347124187766, -0.6881768005100848962 ) ) ;
#42862 = LINE ( 'NONE', #24973, #50168 ) ;
#42863 = CARTESIAN_POINT ( 'NONE',  ( 1.500000000000001332, 0.000000000000000000, 0.000000000000000000 ) ) ;
#42864 = B_SPLINE_CURVE_WITH_KNOTS ( 'NONE', 3,
 ( #53024, #24215, #708, #385 ),
 .UNSPECIFIED., .F., .F.,
 ( 4, 4 ),
 ( 2.194270917860438266E-17, 0.005004741218457450097 ),
 .UNSPECIFIED. ) ;
#42865 =( BOUNDED_SURFACE ( )  B_SPLINE_SURFACE ( 3, 1, ( 
 ( #84, #9498 ),
 ( #27999, #19232 ),
 ( #38651, #5086 ),
 ( #37735, #52406 ) ),
 .UNSPECIFIED., .F., .F., .F. ) 
 B_SPLINE_SURFACE_WITH_KNOTS ( ( 4, 4 ),
 ( 2, 2 ),
 ( 0.000000000000000000, 1.000000000000000000 ),
 ( 0.000000000000000000, 1.000000000000000000 ),
 .UNSPECIFIED. ) 
 GEOMETRIC_REPRESENTATION_ITEM ( )  RATIONAL_B_SPLINE_SURFACE ( (
 ( 1.000000000000000000, 1.000000000000000000),
 ( 0.7269869731126817891, 0.9931720237060910339),
 ( 0.7269869731126817891, 0.9931720237060910339),
 ( 1.000000000000000000, 1.000000000000000000) ) ) 
 REPRESENTATION_ITEM ( '' )  SURFACE ( )  );
#42866 = ORIENTED_EDGE ( 'NONE', *, *, #16028, .F. ) ;
#42867 = CARTESIAN_POINT ( 'NONE',  ( 5.981074661064941900, 18.95903134304778348, 7.862380442164206507 ) ) ;
#42868 = CARTESIAN_POINT ( 'NONE',  ( -19.25580369308461925, -7.824392703123175252, -1.668825094707770740 ) ) ;
#42869 = LINE ( 'NONE', #14977, #32840 ) ;
#42870 = ORIENTED_EDGE ( 'NONE', *, *, #18323, .T. ) ;
#42871 = EDGE_CURVE ( 'NONE', #57538, #28712, #52883, .T. ) ;
#42872 = FACE_OUTER_BOUND ( 'NONE', #23980, .T. ) ;
#42873 = EDGE_CURVE ( 'NONE', #46397, #8504, #55872, .T. ) ;
#42874 = CARTESIAN_POINT ( 'NONE',  ( 5.860006189529246790, 31.78942168514563349, 36.27483683749448318 ) ) ;
#42875 = LINE ( 'NONE', #23746, #40721 ) ;
#42876 = ORIENTED_EDGE ( 'NONE', *, *, #14097, .F. ) ;
#42877 = COLOUR_RGB ( '', 0.09019608, 0.27058824, 0.51372549) ;
#42878 = LINE ( 'NONE', #48784, #53934 ) ;
#42879 = CIRCLE ( 'NONE', #12875, 47.09074272231896430 ) ;
#42880 = EDGE_LOOP ( 'NONE', ( #30187, #1544, #48235, #9981 ) ) ;
#42881 = EDGE_CURVE ( 'NONE', #58891, #49888, #36438, .T. ) ;
#42882 = ADVANCED_FACE ( 'NONE', ( #27853 ), #11740, .F. ) ;
#42883 = CARTESIAN_POINT ( 'NONE',  ( 0.8760168074886965917, 33.37827814204077015, 34.63873394077499768 ) ) ;
#42884 = CARTESIAN_POINT ( 'NONE',  ( 0.8760168074886965917, -19.22870327415332881, 44.09317760313719248 ) ) ;
#42885 = ORIENTED_EDGE ( 'NONE', *, *, #40798, .F. ) ;
#42886 = CARTESIAN_POINT ( 'NONE',  ( 3.783278058412224976, -22.99727281874601204, -36.37891728069894270 ) ) ;
#42887 = EDGE_CURVE ( 'NONE', #33696, #8188, #20780, .T. ) ;
#42888 = FACE_OUTER_BOUND ( 'NONE', #7094, .T. ) ;
#42889 = CARTESIAN_POINT ( 'NONE',  ( 0.5824935313925951874, -8.159134433442462253, -46.18080447925144938 ) ) ;
#42890 = DIRECTION ( 'NONE',  ( 0.1736481776669315524, -0.9848077530122079093, 5.551115123125782702E-17 ) ) ;
#42891 = ORIENTED_EDGE ( 'NONE', *, *, #8967, .T. ) ;
#42892 = DIRECTION ( 'NONE',  ( 1.000000000000000000, 0.000000000000000000, 0.000000000000000000 ) ) ;
#42893 = ORIENTED_EDGE ( 'NONE', *, *, #21351, .F. ) ;
#42894 = CARTESIAN_POINT ( 'NONE',  ( 3.238018933889920792, 10.33920672294401122, 8.515180368487932583 ) ) ;
#42895 = ADVANCED_FACE ( 'NONE', ( #42905 ), #20153, .F. ) ;
#42896 = ORIENTED_EDGE ( 'NONE', *, *, #52076, .F. ) ;
#42897 = EDGE_LOOP ( 'NONE', ( #51556, #49105, #7291, #24711 ) ) ;
#42898 = CARTESIAN_POINT ( 'NONE',  ( -31.75000000000000000, 15.43999999999999240, 0.000000000000000000 ) ) ;
#42899 = CARTESIAN_POINT ( 'NONE',  ( 0.9783242366443538618, -37.52440672474880756, 18.66154843956287479 ) ) ;
#42900 = AXIS2_PLACEMENT_3D ( 'NONE', #48006, #57670, #5054 ) ;
#42901 = AXIS2_PLACEMENT_3D ( 'NONE', #12690, #59647, #16441 ) ;
#42902 = CARTESIAN_POINT ( 'NONE',  ( 0.1310142868023677076, 21.00772081177026607, 37.66054729763597919 ) ) ;
#42903 = DIRECTION ( 'NONE',  ( 0.000000000000000000, 0.000000000000000000, -1.000000000000000000 ) ) ;
#42904 = ORIENTED_EDGE ( 'NONE', *, *, #38858, .F. ) ;
#42905 = FACE_OUTER_BOUND ( 'NONE', #36988, .T. ) ;
#42906 = FACE_OUTER_BOUND ( 'NONE', #34415, .T. ) ;
#42907 = CARTESIAN_POINT ( 'NONE',  ( 0.1154773475650540532, -38.35764556291236005, 21.80904988568074288 ) ) ;
#42908 = ORIENTED_EDGE ( 'NONE', *, *, #1121, .T. ) ;
#42909 = B_SPLINE_CURVE_WITH_KNOTS ( 'NONE', 3,
 ( #25313, #35048, #44158, #58196 ),
 .UNSPECIFIED., .F., .F.,
 ( 4, 4 ),
 ( 1.409462824231155572E-18, 0.004444878191957686055 ),
 .UNSPECIFIED. ) ;
#42910 = ORIENTED_EDGE ( 'NONE', *, *, #39161, .F. ) ;
#42911 = CARTESIAN_POINT ( 'NONE',  ( 3.680882792899937694, -47.94008871805917948, 1.849662971458055472 ) ) ;
#42912 = LINE ( 'NONE', #24087, #788 ) ;
#42913 = CARTESIAN_POINT ( 'NONE',  ( 0.1092565886968785149, 30.71235995742698677, 30.27341312544124818 ) ) ;
#42914 = CARTESIAN_POINT ( 'NONE',  ( -6.063463321072276813, -17.35644658106379623, -8.341115906049296314 ) ) ;
#42915 = CARTESIAN_POINT ( 'NONE',  ( 0.6001305935487315502, 41.92422178329137239, 23.60027211631843969 ) ) ;
#42916 = ORIENTED_EDGE ( 'NONE', *, *, #1423, .F. ) ;
#42917 = VERTEX_POINT ( 'NONE', #15005 ) ;
#42918 = CARTESIAN_POINT ( 'NONE',  ( 0.9790850452238877288, -41.05878386289116833, 8.397237519778984804 ) ) ;
#42919 = CARTESIAN_POINT ( 'NONE',  ( 3.050102900204245682, -39.18813633240142025, -19.99287923164596847 ) ) ;
#42920 = CARTESIAN_POINT ( 'NONE',  ( 0.5807400328401637335, 5.711437504336647208, -47.55718917606836982 ) ) ;
#42921 = CARTESIAN_POINT ( 'NONE',  ( 2.281351352603289140, 11.14238889600285454, 46.66131639318005142 ) ) ;
#42922 = CARTESIAN_POINT ( 'NONE',  ( 0.6028618097248863439, 0.1745704727159134717, 48.10721794025128162 ) ) ;
#42923 = AXIS2_PLACEMENT_3D ( 'NONE', #25257, #53437, #35605 ) ;
#42924 = ADVANCED_FACE ( 'NONE', ( #560 ), #48496, .F. ) ;
#42925 = EDGE_LOOP ( 'NONE', ( #42136, #60109, #48468, #48305 ) ) ;
#42926 = CARTESIAN_POINT ( 'NONE',  ( 5.901764892641288895, 48.57275408226675495, 6.219246602548982317 ) ) ;
#42927 = FACE_OUTER_BOUND ( 'NONE', #41734, .T. ) ;
#42928 = CARTESIAN_POINT ( 'NONE',  ( 0.7762783648524390623, -46.49451980369968851, -11.53708172997868253 ) ) ;
#42929 = CARTESIAN_POINT ( 'NONE',  ( 0.6039202388192952409, 22.86846745447396501, -43.45799016444105689 ) ) ;
#42930 = B_SPLINE_CURVE_WITH_KNOTS ( 'NONE', 3,
 ( #36329, #36024, #55393, #55089 ),
 .UNSPECIFIED., .F., .F.,
 ( 4, 4 ),
 ( 6.254634441385501517E-18, 0.004566006591234646368 ),
 .UNSPECIFIED. ) ;
#42931 = CARTESIAN_POINT ( 'NONE',  ( 3.376099380956838925, -6.821144471874409199, -11.54038005118914434 ) ) ;
#42932 = CARTESIAN_POINT ( 'NONE',  ( 0.9790850452238869517, -34.52257324172052222, 23.75982464230828128 ) ) ;
#42933 = DIRECTION ( 'NONE',  ( 0.9848077530122080203, 0.1736481776669315247, -2.220446049250313081E-16 ) ) ;
#42934 =( BOUNDED_SURFACE ( )  B_SPLINE_SURFACE ( 3, 1, ( 
 ( #25101, #49839 ),
 ( #11635, #44859 ),
 ( #54198, #20111 ),
 ( #20410, #30721 ) ),
 .UNSPECIFIED., .F., .F., .F. ) 
 B_SPLINE_SURFACE_WITH_KNOTS ( ( 4, 4 ),
 ( 2, 2 ),
 ( 0.000000000000000000, 1.000000000000000000 ),
 ( 0.000000000000000000, 1.000000000000000000 ),
 .UNSPECIFIED. ) 
 GEOMETRIC_REPRESENTATION_ITEM ( )  RATIONAL_B_SPLINE_SURFACE ( (
 ( 1.000000000000000000, 1.000000000000000000),
 ( 0.9953485035131437453, 0.8621029689291523912),
 ( 0.9953485035131437453, 0.8621029689291523912),
 ( 1.000000000000000000, 1.000000000000000000) ) ) 
 REPRESENTATION_ITEM ( '' )  SURFACE ( )  );
#42935 = B_SPLINE_CURVE_WITH_KNOTS ( 'NONE', 3,
 ( #12637, #1962, #22024, #21089 ),
 .UNSPECIFIED., .F., .F.,
 ( 4, 4 ),
 ( 9.029002393300562720E-17, 0.005004741218457447495 ),
 .UNSPECIFIED. ) ;
#42936 = DIRECTION ( 'NONE',  ( -1.000000000000000000, -0.000000000000000000, -0.000000000000000000 ) ) ;
#42937 = ORIENTED_EDGE ( 'NONE', *, *, #24176, .F. ) ;
#42938 = VECTOR ( 'NONE', #1031, 1000.000000000000114 ) ;
#42939 = CARTESIAN_POINT ( 'NONE',  ( 0.1100247026804066219, 37.26174279786183519, 21.70899701554537131 ) ) ;
#42940 = CARTESIAN_POINT ( 'NONE',  ( 2.533389852662419894, 23.86852016275539157, -36.98302687684928713 ) ) ;
#42941 = CARTESIAN_POINT ( 'NONE',  ( -6.015611763856276717, -4.870987357968047604, -18.20278301740941629 ) ) ;
#42942 = CARTESIAN_POINT ( 'NONE',  ( 0.6064515330803631477, 42.89337338949368927, -18.96029681483289053 ) ) ;
#42943 = VERTEX_POINT ( 'NONE', #14696 ) ;
#42944 = CARTESIAN_POINT ( 'NONE',  ( 0.9730545539215883499, -36.90443313492345823, 21.89037132892422832 ) ) ;
#42945 = FACE_OUTER_BOUND ( 'NONE', #2131, .T. ) ;
#42946 = EDGE_CURVE ( 'NONE', #15622, #61570, #17020, .T. ) ;
#42947 = CARTESIAN_POINT ( 'NONE',  ( 4.967162193818130511, 8.839793687085215623, 42.16965968614196925 ) ) ;
#42948 = VERTEX_POINT ( 'NONE', #45067 ) ;
#42949 = CARTESIAN_POINT ( 'NONE',  ( -6.078726893082806448, 19.25601281685051802, 0.003415553934478593023 ) ) ;
#42950 = CIRCLE ( 'NONE', #15935, 42.08604991992415023 ) ;
#42951 = EDGE_CURVE ( 'NONE', #44755, #21167, #14031, .T. ) ;
#42952 = CARTESIAN_POINT ( 'NONE',  ( -6.057079549204054558, -19.21686681020091214, 1.242280603864163835 ) ) ;
#42953 = VERTEX_POINT ( 'NONE', #10603 ) ;
#42954 = EDGE_CURVE ( 'NONE', #22153, #1157, #37901, .T. ) ;
#42955 = CARTESIAN_POINT ( 'NONE',  ( -6.016761891674565099, 14.94721834528414917, 11.47373234755508342 ) ) ;
#42956 = VECTOR ( 'NONE', #51902, 1000.000000000000114 ) ;
#42957 = ORIENTED_EDGE ( 'NONE', *, *, #18823, .T. ) ;
#42958 = CARTESIAN_POINT ( 'NONE',  ( 1.231276596079881935, 10.53918392497884149, -40.57341954055061706 ) ) ;
#42959 = EDGE_CURVE ( 'NONE', #38559, #49335, #28197, .T. ) ;
#42960 = ORIENTED_EDGE ( 'NONE', *, *, #14240, .F. ) ;
#42961 = CARTESIAN_POINT ( 'NONE',  ( 0.5839879327111934249, -6.341736898931618072, -47.47435452316581461 ) ) ;
#42962 = EDGE_LOOP ( 'NONE', ( #20, #55847, #26691, #61312 ) ) ;
#42963 = CARTESIAN_POINT ( 'NONE',  ( -6.016104459813374383, 4.871830707673057148, 18.20253432612968680 ) ) ;
#42964 = VERTEX_POINT ( 'NONE', #20616 ) ;
#42965 = CARTESIAN_POINT ( 'NONE',  ( 4.962356264823608143, 0.000000000000000000, 0.000000000000000000 ) ) ;
#42966 = CARTESIAN_POINT ( 'NONE',  ( 0.9762797500689124330, -34.83496347773955648, 23.29914386174426255 ) ) ;
#42967 = CARTESIAN_POINT ( 'NONE',  ( -6.016761891674565099, -18.20023637398595540, -4.880293656735155139 ) ) ;
#42968 = ORIENTED_EDGE ( 'NONE', *, *, #21326, .T. ) ;
#42969 = CARTESIAN_POINT ( 'NONE',  ( 0.1135584504625007513, 14.83285864174382418, 41.55644783483421634 ) ) ;
#42970 = EDGE_CURVE ( 'NONE', #33616, #20911, #25204, .T. ) ;
#42971 = CARTESIAN_POINT ( 'NONE',  ( 0.5848930533535030563, -41.93775812029581829, 20.98803292905553874 ) ) ;
#42972 = CARTESIAN_POINT ( 'NONE',  ( 0.5806925824938499181, 16.34374012233052653, 43.95571090492437349 ) ) ;
#42973 = ORIENTED_EDGE ( 'NONE', *, *, #23615, .F. ) ;
#42974 = CARTESIAN_POINT ( 'NONE',  ( 4.967162193818130511, 2.375726030842579828, 43.02067033766019932 ) ) ;
#42975 = ADVANCED_FACE ( 'NONE', ( #15314 ), #35349, .F. ) ;
#42976 = CARTESIAN_POINT ( 'NONE',  ( 0.7246131072078558777, -13.24054562911158150, 46.24389631750663199 ) ) ;
#42977 = B_SPLINE_CURVE_WITH_KNOTS ( 'NONE', 3,
 ( #60137, #21322, #45763, #54817 ),
 .UNSPECIFIED., .F., .F.,
 ( 4, 4 ),
 ( 2.308109569601360422E-17, 0.004559932413162187670 ),
 .UNSPECIFIED. ) ;
#42978 = ORIENTED_EDGE ( 'NONE', *, *, #30614, .F. ) ;
#42979 = CARTESIAN_POINT ( 'NONE',  ( 0.7056313189692724475, 46.36312287336356519, -7.085864900416160239 ) ) ;
#42980 = ORIENTED_EDGE ( 'NONE', *, *, #61613, .F. ) ;
#42981 = B_SPLINE_CURVE_WITH_KNOTS ( 'NONE', 3,
 ( #45202, #22525, #22219, #14067 ),
 .UNSPECIFIED., .F., .F.,
 ( 4, 4 ),
 ( 0.000000000000000000, 0.004445488388166995118 ),
 .UNSPECIFIED. ) ;
#42982 = AXIS2_PLACEMENT_3D ( 'NONE', #679, #38021, #4743 ) ;
#42983 = CARTESIAN_POINT ( 'NONE',  ( 5.901463166500145796, 12.99631574414091517, -15.34971163961172458 ) ) ;
#42984 = CARTESIAN_POINT ( 'NONE',  ( 0.5830081025819934260, 10.60549139512680483, -45.68101998259383123 ) ) ;
#42985 = ORIENTED_EDGE ( 'NONE', *, *, #30418, .F. ) ;
#42986 = CARTESIAN_POINT ( 'NONE',  ( 0.5834584762367756028, 4.512861497189343041, 46.67836833181272027 ) ) ;
#42987 = CARTESIAN_POINT ( 'NONE',  ( 0.8753041380234530822, 33.66554281472423327, 35.74590263041275762 ) ) ;
#42988 = DIRECTION ( 'NONE',  ( 0.000000000000000000, 0.000000000000000000, -1.000000000000000000 ) ) ;
#42989 = CARTESIAN_POINT ( 'NONE',  ( 0.8751705887134423323, 13.30665218149362516, -46.21789262997744885 ) ) ;
#42990 = CIRCLE ( 'NONE', #33996, 6.866799999999992465 ) ;
#42991 = VERTEX_POINT ( 'NONE', #30613 ) ;
#42992 = CARTESIAN_POINT ( 'NONE',  ( 0.9722240750034583101, 41.59310803641459842, 10.54237121715099867 ) ) ;
#42993 = CARTESIAN_POINT ( 'NONE',  ( 0.5804410086790514622, 36.46521478791908066, 29.49250688439903101 ) ) ;
#42994 = B_SPLINE_CURVE_WITH_KNOTS ( 'NONE', 3,
 ( #11369, #21074, #30454, #16376, #54878, #39903 ),
 .UNSPECIFIED., .F., .F.,
 ( 4, 2, 4 ),
 ( 3.127317220692750759E-18, 0.0002447193893791696538, 0.0004894387787583361635 ),
 .UNSPECIFIED. ) ;
#42995 = CARTESIAN_POINT ( 'NONE',  ( 0.6845945791218034371, -25.96635969083060402, 39.06602981005814001 ) ) ;
#42996 = CARTESIAN_POINT ( 'NONE',  ( 0.8557997880470599172, 46.50333260518575429, -11.51622788066409697 ) ) ;
#42997 = EDGE_CURVE ( 'NONE', #59309, #59890, #23775, .T. ) ;
#42998 = DIRECTION ( 'NONE',  ( -1.000000000000000000, -0.000000000000000000, -0.000000000000000000 ) ) ;
#42999 = CARTESIAN_POINT ( 'NONE',  ( -6.016761891674565099, -2.456125503350587991, -18.68243340030205246 ) ) ;
#43000 = AXIS2_PLACEMENT_3D ( 'NONE', #15507, #53680, #34613 ) ;
#43001 = B_SPLINE_CURVE_WITH_KNOTS ( 'NONE', 3,
 ( #49483, #58557, #945, #625, #34173, #10048 ),
 .UNSPECIFIED., .F., .F.,
 ( 4, 2, 4 ),
 ( 3.476216610979977084E-18, 0.0002291966416970802711, 0.0004583932833941570728 ),
 .UNSPECIFIED. ) ;
#43002 = DIRECTION ( 'NONE',  ( 0.09722883295013595717, -0.9196625129306750246, -0.3804831354386032372 ) ) ;
#43003 = DIRECTION ( 'NONE',  ( 0.000000000000000000, 0.000000000000000000, -1.000000000000000000 ) ) ;
#43004 = CARTESIAN_POINT ( 'NONE',  ( 2.618530812446115519, 12.26263843375515172, 45.38011114840057303 ) ) ;
#43005 = CARTESIAN_POINT ( 'NONE',  ( 0.1145239942831223490, -43.71898434612356965, -5.966228997287612579 ) ) ;
#43006 = CARTESIAN_POINT ( 'NONE',  ( 0.1154773475650540393, 39.83222568495971672, 18.98255586133109318 ) ) ;
#43007 = CARTESIAN_POINT ( 'NONE',  ( 0.9745511491811755800, 36.98831798234376578, 21.74846188963790183 ) ) ;
#43008 = DIRECTION ( 'NONE',  ( 1.000000000000000000, 0.000000000000000000, 0.000000000000000000 ) ) ;
#43009 = CARTESIAN_POINT ( 'NONE',  ( 5.959547316686252039, -20.52562247508876681, 0.003562808152837176282 ) ) ;
#43011 =( BOUNDED_SURFACE ( )  B_SPLINE_SURFACE ( 3, 1, ( 
 ( #4302, #56633 ),
 ( #37884, #32861 ),
 ( #51936, #23439 ),
 ( #61624, #19366 ) ),
 .UNSPECIFIED., .F., .F., .F. ) 
 B_SPLINE_SURFACE_WITH_KNOTS ( ( 4, 4 ),
 ( 2, 2 ),
 ( 0.000000000000000000, 1.000000000000000000 ),
 ( 0.000000000000000000, 1.000000000000000000 ),
 .UNSPECIFIED. ) 
 GEOMETRIC_REPRESENTATION_ITEM ( )  RATIONAL_B_SPLINE_SURFACE ( (
 ( 1.000000000000000000, 1.000000000000000000),
 ( 0.9751682680413298332, 0.9999560080971552356),
 ( 0.9751682680413298332, 0.9999560080971552356),
 ( 1.000000000000000000, 1.000000000000000000) ) ) 
 REPRESENTATION_ITEM ( '' )  SURFACE ( )  );
#43010 = CARTESIAN_POINT ( 'NONE',  ( 5.895881250540457863, -4.658141670565439263, 19.56602662231764356 ) ) ;
#43012 = CARTESIAN_POINT ( 'NONE',  ( 0.2285344041767100598, 21.07743229076804425, 38.75877988693069653 ) ) ;
#43013 = ORIENTED_EDGE ( 'NONE', *, *, #51184, .T. ) ;
#43014 = CARTESIAN_POINT ( 'NONE',  ( 0.5832367798473401255, 29.37285281143894977, -37.83194459509880403 ) ) ;
#43015 = CARTESIAN_POINT ( 'NONE',  ( 0.5839879882012694035, 23.94800997596683345, 41.47910964649803844 ) ) ;
#43016 = DIRECTION ( 'NONE',  ( 1.000000000000000000, 1.836909530733573776E-16, -1.925929944387235853E-32 ) ) ;
#43017 = EDGE_LOOP ( 'NONE', ( #16484, #39702, #48996, #45575 ) ) ;
#43018 = FACE_OUTER_BOUND ( 'NONE', #12044, .T. ) ;
#43019 = B_SPLINE_CURVE_WITH_KNOTS ( 'NONE', 3,
 ( #60197, #40217, #36740, #35496 ),
 .UNSPECIFIED., .F., .F.,
 ( 4, 4 ),
 ( 0.000000000000000000, 0.005013413432710149380 ),
 .UNSPECIFIED. ) ;
#43020 = UNCERTAINTY_MEASURE_WITH_UNIT (LENGTH_MEASURE( 1.000000000000000082E-05 ), #52425, 'distance_accuracy_value', 'NONE');
#43021 = VERTEX_POINT ( 'NONE', #15618 ) ;
#43022 = ORIENTED_EDGE ( 'NONE', *, *, #5684, .T. ) ;
#43023 = LINE ( 'NONE', #28892, #40577 ) ;
#43024 = EDGE_CURVE ( 'NONE', #18600, #15275, #58148, .T. ) ;
#43025 = ORIENTED_EDGE ( 'NONE', *, *, #32383, .F. ) ;
#43026 = VECTOR ( 'NONE', #27297, 1000.000000000000114 ) ;
#43027 = CARTESIAN_POINT ( 'NONE',  ( 4.553261556744875094, -20.51767157960516741, 38.84024612145369559 ) ) ;
#43028 = CARTESIAN_POINT ( 'NONE',  ( 4.694002226626920127, 44.00857453008735121, -11.89664403417540939 ) ) ;
#43029 = ORIENTED_EDGE ( 'NONE', *, *, #17540, .F. ) ;
#43030 = EDGE_CURVE ( 'NONE', #5480, #59176, #18561, .T. ) ;
#43031 = ORIENTED_EDGE ( 'NONE', *, *, #30338, .T. ) ;
#43032 = CARTESIAN_POINT ( 'NONE',  ( 4.956445790443991584, 30.81386304088947625, 35.60960396630300551 ) ) ;
#43033 = ORIENTED_EDGE ( 'NONE', *, *, #3878, .F. ) ;
#43034 = CARTESIAN_POINT ( 'NONE',  ( 4.694002226626921015, 23.33724324709813658, 39.16194388780908753 ) ) ;
#43035 = CARTESIAN_POINT ( 'NONE',  ( 4.549368137175248350, -18.79584381673505789, -38.59302160394747006 ) ) ;
#43036 = DIRECTION ( 'NONE',  ( -1.000000000000000000, 0.000000000000000000, 0.000000000000000000 ) ) ;
#43037 = ORIENTED_EDGE ( 'NONE', *, *, #56679, .F. ) ;
#43038 = CARTESIAN_POINT ( 'NONE',  ( 4.967162193818130511, -24.30453456948135482, 35.57684288741969425 ) ) ;
#43039 = CARTESIAN_POINT ( 'NONE',  ( 5.901463166500146684, -9.653076390470776147, 17.64471554149775301 ) ) ;
#43040 = ORIENTED_EDGE ( 'NONE', *, *, #19412, .T. ) ;
#43041 = ORIENTED_EDGE ( 'NONE', *, *, #36306, .F. ) ;
#43042 = DIRECTION ( 'NONE',  ( 0.09835009131224552170, -0.3736726418952377449, 0.9223318362920724933 ) ) ;
#43043 = AXIS2_PLACEMENT_3D ( 'NONE', #38985, #23628, #28325 ) ;
#43044 = VERTEX_POINT ( 'NONE', #40674 ) ;
#43045 = FACE_OUTER_BOUND ( 'NONE', #27891, .T. ) ;
#43046 = CARTESIAN_POINT ( 'NONE',  ( 4.956445790443988031, 0.000000000000000000, 0.000000000000000000 ) ) ;
#43047 = CARTESIAN_POINT ( 'NONE',  ( -1.600000000000000089, -11.64055411052240352, -1.199999999999999956 ) ) ;
#43048 = CARTESIAN_POINT ( 'NONE',  ( 2.526464513654344657, -15.32058692775020070, 40.15570173027688128 ) ) ;
#43049 = ADVANCED_FACE ( 'NONE', ( #54720 ), #3655, .F. ) ;
#43050 = ORIENTED_EDGE ( 'NONE', *, *, #22179, .T. ) ;
#43051 = CARTESIAN_POINT ( 'NONE',  ( -2.739355103387248747, 6.670587007382340339, -13.35480572408145861 ) ) ;
#43052 = FACE_OUTER_BOUND ( 'NONE', #53501, .T. ) ;
#43053 = CARTESIAN_POINT ( 'NONE',  ( 0.5817216825391112733, 36.52003817910519246, -29.41975124986882406 ) ) ;
#43054 = EDGE_LOOP ( 'NONE', ( #6755, #13350, #22895, #2107, #60504, #81 ) ) ;
#43055 = LINE ( 'NONE', #395, #23515 ) ;
#43056 = PLANE ( 'NONE',  #46435 ) ;
#43057 = ORIENTED_EDGE ( 'NONE', *, *, #53686, .F. ) ;
#43058 = ORIENTED_EDGE ( 'NONE', *, *, #38865, .F. ) ;
#43059 = CARTESIAN_POINT ( 'NONE',  ( -6.072942160501519915, 17.85441038494885646, 7.212779775845826968 ) ) ;
#43060 = CARTESIAN_POINT ( 'NONE',  ( 0.1064266418746774301, 37.62465821955101575, -21.07422140941967825 ) ) ;
#43061 = LINE ( 'NONE', #100, #16819 ) ;
#43062 = CARTESIAN_POINT ( 'NONE',  ( -6.016761891674564211, -11.46828378093569789, 14.95139917749700587 ) ) ;
#43063 = CARTESIAN_POINT ( 'NONE',  ( 0.9745511491811764682, -42.58443036172448615, 5.262846425219458446 ) ) ;
#43064 = CARTESIAN_POINT ( 'NONE',  ( 0.6026777506516368677, -42.70253602701208706, 24.24953210886665644 ) ) ;
#43065 = CARTESIAN_POINT ( 'NONE',  ( 5.901463166500146684, 12.99631574414070023, 15.34971163961190399 ) ) ;
#43066 = CARTESIAN_POINT ( 'NONE',  ( 4.549368137175248350, -13.59764261105721950, -40.71620287708339703 ) ) ;
#43067 = EDGE_CURVE ( 'NONE', #47719, #36320, #8013, .T. ) ;
#43068 = FACE_OUTER_BOUND ( 'NONE', #6150, .T. ) ;
#43069 = B_SPLINE_CURVE_WITH_KNOTS ( 'NONE', 3,
 ( #5584, #25337, #43864, #34751, #6816, #15339 ),
 .UNSPECIFIED., .F., .F.,
 ( 4, 2, 4 ),
 ( 6.805474077711127748E-18, 0.0002291472222819938571, 0.0004582944445639809379 ),
 .UNSPECIFIED. ) ;
#43070 = CARTESIAN_POINT ( 'NONE',  ( 2.648799415243696664, 9.556201303926476598, 48.09570126246661204 ) ) ;
#43071 = DIRECTION ( 'NONE',  ( 0.09722883295013594329, -0.9196625129306804647, 0.3804831354385900810 ) ) ;
#43072 = ORIENTED_EDGE ( 'NONE', *, *, #15280, .T. ) ;
#43073 = CARTESIAN_POINT ( 'NONE',  ( 0.5980894510889448457, 23.44630161211528119, 42.01322166096928612 ) ) ;
#43074 = CARTESIAN_POINT ( 'NONE',  ( 0.1087620492084206275, -33.99140154262286728, -26.53886348602990353 ) ) ;
#43075 = CARTESIAN_POINT ( 'NONE',  ( 0.7056759521544978542, -45.78629854946090916, -10.16679370581612041 ) ) ;
#43076 = CARTESIAN_POINT ( 'NONE',  ( -6.015611763856276717, -14.94556629257433578, 11.47596948473805689 ) ) ;
#43077 = B_SPLINE_CURVE_WITH_KNOTS ( 'NONE', 3,
 ( #59150, #2758, #45099, #54129 ),
 .UNSPECIFIED., .F., .F.,
 ( 4, 4 ),
 ( 0.000000000000000000, 0.004444103432399269631 ),
 .UNSPECIFIED. ) ;
#43078 = CARTESIAN_POINT ( 'NONE',  ( 3.660087539127316880, 25.63019641081328004, 40.62968541507452613 ) ) ;
#43079 = CARTESIAN_POINT ( 'NONE',  ( 5.959547316686252039, 0.003562808152622177690, 20.52562247508876681 ) ) ;
#43080 = ADVANCED_FACE ( 'NONE', ( #55337 ), #39907, .T. ) ;
#43081 = FACE_OUTER_BOUND ( 'NONE', #6703, .T. ) ;
#43082 = CLOSED_SHELL ( 'NONE', ( #55776, #60841, #26588, #29559, #9189, #27099, #5274, #60162, #28821, #59041, #27866, #16226, #28929, #52385, #12454, #15683, #32818, #43401, #33559, #3094, #32266, #11830, #3068, #46610, #59134, #61792, #54024, #7627, #61100 ) ) ;
#43083 = CARTESIAN_POINT ( 'NONE',  ( -2.569797478183783568, -9.259773107242986967, -11.33042594333545061 ) ) ;
#43084 = CARTESIAN_POINT ( 'NONE',  ( 0.5839254288179557273, 12.30867641975577342, 46.28738487712331562 ) ) ;
#43085 = EDGE_CURVE ( 'NONE', #43207, #54066, #2782, .T. ) ;
#43086 = CARTESIAN_POINT ( 'NONE',  ( 0.6000166863083090663, -8.353387137038760457, 48.39467331274393302 ) ) ;
#43088 = VERTEX_POINT ( 'NONE', #3034 ) ;
#43087 = CARTESIAN_POINT ( 'NONE',  ( 4.956653778116975495, 3.690426056929986043, 47.94889704119053420 ) ) ;
#43089 = VERTEX_POINT ( 'NONE', #26541 ) ;
#43090 = VECTOR ( 'NONE', #57129, 1000.000000000000114 ) ;
#43091 = CARTESIAN_POINT ( 'NONE',  ( 0.1097557419366048670, -43.12388302211984126, 0.2231007852158213567 ) ) ;
#43092 = CARTESIAN_POINT ( 'NONE',  ( 0.1087620492084206969, 39.70193592734180754, 16.83695155255847453 ) ) ;
#43093 = FACE_OUTER_BOUND ( 'NONE', #25191, .T. ) ;
#43094 = ORIENTED_EDGE ( 'NONE', *, *, #42997, .F. ) ;
#43095 = CARTESIAN_POINT ( 'NONE',  ( 0.3676999524040366896, 29.04098611012985742, -33.20499524279568249 ) ) ;
#43096 = CARTESIAN_POINT ( 'NONE',  ( 4.975801465491695552, 47.76942479135485797, -3.702618843596948039 ) ) ;
#43097 = CARTESIAN_POINT ( 'NONE',  ( 0.8554163680231708922, 45.48289776771382265, -11.51136324522475540 ) ) ;
#43098 = ORIENTED_EDGE ( 'NONE', *, *, #27026, .F. ) ;
#43099 = EDGE_LOOP ( 'NONE', ( #25365, #28434, #43050, #44941 ) ) ;
#43100 = FACE_OUTER_BOUND ( 'NONE', #14089, .T. ) ;
#43101 = ADVANCED_FACE ( 'NONE', ( #60973 ), #18141, .F. ) ;
#43102 = CARTESIAN_POINT ( 'NONE',  ( 4.975801465491694664, -27.09127437476410805, 39.51822597168447260 ) ) ;
#43103 = CARTESIAN_POINT ( 'NONE',  ( 0.1129192098497455998, 14.78321943369591196, 41.57412910645692961 ) ) ;
#43104 = ADVANCED_FACE ( 'NONE', ( #31550 ), #5651, .F. ) ;
#43105 = CARTESIAN_POINT ( 'NONE',  ( -6.016761891674565099, 13.32172022638591713, 13.32657647165359904 ) ) ;
#43106 = B_SPLINE_CURVE_WITH_KNOTS ( 'NONE', 3,
 ( #16530, #35967, #35656, #19548 ),
 .UNSPECIFIED., .F., .F.,
 ( 4, 4 ),
 ( 0.000000000000000000, 0.005014147105413706458 ),
 .UNSPECIFIED. ) ;
#43107 = DIRECTION ( 'NONE',  ( 0.9848077530122077983, 0.1736481776669316079, -1.387778780781445367E-17 ) ) ;
#43108 = EDGE_CURVE ( 'NONE', #60397, #14724, #52809, .T. ) ;
#43109 =( BOUNDED_SURFACE ( )  B_SPLINE_SURFACE ( 3, 1, ( 
 ( #55905, #50897 ),
 ( #21473, #46228 ),
 ( #60593, #36837 ),
 ( #2975, #49983 ) ),
 .UNSPECIFIED., .F., .F., .F. ) 
 B_SPLINE_SURFACE_WITH_KNOTS ( ( 4, 4 ),
 ( 2, 2 ),
 ( 0.000000000000000000, 1.000000000000000000 ),
 ( 0.000000000000000000, 1.000000000000000000 ),
 .UNSPECIFIED. ) 
 GEOMETRIC_REPRESENTATION_ITEM ( )  RATIONAL_B_SPLINE_SURFACE ( (
 ( 1.000000000000000000, 1.000000000000000000),
 ( 0.7211978278499968642, 0.9934217856018975334),
 ( 0.7211978278499968642, 0.9934217856018975334),
 ( 1.000000000000000000, 1.000000000000000000) ) ) 
 REPRESENTATION_ITEM ( '' )  SURFACE ( )  );
#43110 = CARTESIAN_POINT ( 'NONE',  ( 0.5837374860065631665, 37.88763545422917645, -29.30115996485956842 ) ) ;
#43111 = ORIENTED_EDGE ( 'NONE', *, *, #13257, .T. ) ;
#43112 = CARTESIAN_POINT ( 'NONE',  ( 0.6067099128993235224, -11.71051825714735806, 46.44339333106611178 ) ) ;
#43113 = CARTESIAN_POINT ( 'NONE',  ( 2.009741617377216460, 44.01584547398758218, 1.452385910524921497 ) ) ;
#43114 = ORIENTED_EDGE ( 'NONE', *, *, #30537, .F. ) ;
#43115 = CARTESIAN_POINT ( 'NONE',  ( 0.9722240750034581991, -37.44729079646477032, -20.94823713380376162 ) ) ;
#43116 = DIRECTION ( 'NONE',  ( 0.09835009131224549395, 0.4908642831975363330, -0.8656670924898565156 ) ) ;
#43117 = CARTESIAN_POINT ( 'NONE',  ( 0.8744876279028263033, -39.87136468799916145, 28.64654129726773846 ) ) ;
#43118 = CARTESIAN_POINT ( 'NONE',  ( 0.1129192098497447394, -41.07894348801345075, -16.10814047907924973 ) ) ;
#43119 = EDGE_CURVE ( 'NONE', #19259, #1466, #12588, .T. ) ;
#43120 = VERTEX_POINT ( 'NONE', #51563 ) ;
#43121 = ORIENTED_EDGE ( 'NONE', *, *, #55068, .F. ) ;
#43122 = CARTESIAN_POINT ( 'NONE',  ( -6.016761891674565099, -11.47373234755513671, 14.94721834528410831 ) ) ;
#43123 = CARTESIAN_POINT ( 'NONE',  ( 1.088908134280553996, 10.35121946298470696, -41.64642044161479362 ) ) ;
#43124 = CARTESIAN_POINT ( 'NONE',  ( 0.1095718737110177726, -37.21776476380641441, -21.78439022773142852 ) ) ;
#43125 =( BOUNDED_SURFACE ( )  B_SPLINE_SURFACE ( 3, 1, ( 
 ( #4908, #37543 ),
 ( #38165, #46944 ),
 ( #13729, #520 ),
 ( #9948, #56614 ) ),
 .UNSPECIFIED., .F., .F., .F. ) 
 B_SPLINE_SURFACE_WITH_KNOTS ( ( 4, 4 ),
 ( 2, 2 ),
 ( 0.000000000000000000, 1.000000000000000000 ),
 ( 0.000000000000000000, 1.000000000000000000 ),
 .UNSPECIFIED. ) 
 GEOMETRIC_REPRESENTATION_ITEM ( )  RATIONAL_B_SPLINE_SURFACE ( (
 ( 1.000000000000000000, 1.000000000000000000),
 ( 0.9953390228620291325, 0.8624445117760984880),
 ( 0.9953390228620291325, 0.8624445117760984880),
 ( 1.000000000000000000, 1.000000000000000000) ) ) 
 REPRESENTATION_ITEM ( '' )  SURFACE ( )  );
#43126 = AXIS2_PLACEMENT_3D ( 'NONE', #15682, #53247, #43577 ) ;
#43127 = CARTESIAN_POINT ( 'NONE',  ( 0.5832367798473401255, 28.94059862654991733, 38.16362489683097436 ) ) ;
#43128 = ORIENTED_EDGE ( 'NONE', *, *, #55388, .T. ) ;
#43129 = CARTESIAN_POINT ( 'NONE',  ( 0.7762783648524391733, 41.92424098267939314, 23.17763242108770072 ) ) ;
#43130 = ORIENTED_EDGE ( 'NONE', *, *, #29840, .T. ) ;
#43131 = CARTESIAN_POINT ( 'NONE',  ( 0.1064266379913941518, -26.69589650908261547, -33.86837498006617153 ) ) ;
#43132 = LINE ( 'NONE', #47823, #8390 ) ;
#43133 = VERTEX_POINT ( 'NONE', #14624 ) ;
#43134 = CARTESIAN_POINT ( 'NONE',  ( 0.7245667037590747261, -33.42814706018044291, 34.58857005974894605 ) ) ;
#43135 = CARTESIAN_POINT ( 'NONE',  ( 1.157644175074335813, -30.52765897203332912, -28.72393275939801782 ) ) ;
#43136 = CARTESIAN_POINT ( 'NONE',  ( 5.895596859100789899, 14.91436009500240445, 13.49407448360528861 ) ) ;
#43137 = B_SPLINE_CURVE_WITH_KNOTS ( 'NONE', 3,
 ( #59293, #30474, #2590, #16395, #20793, #30790 ),
 .UNSPECIFIED., .F., .F.,
 ( 4, 2, 4 ),
 ( 8.741117365843378158E-19, 0.0002450742804987339051, 0.0004901485609974669429 ),
 .UNSPECIFIED. ) ;
#43138 = ORIENTED_EDGE ( 'NONE', *, *, #1264, .T. ) ;
#43139 = CARTESIAN_POINT ( 'NONE',  ( 0.5839879882012681822, -18.32902119196533874, -44.25009266679224851 ) ) ;
#43140 = CARTESIAN_POINT ( 'NONE',  ( 4.975801465491694664, 21.70134120755201224, -42.71626295676241369 ) ) ;
#43141 = CARTESIAN_POINT ( 'NONE',  ( 1.154321713695929619, 26.77578845938227659, -33.53917066545392345 ) ) ;
#43142 = CARTESIAN_POINT ( 'NONE',  ( 0.5998501479064708430, 29.69975237324613460, -37.84527566984826308 ) ) ;
#43143 = CARTESIAN_POINT ( 'NONE',  ( -6.015611763856276717, -2.453375430803944823, -18.68284711750060723 ) ) ;
#43144 = ORIENTED_EDGE ( 'NONE', *, *, #29760, .F. ) ;
#43145 = FACE_OUTER_BOUND ( 'NONE', #7526, .T. ) ;
#43146 = EDGE_CURVE ( 'NONE', #37089, #22212, #3553, .T. ) ;
#43147 = CARTESIAN_POINT ( 'NONE',  ( 0.5549461598389363592, -17.04665221628824057, 40.67713539181095683 ) ) ;
#43148 = VERTEX_POINT ( 'NONE', #28389 ) ;
#43149 = EDGE_CURVE ( 'NONE', #26123, #8407, #58805, .T. ) ;
#43150 = DIRECTION ( 'NONE',  ( 0.000000000000000000, 0.000000000000000000, -1.000000000000000000 ) ) ;
#43151 = DIRECTION ( 'NONE',  ( -0.07836865515943411409, 0.8593913859058619487, -0.5052769534812598939 ) ) ;
#43152 = CARTESIAN_POINT ( 'NONE',  ( 0.1129192098497447394, -35.06977877439262414, 26.77802092202325213 ) ) ;
#43153 = CARTESIAN_POINT ( 'NONE',  ( 4.553261556744873317, 27.21079963941887314, -34.48350256002191117 ) ) ;
#43154 = CARTESIAN_POINT ( 'NONE',  ( 0.8557997880470606944, -28.43566216844945771, -38.55640757422467857 ) ) ;
#43155 = CARTESIAN_POINT ( 'NONE',  ( 0.6039202388192953519, 11.09723268158243492, 47.83738224087738189 ) ) ;
#43156 = CARTESIAN_POINT ( 'NONE',  ( 53.13262160778436538, 15.49700215203310272, 0.3490842977376169554 ) ) ;
#43157 = EDGE_CURVE ( 'NONE', #5597, #2574, #45893, .T. ) ;
#43158 = DIRECTION ( 'NONE',  ( 4.404220133270841848E-18, -0.02825280623428194984, 0.9996008097935338288 ) ) ;
#43159 = CARTESIAN_POINT ( 'NONE',  ( 4.958415959904821868, -31.21198115812957852, 33.00024524162211037 ) ) ;
#43160 = CARTESIAN_POINT ( 'NONE',  ( 0.5980271706414734822, -30.07077130958565192, 38.83037413788673575 ) ) ;
#43161 = EDGE_CURVE ( 'NONE', #39811, #51992, #20023, .T. ) ;
#43162 = CARTESIAN_POINT ( 'NONE',  ( 1.227938101723748288, 37.58536632582807613, -20.72293514920711033 ) ) ;
#43164 = ORIENTED_EDGE ( 'NONE', *, *, #29056, .T. ) ;
#43163 = CARTESIAN_POINT ( 'NONE',  ( 0.1095718737110177865, -5.883530294870451094, 42.72125633542923140 ) ) ;
#43165 = VERTEX_POINT ( 'NONE', #8656 ) ;
#43166 = CYLINDRICAL_SURFACE ( 'NONE', #5468, 85.00000000000001421 ) ;
#43167 = CARTESIAN_POINT ( 'NONE',  ( 1.129531546211735016, 0.000000000000000000, 0.000000000000000000 ) ) ;
#43168 = B_SPLINE_CURVE_WITH_KNOTS ( 'NONE', 3,
 ( #893, #44767, #30627, #40081, #58503, #20032 ),
 .UNSPECIFIED., .F., .F.,
 ( 4, 2, 4 ),
 ( 3.476216610979977084E-18, 0.0002291459268755725929, 0.0004582918537511417164 ),
 .UNSPECIFIED. ) ;
#43169 = CARTESIAN_POINT ( 'NONE',  ( 0.5988103622719989083, -48.10388392585942796, -0.6065097949911955055 ) ) ;
#43170 = CARTESIAN_POINT ( 'NONE',  ( 0.9756354156337456729, 42.55820231551297184, -5.471460801652982653 ) ) ;
#43171 = CARTESIAN_POINT ( 'NONE',  ( 1.227938101723747621, 30.94118573761354440, -29.74462687941193551 ) ) ;
#43172 = AXIS2_PLACEMENT_3D ( 'NONE', #24334, #30250, #48149 ) ;
#43173 = ORIENTED_EDGE ( 'NONE', *, *, #40858, .F. ) ;
#43174 = CARTESIAN_POINT ( 'NONE',  ( 0.08486401232817714080, 5.403818426594913263E-15, -44.12552607296456131 ) ) ;
#43175 = EDGE_CURVE ( 'NONE', #29061, #32533, #43211, .T. ) ;
#43176 = CARTESIAN_POINT ( 'NONE',  ( 4.834790513006553603, 29.81904690970663196, -36.65260948856298029 ) ) ;
#43177 = CARTESIAN_POINT ( 'NONE',  ( 2.681483223904247648, -3.070647092368467224, -5.599999999999980105 ) ) ;
#43178 = EDGE_CURVE ( 'NONE', #3369, #21629, #46200, .T. ) ;
#43179 = VERTEX_POINT ( 'NONE', #28700 ) ;
#43180 = CARTESIAN_POINT ( 'NONE',  ( 0.3676999524040323597, -35.84016207189440451, 25.71834687500696859 ) ) ;
#43181 = EDGE_CURVE ( 'NONE', #8457, #29507, #34043, .T. ) ;
#43182 = CARTESIAN_POINT ( 'NONE',  ( 4.975610109902397937, -27.50982196586606321, 40.44328253918227034 ) ) ;
#43183 = ORIENTED_EDGE ( 'NONE', *, *, #53168, .F. ) ;
#43184 = DIRECTION ( 'NONE',  ( -3.273063162220399693E-16, 1.000000000000000000, 1.047380211910527902E-14 ) ) ;
#43185 = VERTEX_POINT ( 'NONE', #30233 ) ;
#43186 = B_SPLINE_CURVE_WITH_KNOTS ( 'NONE', 3,
 ( #48350, #58033, #15154, #34262, #31405, #30457 ),
 .UNSPECIFIED., .F., .F.,
 ( 4, 2, 4 ),
 ( 1.154609648881453222E-16, 0.0002448718616795960779, 0.0004897437233590766882 ),
 .UNSPECIFIED. ) ;
#43187 = CARTESIAN_POINT ( 'NONE',  ( 0.7245667037590785009, -13.24050682223062125, -46.24390958543271068 ) ) ;
#43188 = CARTESIAN_POINT ( 'NONE',  ( 0.6009453534118438522, 33.70725662590610483, 34.32439302680979409 ) ) ;
#43189 = ORIENTED_EDGE ( 'NONE', *, *, #13128, .T. ) ;
#43190 = CARTESIAN_POINT ( 'NONE',  ( 4.956653778116970166, 43.37017594958054900, 20.77844580450576117 ) ) ;
#43191 = DIRECTION ( 'NONE',  ( -0.07439287786467650709, -0.8701500408883610094, -0.4871392060438115013 ) ) ;
#43192 = CARTESIAN_POINT ( 'NONE',  ( 0.9780106845699476636, 40.33556544546049594, 11.37424312428799844 ) ) ;
#43193 = CARTESIAN_POINT ( 'NONE',  ( 4.909518593419350374, 0.8656805903097125610, 8.896908036367455278E-17 ) ) ;
#43194 = EDGE_CURVE ( 'NONE', #60182, #20219, #58722, .T. ) ;
#43195 = ORIENTED_EDGE ( 'NONE', *, *, #59946, .F. ) ;
#43196 = CARTESIAN_POINT ( 'NONE',  ( 0.6024113833632038784, -7.622554341288246604, -48.51225138472728560 ) ) ;
#43197 = ORIENTED_EDGE ( 'NONE', *, *, #43200, .T. ) ;
#43198 = B_SPLINE_CURVE_WITH_KNOTS ( 'NONE', 3,
 ( #6051, #52764, #44626, #48082, #48381, #57757 ),
 .UNSPECIFIED., .F., .F.,
 ( 4, 2, 4 ),
 ( 1.870625823323990238E-17, 0.0002293319059085113093, 0.0004586638118170039162 ),
 .UNSPECIFIED. ) ;
#43199 = CARTESIAN_POINT ( 'NONE',  ( 5.000000000000002665, 0.000000000000000000, -2.700000000000000622 ) ) ;
#43200 = EDGE_CURVE ( 'NONE', #24696, #20064, #14904, .T. ) ;
#43201 = ORIENTED_EDGE ( 'NONE', *, *, #10675, .T. ) ;
#43202 = ORIENTED_EDGE ( 'NONE', *, *, #25666, .F. ) ;
#43203 = CARTESIAN_POINT ( 'NONE',  ( 2.618530812446111078, -21.05599821100593161, 42.02822537933662517 ) ) ;
#43204 = CARTESIAN_POINT ( 'NONE',  ( 5.959828726073459926, -18.96145866559677629, 7.858992891709805306 ) ) ;
#43205 = DIRECTION ( 'NONE',  ( 0.000000000000000000, 0.000000000000000000, 1.000000000000000000 ) ) ;
#43206 = CARTESIAN_POINT ( 'NONE',  ( 0.3676999524040323597, -43.63756228305270213, -6.458617600968101335 ) ) ;
#43207 = VERTEX_POINT ( 'NONE', #11149 ) ;
#43208 = CARTESIAN_POINT ( 'NONE',  ( 0.8760168074887090262, 19.22870327415240155, 44.09317760313759749 ) ) ;
#43209 = CARTESIAN_POINT ( 'NONE',  ( 5.960221823109900008, 16.28072933292531133, 12.49951306783095006 ) ) ;
#43210 = ORIENTED_EDGE ( 'NONE', *, *, #28989, .T. ) ;
#43211 = B_SPLINE_CURVE_WITH_KNOTS ( 'NONE', 3,
 ( #51882, #8980, #33420, #28088 ),
 .UNSPECIFIED., .F., .F.,
 ( 4, 4 ),
 ( 6.206335383118182794E-17, 0.005004948556313865149 ),
 .UNSPECIFIED. ) ;
#43212 = VECTOR ( 'NONE', #11026, 1000.000000000000114 ) ;
#43213 = EDGE_LOOP ( 'NONE', ( #60481, #53980, #13593, #34917 ) ) ;
#43214 = VECTOR ( 'NONE', #53378, 1000.000000000000114 ) ;
#43215 = FILL_AREA_STYLE ('',( #61960 ) ) ;
#43216 = CARTESIAN_POINT ( 'NONE',  ( 1.231276596079881047, 24.17959027891106416, 34.24360064248583768 ) ) ;
#43217 = CARTESIAN_POINT ( 'NONE',  ( -6.077587904424778920, -12.95044751835546393, 14.25068175450744157 ) ) ;
#43218 = CARTESIAN_POINT ( 'NONE',  ( 0.1073791018717578927, -42.68962945260949482, -6.109314776652552403 ) ) ;
#43219 = CARTESIAN_POINT ( 'NONE',  ( 0.9788927965476016402, 38.63831210738078425, 16.23014017574742951 ) ) ;
#43220 = ORIENTED_EDGE ( 'NONE', *, *, #19348, .T. ) ;
#43221 = ORIENTED_EDGE ( 'NONE', *, *, #58371, .T. ) ;
#43222 = ADVANCED_FACE ( 'NONE', ( #15849 ), #48144, .F. ) ;
#43223 = DIRECTION ( 'NONE',  ( 0.000000000000000000, 0.000000000000000000, -1.000000000000000000 ) ) ;
#43224 = CARTESIAN_POINT ( 'NONE',  ( 0.9790724872846795490, -41.07690974463345412, 8.307989877984264027 ) ) ;
#43225 = CARTESIAN_POINT ( 'NONE',  ( -2.708315649062916552, 4.041664582652610527, 14.06540004355483831 ) ) ;
#43226 = CARTESIAN_POINT ( 'NONE',  ( 0.9758171775293935646, -21.44911662810676489, 37.16279804060124548 ) ) ;
#43227 = CARTESIAN_POINT ( 'NONE',  ( 0.5834584762367727162, 4.875245331832543272, -46.64191218172384623 ) ) ;
#43228 = EDGE_CURVE ( 'NONE', #59719, #23902, #40228, .T. ) ;
#43229 = LINE ( 'NONE', #4968, #23857 ) ;
#43230 =( BOUNDED_SURFACE ( )  B_SPLINE_SURFACE ( 3, 1, ( 
 ( #7854, #46101 ),
 ( #22275, #16652 ),
 ( #41403, #40795 ),
 ( #59543, #60459 ) ),
 .UNSPECIFIED., .F., .F., .F. ) 
 B_SPLINE_SURFACE_WITH_KNOTS ( ( 4, 4 ),
 ( 2, 2 ),
 ( 0.000000000000000000, 1.000000000000000000 ),
 ( 0.000000000000000000, 1.000000000000000000 ),
 .UNSPECIFIED. ) 
 GEOMETRIC_REPRESENTATION_ITEM ( )  RATIONAL_B_SPLINE_SURFACE ( (
 ( 1.000000000000000000, 1.000000000000000000),
 ( 0.9953390228620291325, 0.8624445117760984880),
 ( 0.9953390228620291325, 0.8624445117760984880),
 ( 1.000000000000000000, 1.000000000000000000) ) ) 
 REPRESENTATION_ITEM ( '' )  SURFACE ( )  );
#43231 = ORIENTED_EDGE ( 'NONE', *, *, #19156, .T. ) ;
#43232 = CARTESIAN_POINT ( 'NONE',  ( 2.281351352603022242, 47.37344280316144562, 7.562287671717293769 ) ) ;
#43233 = CARTESIAN_POINT ( 'NONE',  ( 4.553261556744875094, 43.59419396814060832, -5.393126930804686303 ) ) ;
#43234 = EDGE_CURVE ( 'NONE', #16525, #12730, #11809, .T. ) ;
#43235 = CARTESIAN_POINT ( 'NONE',  ( 2.528190830796658517, 10.90478310419556962, -40.53812824494315947 ) ) ;
#43236 = EDGE_CURVE ( 'NONE', #45831, #15748, #58415, .T. ) ;
#43237 = CARTESIAN_POINT ( 'NONE',  ( 4.967162193818130511, -42.34252806656598977, 7.970725651239652265 ) ) ;
#43238 = B_SPLINE_CURVE_WITH_KNOTS ( 'NONE', 3,
 ( #30022, #30327, #25633, #15944, #11236, #49437 ),
 .UNSPECIFIED., .F., .F.,
 ( 4, 2, 4 ),
 ( 0.004120275011746843581, 0.005288420935197119671, 0.006456566858647394894 ),
 .UNSPECIFIED. ) ;
#43239 = EDGE_CURVE ( 'NONE', #33938, #3092, #31200, .T. ) ;
#43240 = CARTESIAN_POINT ( 'NONE',  ( 1.231276596079881935, -41.76121777166937221, -3.643825084341031584 ) ) ;
#43241 = B_SPLINE_CURVE_WITH_KNOTS ( 'NONE', 3,
 ( #3552, #28001, #22686, #37737, #60882, #8893 ),
 .UNSPECIFIED., .F., .F.,
 ( 4, 2, 4 ),
 ( 2.335442953235084577E-18, 0.0002447193893791693828, 0.0004894387787583364888 ),
 .UNSPECIFIED. ) ;
#43242 = CARTESIAN_POINT ( 'NONE',  ( 0.9780106845699472196, -34.72773020588816451, 23.45881499996284347 ) ) ;
#43243 = CARTESIAN_POINT ( 'NONE',  ( 0.8554163680231708922, 17.71207986799998579, -43.44522643353822389 ) ) ;
#43244 = ADVANCED_FACE ( 'NONE', ( #39988 ), #10084, .F. ) ;
#43245 = VERTEX_POINT ( 'NONE', #25232 ) ;
#43246 = CARTESIAN_POINT ( 'NONE',  ( 0.3676999524040366896, 39.37931578713023839, -19.88014264185028068 ) ) ;
#43247 = CARTESIAN_POINT ( 'NONE',  ( -4.554074483026735898, -10.53772250678246358, 5.913403440073379425E-14 ) ) ;
#43248 = CARTESIAN_POINT ( 'NONE',  ( 0.5827357941260208340, 17.99287562175647892, -44.38787053017132678 ) ) ;
#43249 = CARTESIAN_POINT ( 'NONE',  ( 5.901463166500145796, 12.97422524546404965, 15.36838799681346046 ) ) ;
#43250 = CARTESIAN_POINT ( 'NONE',  ( 0.1365634738349418564, 4.870270422476211891, -43.85365532809326083 ) ) ;
#43251 = ORIENTED_EDGE ( 'NONE', *, *, #24352, .T. ) ;
#43252 = CARTESIAN_POINT ( 'NONE',  ( 0.9758171775293903449, -37.15687890897636692, 21.45936886481784001 ) ) ;
#43253 = CARTESIAN_POINT ( 'NONE',  ( 3.376099380956838925, 11.29282810595541164, 7.223601387217505554 ) ) ;
#43254 = B_SPLINE_CURVE_WITH_KNOTS ( 'NONE', 3,
 ( #32198, #51905, #8675, #27484 ),
 .UNSPECIFIED., .F., .F.,
 ( 4, 4 ),
 ( 2.602085213965210642E-18, 0.004042984057420976295 ),
 .UNSPECIFIED. ) ;
#43255 = VECTOR ( 'NONE', #32215, 1000.000000000000114 ) ;
#43256 = CARTESIAN_POINT ( 'NONE',  ( 3.680882792899938138, 32.59085259319688532, -35.20667105325183144 ) ) ;
#43257 = VECTOR ( 'NONE', #54765, 1000.000000000000227 ) ;
#43258 = ORIENTED_EDGE ( 'NONE', *, *, #13655, .T. ) ;
#43259 = CARTESIAN_POINT ( 'NONE',  ( 0.7764146366350199724, -35.37865071303732378, -30.79596641435480109 ) ) ;
#43260 = B_SPLINE_CURVE_WITH_KNOTS ( 'NONE', 3,
 ( #22965, #23565, #38012, #33297 ),
 .UNSPECIFIED., .F., .F.,
 ( 4, 4 ),
 ( 0.000000000000000000, 0.004445488388166995118 ),
 .UNSPECIFIED. ) ;
#43261 = CARTESIAN_POINT ( 'NONE',  ( 1.157644175074338699, 25.52398871922472878, -33.24948533947659968 ) ) ;
#43262 = ORIENTED_EDGE ( 'NONE', *, *, #48446, .T. ) ;
#43263 = B_SPLINE_CURVE_WITH_KNOTS ( 'NONE', 3,
 ( #39302, #58357, #6037, #19884, #1053, #44617, #20189, #58057, #25175, #20795, #39612, #53059, #44317, #33670, #30175, #14877 ),
 .UNSPECIFIED., .F., .F.,
 ( 4, 3, 3, 3, 3, 4 ),
 ( 6.938893903907228378E-18, 0.0002724568934985532160, 0.0004086836638483783580, 0.0005449104342063567545, 0.0008173270854453719859, 0.001089761613562697899 ),
 .UNSPECIFIED. ) ;
#43264 = CARTESIAN_POINT ( 'NONE',  ( 0.9730545539215883499, -6.101350888304360787, -42.47233286818623554 ) ) ;
#43265 = ORIENTED_EDGE ( 'NONE', *, *, #28155, .F. ) ;
#43266 = CARTESIAN_POINT ( 'NONE',  ( 4.958415959904816539, 45.35203410338237973, 2.529220533737273069 ) ) ;
#43267 = ORIENTED_EDGE ( 'NONE', *, *, #46899, .F. ) ;
#43268 = CARTESIAN_POINT ( 'NONE',  ( 3.407937589446178528, 2.242416846335596237, 13.51415833181188830 ) ) ;
#43269 = CARTESIAN_POINT ( 'NONE',  ( -6.078457390727109555, 19.09849343800969734, -2.458060096053082511 ) ) ;
#43270 = ORIENTED_EDGE ( 'NONE', *, *, #7987, .F. ) ;
#43271 = CARTESIAN_POINT ( 'NONE',  ( 2.526464513654342880, -39.22765990515334522, 17.56107808841295181 ) ) ;
#43272 = EDGE_CURVE ( 'NONE', #42943, #5776, #39669, .T. ) ;
#43273 = VERTEX_POINT ( 'NONE', #58113 ) ;
#43274 = CARTESIAN_POINT ( 'NONE',  ( 1.227938101723748288, 26.79402671879374864, -33.52879263017835143 ) ) ;
#43275 = EDGE_CURVE ( 'NONE', #45586, #199, #41647, .T. ) ;
#43276 = CARTESIAN_POINT ( 'NONE',  ( 2.526464513654344657, 42.96196573359004134, -1.212545078562930589 ) ) ;
#43277 = ORIENTED_EDGE ( 'NONE', *, *, #25902, .F. ) ;
#43278 = CARTESIAN_POINT ( 'NONE',  ( 0.5804410086790514622, 46.40460073163220756, 6.792119168064950863 ) ) ;
#43279 = CARTESIAN_POINT ( 'NONE',  ( 0.6254311100348666219, 5.596225872411388913, 47.77988293940236275 ) ) ;
#43280 = CARTESIAN_POINT ( 'NONE',  ( 0.1139756605157203201, -23.21278114026133466, -37.52495185112634601 ) ) ;
#43281 = VERTEX_POINT ( 'NONE', #38747 ) ;
#43282 = DIRECTION ( 'NONE',  ( 0.000000000000000000, 0.000000000000000000, 1.000000000000000000 ) ) ;
#43283 = CARTESIAN_POINT ( 'NONE',  ( 0.1155031312995260795, -18.01467581873768609, 40.27918926291336987 ) ) ;
#43284 = ORIENTED_EDGE ( 'NONE', *, *, #16481, .T. ) ;
#43285 = CARTESIAN_POINT ( 'NONE',  ( 5.959547316686252039, 7.851524054666414010, -18.96456592444092593 ) ) ;
#43286 = VERTEX_POINT ( 'NONE', #48731 ) ;
#43287 = CARTESIAN_POINT ( 'NONE',  ( 0.8554163680231816613, -29.58718577084439261, 36.41159034254562243 ) ) ;
#43288 = CARTESIAN_POINT ( 'NONE',  ( 0.8551540677456715978, 0.9122407826475813497, 47.90804413217340851 ) ) ;
#43289 = VERTEX_POINT ( 'NONE', #44377 ) ;
#43290 = CARTESIAN_POINT ( 'NONE',  ( 4.549368137175248350, 0.000000000000000000, 0.000000000000000000 ) ) ;
#43291 = CARTESIAN_POINT ( 'NONE',  ( -6.078726893082806448, -19.21666810860935470, 1.230328440814298041 ) ) ;
#43292 = CARTESIAN_POINT ( 'NONE',  ( 0.1119898979215348395, -0.8531639444010161721, 44.11613559159281550 ) ) ;
#43293 = CARTESIAN_POINT ( 'NONE',  ( 0.9780303403264757334, -22.82262494000252673, -35.14921626783534947 ) ) ;
#43294 = ORIENTED_EDGE ( 'NONE', *, *, #49696, .F. ) ;
#43295 = CARTESIAN_POINT ( 'NONE',  ( 0.6028618097248863439, 18.24855319618746563, -44.51207924874658772 ) ) ;
#43296 = CARTESIAN_POINT ( 'NONE',  ( 0.8551540677456739292, 24.74404575822832797, -41.03346287276401938 ) ) ;
#43297 = B_SPLINE_CURVE_WITH_KNOTS ( 'NONE', 3,
 ( #60074, #45693, #49751, #2742 ),
 .UNSPECIFIED., .F., .F.,
 ( 4, 4 ),
 ( 7.152448122690996019E-18, 0.005004948556313815709 ),
 .UNSPECIFIED. ) ;
#43298 = CIRCLE ( 'NONE', #23292, 42.08604991992415023 ) ;
#43299 = EDGE_CURVE ( 'NONE', #18471, #46940, #52047, .T. ) ;
#43300 = CARTESIAN_POINT ( 'NONE',  ( 4.909518593371827500, 0.8656805903013302661, 3.058095148607754396E-16 ) ) ;
#43301 = CARTESIAN_POINT ( 'NONE',  ( -6.078726893082806448, 15.42998809551227879, 11.51996131248145439 ) ) ;
#43302 =( BOUNDED_SURFACE ( )  B_SPLINE_SURFACE ( 3, 1, ( 
 ( #31265, #50364 ),
 ( #7432, #26563 ),
 ( #46305, #4578 ),
 ( #18717, #52205 ) ),
 .UNSPECIFIED., .F., .F., .F. ) 
 B_SPLINE_SURFACE_WITH_KNOTS ( ( 4, 4 ),
 ( 2, 2 ),
 ( 0.000000000000000000, 1.000000000000000000 ),
 ( 0.000000000000000000, 1.000000000000000000 ),
 .UNSPECIFIED. ) 
 GEOMETRIC_REPRESENTATION_ITEM ( )  RATIONAL_B_SPLINE_SURFACE ( (
 ( 1.000000000000000000, 1.000000000000000000),
 ( 0.9751682680413298332, 0.9999560080971552356),
 ( 0.9751682680413298332, 0.9999560080971552356),
 ( 1.000000000000000000, 1.000000000000000000) ) ) 
 REPRESENTATION_ITEM ( '' )  SURFACE ( )  );
#43303 = CIRCLE ( 'NONE', #46293, 4.000000000000000000 ) ;
#43304 = CARTESIAN_POINT ( 'NONE',  ( -5.995132425357893702, 14.94489030678151487, 11.47834865841101148 ) ) ;
#43305 = EDGE_CURVE ( 'NONE', #37493, #10852, #14684, .T. ) ;
#43306 = FACE_OUTER_BOUND ( 'NONE', #46736, .T. ) ;
#43307 = EDGE_CURVE ( 'NONE', #51963, #37474, #45592, .T. ) ;
#43308 = ADVANCED_FACE ( 'NONE', ( #27089 ), #1275, .F. ) ;
#43309 = CARTESIAN_POINT ( 'NONE',  ( -17.97369999999976642, -7.719455939378112141, -2.099999999999997424 ) ) ;
#43310 = CARTESIAN_POINT ( 'NONE',  ( 0.2885697896453101041, -22.25146201964169990, 36.93108635218660396 ) ) ;
#43311 = CARTESIAN_POINT ( 'NONE',  ( 0.6009452777970413218, 48.10564074251961841, -0.4363873594207403617 ) ) ;
#43312 = B_SPLINE_CURVE_WITH_KNOTS ( 'NONE', 3,
 ( #54501, #12256, #26332, #58907 ),
 .UNSPECIFIED., .F., .F.,
 ( 4, 4 ),
 ( 3.878959614448863476E-18, 0.004042984057420974560 ),
 .UNSPECIFIED. ) ;
#43313 = CARTESIAN_POINT ( 'NONE',  ( 0.5797568665920711517, 33.05098768062517678, 33.26946831461290088 ) ) ;
#43314 = CARTESIAN_POINT ( 'NONE',  ( 4.975610109902397937, 0.000000000000000000, 0.000000000000000000 ) ) ;
#43315 = CARTESIAN_POINT ( 'NONE',  ( 0.6846871229502932144, -28.47437962186101856, -38.52803883689329467 ) ) ;
#43316 = CARTESIAN_POINT ( 'NONE',  ( 0.9790850452238870627, 9.764526516524007604, 40.75526165013907587 ) ) ;
#43317 = VECTOR ( 'NONE', #19431, 1000.000000000000114 ) ;
#43318 = CARTESIAN_POINT ( 'NONE',  ( 0.5837157313716030416, 45.25373608634124878, -12.30188740843450468 ) ) ;
#43319 = CARTESIAN_POINT ( 'NONE',  ( 0.9972139404380270244, 34.43899251299770015, 25.59643345733242370 ) ) ;
#43320 = ORIENTED_EDGE ( 'NONE', *, *, #36019, .F. ) ;
#43321 = EDGE_CURVE ( 'NONE', #34160, #42435, #49062, .T. ) ;
#43322 = CARTESIAN_POINT ( 'NONE',  ( 4.956445790444002242, -40.23882117934093827, 24.46171131046763136 ) ) ;
#43323 = CARTESIAN_POINT ( 'NONE',  ( 4.060580049360325461, 18.24836065817153496, -39.98080824156142654 ) ) ;
#43324 = ORIENTED_EDGE ( 'NONE', *, *, #12925, .F. ) ;
#43325 = ADVANCED_FACE ( 'NONE', ( #7975 ), #58913, .F. ) ;
#43326 = CARTESIAN_POINT ( 'NONE',  ( 3.238018933889920792, -0.1726436309642142564, 13.39319553147569231 ) ) ;
#43327 = CARTESIAN_POINT ( 'NONE',  ( 1.112077966505211846, 26.07276307627627432, 35.54210672845545815 ) ) ;
#43328 = B_SPLINE_CURVE_WITH_KNOTS ( 'NONE', 3,
 ( #32793, #52486, #8333, #46581, #56570, #41893 ),
 .UNSPECIFIED., .F., .F.,
 ( 4, 2, 4 ),
 ( 3.476216610979977084E-18, 0.0002291459268755738398, 0.0004582918537511442101 ),
 .UNSPECIFIED. ) ;
#43329 = B_SPLINE_CURVE_WITH_KNOTS ( 'NONE', 3,
 ( #28992, #9259, #57460, #14293 ),
 .UNSPECIFIED., .F., .F.,
 ( 4, 4 ),
 ( 0.000000000000000000, 0.005004948556313808770 ),
 .UNSPECIFIED. ) ;
#43330 = ORIENTED_EDGE ( 'NONE', *, *, #12647, .F. ) ;
#43331 = ORIENTED_EDGE ( 'NONE', *, *, #44762, .T. ) ;
#43332 = FACE_OUTER_BOUND ( 'NONE', #32135, .T. ) ;
#43333 = VERTEX_POINT ( 'NONE', #60579 ) ;
#43334 = CARTESIAN_POINT ( 'NONE',  ( 5.959828726073459926, -12.49879082830556953, -16.28130559351260587 ) ) ;
#43335 = ORIENTED_EDGE ( 'NONE', *, *, #19809, .T. ) ;
#43336 = ORIENTED_EDGE ( 'NONE', *, *, #57655, .F. ) ;
#43337 = DIRECTION ( 'NONE',  ( 0.07500201931887538753, -0.7741482765856521064, -0.6285452592753808521 ) ) ;
#43338 = ORIENTED_EDGE ( 'NONE', *, *, #17192, .T. ) ;
#43339 = CARTESIAN_POINT ( 'NONE',  ( -6.016761891674565099, -13.32172022638582121, -13.32657647165369141 ) ) ;
#43340 = CARTESIAN_POINT ( 'NONE',  ( 3.238931869106854045, -32.96367555688129869, 27.59912060131716416 ) ) ;
#43341 = MECHANICAL_DESIGN_GEOMETRIC_PRESENTATION_REPRESENTATION (  '', ( #25292 ), #46333 ) ;
#43342 = CARTESIAN_POINT ( 'NONE',  ( 0.1119898979215352836, 9.270610865333816619, -43.13950721131830335 ) ) ;
#43343 = VERTEX_POINT ( 'NONE', #12387 ) ;
#43344 = CARTESIAN_POINT ( 'NONE',  ( 0.5809828226811553087, -12.92184523170170607, -46.11980934799353093 ) ) ;
#43345 = EDGE_CURVE ( 'NONE', #9401, #34772, #17694, .T. ) ;
#43346 = ORIENTED_EDGE ( 'NONE', *, *, #35934, .T. ) ;
#43347 = ORIENTED_EDGE ( 'NONE', *, *, #19402, .T. ) ;
#43348 = CARTESIAN_POINT ( 'NONE',  ( 3.238018933889920792, 10.68005193312860790, -8.083562523623408325 ) ) ;
#43349 = ORIENTED_EDGE ( 'NONE', *, *, #44998, .F. ) ;
#43350 = CARTESIAN_POINT ( 'NONE',  ( 0.7413678028165007206, 34.17436483739517428, 27.86752374594578185 ) ) ;
#43351 = LINE ( 'NONE', #38650, #58228 ) ;
#43352 = DIRECTION ( 'NONE',  ( 1.000000000000000000, 0.000000000000000000, 0.000000000000000000 ) ) ;
#43353 = B_SPLINE_CURVE_WITH_KNOTS ( 'NONE', 3,
 ( #55947, #51549, #33405, #13065 ),
 .UNSPECIFIED., .F., .F.,
 ( 4, 4 ),
 ( 0.000000000000000000, 0.005004741218457401525 ),
 .UNSPECIFIED. ) ;
#43354 = AXIS2_PLACEMENT_3D ( 'NONE', #21721, #22039, #25801 ) ;
#43355 = ORIENTED_EDGE ( 'NONE', *, *, #7617, .T. ) ;
#43356 = CARTESIAN_POINT ( 'NONE',  ( 0.6030672727741701600, -12.53539249098747099, 46.44558360016990406 ) ) ;
#43357 = DIRECTION ( 'NONE',  ( 0.000000000000000000, 0.000000000000000000, 1.000000000000000000 ) ) ;
#43358 = CARTESIAN_POINT ( 'NONE',  ( 0.7056313189692733356, -30.91979901656658214, -35.26633908889165525 ) ) ;
#43359 = CARTESIAN_POINT ( 'NONE',  ( 0.6001305935487422083, 6.798494447612207559, -47.62765676940936999 ) ) ;
#43360 = VERTEX_POINT ( 'NONE', #60270 ) ;
#43361 = FACE_OUTER_BOUND ( 'NONE', #44232, .T. ) ;
#43362 = CARTESIAN_POINT ( 'NONE',  ( 0.1152339509894530906, 36.85759422494557214, -24.25820352797176938 ) ) ;
#43363 = CARTESIAN_POINT ( 'NONE',  ( -6.077587904424778920, 9.987489566522819828, -16.46347695818013435 ) ) ;
#43364 = CARTESIAN_POINT ( 'NONE',  ( 2.009741617377216460, -5.672209269575592572, 43.67299073369244411 ) ) ;
#43365 = ORIENTED_EDGE ( 'NONE', *, *, #8917, .T. ) ;
#43366 = VERTEX_POINT ( 'NONE', #11770 ) ;
#43367 = CARTESIAN_POINT ( 'NONE',  ( 50.50000000000024869, 1.836970198721029747E-14, -7.703719777548943412E-31 ) ) ;
#43368 = CARTESIAN_POINT ( 'NONE',  ( 0.1129192098497455998, 37.24220309526837980, -23.66368729500826618 ) ) ;
#43369 = CARTESIAN_POINT ( 'NONE',  ( 5.895881250540457863, -9.669871309366996570, -17.63579514704630213 ) ) ;
#43370 = CARTESIAN_POINT ( 'NONE',  ( 3.240649175237395596, 42.79365579596336744, 10.19646708493989706 ) ) ;
#43371 = DIRECTION ( 'NONE',  ( 1.000000000000000000, 0.000000000000000000, 0.000000000000000000 ) ) ;
#43372 = FACE_OUTER_BOUND ( 'NONE', #37836, .T. ) ;
#43373 = CARTESIAN_POINT ( 'NONE',  ( 1.088908134280552886, -22.12904883058530459, -36.76788378223852760 ) ) ;
#43374 = CARTESIAN_POINT ( 'NONE',  ( 4.975610109902397937, -47.89734868211986907, 9.914302615978730415 ) ) ;
#43375 = CARTESIAN_POINT ( 'NONE',  ( 1.227938101723748288, 37.58536632582807613, -20.72293514920711033 ) ) ;
#43376 = CARTESIAN_POINT ( 'NONE',  ( 0.5804410086790514622, -30.69452151258693462, -35.45935984995688983 ) ) ;
#43377 = B_SPLINE_CURVE_WITH_KNOTS ( 'NONE', 3,
 ( #31418, #54576, #50516, #46156, #59290, #30788 ),
 .UNSPECIFIED., .F., .F.,
 ( 4, 2, 4 ),
 ( 0.000000000000000000, 0.0002447195606305742582, 0.0004894391212611485164 ),
 .UNSPECIFIED. ) ;
#43378 = EDGE_CURVE ( 'NONE', #2222, #6486, #25868, .T. ) ;
#43379 = CARTESIAN_POINT ( 'NONE',  ( 0.6017667736363750963, -18.08696174077359586, -44.57803721604144442 ) ) ;
#43380 =( BOUNDED_SURFACE ( )  B_SPLINE_SURFACE ( 3, 1, ( 
 ( #1383, #16433 ),
 ( #2314, #49023 ),
 ( #35561, #58702 ),
 ( #15827, #21441 ) ),
 .UNSPECIFIED., .F., .F., .F. ) 
 B_SPLINE_SURFACE_WITH_KNOTS ( ( 4, 4 ),
 ( 2, 2 ),
 ( 0.000000000000000000, 1.000000000000000000 ),
 ( 0.000000000000000000, 1.000000000000000000 ),
 .UNSPECIFIED. ) 
 GEOMETRIC_REPRESENTATION_ITEM ( )  RATIONAL_B_SPLINE_SURFACE ( (
 ( 1.000000000000000000, 1.000000000000000000),
 ( 0.7223157951917476005, 0.9931996967497186413),
 ( 0.7223157951917476005, 0.9931996967497186413),
 ( 1.000000000000000000, 1.000000000000000000) ) ) 
 REPRESENTATION_ITEM ( '' )  SURFACE ( )  );
#43381 = CARTESIAN_POINT ( 'NONE',  ( 4.962356264823608143, 0.000000000000000000, 0.000000000000000000 ) ) ;
#43382 = EDGE_LOOP ( 'NONE', ( #53697, #10033, #1307, #7292 ) ) ;
#43383 = ADVANCED_FACE ( 'NONE', ( #51189 ), #2024, .F. ) ;
#43384 = CYLINDRICAL_SURFACE ( 'NONE', #6863, 2.649999999999992806 ) ;
#43385 = CARTESIAN_POINT ( 'NONE',  ( 0.1095718737110178143, -34.05592812063363795, -26.45591486700744355 ) ) ;
#43386 = CARTESIAN_POINT ( 'NONE',  ( 0.1129192098497447394, -35.06977877439262414, 26.77802092202325213 ) ) ;
#43387 = CARTESIAN_POINT ( 'NONE',  ( -6.016761891674564211, -0.003433883959652091721, -18.84319130225482297 ) ) ;
#43388 = CARTESIAN_POINT ( 'NONE',  ( 3.680882792899937694, -46.78529781139681631, -10.62117075007632039 ) ) ;
#43389 = VECTOR ( 'NONE', #41083, 999.9999999999998863 ) ;
#43390 = CARTESIAN_POINT ( 'NONE',  ( 0.6029303876144825880, -46.50193792184033015, 12.32464004947798664 ) ) ;
#43391 = CARTESIAN_POINT ( 'NONE',  ( 0.5998501479064699549, 23.59887241503354716, -41.92175333043595487 ) ) ;
#43392 = CARTESIAN_POINT ( 'NONE',  ( 0.9756008150404611445, -26.00810955565536275, 34.12792951168094646 ) ) ;
#43393 = FACE_OUTER_BOUND ( 'NONE', #23150, .T. ) ;
#43394 = CARTESIAN_POINT ( 'NONE',  ( 0.9756950546413932779, -11.01205619898749077, 41.47131842451901917 ) ) ;
#43395 = CARTESIAN_POINT ( 'NONE',  ( 4.962356264823608143, -40.70360067759239087, 10.69824704058788711 ) ) ;
#43396 = CARTESIAN_POINT ( 'NONE',  ( 0.6001305935487422083, -12.95698906763778879, -46.33281397023058901 ) ) ;
#43397 =( BOUNDED_SURFACE ( )  B_SPLINE_SURFACE ( 3, 1, ( 
 ( #10861, #33749 ),
 ( #52831, #30556 ),
 ( #20866, #27105 ),
 ( #40310, #31814 ) ),
 .UNSPECIFIED., .F., .F., .F. ) 
 B_SPLINE_SURFACE_WITH_KNOTS ( ( 4, 4 ),
 ( 2, 2 ),
 ( 0.000000000000000000, 1.000000000000000000 ),
 ( 0.000000000000000000, 1.000000000000000000 ),
 .UNSPECIFIED. ) 
 GEOMETRIC_REPRESENTATION_ITEM ( )  RATIONAL_B_SPLINE_SURFACE ( (
 ( 1.000000000000000000, 1.000000000000000000),
 ( 0.7211978278499970862, 0.9934217856018976445),
 ( 0.7211978278499970862, 0.9934217856018976445),
 ( 1.000000000000000000, 1.000000000000000000) ) ) 
 REPRESENTATION_ITEM ( '' )  SURFACE ( )  );
#43399 = ORIENTED_EDGE ( 'NONE', *, *, #49877, .T. ) ;
#43398 = DIRECTION ( 'NONE',  ( 0.000000000000000000, 1.000000000000000000, 0.000000000000000000 ) ) ;
#43400 = ORIENTED_EDGE ( 'NONE', *, *, #31188, .T. ) ;
#43401 = ADVANCED_FACE ( 'NONE', ( #45293, #22083 ), #2335, .T. ) ;
#43402 = CARTESIAN_POINT ( 'NONE',  ( 5.910764540655178756, 19.70610972188039511, -4.021253299454559560 ) ) ;
#43403 = CARTESIAN_POINT ( 'NONE',  ( 0.1103878639767399000, 39.86034920885563082, 16.45816205842777791 ) ) ;
#43404 = CARTESIAN_POINT ( 'NONE',  ( 1.199999999999992628, 0.000000000000000000, 0.000000000000000000 ) ) ;
#43405 = EDGE_CURVE ( 'NONE', #60737, #26144, #31888, .T. ) ;
#43406 = ORIENTED_EDGE ( 'NONE', *, *, #59757, .F. ) ;
#43407 = CARTESIAN_POINT ( 'NONE',  ( 4.962356264823608143, 12.88441948660223169, -40.06528837230067097 ) ) ;
#43408 = CARTESIAN_POINT ( 'NONE',  ( 0.2224561200757608492, -29.94832483818017366, -31.02237548791941890 ) ) ;
#43409 = CARTESIAN_POINT ( 'NONE',  ( 4.303969348037246512, -16.39840148505059503, -45.22910199346991789 ) ) ;
#43410 = ORIENTED_EDGE ( 'NONE', *, *, #30971, .F. ) ;
#43411 = EDGE_LOOP ( 'NONE', ( #50477, #3688, #5912, #22679 ) ) ;
#43412 = CARTESIAN_POINT ( 'NONE',  ( 4.694002226626920127, 44.18338616738611080, 11.23001149731239678 ) ) ;
#43413 = CARTESIAN_POINT ( 'NONE',  ( 0.3622758884714600280, 17.25816669464994746, -39.50828911766980411 ) ) ;
#43414 = DIRECTION ( 'NONE',  ( -1.000000000000000000, -0.000000000000000000, -0.000000000000000000 ) ) ;
#43415 = CARTESIAN_POINT ( 'NONE',  ( 0.5837800005270551429, 16.85475894598384627, -43.76245376478063065 ) ) ;
#43416 = CARTESIAN_POINT ( 'NONE',  ( 0.1129192098497455998, 19.97823103613628248, 39.34236993944205807 ) ) ;
#43417 = B_SPLINE_CURVE_WITH_KNOTS ( 'NONE', 3,
 ( #13630, #9219, #32735, #31807 ),
 .UNSPECIFIED., .F., .F.,
 ( 4, 4 ),
 ( 7.112366251504909087E-17, 0.005004741218457488261 ),
 .UNSPECIFIED. ) ;
#43418 = CARTESIAN_POINT ( 'NONE',  ( 4.956445790443991584, 35.28522167764473494, 31.18479086508529363 ) ) ;
#43419 = EDGE_CURVE ( 'NONE', #473, #10036, #29639, .T. ) ;
#43420 = CARTESIAN_POINT ( 'NONE',  ( 0.5836750258453351492, 38.10871351907229609, -29.01293504009503366 ) ) ;
#43421 = ORIENTED_EDGE ( 'NONE', *, *, #57125, .F. ) ;
#43422 = EDGE_LOOP ( 'NONE', ( #2601, #40190, #28383, #38666 ) ) ;
#43423 = CARTESIAN_POINT ( 'NONE',  ( 4.956445790444027999, 20.31112743693101663, -42.48524629068760561 ) ) ;
#43424 = CARTESIAN_POINT ( 'NONE',  ( 2.879087469061463178, 43.98767675069456118, 1.089022892222180072 ) ) ;
#43425 = B_SPLINE_CURVE_WITH_KNOTS ( 'NONE', 3,
 ( #42774, #61828, #47770, #32210 ),
 .UNSPECIFIED., .F., .F.,
 ( 4, 4 ),
 ( 4.443059973708341306E-17, 0.005004948556313842598 ),
 .UNSPECIFIED. ) ;
#43426 = ORIENTED_EDGE ( 'NONE', *, *, #3872, .T. ) ;
#43427 = CARTESIAN_POINT ( 'NONE',  ( 0.1157991065609915715, 41.90187902746315984, -13.82660115522040378 ) ) ;
#43428 = CARTESIAN_POINT ( 'NONE',  ( 0.2885700199627500018, 37.73587457854637250, 20.85752789928075046 ) ) ;
#43429 = CARTESIAN_POINT ( 'NONE',  ( 0.6029303876144825880, 46.43417959025973829, 12.57751758557285982 ) ) ;
#43430 = LINE ( 'NONE', #19931, #11362 ) ;
#43431 = VECTOR ( 'NONE', #1123, 1000.000000000000000 ) ;
#43432 = EDGE_LOOP ( 'NONE', ( #21750, #20906, #2916, #60691 ) ) ;
#43433 = EDGE_LOOP ( 'NONE', ( #32856, #33171, #54538, #29817 ) ) ;
#43434 = CARTESIAN_POINT ( 'NONE',  ( 2.624215991343608501, -45.98641578154020948, -13.78323291683831364 ) ) ;
#43435 = CARTESIAN_POINT ( 'NONE',  ( 0.9736507210033059634, -42.48017254354720507, -6.046964561328380228 ) ) ;
#43436 = LINE ( 'NONE', #44067, #38209 ) ;
#43437 = CARTESIAN_POINT ( 'NONE',  ( 5.896278296736517710, -11.92612757635576237, 16.19550742171637836 ) ) ;
#43438 = ORIENTED_EDGE ( 'NONE', *, *, #58669, .T. ) ;
#43439 = CARTESIAN_POINT ( 'NONE',  ( 0.6008123274975391004, 5.148685779782010030, -48.83692850599358337 ) ) ;
#43440 = ORIENTED_EDGE ( 'NONE', *, *, #15650, .F. ) ;
#43441 = CARTESIAN_POINT ( 'NONE',  ( 21.00000000000000355, 2.789133085058097101E-16, -2.055000000000000160 ) ) ;
#43442 = CARTESIAN_POINT ( 'NONE',  ( 0.6001305935487315502, -41.92422178329153581, -23.60027211631814481 ) ) ;
#43443 = ORIENTED_EDGE ( 'NONE', *, *, #15635, .F. ) ;
#43444 = CARTESIAN_POINT ( 'NONE',  ( 0.5827359174754831450, -47.43746338751527247, -6.611633125157290181 ) ) ;
#43445 = DIRECTION ( 'NONE',  ( 0.000000000000000000, 0.000000000000000000, 1.000000000000000000 ) ) ;
#43446 = CARTESIAN_POINT ( 'NONE',  ( 5.895596859100789899, 14.91916793517901496, 13.48875870250535058 ) ) ;
#43447 = VECTOR ( 'NONE', #28696, 1000.000000000000114 ) ;
#43448 = ORIENTED_EDGE ( 'NONE', *, *, #50949, .F. ) ;
#43449 = DIRECTION ( 'NONE',  ( 1.000000000000000000, 1.836909530733573776E-16, 0.000000000000000000 ) ) ;
#43450 = CARTESIAN_POINT ( 'NONE',  ( 3.661921753702001237, -18.07631870279536557, 43.42669485453627232 ) ) ;
#43451 = CARTESIAN_POINT ( 'NONE',  ( 1.227938101723756947, 34.55893248994507161, 25.45152231597068848 ) ) ;
#43452 = DIRECTION ( 'NONE',  ( 0.000000000000000000, 0.000000000000000000, 1.000000000000000000 ) ) ;
#43453 = ORIENTED_EDGE ( 'NONE', *, *, #46774, .T. ) ;
#43455 = EDGE_CURVE ( 'NONE', #58751, #59261, #33902, .T. ) ;
#43454 = CARTESIAN_POINT ( 'NONE',  ( 0.5832366564991509073, -23.71163571971552386, 41.61464700196766842 ) ) ;
#43456 = DIRECTION ( 'NONE',  ( 0.07439287786467664587, 0.9665813013808195464, -0.2453289374370102860 ) ) ;
#43457 = CARTESIAN_POINT ( 'NONE',  ( 0.5806925824938499181, 4.150136846022649095, 46.71186922510005957 ) ) ;
#43458 = ORIENTED_EDGE ( 'NONE', *, *, #30706, .T. ) ;
#43459 = EDGE_CURVE ( 'NONE', #39250, #8721, #55038, .T. ) ;
#43460 = CARTESIAN_POINT ( 'NONE',  ( 0.5809828226811553087, 38.32755012159145025, 28.72298383114502229 ) ) ;
#43461 = CARTESIAN_POINT ( 'NONE',  ( 4.553261556744875094, 0.000000000000000000, 0.000000000000000000 ) ) ;
#43462 = DIRECTION ( 'NONE',  ( 0.000000000000000000, 0.000000000000000000, -1.000000000000000000 ) ) ;
#43463 = DIRECTION ( 'NONE',  ( 0.000000000000000000, 0.000000000000000000, -1.000000000000000000 ) ) ;
#43464 = CARTESIAN_POINT ( 'NONE',  ( 4.691466044806102076, 3.249105306918426805, -44.46979273209132089 ) ) ;
#43465 = CARTESIAN_POINT ( 'NONE',  ( 0.6021448801613057400, -20.11648276748766762, 44.79808321448942365 ) ) ;
#43466 = DIRECTION ( 'NONE',  ( 1.000000000000000000, 0.000000000000000000, 0.000000000000000000 ) ) ;
#43467 = ADVANCED_FACE ( 'NONE', ( #52419 ), #52114, .T. ) ;
#43468 = DIRECTION ( 'NONE',  ( 0.1614216396873988379, -0.8170448096416224049, -0.5535167868080577147 ) ) ;
#43469 = CARTESIAN_POINT ( 'NONE',  ( 0.1064266379913942212, -41.79703901861809356, -10.61815631313347552 ) ) ;
#43470 = CARTESIAN_POINT ( 'NONE',  ( 0.9780303403264770656, -6.651109705658430293, 41.37755856836385249 ) ) ;
#43471 = CARTESIAN_POINT ( 'NONE',  ( 4.967162193818130511, -28.07411493385273715, -32.68434214048198072 ) ) ;
#43473 = ORIENTED_EDGE ( 'NONE', *, *, #33129, .T. ) ;
#43472 = DIRECTION ( 'NONE',  ( 0.000000000000000000, 0.000000000000000000, 1.000000000000000000 ) ) ;
#43474 = VERTEX_POINT ( 'NONE', #41830 ) ;
#43475 = CARTESIAN_POINT ( 'NONE',  ( 0.8753041380234465318, -47.71532843791173661, 11.59248721953970573 ) ) ;
#43476 = DIRECTION ( 'NONE',  ( 1.000000000000000000, 1.836909530733573776E-16, 0.000000000000000000 ) ) ;
#43477 = CARTESIAN_POINT ( 'NONE',  ( 49.16403548792207090, 15.32681626569766209, -2.314452977059477945 ) ) ;
#43478 = ADVANCED_FACE ( 'NONE', ( #28015 ), #7684, .F. ) ;
#43479 = CARTESIAN_POINT ( 'NONE',  ( 0.7764146366350278550, 23.31927532629819666, 40.69707448853623788 ) ) ;
#43480 = CARTESIAN_POINT ( 'NONE',  ( 4.549368137175248350, 24.02461520945271900, -35.57418903283089406 ) ) ;
#43481 = CARTESIAN_POINT ( 'NONE',  ( 0.1158816050234198619, 9.813012560525406158, -43.01914487518472185 ) ) ;
#43482 =( BOUNDED_SURFACE ( )  B_SPLINE_SURFACE ( 3, 1, ( 
 ( #24642, #28403 ),
 ( #4576, #10234 ),
 ( #10541, #29636 ),
 ( #61896, #23716 ) ),
 .UNSPECIFIED., .F., .F., .F. ) 
 B_SPLINE_SURFACE_WITH_KNOTS ( ( 4, 4 ),
 ( 2, 2 ),
 ( 0.000000000000000000, 1.000000000000000000 ),
 ( 0.000000000000000000, 1.000000000000000000 ),
 .UNSPECIFIED. ) 
 GEOMETRIC_REPRESENTATION_ITEM ( )  RATIONAL_B_SPLINE_SURFACE ( (
 ( 1.000000000000000000, 1.000000000000000000),
 ( 0.7223157951917476005, 0.9931996967497186413),
 ( 0.7223157951917476005, 0.9931996967497186413),
 ( 1.000000000000000000, 1.000000000000000000) ) ) 
 REPRESENTATION_ITEM ( '' )  SURFACE ( )  );
#43483 = ORIENTED_EDGE ( 'NONE', *, *, #59237, .F. ) ;
#43484 = CIRCLE ( 'NONE', #13470, 10.00000000000000355 ) ;
#43485 = CARTESIAN_POINT ( 'NONE',  ( 0.8560838555295158248, 44.99141268455571208, 13.27198623905747432 ) ) ;
#43486 = CARTESIAN_POINT ( 'NONE',  ( -18.65472868113690907, -7.748419048184884694, 1.991217322887269825 ) ) ;
#43487 = CARTESIAN_POINT ( 'NONE',  ( 45.00000000000001421, 0.000000000000000000, 75.00000000000001421 ) ) ;
#43488 = ORIENTED_EDGE ( 'NONE', *, *, #49263, .F. ) ;
#43489 = AXIS2_PLACEMENT_3D ( 'NONE', #17828, #2778, #8401 ) ;
#43490 = DIRECTION ( 'NONE',  ( 0.000000000000000000, 0.000000000000000000, 1.000000000000000000 ) ) ;
#43491 = CARTESIAN_POINT ( 'NONE',  ( 4.956653778116966613, 0.000000000000000000, 0.000000000000000000 ) ) ;
#43492 = ORIENTED_EDGE ( 'NONE', *, *, #9034, .F. ) ;
#43493 =( BOUNDED_SURFACE ( )  B_SPLINE_SURFACE ( 3, 1, ( 
 ( #51522, #56537 ),
 ( #33077, #27739 ),
 ( #46869, #3909 ),
 ( #52148, #18980 ) ),
 .UNSPECIFIED., .F., .F., .F. ) 
 B_SPLINE_SURFACE_WITH_KNOTS ( ( 4, 4 ),
 ( 2, 2 ),
 ( 0.000000000000000000, 1.000000000000000000 ),
 ( 0.000000000000000000, 1.000000000000000000 ),
 .UNSPECIFIED. ) 
 GEOMETRIC_REPRESENTATION_ITEM ( )  RATIONAL_B_SPLINE_SURFACE ( (
 ( 1.000000000000000000, 1.000000000000000000),
 ( 0.7282232189291693025, 0.9929344683865674037),
 ( 0.7282232189291693025, 0.9929344683865674037),
 ( 1.000000000000000000, 1.000000000000000000) ) ) 
 REPRESENTATION_ITEM ( '' )  SURFACE ( )  );
#43494 = CARTESIAN_POINT ( 'NONE',  ( 0.7762777257811899201, -44.59086130178263119, 17.50713318242622307 ) ) ;
#43495 = VERTEX_POINT ( 'NONE', #47433 ) ;
#43496 = B_SPLINE_CURVE_WITH_KNOTS ( 'NONE', 3,
 ( #37595, #56662, #9058, #28166 ),
 .UNSPECIFIED., .F., .F.,
 ( 4, 4 ),
 ( 6.397344083151129036E-17, 0.005004741218457495200 ),
 .UNSPECIFIED. ) ;
#43497 = CARTESIAN_POINT ( 'NONE',  ( 0.6254087463353930065, -13.11428234126331205, -46.28445368454747211 ) ) ;
#43498 = CARTESIAN_POINT ( 'NONE',  ( 4.335381028904201628, 2.583895202257807888, 48.91912032373532071 ) ) ;
#43499 = ORIENTED_EDGE ( 'NONE', *, *, #26243, .T. ) ;
#43500 = FACE_BOUND ( 'NONE', #59327, .T. ) ;
#43501 = CARTESIAN_POINT ( 'NONE',  ( 4.553261556744873317, 1.633632119646958980, 43.89613664004264848 ) ) ;
#43502 = LINE ( 'NONE', #52554, #21717 ) ;
#43503 = CARTESIAN_POINT ( 'NONE',  ( 0.5839879882012672940, -37.99840755997069408, 29.15724166963637032 ) ) ;
#43504 = EDGE_CURVE ( 'NONE', #9360, #22050, #38653, .T. ) ;
#43505 = ORIENTED_EDGE ( 'NONE', *, *, #25097, .T. ) ;
#43506 = ADVANCED_FACE ( 'NONE', ( #46836 ), #3289, .F. ) ;
#43507 = CARTESIAN_POINT ( 'NONE',  ( 5.901764892641288895, -27.98073834948296934, 40.18793038783474714 ) ) ;
#43508 = EDGE_LOOP ( 'NONE', ( #30376, #58737, #27229, #19823 ) ) ;
#43509 = DIRECTION ( 'NONE',  ( 1.000000000000000000, 1.558861125776144859E-16, -3.851859888774471706E-32 ) ) ;
#43510 = VECTOR ( 'NONE', #58839, 1000.000000000000000 ) ;
#43511 = ORIENTED_EDGE ( 'NONE', *, *, #15022, .T. ) ;
#43512 = ADVANCED_FACE ( 'NONE', ( #47136 ), #922, .F. ) ;
#43513 = EDGE_LOOP ( 'NONE', ( #59032, #14136 ) ) ;
#43514 = CARTESIAN_POINT ( 'NONE',  ( 5.910764540655178756, 8.451874527002367188, -18.25012480639438195 ) ) ;
#43515 = CARTESIAN_POINT ( 'NONE',  ( 3.678834586032787346, 40.00782562460102554, 28.24865055927222102 ) ) ;
#43516 = DIRECTION ( 'NONE',  ( -0.07906939808003035641, -0.8860534191553621763, 0.4567902896191575191 ) ) ;
#43517 = ORIENTED_EDGE ( 'NONE', *, *, #28670, .F. ) ;
#43518 = CARTESIAN_POINT ( 'NONE',  ( 5.895881250540457863, -4.658141670565172809, -19.56602662231770395 ) ) ;
#43519 = CARTESIAN_POINT ( 'NONE',  ( 1.600000000000000089, -11.64055411052240352, -1.199999999999999956 ) ) ;
#43520 = CARTESIAN_POINT ( 'NONE',  ( 0.1365634738349439103, -28.00541523581697589, 34.09632439270718152 ) ) ;
#43521 = ORIENTED_EDGE ( 'NONE', *, *, #23645, .F. ) ;
#43522 = B_SPLINE_CURVE_WITH_KNOTS ( 'NONE', 3,
 ( #30483, #1660, #48993, #40547, #30797, #16406, #49597, #53662, #59301, #1061, #29881, #49919, #59611, #26108, #16719, #35839 ),
 .UNSPECIFIED., .F., .F.,
 ( 4, 3, 3, 3, 3, 4 ),
 ( 2.194378057379452627E-17, 0.0002612764279487758733, 0.0003919131003184795161, 0.0005225497727000660148, 0.0007837925190632443785, 0.001045051706266715867 ),
 .UNSPECIFIED. ) ;
#43523 = ORIENTED_EDGE ( 'NONE', *, *, #17343, .T. ) ;
#43524 = CARTESIAN_POINT ( 'NONE',  ( 5.000000000000007994, -54.69470952477895054, -58.44237546506863623 ) ) ;
#43525 = DIRECTION ( 'NONE',  ( 1.000000000000000000, 0.000000000000000000, 0.000000000000000000 ) ) ;
#43526 = CARTESIAN_POINT ( 'NONE',  ( -6.078726893082806448, -12.94836301907752585, 14.25250631976375004 ) ) ;
#43527 = FACE_OUTER_BOUND ( 'NONE', #10056, .T. ) ;
#43529 = AXIS2_PLACEMENT_3D ( 'NONE', #7418, #60658, #16538 ) ;
#43528 = DIRECTION ( 'NONE',  ( 0.000000000000000000, 0.000000000000000000, 1.000000000000000000 ) ) ;
#43530 = ORIENTED_EDGE ( 'NONE', *, *, #25506, .F. ) ;
#43531 = EDGE_CURVE ( 'NONE', #46447, #19529, #37891, .T. ) ;
#43532 = VERTEX_POINT ( 'NONE', #8906 ) ;
#43533 = CIRCLE ( 'NONE', #56502, 48.91267123290010943 ) ;
#43534 = DIRECTION ( 'NONE',  ( -1.000000000000000000, 0.000000000000000000, 0.000000000000000000 ) ) ;
#43535 = VECTOR ( 'NONE', #47568, 1000.000000000000000 ) ;
#43536 = CARTESIAN_POINT ( 'NONE',  ( 0.3676999524040323597, -32.25712563511804376, 30.09033780274075198 ) ) ;
#43537 = CARTESIAN_POINT ( 'NONE',  ( 2.359973842542475886, 11.26178937822771253, 42.55946421928896228 ) ) ;
#43538 = ADVANCED_FACE ( 'NONE', ( #28317 ), #8887, .F. ) ;
#43539 = CARTESIAN_POINT ( 'NONE',  ( 3.270143674763207553, 6.605065939546814313, 11.98875605389982013 ) ) ;
#43540 = ORIENTED_EDGE ( 'NONE', *, *, #8152, .F. ) ;
#43541 = FACE_OUTER_BOUND ( 'NONE', #7112, .T. ) ;
#43542 = CARTESIAN_POINT ( 'NONE',  ( -6.057079549204054558, 9.989941839882863661, 16.46305843807571989 ) ) ;
#43543 = FACE_OUTER_BOUND ( 'NONE', #24588, .T. ) ;
#43544 = CARTESIAN_POINT ( 'NONE',  ( 4.963659409799333844, -43.98510776953416013, 8.262218268420326694 ) ) ;
#43545 = CARTESIAN_POINT ( 'NONE',  ( -2.601141883200665639, -8.951945844433334187, -11.94395634066540701 ) ) ;
#43546 = EDGE_CURVE ( 'NONE', #44582, #36033, #23621, .T. ) ;
#43547 = CARTESIAN_POINT ( 'NONE',  ( 0.9789233960466705575, -34.62550353117659085, 23.60955806542803614 ) ) ;
#43548 = CARTESIAN_POINT ( 'NONE',  ( 4.956445790444027111, 8.365049606152357597, -46.34181691762039179 ) ) ;
#43549 = B_SPLINE_CURVE_WITH_KNOTS ( 'NONE', 3,
 ( #48306, #5663, #4737, #34839 ),
 .UNSPECIFIED., .F., .F.,
 ( 4, 4 ),
 ( 2.294131830766625192E-17, 0.004564976165746188579 ),
 .UNSPECIFIED. ) ;
#43550 = AXIS2_PLACEMENT_3D ( 'NONE', #5747, #10487, #39948 ) ;
#43551 = ORIENTED_EDGE ( 'NONE', *, *, #5980, .F. ) ;
#43552 = CARTESIAN_POINT ( 'NONE',  ( 3.782542959838402830, -39.11335357675642399, -15.40725236296878542 ) ) ;
#43553 = CARTESIAN_POINT ( 'NONE',  ( 0.5997462898726536595, 49.03735788587803768, -2.624721264558313560 ) ) ;
#43554 = CARTESIAN_POINT ( 'NONE',  ( -6.016761891674564211, -4.880293656734836283, -18.20023637398604066 ) ) ;
#43555 = CARTESIAN_POINT ( 'NONE',  ( 3.727782113643637096, 40.49037343455033522, 17.12622068749071857 ) ) ;
#43556 = LINE ( 'NONE', #10961, #40780 ) ;
#43557 = ORIENTED_EDGE ( 'NONE', *, *, #57053, .T. ) ;
#43558 = CARTESIAN_POINT ( 'NONE',  ( 4.956445790444027111, 8.365049606152357597, -46.34181691762039179 ) ) ;
#43559 = CARTESIAN_POINT ( 'NONE',  ( 0.5804410086790514622, -44.12183670707880623, 15.89916279082866168 ) ) ;
#43560 = B_SPLINE_CURVE_WITH_KNOTS ( 'NONE', 3,
 ( #9509, #28613, #53034, #4784 ),
 .UNSPECIFIED., .F., .F.,
 ( 4, 4 ),
 ( 0.000000000000000000, 0.005004741218457429280 ),
 .UNSPECIFIED. ) ;
#43561 = B_SPLINE_CURVE_WITH_KNOTS ( 'NONE', 3,
 ( #3664, #36298, #2745, #21877, #46620, #7124, #41928, #55364, #55058, #2436, #50369, #32205, #60678, #12185, #36922, #55671 ),
 .UNSPECIFIED., .F., .F.,
 ( 4, 3, 3, 3, 3, 4 ),
 ( 2.221635811791082109E-17, 0.0002618515315864433320, 0.0003927756766342010270, 0.0005236998216950543121, 0.0007855159896329938019, 0.001047349442285927870 ),
 .UNSPECIFIED. ) ;
#43562 = CARTESIAN_POINT ( 'NONE',  ( 4.335381028904216727, 18.89720170524636700, 45.19571456870197323 ) ) ;
#43563 = ORIENTED_EDGE ( 'NONE', *, *, #51546, .F. ) ;
#43564 = CARTESIAN_POINT ( 'NONE',  ( 0.1073791018717483448, -16.95003405440287381, -39.65380858626208038 ) ) ;
#43565 = VECTOR ( 'NONE', #55624, 1000.000000000000114 ) ;
#43566 = CARTESIAN_POINT ( 'NONE',  ( 4.956653778116987041, -48.02038484091099235, -2.599733001514835884 ) ) ;
#43567 = EDGE_LOOP ( 'NONE', ( #6782, #47201, #48730, #9714 ) ) ;
#43568 = CARTESIAN_POINT ( 'NONE',  ( 0.3676999524040323597, 41.59822836379060362, 14.68121181363330408 ) ) ;
#43569 = AXIS2_PLACEMENT_3D ( 'NONE', #13274, #51769, #38026 ) ;
#43570 = ORIENTED_EDGE ( 'NONE', *, *, #48446, .F. ) ;
#43571 = FACE_BOUND ( 'NONE', #44636, .T. ) ;
#43572 = ORIENTED_EDGE ( 'NONE', *, *, #59624, .F. ) ;
#43573 = CARTESIAN_POINT ( 'NONE',  ( 0.8744876279028263033, 48.92939099258497038, 4.032957658374010101 ) ) ;
#43574 = CARTESIAN_POINT ( 'NONE',  ( 4.553261556744875094, 0.000000000000000000, 0.000000000000000000 ) ) ;
#43575 = EDGE_CURVE ( 'NONE', #58937, #13269, #43936, .T. ) ;
#43576 = VERTEX_POINT ( 'NONE', #58335 ) ;
#43577 = DIRECTION ( 'NONE',  ( 0.000000000000000000, 0.000000000000000000, 1.000000000000000000 ) ) ;
#43578 = VECTOR ( 'NONE', #35980, 1000.000000000000114 ) ;
#43579 = CONICAL_SURFACE ( 'NONE', #8525, 43.08621763946400307, 1.568696531533066763 ) ;
#43580 = ORIENTED_EDGE ( 'NONE', *, *, #47265, .T. ) ;
#43581 = EDGE_CURVE ( 'NONE', #24805, #600, #38668, .T. ) ;
#43582 = LINE ( 'NONE', #43903, #12753 ) ;
#43583 = CARTESIAN_POINT ( 'NONE',  ( 0.6027935024548037868, -38.27223087442867211, 29.14731236071003906 ) ) ;
#43584 = EDGE_CURVE ( 'NONE', #21723, #54066, #20776, .T. ) ;
#43585 = VERTEX_POINT ( 'NONE', #29544 ) ;
#43586 = EDGE_CURVE ( 'NONE', #52714, #7789, #24909, .T. ) ;
#43587 = CARTESIAN_POINT ( 'NONE',  ( 1.112077966505210957, -35.94411555399670988, -25.51569873958945678 ) ) ;
#43588 = B_SPLINE_CURVE_WITH_KNOTS ( 'NONE', 3,
 ( #41731, #50788, #51393, #17918, #8182, #59879, #8481, #46425, #36722, #46734, #7878, #60484, #45817, #56101, #36110, #13213, #45504, #16993, #55480 ),
 .UNSPECIFIED., .F., .F.,
 ( 4, 3, 3, 3, 3, 3, 4 ),
 ( 6.938893903907228378E-18, 0.0002724573126191798754, 0.0004086839781548472846, 0.0005449106435901838715, 0.0006811373090491498316, 0.0008459866663933777228, 0.001010840725717216835 ),
 .UNSPECIFIED. ) ;
#43589 = CARTESIAN_POINT ( 'NONE',  ( 5.965394784446458765, 2.664747781316112896, -20.35165389555755766 ) ) ;
#43590 = DIRECTION ( 'NONE',  ( 0.1024043820194936449, 0.7971196296869256237, 0.5950744814819269868 ) ) ;
#43592 = ORIENTED_EDGE ( 'NONE', *, *, #19048, .F. ) ;
#43591 = EDGE_CURVE ( 'NONE', #9433, #50250, #57235, .T. ) ;
#43593 = CARTESIAN_POINT ( 'NONE',  ( 0.5827357941260206120, -34.12346967353437321, -33.60975216782522068 ) ) ;
#43594 = CARTESIAN_POINT ( 'NONE',  ( 4.956653778116980824, -40.28700667097698584, 26.26162724282358951 ) ) ;
#43595 = VERTEX_POINT ( 'NONE', #24859 ) ;
#43596 = CARTESIAN_POINT ( 'NONE',  ( 4.553261556744875094, 0.000000000000000000, 0.000000000000000000 ) ) ;
#43597 = EDGE_LOOP ( 'NONE', ( #26630, #25674 ) ) ;
#43598 = DIRECTION ( 'NONE',  ( 0.000000000000000000, 0.000000000000000000, 1.000000000000000000 ) ) ;
#43599 = ADVANCED_FACE ( 'NONE', ( #14853 ), #54507, .F. ) ;
#43600 =( BOUNDED_SURFACE ( )  B_SPLINE_SURFACE ( 3, 1, ( 
 ( #8535, #17966 ),
 ( #37086, #18272 ),
 ( #56153, #51442 ),
 ( #27658, #46792 ) ),
 .UNSPECIFIED., .F., .F., .F. ) 
 B_SPLINE_SURFACE_WITH_KNOTS ( ( 4, 4 ),
 ( 2, 2 ),
 ( 0.000000000000000000, 1.000000000000000000 ),
 ( 0.000000000000000000, 1.000000000000000000 ),
 .UNSPECIFIED. ) 
 GEOMETRIC_REPRESENTATION_ITEM ( )  RATIONAL_B_SPLINE_SURFACE ( (
 ( 1.000000000000000000, 1.000000000000000000),
 ( 0.7211978278499970862, 0.9934217856018976445),
 ( 0.7211978278499970862, 0.9934217856018976445),
 ( 1.000000000000000000, 1.000000000000000000) ) ) 
 REPRESENTATION_ITEM ( '' )  SURFACE ( )  );
#43601 = CARTESIAN_POINT ( 'NONE',  ( 0.9787284016396619046, 40.36974178881868625, -11.25255290291651633 ) ) ;
#43602 = ORIENTED_EDGE ( 'NONE', *, *, #15721, .T. ) ;
#43603 = CARTESIAN_POINT ( 'NONE',  ( 3.660176727303405819, -45.06760739764698087, 16.63097650367952340 ) ) ;
#43604 = CARTESIAN_POINT ( 'NONE',  ( 4.962356264823608143, 37.36413190407361640, 19.36897635181929545 ) ) ;
#43605 = CARTESIAN_POINT ( 'NONE',  ( 4.956445790444002242, -43.14021684453514638, 18.88014143872134554 ) ) ;
#43606 = CARTESIAN_POINT ( 'NONE',  ( 0.5988103622719985752, 13.03604477829290786, -46.30780754281420286 ) ) ;
#43607 = EDGE_CURVE ( 'NONE', #6221, #4433, #6416, .T. ) ;
#43608 = ORIENTED_EDGE ( 'NONE', *, *, #34774, .F. ) ;
#43609 = CARTESIAN_POINT ( 'NONE',  ( 0.6031356219577718170, 18.32926896140831019, -44.47888959008680132 ) ) ;
#43610 = CARTESIAN_POINT ( 'NONE',  ( 2.301430502907645614, -46.71331171933241677, 11.18388433759636413 ) ) ;
#43611 = FACE_OUTER_BOUND ( 'NONE', #3765, .T. ) ;
#43612 = DIRECTION ( 'NONE',  ( -0.07500201931887527651, 0.1132404149163036555, 0.9907327114452587624 ) ) ;
#43613 = CARTESIAN_POINT ( 'NONE',  ( -6.079354080745853928, 15.43131048252502069, 11.51814273396867705 ) ) ;
#43614 = VECTOR ( 'NONE', #11059, 1000.000000000000000 ) ;
#43615 = DIRECTION ( 'NONE',  ( 0.000000000000000000, 0.000000000000000000, 1.000000000000000000 ) ) ;
#43616 = CARTESIAN_POINT ( 'NONE',  ( 2.281351352603290916, -25.11567449372737215, 40.87339198768986392 ) ) ;
#43617 = B_SPLINE_CURVE_WITH_KNOTS ( 'NONE', 3,
 ( #31389, #59571, #7244, #26374 ),
 .UNSPECIFIED., .F., .F.,
 ( 4, 4 ),
 ( 0.000000000000000000, 0.004447772540403816324 ),
 .UNSPECIFIED. ) ;
#43618 = CIRCLE ( 'NONE', #4573, 11.40403086437694569 ) ;
#43619 = CARTESIAN_POINT ( 'NONE',  ( 0.5809828226811617480, 38.32755012159184815, -28.72298383114449294 ) ) ;
#43620 = CARTESIAN_POINT ( 'NONE',  ( 2.281448460670577383, 45.98107640562115250, -13.68109378871662329 ) ) ;
#43621 = CARTESIAN_POINT ( 'NONE',  ( 0.9747592971366210168, 30.11108831501880445, -30.56898208368244596 ) ) ;
#43622 = EDGE_CURVE ( 'NONE', #35346, #4544, #48654, .T. ) ;
#43623 = CARTESIAN_POINT ( 'NONE',  ( 1.084202172485504434E-14, 4.618802153517020059, -5.242734410091827613 ) ) ;
#43624 = CARTESIAN_POINT ( 'NONE',  ( 0.1158516988532803244, 39.77583507406630758, 19.10039536222936007 ) ) ;
#43625 = CARTESIAN_POINT ( 'NONE',  ( 0.7048096507298579061, -11.63498350884304244, -46.68221792389235958 ) ) ;
#43626 = EDGE_CURVE ( 'NONE', #36274, #60182, #52920, .T. ) ;
#43627 = CARTESIAN_POINT ( 'NONE',  ( 4.967162193818130511, 0.000000000000000000, 0.000000000000000000 ) ) ;
#43628 = CARTESIAN_POINT ( 'NONE',  ( 0.6039202388192953519, -48.68192096202343322, 6.452463428512738908 ) ) ;
#43629 = CIRCLE ( 'NONE', #18621, 42.08604991992415023 ) ;
#43630 = ORIENTED_EDGE ( 'NONE', *, *, #8388, .F. ) ;
#43631 = CARTESIAN_POINT ( 'NONE',  ( 0.5827357941260228325, 28.86820951701486493, -38.21849163199643584 ) ) ;
#43632 = CARTESIAN_POINT ( 'NONE',  ( 0.9789889208857696090, -1.304255160821619519, 41.88834941266890155 ) ) ;
#43633 = CARTESIAN_POINT ( 'NONE',  ( 1.092182651088184020, 38.27635607255189854, -17.07869287297789285 ) ) ;
#43634 = ORIENTED_EDGE ( 'NONE', *, *, #17656, .F. ) ;
#43635 = PRODUCT_DEFINITION ( 'UNKNOWN', '', #2860, #24815 ) ;
#43636 = CARTESIAN_POINT ( 'NONE',  ( 5.960221823109900008, -20.35070456576736220, 2.673723662180992555 ) ) ;
#43638 = FACE_OUTER_BOUND ( 'NONE', #2628, .T. ) ;
#43637 = B_SPLINE_CURVE_WITH_KNOTS ( 'NONE', 3,
 ( #26825, #46882, #3608, #8019 ),
 .UNSPECIFIED., .F., .F.,
 ( 4, 4 ),
 ( 0.000000000000000000, 0.005014147105413705591 ),
 .UNSPECIFIED. ) ;
#43639 = ORIENTED_EDGE ( 'NONE', *, *, #13225, .F. ) ;
#43640 = ORIENTED_EDGE ( 'NONE', *, *, #34680, .T. ) ;
#43641 = CARTESIAN_POINT ( 'NONE',  ( 0.5786265663353196143, -13.09387673186367707, 46.07681357296480940 ) ) ;
#43642 = ORIENTED_EDGE ( 'NONE', *, *, #42526, .T. ) ;
#43643 = CARTESIAN_POINT ( 'NONE',  ( 0.8551540677456715978, 28.44084013485117879, 38.56334384152441430 ) ) ;
#43644 = ORIENTED_EDGE ( 'NONE', *, *, #42600, .F. ) ;
#43645 = ORIENTED_EDGE ( 'NONE', *, *, #54861, .T. ) ;
#43646 = DIRECTION ( 'NONE',  ( -1.000000000000000000, -0.000000000000000000, -0.000000000000000000 ) ) ;
#43647 = ADVANCED_FACE ( 'NONE', ( #24545, #53039 ), #5710, .T. ) ;
#43648 = EDGE_LOOP ( 'NONE', ( #45356, #13567, #38741, #14071 ) ) ;
#43649 = CARTESIAN_POINT ( 'NONE',  ( 1.231276596079887264, -2.246340108599748309, -41.85965512441022440 ) ) ;
#43650 = CARTESIAN_POINT ( 'NONE',  ( -2.700785417809981936, -13.56184546075580322, 3.000000000000003997 ) ) ;
#43651 = CARTESIAN_POINT ( 'NONE',  ( 0.6001305935487422083, -41.92422178329154292, -23.60027211631814126 ) ) ;
#43652 = ORIENTED_EDGE ( 'NONE', *, *, #1404, .T. ) ;
#43653 = ADVANCED_FACE ( 'NONE', ( #1639 ), #2927, .F. ) ;
#43654 = CARTESIAN_POINT ( 'NONE',  ( 0.8560838555295158248, 23.34035564869604684, -40.68907263964262455 ) ) ;
#43655 = B_SPLINE_CURVE_WITH_KNOTS ( 'NONE', 3,
 ( #38824, #15007, #57881, #43841 ),
 .UNSPECIFIED., .F., .F.,
 ( 4, 4 ),
 ( 0.000000000000000000, 0.004444103432399267896 ),
 .UNSPECIFIED. ) ;
#43656 = CARTESIAN_POINT ( 'NONE',  ( 0.6009452777970412107, -48.10564074251961131, 0.4363873594210762041 ) ) ;
#43657 = ORIENTED_EDGE ( 'NONE', *, *, #33403, .F. ) ;
#43658 = VERTEX_POINT ( 'NONE', #48970 ) ;
#43659 = EDGE_CURVE ( 'NONE', #35390, #36038, #11075, .T. ) ;
#43660 = CARTESIAN_POINT ( 'NONE',  ( 0.8760168074886965917, -29.98565522133375083, 37.61398439004481986 ) ) ;
#43661 = VECTOR ( 'NONE', #28996, 1000.000000000000000 ) ;
#43662 = VERTEX_POINT ( 'NONE', #24232 ) ;
#43663 = CARTESIAN_POINT ( 'NONE',  ( 0.6845945791218034371, 16.04817208170904408, 44.07791616614603925 ) ) ;
#43664 = DIRECTION ( 'NONE',  ( 0.000000000000000000, 0.000000000000000000, 1.000000000000000000 ) ) ;
#43665 = CIRCLE ( 'NONE', #53621, 43.08621763946400307 ) ;
#43666 = DIRECTION ( 'NONE',  ( -0.07906939808003035641, -0.2876259487683229810, 0.9544733332484380828 ) ) ;
#43667 = EDGE_CURVE ( 'NONE', #59068, #28949, #11679, .T. ) ;
#43668 = CARTESIAN_POINT ( 'NONE',  ( 0.000000000000000000, 0.000000000000000000, -0.3080913168122707546 ) ) ;
#43669 = ORIENTED_EDGE ( 'NONE', *, *, #41715, .F. ) ;
#43670 = CARTESIAN_POINT ( 'NONE',  ( 0.1158403557922069033, -1.376402091003258166, -44.10267366575070724 ) ) ;
#43671 = CARTESIAN_POINT ( 'NONE',  ( -6.015611763856276717, 0.006214430185141332774, 18.84324252354755203 ) ) ;
#43672 =( BOUNDED_SURFACE ( )  B_SPLINE_SURFACE ( 3, 1, ( 
 ( #15630, #6799 ),
 ( #6181, #1492 ),
 ( #48820, #48505 ),
 ( #1804, #35362 ) ),
 .UNSPECIFIED., .F., .F., .F. ) 
 B_SPLINE_SURFACE_WITH_KNOTS ( ( 4, 4 ),
 ( 2, 2 ),
 ( 0.000000000000000000, 1.000000000000000000 ),
 ( 0.000000000000000000, 1.000000000000000000 ),
 .UNSPECIFIED. ) 
 GEOMETRIC_REPRESENTATION_ITEM ( )  RATIONAL_B_SPLINE_SURFACE ( (
 ( 1.000000000000000000, 1.000000000000000000),
 ( 0.7223157951917480446, 0.9931996967497186413),
 ( 0.7223157951917480446, 0.9931996967497186413),
 ( 1.000000000000000000, 1.000000000000000000) ) ) 
 REPRESENTATION_ITEM ( '' )  SURFACE ( )  );
#43673 = CARTESIAN_POINT ( 'NONE',  ( 0.8554163680231738898, -24.47000373826152853, -40.03029340588557972 ) ) ;
#43674 = LINE ( 'NONE', #1630, #3031 ) ;
#43675 = ORIENTED_EDGE ( 'NONE', *, *, #1045, .F. ) ;
#43676 = CARTESIAN_POINT ( 'NONE',  ( 5.838029081930957709, 46.29164171884931989, 9.388768030290695066 ) ) ;
#43677 = CARTESIAN_POINT ( 'NONE',  ( 0.1157506346131639274, 36.92923354691153293, -24.14896207791336380 ) ) ;
#43678 = CARTESIAN_POINT ( 'NONE',  ( -6.016104459813371719, 18.19977249352317372, -4.882138007282559755 ) ) ;
#43679 = CARTESIAN_POINT ( 'NONE',  ( 1.231276596079887264, 41.91134057782999633, -0.8463462572780159343 ) ) ;
#43680 = CONICAL_SURFACE ( 'NONE', #5572, 42.08604991992415023, 1.569615340895231137 ) ;
#43681 = VERTEX_POINT ( 'NONE', #35818 ) ;
#43682 = EDGE_LOOP ( 'NONE', ( #21813, #24378, #13074, #7869 ) ) ;
#43683 = CARTESIAN_POINT ( 'NONE',  ( 5.981074661064941900, 16.27808421740009592, 12.50143471347286805 ) ) ;
#43684 = DIRECTION ( 'NONE',  ( 1.000000000000000000, 0.000000000000000000, 0.000000000000000000 ) ) ;
#43685 = CARTESIAN_POINT ( 'NONE',  ( 0.5980894510889457338, -19.05812566676475583, -44.17723055703945079 ) ) ;
#43686 = CARTESIAN_POINT ( 'NONE',  ( 3.240649175237396484, 43.49255432869266258, -6.607770831632137742 ) ) ;
#43687 = CARTESIAN_POINT ( 'NONE',  ( 3.407937589446174087, -3.987184287467878896, 13.10584870154465520 ) ) ;
#43688 = CARTESIAN_POINT ( 'NONE',  ( 4.962356264823608143, 0.000000000000000000, 0.000000000000000000 ) ) ;
#43689 = CARTESIAN_POINT ( 'NONE',  ( 5.838029081930957709, -28.03445132514680793, -38.01492597718551991 ) ) ;
#43690 = B_SPLINE_CURVE_WITH_KNOTS ( 'NONE', 3,
 ( #28721, #53127, #47843, #24329 ),
 .UNSPECIFIED., .F., .F.,
 ( 4, 4 ),
 ( 2.410497451455474575E-17, 0.004564976165746185977 ),
 .UNSPECIFIED. ) ;
#43691 = CARTESIAN_POINT ( 'NONE',  ( 1.827326673878742147, 31.30008222956382724, -29.55671596281176505 ) ) ;
#43692 = CARTESIAN_POINT ( 'NONE',  ( 4.691466044806103852, -42.32811009116544909, -14.01607102724528353 ) ) ;
#43693 = CARTESIAN_POINT ( 'NONE',  ( 0.6031356219577718170, -18.49057407199426706, -44.41207482560199793 ) ) ;
#43694 = DIRECTION ( 'NONE',  ( 1.000000000000000000, 0.000000000000000000, -0.000000000000000000 ) ) ;
#43695 = ORIENTED_EDGE ( 'NONE', *, *, #2309, .T. ) ;
#43696 = CARTESIAN_POINT ( 'NONE',  ( 0.1129192098497447394, -7.520259262076021578, -43.47870154933693243 ) ) ;
#43697 = DIRECTION ( 'NONE',  ( -1.000000000000000000, -0.000000000000000000, -0.000000000000000000 ) ) ;
#43698 = CARTESIAN_POINT ( 'NONE',  ( 47.85000000000000853, 15.50000000000000711, 1.598617397282144235E-15 ) ) ;
#43699 = CARTESIAN_POINT ( 'NONE',  ( 0.7048096507298579061, 38.67623024744047910, -28.61383451045657722 ) ) ;
#43700 = CARTESIAN_POINT ( 'NONE',  ( 0.8760168074887090262, -17.58183840866430003, 44.77533136581851636 ) ) ;
#43701 = CARTESIAN_POINT ( 'NONE',  ( 0.6017666602106488405, -46.37677619531720552, 12.78804974226019553 ) ) ;
#43702 = CYLINDRICAL_SURFACE ( 'NONE', #11691, 2.500000000000000444 ) ;
#43703 = CONTEXT_DEPENDENT_SHAPE_REPRESENTATION ( #18447, #58870 ) ;
#43704 = CARTESIAN_POINT ( 'NONE',  ( 4.549368137175248350, 0.000000000000000000, 0.000000000000000000 ) ) ;
#43705 = CARTESIAN_POINT ( 'NONE',  ( 0.6029442701453592290, 22.63682954516835011, -43.57888448895027267 ) ) ;
#43706 = EDGE_CURVE ( 'NONE', #46608, #48653, #16229, .T. ) ;
#43707 = CARTESIAN_POINT ( 'NONE',  ( 0.9740398440564321803, -10.70454588197315715, 41.55177796653844524 ) ) ;
#43708 = AXIS2_PLACEMENT_3D ( 'NONE', #58735, #24636, #6108 ) ;
#43709 = CARTESIAN_POINT ( 'NONE',  ( 2.301430502907646058, 46.04685681264146524, 13.67112791032058361 ) ) ;
#43710 = CARTESIAN_POINT ( 'NONE',  ( 0.9754292589017248272, -37.13786011588246794, 19.41923821648057569 ) ) ;
#43712 = ORIENTED_EDGE ( 'NONE', *, *, #15978, .T. ) ;
#43711 = CARTESIAN_POINT ( 'NONE',  ( 3.678834586032786458, -18.11945796638148209, -45.50052321273776812 ) ) ;
#43713 = ORIENTED_EDGE ( 'NONE', *, *, #35608, .T. ) ;
#43714 = VECTOR ( 'NONE', #41108, 999.9999999999998863 ) ;
#43715 = CARTESIAN_POINT ( 'NONE',  ( 3.376099380956842921, -12.16518930220319561, -5.631745100200117093 ) ) ;
#43716 = CARTESIAN_POINT ( 'NONE',  ( 0.5804410086790514622, 32.20888702807410908, -34.08969709850992302 ) ) ;
#43717 = CIRCLE ( 'NONE', #21642, 2.649999999999997691 ) ;
#43718 = CARTESIAN_POINT ( 'NONE',  ( 1.227938101723748288, 39.96870412324358313, -15.63977281655798812 ) ) ;
#43719 = ORIENTED_EDGE ( 'NONE', *, *, #40723, .T. ) ;
#43720 = CARTESIAN_POINT ( 'NONE',  ( 2.301529144917013436, -33.04216096093427524, 34.86298839095273649 ) ) ;
#43721 = FACE_OUTER_BOUND ( 'NONE', #18373, .T. ) ;
#43722 = CARTESIAN_POINT ( 'NONE',  ( 0.5809828226811617480, -41.20389530892290253, -24.41822904836968178 ) ) ;
#43723 = ORIENTED_EDGE ( 'NONE', *, *, #20055, .F. ) ;
#43724 = ORIENTED_EDGE ( 'NONE', *, *, #27825, .F. ) ;
#43725 = B_SPLINE_CURVE_WITH_KNOTS ( 'NONE', 3,
 ( #31596, #11898, #36014, #11256, #21581, #45406 ),
 .UNSPECIFIED., .F., .F.,
 ( 4, 2, 4 ),
 ( 3.551486221896847302E-18, 0.0002445244328975372940, 0.0004890488657950710100 ),
 .UNSPECIFIED. ) ;
#43726 = CARTESIAN_POINT ( 'NONE',  ( 0.9268187852002115479, 28.89887655679548573, -33.29578451791941518 ) ) ;
#43727 = CARTESIAN_POINT ( 'NONE',  ( 4.975610109902397937, 42.33317580307119954, 24.50207406657730047 ) ) ;
#43728 = AXIS2_PLACEMENT_3D ( 'NONE', #46630, #50991, #27198 ) ;
#43729 = CARTESIAN_POINT ( 'NONE',  ( 0.9762797500689124330, 36.31338395866797697, 20.92039508843128814 ) ) ;
#43730 = CARTESIAN_POINT ( 'NONE',  ( 0.5824935313925958535, 46.89462116659080237, -0.3642563599602811064 ) ) ;
#43731 = CARTESIAN_POINT ( 'NONE',  ( 1.227938101723748288, -10.28900963485351205, -41.66816631169202623 ) ) ;
#43732 = AXIS2_PLACEMENT_3D ( 'NONE', #41384, #60440, #17562 ) ;
#43733 = CARTESIAN_POINT ( 'NONE',  ( 4.960156602257184133, 43.79161740034498251, -15.40604254112596649 ) ) ;
#43734 = EDGE_CURVE ( 'NONE', #34317, #23714, #26648, .T. ) ;
#43735 = CARTESIAN_POINT ( 'NONE',  ( 0.8744876279028306332, -34.64280934553560343, 34.78829991575276637 ) ) ;
#43736 = ADVANCED_FACE ( 'NONE', ( #55503 ), #24525, .F. ) ;
#43737 = EDGE_LOOP ( 'NONE', ( #20610, #49472, #39765, #48178 ) ) ;
#43738 = ORIENTED_EDGE ( 'NONE', *, *, #33681, .F. ) ;
#43739 = B_SPLINE_CURVE_WITH_KNOTS ( 'NONE', 3,
 ( #29989, #34705, #40655, #10900, #53470, #54701 ),
 .UNSPECIFIED., .F., .F.,
 ( 4, 2, 4 ),
 ( 1.084202172485504434E-19, 0.0002445244328975344208, 0.0004890488657950687332 ),
 .UNSPECIFIED. ) ;
#43740 = CARTESIAN_POINT ( 'NONE',  ( -2.708315649062910779, -3.532515819624256537, -14.20182604343558985 ) ) ;
#43741 = CARTESIAN_POINT ( 'NONE',  ( 1.231276596079881047, -41.87427716283725943, 1.954912557623087022 ) ) ;
#43742 = EDGE_LOOP ( 'NONE', ( #7504, #51926 ) ) ;
#43743 = CARTESIAN_POINT ( 'NONE',  ( 4.975801465491695552, 21.70134120755140827, 42.71626295676271212 ) ) ;
#43744 = CARTESIAN_POINT ( 'NONE',  ( 0.6845945791218023269, -2.432797934429159703, -46.84536278997295256 ) ) ;
#43745 = EDGE_CURVE ( 'NONE', #32075, #16670, #8935, .T. ) ;
#43746 = CARTESIAN_POINT ( 'NONE',  ( 0.5980894510889448457, -23.44630161211557606, -42.01322166096910848 ) ) ;
#43747 = CARTESIAN_POINT ( 'NONE',  ( 5.895881250540457863, 3.340873024792334167, 19.83346286054243279 ) ) ;
#43748 = ORIENTED_EDGE ( 'NONE', *, *, #43321, .F. ) ;
#43749 = CYLINDRICAL_SURFACE ( 'NONE', #41787, 10.00000000000000000 ) ;
#43750 = CARTESIAN_POINT ( 'NONE',  ( 0.6041374136657475802, -44.37863742124655175, -18.57118264377523076 ) ) ;
#43751 = CARTESIAN_POINT ( 'NONE',  ( 0.5997462898726536595, 28.52220283460682282, -39.97543715340528081 ) ) ;
#43752 = CARTESIAN_POINT ( 'NONE',  ( -31.75000000000000000, 0.000000000000000000, 0.000000000000000000 ) ) ;
#43753 = ORIENTED_EDGE ( 'NONE', *, *, #41759, .T. ) ;
#43754 = DIRECTION ( 'NONE',  ( -1.000000000000000000, -1.836909530733554547E-16, -1.836909530733573529E-16 ) ) ;
#43755 = CIRCLE ( 'NONE', #51712, 48.91267123290010943 ) ;
#43756 = VERTEX_POINT ( 'NONE', #6954 ) ;
#43757 = CARTESIAN_POINT ( 'NONE',  ( -1.500000000000000888, 6.728125000000022560, 0.000000000000000000 ) ) ;
#43758 = CARTESIAN_POINT ( 'NONE',  ( 0.5837374860065628335, 23.79054246378028026, -41.56971235019459954 ) ) ;
#43759 =( BOUNDED_SURFACE ( )  B_SPLINE_SURFACE ( 3, 1, ( 
 ( #37014, #32919 ),
 ( #61379, #22582 ),
 ( #13188, #17574 ),
 ( #41708, #23491 ) ),
 .UNSPECIFIED., .F., .F., .F. ) 
 B_SPLINE_SURFACE_WITH_KNOTS ( ( 4, 4 ),
 ( 2, 2 ),
 ( 0.000000000000000000, 1.000000000000000000 ),
 ( 0.000000000000000000, 1.000000000000000000 ),
 .UNSPECIFIED. ) 
 GEOMETRIC_REPRESENTATION_ITEM ( )  RATIONAL_B_SPLINE_SURFACE ( (
 ( 1.000000000000000000, 1.000000000000000000),
 ( 0.7211978278499970862, 0.9934217856018976445),
 ( 0.7211978278499970862, 0.9934217856018976445),
 ( 1.000000000000000000, 1.000000000000000000) ) ) 
 REPRESENTATION_ITEM ( '' )  SURFACE ( )  );
#43760 = EDGE_CURVE ( 'NONE', #9945, #57622, #46874, .T. ) ;
#43761 = STYLED_ITEM ( 'NONE', ( #50742 ), #32490 ) ;
#43762 = ORIENTED_EDGE ( 'NONE', *, *, #22576, .F. ) ;
#43763 = CARTESIAN_POINT ( 'NONE',  ( -6.017396004339686577, -4.875835690939308797, 18.20140164570667807 ) ) ;
#43764 = VECTOR ( 'NONE', #23901, 1000.000000000000000 ) ;
#43765 = CARTESIAN_POINT ( 'NONE',  ( 0.6017666602106490625, -47.64919188470832978, 6.625262199740270752 ) ) ;
#43766 = EDGE_CURVE ( 'NONE', #61780, #33708, #31409, .T. ) ;
#43767 = CARTESIAN_POINT ( 'NONE',  ( 0.5848930533535030563, -34.65838163711107711, -31.59224057714044775 ) ) ;
#43768 = CARTESIAN_POINT ( 'NONE',  ( 4.553261556744873317, 43.53643125131393532, -5.841123155973635406 ) ) ;
#43769 = CARTESIAN_POINT ( 'NONE',  ( 0.1135584504625008206, 33.87666299352049748, -28.27231431203839307 ) ) ;
#43770 = DIRECTION ( 'NONE',  ( 1.000000000000000000, -0.000000000000000000, -0.000000000000000000 ) ) ;
#43771 = CARTESIAN_POINT ( 'NONE',  ( 3.238018933889920792, 10.68005193312848888, 8.083562523623562868 ) ) ;
#43772 = CYLINDRICAL_SURFACE ( 'NONE', #1778, 2.649999999999992806 ) ;
#43773 = ORIENTED_EDGE ( 'NONE', *, *, #45871, .T. ) ;
#43774 = FACE_OUTER_BOUND ( 'NONE', #28014, .T. ) ;
#43775 = AXIS2_PLACEMENT_3D ( 'NONE', #31989, #42326, #37309 ) ;
#43776 = CARTESIAN_POINT ( 'NONE',  ( 1.000433927950263424, 14.44615545540195356, -39.34116508456767747 ) ) ;
#43777 =( BOUNDED_SURFACE ( )  B_SPLINE_SURFACE ( 3, 1, ( 
 ( #5036, #57046 ),
 ( #19481, #52659 ),
 ( #52046, #42995 ),
 ( #4108, #9139 ) ),
 .UNSPECIFIED., .F., .F., .F. ) 
 B_SPLINE_SURFACE_WITH_KNOTS ( ( 4, 4 ),
 ( 2, 2 ),
 ( 0.000000000000000000, 1.000000000000000000 ),
 ( 0.000000000000000000, 1.000000000000000000 ),
 .UNSPECIFIED. ) 
 GEOMETRIC_REPRESENTATION_ITEM ( )  RATIONAL_B_SPLINE_SURFACE ( (
 ( 1.000000000000000000, 1.000000000000000000),
 ( 0.9952954269826590483, 0.8620686068821339365),
 ( 0.9952954269826590483, 0.8620686068821339365),
 ( 1.000000000000000000, 1.000000000000000000) ) ) 
 REPRESENTATION_ITEM ( '' )  SURFACE ( )  );
#43778 = LINE ( 'NONE', #48141, #55796 ) ;
#43779 = ORIENTED_EDGE ( 'NONE', *, *, #57903, .F. ) ;
#43781 = CARTESIAN_POINT ( 'NONE',  ( -16.69292671586258336, -12.38819954910475118, 1.669860868477914151 ) ) ;
#43780 =( BOUNDED_SURFACE ( )  B_SPLINE_SURFACE ( 3, 1, ( 
 ( #3305, #40041 ),
 ( #59091, #21204 ),
 ( #40963, #45963 ),
 ( #41258, #16202 ) ),
 .UNSPECIFIED., .F., .F., .F. ) 
 B_SPLINE_SURFACE_WITH_KNOTS ( ( 4, 4 ),
 ( 2, 2 ),
 ( 0.000000000000000000, 1.000000000000000000 ),
 ( 0.000000000000000000, 1.000000000000000000 ),
 .UNSPECIFIED. ) 
 GEOMETRIC_REPRESENTATION_ITEM ( )  RATIONAL_B_SPLINE_SURFACE ( (
 ( 1.000000000000000000, 1.000000000000000000),
 ( 0.9754377213608244057, 0.9999580625633939235),
 ( 0.9754377213608244057, 0.9999580625633939235),
 ( 1.000000000000000000, 1.000000000000000000) ) ) 
 REPRESENTATION_ITEM ( '' )  SURFACE ( )  );
#43782 = CARTESIAN_POINT ( 'NONE',  ( 4.694002226626921015, 39.88981857773250539, 22.07005086722095299 ) ) ;
#43783 = CARTESIAN_POINT ( 'NONE',  ( 0.6028777368367060907, 22.63683791566365500, 43.57881823192369097 ) ) ;
#43784 = B_SPLINE_CURVE_WITH_KNOTS ( 'NONE', 3,
 ( #30086, #6558, #25083, #11004 ),
 .UNSPECIFIED., .F., .F.,
 ( 4, 4 ),
 ( 0.000000000000000000, 0.004445488388166991649 ),
 .UNSPECIFIED. ) ;
#43785 = CARTESIAN_POINT ( 'NONE',  ( -6.016489644550737204, -17.40716454747924047, -7.215050741358225217 ) ) ;
#43786 = CARTESIAN_POINT ( 'NONE',  ( 4.956445790444011124, -16.41925925744418180, -44.13554095710700409 ) ) ;
#43787 = DIRECTION ( 'NONE',  ( 0.000000000000000000, 0.000000000000000000, 1.000000000000000000 ) ) ;
#43788 = CARTESIAN_POINT ( 'NONE',  ( 0.8751705887134423323, 17.57879340691479797, 44.76769609654243709 ) ) ;
#43789 = EDGE_CURVE ( 'NONE', #48040, #48449, #34868, .T. ) ;
#43790 = CARTESIAN_POINT ( 'NONE',  ( 2.500000000000000000, 0.000000000000000000, 0.000000000000000000 ) ) ;
#43791 = AXIS2_PLACEMENT_3D ( 'NONE', #42467, #18033, #42772 ) ;
#43792 = CARTESIAN_POINT ( 'NONE',  ( 0.2885697896453109368, -25.60460893337453214, -34.69058521462526556 ) ) ;
#43794 = VERTEX_POINT ( 'NONE', #25778 ) ;
#43793 = DIRECTION ( 'NONE',  ( -1.000000000000000000, -0.000000000000000000, -0.000000000000000000 ) ) ;
#43795 = VERTEX_POINT ( 'NONE', #7264 ) ;
#43796 = CARTESIAN_POINT ( 'NONE',  ( 0.5806925824938499181, 46.89268439822727430, 0.5463627657667635695 ) ) ;
#43797 = CARTESIAN_POINT ( 'NONE',  ( 0.7048096507298635682, 0.8437160066900629696, 48.10291524268443197 ) ) ;
#43798 = CARTESIAN_POINT ( 'NONE',  ( 0.1101816497532063233, 16.62841624476621050, 39.78963561881071342 ) ) ;
#43799 = ADVANCED_FACE ( 'NONE', ( #26702 ), #54888, .F. ) ;
#43800 = CARTESIAN_POINT ( 'NONE',  ( 0.5850706913938534814, 47.50996714391782660, 6.071602062250778253 ) ) ;
#43801 = CARTESIAN_POINT ( 'NONE',  ( 0.7245667037590752813, 11.65533952568352483, -46.66865388241075152 ) ) ;
#43802 = EDGE_LOOP ( 'NONE', ( #48191, #30219, #20762, #45226 ) ) ;
#43803 = AXIS2_PLACEMENT_3D ( 'NONE', #54011, #21445, #11134 ) ;
#43804 = CARTESIAN_POINT ( 'NONE',  ( 0.5848930533535030563, -14.06811673146470909, -44.73657534967826876 ) ) ;
#43805 = AXIS2_PLACEMENT_3D ( 'NONE', #23309, #41200, #2948 ) ;
#43806 = CARTESIAN_POINT ( 'NONE',  ( 7.999999999999986677, 58.44237546506807490, 54.69470952477956871 ) ) ;
#43807 = VECTOR ( 'NONE', #53927, 1000.000000000000000 ) ;
#43808 = CARTESIAN_POINT ( 'NONE',  ( 1.231276596079887264, -11.60895935156443848, 40.28037777618019533 ) ) ;
#43809 = ORIENTED_EDGE ( 'NONE', *, *, #20579, .T. ) ;
#43810 = B_SPLINE_CURVE_WITH_KNOTS ( 'NONE', 3,
 ( #36079, #46389, #41699, #55137, #31354, #36385 ),
 .UNSPECIFIED., .F., .F.,
 ( 4, 2, 4 ),
 ( 1.246832498358330292E-18, 0.0002293801035737089925, 0.0004587602071474167383 ),
 .UNSPECIFIED. ) ;
#43811 = DIRECTION ( 'NONE',  ( -1.000000000000000000, -0.000000000000000000, -0.000000000000000000 ) ) ;
#43812 = FACE_OUTER_BOUND ( 'NONE', #10346, .T. ) ;
#43813 = EDGE_LOOP ( 'NONE', ( #11052, #12130, #37355, #26345 ) ) ;
#43814 = FACE_OUTER_BOUND ( 'NONE', #10375, .T. ) ;
#43815 = EDGE_CURVE ( 'NONE', #10282, #37103, #7579, .T. ) ;
#43816 = ORIENTED_EDGE ( 'NONE', *, *, #14610, .T. ) ;
#43817 = CARTESIAN_POINT ( 'NONE',  ( 51.82869273375258956, 15.32880936072750799, -2.299358913708370533 ) ) ;
#43818 = FACE_OUTER_BOUND ( 'NONE', #8593, .T. ) ;
#43819 = ORIENTED_EDGE ( 'NONE', *, *, #61432, .F. ) ;
#43820 = FACE_OUTER_BOUND ( 'NONE', #23371, .T. ) ;
#43821 = CARTESIAN_POINT ( 'NONE',  ( 0.8554163680231738898, 46.90810212776802501, 0.9140174411379243802 ) ) ;
#43822 = EDGE_CURVE ( 'NONE', #45706, #9797, #13236, .T. ) ;
#43823 = CARTESIAN_POINT ( 'NONE',  ( 0.7242486021783808292, 21.98223893955317010, 43.90663541628263289 ) ) ;
#43824 = CARTESIAN_POINT ( 'NONE',  ( 2.500000000000000000, 1.178949249685212974, -2.042000000000001148 ) ) ;
#43825 = ORIENTED_EDGE ( 'NONE', *, *, #38350, .T. ) ;
#43826 = CARTESIAN_POINT ( 'NONE',  ( 2.618530812446115519, -35.79257080906851485, -30.47324505325967792 ) ) ;
#43827 = CARTESIAN_POINT ( 'NONE',  ( 0.6017666602106490625, -0.3491145841135456229, -48.10631669010027878 ) ) ;
#43828 = ORIENTED_EDGE ( 'NONE', *, *, #14011, .F. ) ;
#43829 = DIRECTION ( 'NONE',  ( 0.000000000000000000, 0.000000000000000000, 1.000000000000000000 ) ) ;
#43830 = EDGE_LOOP ( 'NONE', ( #45727, #45954, #57226, #27013 ) ) ;
#43831 = CARTESIAN_POINT ( 'NONE',  ( -6.079354080745853928, -14.66314846858153054, -12.48138743235291059 ) ) ;
#43832 = AXIS2_PLACEMENT_3D ( 'NONE', #61235, #33690, #13654 ) ;
#43833 = ORIENTED_EDGE ( 'NONE', *, *, #3537, .T. ) ;
#43834 = CARTESIAN_POINT ( 'NONE',  ( 0.7056313189692720034, -46.84548992230426023, -2.291008052550091101 ) ) ;
#43835 = FACE_OUTER_BOUND ( 'NONE', #48696, .T. ) ;
#43836 = CARTESIAN_POINT ( 'NONE',  ( 0.2940133293163007533, 10.59968119980750423, -42.82391047114322902 ) ) ;
#43837 = ORIENTED_EDGE ( 'NONE', *, *, #30725, .F. ) ;
#43838 = CARTESIAN_POINT ( 'NONE',  ( 4.549368137175248350, 28.46244473166628097, 32.13400537129935230 ) ) ;
#43839 = CARTESIAN_POINT ( 'NONE',  ( 0.2285344041767068402, -38.06330129766492831, 22.30888308765448258 ) ) ;
#43840 = EDGE_CURVE ( 'NONE', #48016, #41399, #59471, .T. ) ;
#43841 = CARTESIAN_POINT ( 'NONE',  ( 0.8744876279028263033, -26.20733431478184983, 41.51536677536103070 ) ) ;
#43842 = ORIENTED_EDGE ( 'NONE', *, *, #56835, .F. ) ;
#43843 = ORIENTED_EDGE ( 'NONE', *, *, #7536, .T. ) ;
#43844 = CARTESIAN_POINT ( 'NONE',  ( 4.691466044806102076, 43.79545162262309077, -8.371234562541387092 ) ) ;
#43845 = CARTESIAN_POINT ( 'NONE',  ( 4.553261556744875094, 0.000000000000000000, 0.000000000000000000 ) ) ;
#43846 = CARTESIAN_POINT ( 'NONE',  ( 0.7044674535453004927, 32.38853019898915164, -36.91592927666964385 ) ) ;
#43847 = CARTESIAN_POINT ( 'NONE',  ( 0.7242003506639982380, -13.18377730284193028, 47.29904534084272427 ) ) ;
#43848 = CARTESIAN_POINT ( 'NONE',  ( 0.9769922540276054779, 38.40851559224979184, 16.76655853435725163 ) ) ;
#43849 = ORIENTED_EDGE ( 'NONE', *, *, #16140, .T. ) ;
#43850 = CARTESIAN_POINT ( 'NONE',  ( 0.8554163680231720024, 28.56078411578431542, 37.22213163970302219 ) ) ;
#43851 = ORIENTED_EDGE ( 'NONE', *, *, #33615, .F. ) ;
#43852 = CIRCLE ( 'NONE', #25790, 9.499999999999996447 ) ;
#43853 = CARTESIAN_POINT ( 'NONE',  ( 0.6029303876144825880, 12.32464004947814651, 46.50193792184029462 ) ) ;
#43854 = CARTESIAN_POINT ( 'NONE',  ( 4.975610109902397937, 0.000000000000000000, 0.000000000000000000 ) ) ;
#43855 = DIRECTION ( 'NONE',  ( -1.000000000000000000, -0.000000000000000000, -0.000000000000000000 ) ) ;
#43856 = CARTESIAN_POINT ( 'NONE',  ( 0.9741495583595186636, -21.79582154536828753, 36.96045061395525266 ) ) ;
#43857 = CARTESIAN_POINT ( 'NONE',  ( -6.078457390727109555, 19.09849343800966182, 2.458060096053366284 ) ) ;
#43858 = DIRECTION ( 'NONE',  ( 0.000000000000000000, 0.000000000000000000, 1.000000000000000000 ) ) ;
#43859 =( BOUNDED_SURFACE ( )  B_SPLINE_SURFACE ( 3, 1, ( 
 ( #6033, #40534 ),
 ( #35520, #15175 ),
 ( #39609, #35210 ),
 ( #30789, #30473 ) ),
 .UNSPECIFIED., .F., .F., .F. ) 
 B_SPLINE_SURFACE_WITH_KNOTS ( ( 4, 4 ),
 ( 2, 2 ),
 ( 0.000000000000000000, 1.000000000000000000 ),
 ( 0.000000000000000000, 1.000000000000000000 ),
 .UNSPECIFIED. ) 
 GEOMETRIC_REPRESENTATION_ITEM ( )  RATIONAL_B_SPLINE_SURFACE ( (
 ( 1.000000000000000000, 1.000000000000000000),
 ( 0.9952954269826590483, 0.8620686068821307169),
 ( 0.9952954269826590483, 0.8620686068821307169),
 ( 1.000000000000000000, 1.000000000000000000) ) ) 
 REPRESENTATION_ITEM ( '' )  SURFACE ( )  );
#43860 = CARTESIAN_POINT ( 'NONE',  ( 0.1140933569871964010, 20.74467474435255809, -38.94365699102905864 ) ) ;
#43861 = CARTESIAN_POINT ( 'NONE',  ( 4.549368137175248350, 23.67244292351589507, 35.80950303116109268 ) ) ;
#43862 = CARTESIAN_POINT ( 'NONE',  ( -6.077587904424778920, 3.079371755031420133, 19.00824797261034149 ) ) ;
#43863 =( BOUNDED_SURFACE ( )  B_SPLINE_SURFACE ( 3, 1, ( 
 ( #23999, #163 ),
 ( #9580, #47819 ),
 ( #48121, #4867 ),
 ( #53411, #4248 ) ),
 .UNSPECIFIED., .F., .F., .F. ) 
 B_SPLINE_SURFACE_WITH_KNOTS ( ( 4, 4 ),
 ( 2, 2 ),
 ( 0.000000000000000000, 1.000000000000000000 ),
 ( 0.000000000000000000, 1.000000000000000000 ),
 .UNSPECIFIED. ) 
 GEOMETRIC_REPRESENTATION_ITEM ( )  RATIONAL_B_SPLINE_SURFACE ( (
 ( 1.000000000000000000, 1.000000000000000000),
 ( 0.9751682680413298332, 0.9999560080971552356),
 ( 0.9751682680413298332, 0.9999560080971552356),
 ( 1.000000000000000000, 1.000000000000000000) ) ) 
 REPRESENTATION_ITEM ( '' )  SURFACE ( )  );
#43864 = CARTESIAN_POINT ( 'NONE',  ( 1.092182651088185796, 4.971552582430809331, 41.61784292058406720 ) ) ;
#43865 = AXIS2_PLACEMENT_3D ( 'NONE', #19328, #56897, #34057 ) ;
#43866 = DIRECTION ( 'NONE',  ( -1.000000000000000000, -0.000000000000000000, -0.000000000000000000 ) ) ;
#43867 = CARTESIAN_POINT ( 'NONE',  ( 2.648799415243696664, -18.57388519568332086, -45.38202564922784177 ) ) ;
#43868 = DIRECTION ( 'NONE',  ( -0.1736481776669314137, 0.9848077530122077983, -5.551115123125779004E-17 ) ) ;
#43869 = EDGE_CURVE ( 'NONE', #23834, #9388, #8660, .T. ) ;
#43870 =( GEOMETRIC_REPRESENTATION_CONTEXT ( 3 ) GLOBAL_UNCERTAINTY_ASSIGNED_CONTEXT ( ( #19209 ) ) GLOBAL_UNIT_ASSIGNED_CONTEXT ( ( #60142, #53209, #24719 ) ) REPRESENTATION_CONTEXT ( 'NONE', 'WORKASPACE' ) );
#43871 = VERTEX_POINT ( 'NONE', #18543 ) ;
#43872 = EDGE_CURVE ( 'NONE', #56645, #47069, #9442, .T. ) ;
#43873 =( LENGTH_UNIT ( ) NAMED_UNIT ( * ) SI_UNIT ( .MILLI., .METRE. ) );
#43874 = CARTESIAN_POINT ( 'NONE',  ( 4.956445790443988031, 0.000000000000000000, 0.000000000000000000 ) ) ;
#43875 = CARTESIAN_POINT ( 'NONE',  ( 0.6029442701453591180, -47.52343932222595413, -12.37206288963105116 ) ) ;
#43876 = DIRECTION ( 'NONE',  ( -1.000000000000000000, -0.000000000000000000, -0.000000000000000000 ) ) ;
#43877 = CARTESIAN_POINT ( 'NONE',  ( 4.967162193818130511, 38.83676580803767564, 18.65818244221271627 ) ) ;
#43878 = ORIENTED_EDGE ( 'NONE', *, *, #53780, .F. ) ;
#43879 = DIRECTION ( 'NONE',  ( 0.000000000000000000, 0.000000000000000000, 1.000000000000000000 ) ) ;
#43880 = LINE ( 'NONE', #34768, #5892 ) ;
#43881 = B_SPLINE_CURVE_WITH_KNOTS ( 'NONE', 3,
 ( #32397, #12369, #32088, #2938, #51468, #42128 ),
 .UNSPECIFIED., .F., .F.,
 ( 4, 2, 4 ),
 ( 1.289608238010044742E-17, 0.0002291978881530118233, 0.0004583957763060107445 ),
 .UNSPECIFIED. ) ;
#43882 = FACE_OUTER_BOUND ( 'NONE', #16228, .T. ) ;
#43883 = ORIENTED_EDGE ( 'NONE', *, *, #31991, .T. ) ;
#43885 = CARTESIAN_POINT ( 'NONE',  ( 4.553261556744873317, -29.69864478935373242, -32.36556910513746743 ) ) ;
#43884 = B_SPLINE_CURVE_WITH_KNOTS ( 'NONE', 3,
 ( #32611, #23821, #4366, #42335 ),
 .UNSPECIFIED., .F., .F.,
 ( 4, 4 ),
 ( 0.000000000000000000, 0.005013413432710141573 ),
 .UNSPECIFIED. ) ;
#43886 = CARTESIAN_POINT ( 'NONE',  ( 0.5807400328401637335, 6.791881299635582181, 47.41494605191445544 ) ) ;
#43887 = EDGE_CURVE ( 'NONE', #55761, #17913, #4987, .T. ) ;
#43888 = ORIENTED_EDGE ( 'NONE', *, *, #65, .F. ) ;
#43889 = AXIS2_PLACEMENT_3D ( 'NONE', #8716, #56015, #60392 ) ;
#43890 = CARTESIAN_POINT ( 'NONE',  ( 1.154321485836934169, -6.418927614505812507, -42.43366804742923648 ) ) ;
#43891 = CIRCLE ( 'NONE', #57837, 48.91267123290010943 ) ;
#43892 = VERTEX_POINT ( 'NONE', #3494 ) ;
#43893 = FACE_BOUND ( 'NONE', #21209, .T. ) ;
#43895 = EDGE_LOOP ( 'NONE', ( #35933, #4822, #42346, #35868 ) ) ;
#43894 = EDGE_CURVE ( 'NONE', #35714, #6983, #9136, .T. ) ;
#43896 = CARTESIAN_POINT ( 'NONE',  ( 0.1152339509894530906, 29.49895703548700965, -32.81393338619639621 ) ) ;
#43897 = CARTESIAN_POINT ( 'NONE',  ( 0.8751705887134423323, -28.56654290188627243, -38.69254731947824411 ) ) ;
#43898 = ORIENTED_EDGE ( 'NONE', *, *, #38983, .T. ) ;
#43899 = CARTESIAN_POINT ( 'NONE',  ( 1.227938101723756947, -39.32113113558978057, 17.20315230597830336 ) ) ;
#43900 = ORIENTED_EDGE ( 'NONE', *, *, #52275, .T. ) ;
#43901 = CARTESIAN_POINT ( 'NONE',  ( 0.3622758884714730732, -41.42293301073634382, 11.95365414648425428 ) ) ;
#43902 = EDGE_CURVE ( 'NONE', #32533, #24195, #15921, .T. ) ;
#43903 = CARTESIAN_POINT ( 'NONE',  ( 3.407937589446178528, 5.663729899985073146, 12.47329436636630717 ) ) ;
#43904 = CARTESIAN_POINT ( 'NONE',  ( 0.5824936645240090805, 40.16258313460651408, 24.21167270132587390 ) ) ;
#43905 = ORIENTED_EDGE ( 'NONE', *, *, #45334, .T. ) ;
#43906 = DIRECTION ( 'NONE',  ( 0.000000000000000000, 0.000000000000000000, -1.000000000000000000 ) ) ;
#43907 = CARTESIAN_POINT ( 'NONE',  ( 1.479689385636123067, -36.00353389669128745, -25.40333427362427088 ) ) ;
#43908 = B_SPLINE_CURVE_WITH_KNOTS ( 'NONE', 3,
 ( #11166, #57502, #14641, #9934 ),
 .UNSPECIFIED., .F., .F.,
 ( 4, 4 ),
 ( 0.000000000000000000, 0.004445488388166994251 ),
 .UNSPECIFIED. ) ;
#43909 = CIRCLE ( 'NONE', #40910, 47.09074272231896430 ) ;
#43910 = CARTESIAN_POINT ( 'NONE',  ( 0.8560838555295158248, -34.16988317699912159, -32.13708010619451727 ) ) ;
#43911 = CARTESIAN_POINT ( 'NONE',  ( 4.833616638992205949, 38.20222678111901615, 26.07076047129148932 ) ) ;
#43912 = ORIENTED_EDGE ( 'NONE', *, *, #1765, .F. ) ;
#43913 = FACE_OUTER_BOUND ( 'NONE', #61333, .T. ) ;
#43914 = EDGE_CURVE ( 'NONE', #42725, #33861, #24426, .T. ) ;
#43915 = CARTESIAN_POINT ( 'NONE',  ( 0.5988103622719992414, -13.03604477829323116, 46.30780754281411049 ) ) ;
#43916 = ORIENTED_EDGE ( 'NONE', *, *, #61302, .F. ) ;
#43917 = DIRECTION ( 'NONE',  ( 0.1736481776669315247, -0.9848077530122079093, 5.551115123125782702E-17 ) ) ;
#43918 = ORIENTED_EDGE ( 'NONE', *, *, #38279, .T. ) ;
#43919 = AXIS2_PLACEMENT_3D ( 'NONE', #44097, #20562, #25872 ) ;
#43920 = CARTESIAN_POINT ( 'NONE',  ( 0.5809828226811617480, -47.55412398569210808, 5.711058609465143654 ) ) ;
#43921 = CARTESIAN_POINT ( 'NONE',  ( 0.9791128995231621612, 40.41828153704135218, -11.07700103090292387 ) ) ;
#43922 = EDGE_LOOP ( 'NONE', ( #60782, #6604, #21810, #53740 ) ) ;
#43923 = CARTESIAN_POINT ( 'NONE',  ( 0.9791128995231614951, -12.42139118001737508, -40.02557276790864194 ) ) ;
#43924 = CARTESIAN_POINT ( 'NONE',  ( 4.958415959904820092, -41.61824873627326582, 18.19684934125486819 ) ) ;
#43925 = CARTESIAN_POINT ( 'NONE',  ( 0.3676999524040323597, -42.45338881270421894, -11.98584004733086061 ) ) ;
#43926 = CARTESIAN_POINT ( 'NONE',  ( -6.072942160501519027, 15.44092479507881421, -11.50573786255104913 ) ) ;
#43927 = ORIENTED_EDGE ( 'NONE', *, *, #31292, .F. ) ;
#43928 = DIRECTION ( 'NONE',  ( 0.000000000000000000, 0.000000000000000000, 1.000000000000000000 ) ) ;
#43929 = CARTESIAN_POINT ( 'NONE',  ( 4.956653778116966613, 0.000000000000000000, 0.000000000000000000 ) ) ;
#43930 = FACE_OUTER_BOUND ( 'NONE', #4057, .T. ) ;
#43931 = CARTESIAN_POINT ( 'NONE',  ( 0.6067375320500725255, 46.07640252006478221, 13.08014790719042253 ) ) ;
#43932 = CARTESIAN_POINT ( 'NONE',  ( 3.221118495291109607, -8.878221871482150362, -43.08060579962272385 ) ) ;
#43933 = CIRCLE ( 'NONE', #26910, 43.92652462719577500 ) ;
#43934 = CARTESIAN_POINT ( 'NONE',  ( 5.959547316686252039, -17.77392908783941294, 10.26589671991332331 ) ) ;
#43935 = EDGE_CURVE ( 'NONE', #48550, #59818, #32655, .T. ) ;
#43936 = CIRCLE ( 'NONE', #12889, 42.92674063221959813 ) ;
#43937 = CARTESIAN_POINT ( 'NONE',  ( -15.88721936851159811, -7.996419009245403942, 0.2752209306966177937 ) ) ;
#43938 = LINE ( 'NONE', #30100, #60374 ) ;
#43939 = EDGE_CURVE ( 'NONE', #4, #3487, #23527, .T. ) ;
#43940 = CARTESIAN_POINT ( 'NONE',  ( -6.015611763856276717, -16.31561949997082905, 9.427003116184113907 ) ) ;
#43941 = LINE ( 'NONE', #52670, #39154 ) ;
#43942 = CARTESIAN_POINT ( 'NONE',  ( 0.1155031312995260795, 39.68109568858822911, 19.29643172933567996 ) ) ;
#43943 = CARTESIAN_POINT ( 'NONE',  ( 4.956445790444003130, -40.78973928653796577, 23.53157918788916803 ) ) ;
#43944 = EDGE_CURVE ( 'NONE', #31565, #44340, #40773, .T. ) ;
#43945 = ADVANCED_FACE ( 'NONE', ( #4104, #42073 ), #18243, .F. ) ;
#43946 = CARTESIAN_POINT ( 'NONE',  ( 0.5838002273316416080, 33.77111476497777431, 33.96372661229951007 ) ) ;
#43947 = CARTESIAN_POINT ( 'NONE',  ( -2.601141883200665639, 14.86024923780642304, 1.403003941427925394 ) ) ;
#43948 = ADVANCED_FACE ( 'NONE', ( #60820 ), #17940, .T. ) ;
#43949 = ORIENTED_EDGE ( 'NONE', *, *, #9500, .T. ) ;
#43950 = CIRCLE ( 'NONE', #50245, 42.92674063221959813 ) ;
#43951 = CARTESIAN_POINT ( 'NONE',  ( 0.8560838555295158248, -39.18289055412748922, 25.78902716088759206 ) ) ;
#43952 = CARTESIAN_POINT ( 'NONE',  ( 0.9780106845699476636, -1.713796700228813918, 41.87354949518520186 ) ) ;
#43953 = LINE ( 'NONE', #14806, #52711 ) ;
#43954 = ORIENTED_EDGE ( 'NONE', *, *, #60314, .F. ) ;
#43955 = CARTESIAN_POINT ( 'NONE',  ( 0.9740398440564311811, 6.011466167924099935, 42.48528956276139468 ) ) ;
#43956 = CARTESIAN_POINT ( 'NONE',  ( 0.6845945791218034371, 36.27071225238031360, 29.74629310383012992 ) ) ;
#43957 = ORIENTED_EDGE ( 'NONE', *, *, #10884, .F. ) ;
#43958 = ORIENTED_EDGE ( 'NONE', *, *, #50062, .F. ) ;
#43959 = CARTESIAN_POINT ( 'NONE',  ( 5.959547316686252039, 16.28190225198618535, -12.49803383497733122 ) ) ;
#43960 = EDGE_CURVE ( 'NONE', #14660, #17426, #13130, .T. ) ;
#43961 = ORIENTED_EDGE ( 'NONE', *, *, #1107, .F. ) ;
#43962 = CARTESIAN_POINT ( 'NONE',  ( 0.8751705887134553219, -17.57879340691572878, 44.76769609654206050 ) ) ;
#43964 = ORIENTED_EDGE ( 'NONE', *, *, #35203, .T. ) ;
#43963 = EDGE_CURVE ( 'NONE', #49963, #11438, #52655, .T. ) ;
#43965 = VERTEX_POINT ( 'NONE', #19791 ) ;
#43966 = FACE_OUTER_BOUND ( 'NONE', #15898, .T. ) ;
#43967 = ORIENTED_EDGE ( 'NONE', *, *, #29204, .F. ) ;
#43968 = DIRECTION ( 'NONE',  ( 0.9848077530122077983, 0.1736481776669316079, -1.387778780781445367E-17 ) ) ;
#43969 = CARTESIAN_POINT ( 'NONE',  ( 4.549368137175248350, 0.000000000000000000, 0.000000000000000000 ) ) ;
#43970 = LINE ( 'NONE', #19837, #16590 ) ;
#43971 = ORIENTED_EDGE ( 'NONE', *, *, #45876, .F. ) ;
#43972 = CARTESIAN_POINT ( 'NONE',  ( 1.000110580585050979, -34.17542785014344275, -24.25814531310138733 ) ) ;
#43973 = EDGE_CURVE ( 'NONE', #28832, #14276, #10957, .T. ) ;
#43974 =( BOUNDED_SURFACE ( )  B_SPLINE_SURFACE ( 3, 1, ( 
 ( #42396, #14196 ),
 ( #13265, #18573 ),
 ( #32995, #32677 ),
 ( #51759, #9161 ) ),
 .UNSPECIFIED., .F., .F., .F. ) 
 B_SPLINE_SURFACE_WITH_KNOTS ( ( 4, 4 ),
 ( 2, 2 ),
 ( 0.000000000000000000, 1.000000000000000000 ),
 ( 0.000000000000000000, 1.000000000000000000 ),
 .UNSPECIFIED. ) 
 GEOMETRIC_REPRESENTATION_ITEM ( )  RATIONAL_B_SPLINE_SURFACE ( (
 ( 1.000000000000000000, 1.000000000000000000),
 ( 0.7223157951917476005, 0.9931996967497186413),
 ( 0.7223157951917476005, 0.9931996967497186413),
 ( 1.000000000000000000, 1.000000000000000000) ) ) 
 REPRESENTATION_ITEM ( '' )  SURFACE ( )  );
#43975 = FACE_OUTER_BOUND ( 'NONE', #2375, .T. ) ;
#43976 = ORIENTED_EDGE ( 'NONE', *, *, #6565, .F. ) ;
#43977 = ORIENTED_EDGE ( 'NONE', *, *, #43234, .T. ) ;
#43978 = LINE ( 'NONE', #58014, #3542 ) ;
#43979 = B_SPLINE_CURVE_WITH_KNOTS ( 'NONE', 3,
 ( #39905, #31095, #50196, #40838 ),
 .UNSPECIFIED., .F., .F.,
 ( 4, 4 ),
 ( 0.000000000000000000, 0.005004741218457413668 ),
 .UNSPECIFIED. ) ;
#43980 = VECTOR ( 'NONE', #8505, 1000.000000000000114 ) ;
#43981 = LINE ( 'NONE', #29218, #26508 ) ;
#43982 = FACE_OUTER_BOUND ( 'NONE', #9634, .T. ) ;
#43983 = DIRECTION ( 'NONE',  ( -1.836909530733573776E-16, 1.000000000000000000, 0.000000000000000000 ) ) ;
#43984 = ADVANCED_FACE ( 'NONE', ( #47984 ), #30937, .F. ) ;
#43985 = VERTEX_POINT ( 'NONE', #15709 ) ;
#43986 = CARTESIAN_POINT ( 'NONE',  ( 0.1145239942831223490, -1.087792730805732466, -44.11079445758689843 ) ) ;
#43987 = FACE_OUTER_BOUND ( 'NONE', #6292, .T. ) ;
#43988 = EDGE_CURVE ( 'NONE', #55501, #45566, #10112, .T. ) ;
#43989 = CARTESIAN_POINT ( 'NONE',  ( -90.00000000000000000, 0.000000000000000000, 0.000000000000000000 ) ) ;
#43990 = DIRECTION ( 'NONE',  ( 0.000000000000000000, 0.000000000000000000, 1.000000000000000000 ) ) ;
#43991 = EDGE_LOOP ( 'NONE', ( #23211, #37670, #59690, #28890 ) ) ;
#43992 = CARTESIAN_POINT ( 'NONE',  ( 4.553261556744875094, -43.07273893850278768, -8.618510669438375515 ) ) ;
#43993 = CARTESIAN_POINT ( 'NONE',  ( 0.8560838555295158248, 45.47430759461114747, -11.50913475776619599 ) ) ;
#43994 = FACE_OUTER_BOUND ( 'NONE', #12794, .T. ) ;
#43995 = CARTESIAN_POINT ( 'NONE',  ( 1.157644175074338699, 33.40146148540439697, -25.32478323931382391 ) ) ;
#43996 = AXIS2_PLACEMENT_3D ( 'NONE', #57810, #52819, #57187 ) ;
#43997 = ORIENTED_EDGE ( 'NONE', *, *, #1458, .F. ) ;
#43998 = ORIENTED_EDGE ( 'NONE', *, *, #39512, .T. ) ;
#43999 = DIRECTION ( 'NONE',  ( -1.000000000000000000, -0.000000000000000000, -0.000000000000000000 ) ) ;
#44000 = CARTESIAN_POINT ( 'NONE',  ( 0.8557997880470606944, -13.27832040216671317, 46.03118133706021808 ) ) ;
#44001 = CARTESIAN_POINT ( 'NONE',  ( 0.9784957157296370056, 14.84483425312139282, -39.19137600276013700 ) ) ;
#44002 = LINE ( 'NONE', #39914, #36818 ) ;
#44003 = B_SPLINE_CURVE_WITH_KNOTS ( 'NONE', 3,
 ( #32256, #8419, #50422, #13456, #22848, #7810, #41066, #32568, #27543, #51645, #26308, #2490, #21614, #40753, #60125, #17231, #36354, #55414, #12540 ),
 .UNSPECIFIED., .F., .F.,
 ( 4, 3, 3, 3, 3, 3, 4 ),
 ( 1.734723475976807094E-18, 0.0002724573126191750507, 0.0004086839781548473388, 0.0005449106435901799684, 0.0006811373090491421338, 0.0008459866663933654713, 0.001010840725717215968 ),
 .UNSPECIFIED. ) ;
#44004 = CARTESIAN_POINT ( 'NONE',  ( 0.8557997880470690211, -29.88293891557446003, -37.44587306708127983 ) ) ;
#44005 = CARTESIAN_POINT ( 'NONE',  ( 4.967162193818130511, 35.57684288742009215, -24.30453456948074376 ) ) ;
#44006 = CARTESIAN_POINT ( 'NONE',  ( 0.9769922540276050338, 10.14454102355774801, -40.66226558502955868 ) ) ;
#44007 = CARTESIAN_POINT ( 'NONE',  ( 0.6039202388192953519, 44.31978288059509907, 21.14995409607076837 ) ) ;
#44008 = CARTESIAN_POINT ( 'NONE',  ( 5.959547316686252039, 16.28624005235099403, -12.49238070347959351 ) ) ;
#44009 = CARTESIAN_POINT ( 'NONE',  ( 0.1081432562775997280, 30.79166192943845104, -30.19275717928091396 ) ) ;
#44010 = DIRECTION ( 'NONE',  ( -1.000000000000000000, -0.000000000000000000, -0.000000000000000000 ) ) ;
#44011 = ORIENTED_EDGE ( 'NONE', *, *, #32914, .F. ) ;
#44012 = CARTESIAN_POINT ( 'NONE',  ( 0.5809828226811617480, -28.72298383114462439, -38.32755012159175578 ) ) ;
#44013 = CARTESIAN_POINT ( 'NONE',  ( 4.956445790444035104, 38.51510088324747016, -27.09474218539284252 ) ) ;
#44014 = EDGE_CURVE ( 'NONE', #16034, #37474, #12351, .T. ) ;
#44015 = CARTESIAN_POINT ( 'NONE',  ( 0.1147471544378677044, -35.17521250930997212, 26.63938087490264195 ) ) ;
#44016 = CARTESIAN_POINT ( 'NONE',  ( -6.016489644550736315, -14.94663725562923773, 11.47450955518482374 ) ) ;
#44017 = B_SPLINE_CURVE_WITH_KNOTS ( 'NONE', 3,
 ( #51999, #17897, #18821, #8458 ),
 .UNSPECIFIED., .F., .F.,
 ( 4, 4 ),
 ( 0.000000000000000000, 0.005004948556313804434 ),
 .UNSPECIFIED. ) ;
#44018 = CARTESIAN_POINT ( 'NONE',  ( 4.956445790444029775, 29.98832127573299289, -36.30755619981957949 ) ) ;
#44019 = CARTESIAN_POINT ( 'NONE',  ( 0.6028777368367060907, 33.07937202223710216, -36.29455848919381111 ) ) ;
#44020 = FACE_OUTER_BOUND ( 'NONE', #37192, .T. ) ;
#44022 = ADVANCED_FACE ( 'NONE', ( #25394 ), #57966, .F. ) ;
#44021 = CARTESIAN_POINT ( 'NONE',  ( 0.9758171775293917882, -26.11633498242650830, 34.04519363167623425 ) ) ;
#44023 = CARTESIAN_POINT ( 'NONE',  ( 5.960721111146673579, -16.28787783074218964, -12.49016043756465422 ) ) ;
#44024 = ADVANCED_FACE ( 'NONE', ( #57341 ), #44153, .F. ) ;
#44025 = DIRECTION ( 'NONE',  ( 0.07906939808003035641, -0.9868658484044052770, -0.1408681210931520544 ) ) ;
#44026 = EDGE_CURVE ( 'NONE', #28153, #44393, #12247, .T. ) ;
#44028 = ORIENTED_EDGE ( 'NONE', *, *, #33951, .T. ) ;
#44027 = CARTESIAN_POINT ( 'NONE',  ( 0.7056555295713302645, 41.05687446835474930, -24.67549844185496966 ) ) ;
#44029 = VERTEX_POINT ( 'NONE', #16626 ) ;
#44030 = VECTOR ( 'NONE', #39722, 1000.000000000000000 ) ;
#44031 = DIRECTION ( 'NONE',  ( -0.07500201931887526263, 0.9863955245047982823, -0.1462824881350971995 ) ) ;
#44032 = CARTESIAN_POINT ( 'NONE',  ( 0.2285344041767096157, -43.84762605143654213, -4.887418536286803672 ) ) ;
#44033 = ADVANCED_FACE ( 'NONE', ( #45158 ), #9706, .F. ) ;
#44034 = CARTESIAN_POINT ( 'NONE',  ( 3.783278058412227640, 40.39104487792942422, 14.86148287637747956 ) ) ;
#44035 = ORIENTED_EDGE ( 'NONE', *, *, #4761, .F. ) ;
#44036 = DIRECTION ( 'NONE',  ( 0.000000000000000000, 0.000000000000000000, -1.000000000000000000 ) ) ;
#44037 = CARTESIAN_POINT ( 'NONE',  ( 0.8753041380234524160, 10.05717963662871561, -48.06237057854679051 ) ) ;
#44038 = CARTESIAN_POINT ( 'NONE',  ( 5.965394784446458765, 7.868087674480683802, 18.95742317323948001 ) ) ;
#44039 =( BOUNDED_SURFACE ( )  B_SPLINE_SURFACE ( 3, 1, ( 
 ( #1546, #53551 ),
 ( #58245, #20683 ),
 ( #5614, #29758 ),
 ( #6229, #24759 ) ),
 .UNSPECIFIED., .F., .F., .F. ) 
 B_SPLINE_SURFACE_WITH_KNOTS ( ( 4, 4 ),
 ( 2, 2 ),
 ( 0.000000000000000000, 1.000000000000000000 ),
 ( 0.000000000000000000, 1.000000000000000000 ),
 .UNSPECIFIED. ) 
 GEOMETRIC_REPRESENTATION_ITEM ( )  RATIONAL_B_SPLINE_SURFACE ( (
 ( 1.000000000000000000, 1.000000000000000000),
 ( 0.9754377213608244057, 0.9999580625633939235),
 ( 0.9754377213608244057, 0.9999580625633939235),
 ( 1.000000000000000000, 1.000000000000000000) ) ) 
 REPRESENTATION_ITEM ( '' )  SURFACE ( )  );
#44040 = VERTEX_POINT ( 'NONE', #30393 ) ;
#44041 = ORIENTED_EDGE ( 'NONE', *, *, #12060, .F. ) ;
#44042 = EDGE_CURVE ( 'NONE', #38817, #3786, #1886, .T. ) ;
#44043 = CARTESIAN_POINT ( 'NONE',  ( 0.6031356755773454870, -24.05374386753687688, -41.66225520948395911 ) ) ;
#44044 = CARTESIAN_POINT ( 'NONE',  ( 4.967162193818131399, -42.34252806656588319, -7.970725651240238463 ) ) ;
#44045 = CIRCLE ( 'NONE', #12995, 2.649999999999985700 ) ;
#44046 = CARTESIAN_POINT ( 'NONE',  ( 0.5786265663353196143, 29.72999788434346868, -37.55861529268522503 ) ) ;
#44047 = DIRECTION ( 'NONE',  ( -1.000000000000000000, -0.000000000000000000, -0.000000000000000000 ) ) ;
#44048 = CARTESIAN_POINT ( 'NONE',  ( 2.009741617377216460, -11.21041860717905791, 42.58909006159744592 ) ) ;
#44049 = CARTESIAN_POINT ( 'NONE',  ( 0.8751705887134423323, -41.19904111682490822, -24.81530984069193480 ) ) ;
#44050 = B_SPLINE_CURVE_WITH_KNOTS ( 'NONE', 3,
 ( #35979, #2104, #40374, #49426, #39760, #15933 ),
 .UNSPECIFIED., .F., .F.,
 ( 4, 2, 4 ),
 ( 8.949102196395036105E-18, 0.0002291978881530155638, 0.0004583957763060221829 ),
 .UNSPECIFIED. ) ;
#44051 = DIRECTION ( 'NONE',  ( 0.000000000000000000, 1.000000000000000000, 0.000000000000000000 ) ) ;
#44052 =( BOUNDED_SURFACE ( )  B_SPLINE_SURFACE ( 3, 1, ( 
 ( #48893, #49198 ),
 ( #6247, #59202 ),
 ( #44229, #20394 ),
 ( #10686, #44536 ) ),
 .UNSPECIFIED., .F., .F., .F. ) 
 B_SPLINE_SURFACE_WITH_KNOTS ( ( 4, 4 ),
 ( 2, 2 ),
 ( 0.000000000000000000, 1.000000000000000000 ),
 ( 0.000000000000000000, 1.000000000000000000 ),
 .UNSPECIFIED. ) 
 GEOMETRIC_REPRESENTATION_ITEM ( )  RATIONAL_B_SPLINE_SURFACE ( (
 ( 1.000000000000000000, 1.000000000000000000),
 ( 0.9953485035131437453, 0.8621029689291515030),
 ( 0.9953485035131437453, 0.8621029689291515030),
 ( 1.000000000000000000, 1.000000000000000000) ) ) 
 REPRESENTATION_ITEM ( '' )  SURFACE ( )  );
#44053 = CARTESIAN_POINT ( 'NONE',  ( 0.9740398440564312921, 42.59352035928887403, 5.189371650077005960 ) ) ;
#44054 = EDGE_LOOP ( 'NONE', ( #19092, #21697, #59420, #56261 ) ) ;
#44055 = B_SPLINE_CURVE_WITH_KNOTS ( 'NONE', 3,
 ( #42770, #61826, #27409, #38083, #18963, #41852 ),
 .UNSPECIFIED., .F., .F.,
 ( 4, 2, 4 ),
 ( 9.543442895606953578E-18, 0.0002291978881530146693, 0.0004583957763060197976 ),
 .UNSPECIFIED. ) ;
#44056 = ORIENTED_EDGE ( 'NONE', *, *, #50491, .T. ) ;
#44057 = CARTESIAN_POINT ( 'NONE',  ( 0.1129192098497447394, 33.91039995638862337, 28.23183597612653983 ) ) ;
#44058 = CARTESIAN_POINT ( 'NONE',  ( 0.9722240741986376555, -0.5819399500323430008, 42.90442369863401950 ) ) ;
#44059 = ORIENTED_EDGE ( 'NONE', *, *, #27073, .T. ) ;
#44060 = CARTESIAN_POINT ( 'NONE',  ( -6.001507490154110336, -13.31361390284169133, 13.33564355450103633 ) ) ;
#44061 = CARTESIAN_POINT ( 'NONE',  ( 5.895596859100789899, 0.6684898708301673098, 20.10177366565161705 ) ) ;
#44062 = CARTESIAN_POINT ( 'NONE',  ( 0.5987334363312691865, -39.71456561150246500, 28.88453192907479306 ) ) ;
#44063 = CARTESIAN_POINT ( 'NONE',  ( 3.238018933889920792, 3.371911215444676646, -12.96293589904738575 ) ) ;
#44064 = ORIENTED_EDGE ( 'NONE', *, *, #3382, .F. ) ;
#44065 = CARTESIAN_POINT ( 'NONE',  ( 5.965394784446458765, 19.82972329408678291, 5.298374383010704847 ) ) ;
#44066 = CARTESIAN_POINT ( 'NONE',  ( 0.9741495583595174423, -42.48790363482600441, -5.992561317325607817 ) ) ;
#44067 = CARTESIAN_POINT ( 'NONE',  ( 3.376099380956838925, -6.056959685666334359, 11.95916481190387870 ) ) ;
#44068 = EDGE_CURVE ( 'NONE', #59959, #988, #42977, .T. ) ;
#44069 = CARTESIAN_POINT ( 'NONE',  ( 0.5827357941260208340, 29.44458568814510713, 37.77622264066022950 ) ) ;
#44070 = ORIENTED_EDGE ( 'NONE', *, *, #37941, .F. ) ;
#44071 = CARTESIAN_POINT ( 'NONE',  ( 0.5807400328401574052, 24.41979442053226634, -41.20655774452943376 ) ) ;
#44072 = ORIENTED_EDGE ( 'NONE', *, *, #3308, .F. ) ;
#44073 = CARTESIAN_POINT ( 'NONE',  ( 4.691466044806102076, -37.25818859570323838, 24.49380602310747790 ) ) ;
#44074 = CARTESIAN_POINT ( 'NONE',  ( 0.5834872094924171693, 24.14431479207748765, -41.36515088387890415 ) ) ;
#44075 = ORIENTED_EDGE ( 'NONE', *, *, #52051, .F. ) ;
#44076 = DIRECTION ( 'NONE',  ( -1.000000000000000000, -1.836909530733573776E-16, 1.925929944387235853E-32 ) ) ;
#44077 = CARTESIAN_POINT ( 'NONE',  ( -5.283180000000052168, 0.000000000000000000, 0.000000000000000000 ) ) ;
#44078 = CARTESIAN_POINT ( 'NONE',  ( 3.376099380956838925, 12.15487954915001900, 5.653962042472672422 ) ) ;
#44079 = CARTESIAN_POINT ( 'NONE',  ( 0.8557997880470697982, -19.17299735371977221, -43.90420959842202109 ) ) ;
#44080 = CARTESIAN_POINT ( 'NONE',  ( 0.9730545539215883499, -6.101350888304360787, -42.47233286818623554 ) ) ;
#44081 = CARTESIAN_POINT ( 'NONE',  ( 0.7762783648524373969, 5.369627767360514170, -47.60264408896659916 ) ) ;
#44082 = VECTOR ( 'NONE', #37479, 1000.000000000000000 ) ;
#44083 = CARTESIAN_POINT ( 'NONE',  ( 0.1313383488274169619, -21.00709374781567362, 37.66088038379808722 ) ) ;
#44084 = CARTESIAN_POINT ( 'NONE',  ( 4.833616638992208614, 20.04871863793809439, -41.67905425467686342 ) ) ;
#44085 = ORIENTED_EDGE ( 'NONE', *, *, #52302, .T. ) ;
#44086 = CARTESIAN_POINT ( 'NONE',  ( 0.5834872094924177244, -24.14431479207719633, 41.36515088387906758 ) ) ;
#44087 = CARTESIAN_POINT ( 'NONE',  ( 0.9790724872846782167, 41.52931421318174188, 5.625946228348769118 ) ) ;
#44088 = CARTESIAN_POINT ( 'NONE',  ( 1.112077966505211846, -16.87764873673971167, 40.72069864636144132 ) ) ;
#44089 = AXIS2_PLACEMENT_3D ( 'NONE', #978, #25405, #34515 ) ;
#44090 = ORIENTED_EDGE ( 'NONE', *, *, #29356, .T. ) ;
#44091 = CARTESIAN_POINT ( 'NONE',  ( 5.959828726073459926, 2.683617577144381983, -20.34941966491236442 ) ) ;
#44092 = CARTESIAN_POINT ( 'NONE',  ( -2.708315649062910779, -13.41752550814506861, -5.842990691604553533 ) ) ;
#44093 = CARTESIAN_POINT ( 'NONE',  ( 4.303969348037246512, -4.133486515472991840, -47.93217632892352498 ) ) ;
#44094 =( REPRESENTATION_RELATIONSHIP ('NONE','NONE', #44881, #53251 ) REPRESENTATION_RELATIONSHIP_WITH_TRANSFORMATION ( #24571 )SHAPE_REPRESENTATION_RELATIONSHIP( ) );
#44095 = CARTESIAN_POINT ( 'NONE',  ( 0.6001305935487315502, 44.64600790884030346, 17.92615948558555772 ) ) ;
#44096 = FACE_OUTER_BOUND ( 'NONE', #34278, .T. ) ;
#44097 = CARTESIAN_POINT ( 'NONE',  ( -1.599999999999965672, 80.00000000000001421, -9.054715201685574691E-15 ) ) ;
#44099 = EDGE_CURVE ( 'NONE', #50629, #35664, #38962, .T. ) ;
#44098 = CARTESIAN_POINT ( 'NONE',  ( 5.896782393890504181, -9.660289833039353624, -17.64100017628503991 ) ) ;
#44100 = CARTESIAN_POINT ( 'NONE',  ( 0.7245667037590769466, 46.66865388241069468, 11.65533952568368647 ) ) ;
#44101 = EDGE_CURVE ( 'NONE', #42435, #16773, #25708, .T. ) ;
#44102 = CARTESIAN_POINT ( 'NONE',  ( 0.9789889208857696090, 29.06536874308044816, -30.19170809793860144 ) ) ;
#44103 = EDGE_CURVE ( 'NONE', #47280, #41171, #9324, .T. ) ;
#44105 = ORIENTED_EDGE ( 'NONE', *, *, #15287, .T. ) ;
#44104 = CARTESIAN_POINT ( 'NONE',  ( 4.956653778116975495, -2.599733001514665798, 48.02038484091099235 ) ) ;
#44106 = EDGE_LOOP ( 'NONE', ( #11591, #31603, #59558, #56879 ) ) ;
#44107 = CARTESIAN_POINT ( 'NONE',  ( 5.960221823109900008, 16.28736530777590730, -12.49086489703211100 ) ) ;
#44108 = DIRECTION ( 'NONE',  ( 0.9848077530122079093, 0.1736481776669314414, -5.551115123125783935E-17 ) ) ;
#44109 = EDGE_CURVE ( 'NONE', #49527, #8500, #54916, .T. ) ;
#44110 = CARTESIAN_POINT ( 'NONE',  ( 5.958863334805807099, -16.28335246510359369, -12.49619391867176610 ) ) ;
#44111 = DIRECTION ( 'NONE',  ( 1.000000000000000000, 1.836909530733573776E-16, 0.000000000000000000 ) ) ;
#44112 = CARTESIAN_POINT ( 'NONE',  ( 5.959547316686252039, -20.34955788964374790, -2.682663672454841386 ) ) ;
#44113 = CARTESIAN_POINT ( 'NONE',  ( 0.6254087463353920073, 11.78492518233810493, -46.64065386173403738 ) ) ;
#44114 = VERTEX_POINT ( 'NONE', #26022 ) ;
#44115 = ORIENTED_EDGE ( 'NONE', *, *, #51133, .T. ) ;
#44116 = DIRECTION ( 'NONE',  ( 0.000000000000000000, 0.000000000000000000, -1.000000000000000000 ) ) ;
#44117 = EDGE_CURVE ( 'NONE', #44894, #19785, #26526, .T. ) ;
#44118 = CARTESIAN_POINT ( 'NONE',  ( 3.238018933889920792, -3.704930136113204320, -12.87171259212126628 ) ) ;
#44119 = CARTESIAN_POINT ( 'NONE',  ( -2.601141883200665639, -13.21958573851854268, 6.930943685483663685 ) ) ;
#44120 = ORIENTED_EDGE ( 'NONE', *, *, #30259, .F. ) ;
#44121 = ADVANCED_FACE ( 'NONE', ( #59206 ), #37358, .F. ) ;
#44122 = B_SPLINE_CURVE_WITH_KNOTS ( 'NONE', 3,
 ( #47645, #28216, #4689, #307, #23835, #24134 ),
 .UNSPECIFIED., .F., .F.,
 ( 4, 2, 4 ),
 ( 1.910758783386232924E-17, 0.0002293755540694306951, 0.0004587511081388422540 ),
 .UNSPECIFIED. ) ;
#44123 = CARTESIAN_POINT ( 'NONE',  ( 0.1103872315293168843, -0.02583155086994256763, 43.12442619660166088 ) ) ;
#44124 = CARTESIAN_POINT ( 'NONE',  ( 0.5837800005270555870, -25.23393936835100959, -39.52826283301821775 ) ) ;
#44125 = ORIENTED_EDGE ( 'NONE', *, *, #53041, .T. ) ;
#44126 = VECTOR ( 'NONE', #11347, 1000.000000000000000 ) ;
#44127 = CARTESIAN_POINT ( 'NONE',  ( 4.553261556744875094, 0.000000000000000000, 0.000000000000000000 ) ) ;
#44128 = EDGE_LOOP ( 'NONE', ( #20328, #12613, #13771 ) ) ;
#44129 =( BOUNDED_SURFACE ( )  B_SPLINE_SURFACE ( 3, 1, ( 
 ( #61835, #41861 ),
 ( #56841, #42780 ),
 ( #8610, #33075 ),
 ( #51215, #8298 ) ),
 .UNSPECIFIED., .F., .F., .F. ) 
 B_SPLINE_SURFACE_WITH_KNOTS ( ( 4, 4 ),
 ( 2, 2 ),
 ( 0.000000000000000000, 1.000000000000000000 ),
 ( 0.000000000000000000, 1.000000000000000000 ),
 .UNSPECIFIED. ) 
 GEOMETRIC_REPRESENTATION_ITEM ( )  RATIONAL_B_SPLINE_SURFACE ( (
 ( 1.000000000000000000, 1.000000000000000000),
 ( 0.9729067724841187204, 0.9999501103223794596),
 ( 0.9729067724841187204, 0.9999501103223794596),
 ( 1.000000000000000000, 1.000000000000000000) ) ) 
 REPRESENTATION_ITEM ( '' )  SURFACE ( )  );
#44130 = CARTESIAN_POINT ( 'NONE',  ( 0.5837800005270556980, -34.78049932281108170, 31.45714744692725517 ) ) ;
#44131 = CARTESIAN_POINT ( 'NONE',  ( 0.6025881611877910160, 33.86250327239848446, 34.17105830828427315 ) ) ;
#44132 = ORIENTED_EDGE ( 'NONE', *, *, #35890, .T. ) ;
#44133 = CARTESIAN_POINT ( 'NONE',  ( 4.962356264823608143, -40.47344704301786322, -11.53844366967987334 ) ) ;
#44134 = CARTESIAN_POINT ( 'NONE',  ( 2.282816707992306071, 43.74200569621534385, 17.12115370178745266 ) ) ;
#44135 = CARTESIAN_POINT ( 'NONE',  ( 0.9785694773339252972, 40.36023435788206370, 11.28658000864342092 ) ) ;
#44136 = CARTESIAN_POINT ( 'NONE',  ( -90.00000000000000000, 0.000000000000000000, 0.000000000000000000 ) ) ;
#44137 = ORIENTED_EDGE ( 'NONE', *, *, #13892, .T. ) ;
#44138 = CARTESIAN_POINT ( 'NONE',  ( 4.291220156522060236, -37.58001468972601344, 28.41005971879809167 ) ) ;
#44139 = CARTESIAN_POINT ( 'NONE',  ( 0.5549461598389365813, -0.5360408303695749499, 44.10136455592935079 ) ) ;
#44140 = ORIENTED_EDGE ( 'NONE', *, *, #52398, .F. ) ;
#44141 = CARTESIAN_POINT ( 'NONE',  ( 0.5997462898726536595, 5.235280152387000285, 48.82769165002921596 ) ) ;
#44142 = EDGE_CURVE ( 'NONE', #24192, #15612, #21942, .T. ) ;
#44143 = ORIENTED_EDGE ( 'NONE', *, *, #7150, .F. ) ;
#44144 = CARTESIAN_POINT ( 'NONE',  ( -6.063463321072278589, 18.62294427965537835, 4.899632520538766300 ) ) ;
#44145 = VERTEX_POINT ( 'NONE', #39845 ) ;
#44146 = LINE ( 'NONE', #15919, #48636 ) ;
#44147 = CARTESIAN_POINT ( 'NONE',  ( 0.6016118706126976079, -48.65860383458689853, -6.625053030176840885 ) ) ;
#44148 =( BOUNDED_SURFACE ( )  B_SPLINE_SURFACE ( 3, 1, ( 
 ( #35107, #44518 ),
 ( #53860, #45134 ),
 ( #24764, #10988 ),
 ( #39504, #35415 ) ),
 .UNSPECIFIED., .F., .F., .F. ) 
 B_SPLINE_SURFACE_WITH_KNOTS ( ( 4, 4 ),
 ( 2, 2 ),
 ( 0.000000000000000000, 1.000000000000000000 ),
 ( 0.000000000000000000, 1.000000000000000000 ),
 .UNSPECIFIED. ) 
 GEOMETRIC_REPRESENTATION_ITEM ( )  RATIONAL_B_SPLINE_SURFACE ( (
 ( 1.000000000000000000, 1.000000000000000000),
 ( 0.9952954269826590483, 0.8620686068821307169),
 ( 0.9952954269826590483, 0.8620686068821307169),
 ( 1.000000000000000000, 1.000000000000000000) ) ) 
 REPRESENTATION_ITEM ( '' )  SURFACE ( )  );
#44149 = CARTESIAN_POINT ( 'NONE',  ( -6.078726893082806448, 16.77980020642702641, 9.446287434813308792 ) ) ;
#44150 = ORIENTED_EDGE ( 'NONE', *, *, #19491, .F. ) ;
#44151 = CARTESIAN_POINT ( 'NONE',  ( 0.5837374860065653870, 6.431731162805769841, 47.46223477511612288 ) ) ;
#44152 = LINE ( 'NONE', #1179, #4739 ) ;
#44153 =( BOUNDED_SURFACE ( )  B_SPLINE_SURFACE ( 3, 1, ( 
 ( #14473, #5034 ),
 ( #24159, #332 ),
 ( #55431, #7825 ),
 ( #30709, #59515 ) ),
 .UNSPECIFIED., .F., .F., .F. ) 
 B_SPLINE_SURFACE_WITH_KNOTS ( ( 4, 4 ),
 ( 2, 2 ),
 ( 0.000000000000000000, 1.000000000000000000 ),
 ( 0.000000000000000000, 1.000000000000000000 ),
 .UNSPECIFIED. ) 
 GEOMETRIC_REPRESENTATION_ITEM ( )  RATIONAL_B_SPLINE_SURFACE ( (
 ( 1.000000000000000000, 1.000000000000000000),
 ( 0.9953040768229013402, 0.8617119497784988535),
 ( 0.9953040768229013402, 0.8617119497784988535),
 ( 1.000000000000000000, 1.000000000000000000) ) ) 
 REPRESENTATION_ITEM ( '' )  SURFACE ( )  );
#44154 = B_SPLINE_CURVE_WITH_KNOTS ( 'NONE', 3,
 ( #13367, #60957, #4543, #37817, #23679, #14299 ),
 .UNSPECIFIED., .F., .F.,
 ( 4, 2, 4 ),
 ( 1.274743298368305687E-16, 0.0002450741128632359200, 0.0004901482257263444463 ),
 .UNSPECIFIED. ) ;
#44155 = CARTESIAN_POINT ( 'NONE',  ( 5.894904586330512508, -7.229884331608547043, -18.76854242111528137 ) ) ;
#44156 = VERTEX_POINT ( 'NONE', #58900 ) ;
#44157 = VERTEX_POINT ( 'NONE', #16017 ) ;
#44158 = CARTESIAN_POINT ( 'NONE',  ( 3.660087539127326206, -25.63019641081301003, -40.62968541507471087 ) ) ;
#44159 = CARTESIAN_POINT ( 'NONE',  ( 4.967162193818130511, 13.42934394584221280, -40.93989340068594629 ) ) ;
#44160 = CARTESIAN_POINT ( 'NONE',  ( 0.2279481005628741785, 24.61482262596651438, 36.61439599618051943 ) ) ;
#44161 = CARTESIAN_POINT ( 'NONE',  ( -2.739355103387247858, -14.50431811309224095, 3.531617621606463864 ) ) ;
#44162 = CARTESIAN_POINT ( 'NONE',  ( 0.9787284016396606834, -27.20011616372034524, -31.88243528353739720 ) ) ;
#44163 = CARTESIAN_POINT ( 'NONE',  ( 0.9791128995231600518, 38.58521266320476428, 16.35600189476109634 ) ) ;
#44164 = ORIENTED_EDGE ( 'NONE', *, *, #21708, .F. ) ;
#44165 = CARTESIAN_POINT ( 'NONE',  ( 5.896278296736517710, -11.92612757635554033, -16.19550742171654534 ) ) ;
#44166 = ORIENTED_EDGE ( 'NONE', *, *, #43939, .F. ) ;
#44167 = CARTESIAN_POINT ( 'NONE',  ( 0.6027935024548037868, 12.28245664247781477, 46.51312430684509991 ) ) ;
#44168 = CARTESIAN_POINT ( 'NONE',  ( 0.1129192098497447394, 24.84520063729181416, -36.46461014569973713 ) ) ;
#44169 = CARTESIAN_POINT ( 'NONE',  ( 0.1152339509894530906, -42.62387090632541486, 11.40825663351544073 ) ) ;
#44170 = CARTESIAN_POINT ( 'NONE',  ( 4.691466044806103852, -20.01963481131631539, -39.84135254923129565 ) ) ;
#44171 = CARTESIAN_POINT ( 'NONE',  ( 0.8751705887134553219, 44.08562551107081617, -19.22545746485614870 ) ) ;
#44172 = SURFACE_STYLE_USAGE ( .BOTH. , #49752 ) ;
#44173 = AXIS2_PLACEMENT_3D ( 'NONE', #44616, #45242, #45539 ) ;
#44174 = CARTESIAN_POINT ( 'NONE',  ( 0.6029443449137436017, 37.42085009926554307, -31.79967792024990914 ) ) ;
#44175 = CARTESIAN_POINT ( 'NONE',  ( -6.057079549204054558, -11.02420820863765449, -15.78917554758146835 ) ) ;
#44176 = ADVANCED_FACE ( 'NONE', ( #54187 ), #29949, .T. ) ;
#44177 = CARTESIAN_POINT ( 'NONE',  ( 5.895881250540457863, 17.95317081027908657, -9.067046898811309319 ) ) ;
#44178 = CARTESIAN_POINT ( 'NONE',  ( 0.2940135542859016460, -2.218054204175251787, -44.06042197072970623 ) ) ;
#44179 = CARTESIAN_POINT ( 'NONE',  ( 4.553261556744875094, 0.000000000000000000, 0.000000000000000000 ) ) ;
#44180 = EDGE_CURVE ( 'NONE', #40399, #6110, #33320, .T. ) ;
#44181 = CARTESIAN_POINT ( 'NONE',  ( 3.390910168358336918, -19.58529142663901013, -39.37656023914808401 ) ) ;
#44182 = CARTESIAN_POINT ( 'NONE',  ( 0.6001305935487315502, 47.76436356026967900, -5.760103278697520146 ) ) ;
#44183 = DIRECTION ( 'NONE',  ( -0.1011922191286467460, 0.01903003979491558334, 0.9946848708878726075 ) ) ;
#44184 = ORIENTED_EDGE ( 'NONE', *, *, #50336, .F. ) ;
#44185 = CARTESIAN_POINT ( 'NONE',  ( 0.3676999524040323597, -41.19158123804999860, 15.78620342045440239 ) ) ;
#44186 = CARTESIAN_POINT ( 'NONE',  ( 4.549368137175248350, 3.018832571115968033, 42.82045902618773425 ) ) ;
#44187 = CARTESIAN_POINT ( 'NONE',  ( 0.5836750258453353712, 18.49664649301250563, -44.18029554260614589 ) ) ;
#44188 = CARTESIAN_POINT ( 'NONE',  ( 4.291220156522060236, -32.02897670715545075, -34.54755633034253748 ) ) ;
#44189 = CARTESIAN_POINT ( 'NONE',  ( 4.960156602257181468, 41.40608197274663382, -20.99019478193005739 ) ) ;
#44190 = ORIENTED_EDGE ( 'NONE', *, *, #25759, .T. ) ;
#44191 = EDGE_CURVE ( 'NONE', #55165, #8492, #32581, .T. ) ;
#44192 = CARTESIAN_POINT ( 'NONE',  ( 0.9745511491811744698, -37.32887948083614305, 21.15859207114736407 ) ) ;
#44193 = CARTESIAN_POINT ( 'NONE',  ( 5.960721111146673579, 10.26825948882901152, 17.77250458025995528 ) ) ;
#44194 = CARTESIAN_POINT ( 'NONE',  ( 1.231276596079881047, 38.25526645152027072, 17.14092645516147684 ) ) ;
#44195 = ORIENTED_EDGE ( 'NONE', *, *, #46529, .T. ) ;
#44196 = PLANE ( 'NONE',  #54033 ) ;
#44197 = DIRECTION ( 'NONE',  ( 1.000000000000000000, 0.000000000000000000, 0.000000000000000000 ) ) ;
#44198 = ORIENTED_EDGE ( 'NONE', *, *, #14387, .T. ) ;
#44199 = LINE ( 'NONE', #15675, #51847 ) ;
#44200 = VERTEX_POINT ( 'NONE', #27869 ) ;
#44201 = CARTESIAN_POINT ( 'NONE',  ( 0.6000166863083106206, -35.63988196839385125, 33.78790160674984833 ) ) ;
#44202 = ORIENTED_EDGE ( 'NONE', *, *, #30280, .T. ) ;
#44203 = CARTESIAN_POINT ( 'NONE',  ( 4.553261556744875094, 43.53643125131386427, 5.841123155974254466 ) ) ;
#44204 = CARTESIAN_POINT ( 'NONE',  ( 4.833616638992205949, 30.15290813935854430, 35.06988470649578460 ) ) ;
#44205 = ORIENTED_EDGE ( 'NONE', *, *, #43531, .F. ) ;
#44206 = CARTESIAN_POINT ( 'NONE',  ( 4.960156602257182357, -20.99019478193021371, -41.40608197274659119 ) ) ;
#44207 = AXIS2_PLACEMENT_3D ( 'NONE', #35770, #12886, #2529 ) ;
#44208 = ORIENTED_EDGE ( 'NONE', *, *, #58152, .T. ) ;
#44209 = CARTESIAN_POINT ( 'NONE',  ( 0.9791128995231609400, 20.13607257681962892, -36.75426526849933850 ) ) ;
#44210 = CONICAL_SURFACE ( 'NONE', #60167, 43.92652462719577500, 1.486293639869522343 ) ;
#44211 = EDGE_CURVE ( 'NONE', #49641, #15442, #7886, .T. ) ;
#44212 = VERTEX_POINT ( 'NONE', #51349 ) ;
#44213 = CARTESIAN_POINT ( 'NONE',  ( 4.967162193818129623, -38.44485641567058565, -19.45289607368863116 ) ) ;
#44214 = CARTESIAN_POINT ( 'NONE',  ( 2.879087469061463178, -36.27144865066016877, -24.90951002259781433 ) ) ;
#44215 = CARTESIAN_POINT ( 'NONE',  ( 0.6025881611877910160, 23.86454577211506844, 41.77096849334458284 ) ) ;
#44216 = CARTESIAN_POINT ( 'NONE',  ( -6.077587904424778920, 17.85108912406252912, -7.220432014686311462 ) ) ;
#44217 = EDGE_LOOP ( 'NONE', ( #57138, #2845, #37341 ) ) ;
#44218 = CARTESIAN_POINT ( 'NONE',  ( 0.6041374136657476912, -46.51335992032610278, -12.28249295042029132 ) ) ;
#44219 = CARTESIAN_POINT ( 'NONE',  ( 0.9972139404380300221, -10.46878911444705018, 41.61281131482459728 ) ) ;
#44220 = ORIENTED_EDGE ( 'NONE', *, *, #21576, .F. ) ;
#44221 = CARTESIAN_POINT ( 'NONE',  ( 4.956445790444004018, -46.73954499432468879, 5.740468958468036398 ) ) ;
#44222 =( BOUNDED_SURFACE ( )  B_SPLINE_SURFACE ( 3, 1, ( 
 ( #54479, #6868 ),
 ( #16614, #7491 ),
 ( #50424, #11938 ),
 ( #31014, #50123 ) ),
 .UNSPECIFIED., .F., .F., .F. ) 
 B_SPLINE_SURFACE_WITH_KNOTS ( ( 4, 4 ),
 ( 2, 2 ),
 ( 0.000000000000000000, 1.000000000000000000 ),
 ( 0.000000000000000000, 1.000000000000000000 ),
 .UNSPECIFIED. ) 
 GEOMETRIC_REPRESENTATION_ITEM ( )  RATIONAL_B_SPLINE_SURFACE ( (
 ( 1.000000000000000000, 1.000000000000000000),
 ( 0.7211978278499968642, 0.9934217856018975334),
 ( 0.7211978278499968642, 0.9934217856018975334),
 ( 1.000000000000000000, 1.000000000000000000) ) ) 
 REPRESENTATION_ITEM ( '' )  SURFACE ( )  );
#44223 = B_SPLINE_CURVE_WITH_KNOTS ( 'NONE', 3,
 ( #17119, #2995, #6433, #45331, #35926, #16814, #54366, #55300, #2059, #35003, #12123, #31201, #49688, #50605, #30889, #21190, #41245, #11488, #12421 ),
 .UNSPECIFIED., .F., .F.,
 ( 4, 3, 3, 3, 3, 3, 4 ),
 ( 1.161276725443423652E-16, 0.0002618519381806254831, 0.0003927759815485982521, 0.0005237000248299445142, 0.0006546240681324981504, 0.0007855481115631305408, 0.0009699050456655098577 ),
 .UNSPECIFIED. ) ;
#44224 = ORIENTED_EDGE ( 'NONE', *, *, #45416, .T. ) ;
#44225 = CARTESIAN_POINT ( 'NONE',  ( 3.680882792899937250, -8.091276083385070095, -47.28852514876952995 ) ) ;
#44226 = CARTESIAN_POINT ( 'NONE',  ( 4.956653778116973719, 31.29546495791849736, 36.51451553856430365 ) ) ;
#44227 = EDGE_LOOP ( 'NONE', ( #26169, #30452, #16741, #40430 ) ) ;
#44228 = CARTESIAN_POINT ( 'NONE',  ( 0.9787284016396597952, -12.59522306292760163, -39.97119406427494681 ) ) ;
#44229 = CARTESIAN_POINT ( 'NONE',  ( -6.078457390727109555, 5.474669697363819587, 18.46137867934771393 ) ) ;
#44230 = CARTESIAN_POINT ( 'NONE',  ( 51.35512545846777499, 12.24472452707400549, 2.514220983385977881 ) ) ;
#44231 = CARTESIAN_POINT ( 'NONE',  ( 2.648799415243708655, -38.45353011080888450, 30.42767630475112028 ) ) ;
#44232 = EDGE_LOOP ( 'NONE', ( #5288, #15056, #21905, #24919 ) ) ;
#44233 = CARTESIAN_POINT ( 'NONE',  ( 0.6030672727741701600, 18.49051564326133601, -44.41203814406388517 ) ) ;
#44234 = DIRECTION ( 'NONE',  ( 0.1736481776669316079, -0.9848077530122079093, -5.551115123125822145E-17 ) ) ;
#44235 = B_SPLINE_CURVE_WITH_KNOTS ( 'NONE', 3,
 ( #32696, #12430, #56778, #43032 ),
 .UNSPECIFIED., .F., .F.,
 ( 4, 4 ),
 ( 0.000000000000000000, 0.005004948556313791423 ),
 .UNSPECIFIED. ) ;
#44236 = CARTESIAN_POINT ( 'NONE',  ( 0.5819845079324663661, -44.07435181061349994, 18.74766465427208217 ) ) ;
#44237 = CARTESIAN_POINT ( 'NONE',  ( 0.5809828226811617480, 46.11980934799338883, 12.92184523170220345 ) ) ;
#44238 = CARTESIAN_POINT ( 'NONE',  ( 4.975610109902397937, 0.000000000000000000, 0.000000000000000000 ) ) ;
#44239 = EDGE_CURVE ( 'NONE', #4479, #44253, #57130, .T. ) ;
#44240 = DIRECTION ( 'NONE',  ( -1.000000000000000000, -0.000000000000000000, -0.000000000000000000 ) ) ;
#44241 = CARTESIAN_POINT ( 'NONE',  ( -17.04037160131633399, -7.774647616731808597, 1.886217860945154534 ) ) ;
#44242 = EDGE_CURVE ( 'NONE', #54938, #39717, #41375, .T. ) ;
#44243 = CARTESIAN_POINT ( 'NONE',  ( 3.680974057930772592, -16.63696281867829185, -44.99871514631785629 ) ) ;
#44244 = CARTESIAN_POINT ( 'NONE',  ( 4.962356264823608143, 0.000000000000000000, 0.000000000000000000 ) ) ;
#44245 = CARTESIAN_POINT ( 'NONE',  ( 0.1149546198390368756, -43.72609045126175431, -5.914015460860355233 ) ) ;
#44246 = DIRECTION ( 'NONE',  ( 1.000000000000000000, -0.000000000000000000, -0.000000000000000000 ) ) ;
#44247 = CIRCLE ( 'NONE', #10238, 43.92652462719577500 ) ;
#44248 = CARTESIAN_POINT ( 'NONE',  ( 4.553261556744873317, 17.57396821678933563, -40.25785894628420181 ) ) ;
#44249 = EDGE_CURVE ( 'NONE', #1997, #28601, #24312, .T. ) ;
#44250 = AXIS2_PLACEMENT_3D ( 'NONE', #27822, #3988, #3375 ) ;
#44251 = LINE ( 'NONE', #30110, #11261 ) ;
#44252 = CARTESIAN_POINT ( 'NONE',  ( 0.1156495703730067298, 37.05413706972513666, 23.95691714827038865 ) ) ;
#44253 = VERTEX_POINT ( 'NONE', #3422 ) ;
#44254 = CARTESIAN_POINT ( 'NONE',  ( 4.390527457369401532, -3.899219021785376160, -43.76050077008678585 ) ) ;
#44255 = CARTESIAN_POINT ( 'NONE',  ( 0.9772918015221172539, -0.9856339699200908910, 41.89708082227232211 ) ) ;
#44256 = CARTESIAN_POINT ( 'NONE',  ( 4.967162193818130511, -35.57684288741994294, 24.30453456948097823 ) ) ;
#44257 = VERTEX_POINT ( 'NONE', #17551 ) ;
#44258 = EDGE_CURVE ( 'NONE', #60259, #7019, #31085, .T. ) ;
#44259 = CARTESIAN_POINT ( 'NONE',  ( 0.9747592971366240144, 5.921534893734127003, 42.49794971112893904 ) ) ;
#44260 = DIRECTION ( 'NONE',  ( 0.000000000000000000, 0.000000000000000000, 1.000000000000000000 ) ) ;
#44261 = ORIENTED_EDGE ( 'NONE', *, *, #34378, .F. ) ;
#44262 = ORIENTED_EDGE ( 'NONE', *, *, #51678, .F. ) ;
#44263 = FACE_OUTER_BOUND ( 'NONE', #60889, .T. ) ;
#44264 = ORIENTED_EDGE ( 'NONE', *, *, #31196, .F. ) ;
#44265 = CARTESIAN_POINT ( 'NONE',  ( 0.8744876279028306332, 48.01195819035234535, -10.25679877482985169 ) ) ;
#44266 = ORIENTED_EDGE ( 'NONE', *, *, #31259, .T. ) ;
#44267 = ORIENTED_EDGE ( 'NONE', *, *, #49804, .F. ) ;
#44268 = CARTESIAN_POINT ( 'NONE',  ( 1.114300000000000068, 0.000000000000000000, 0.000000000000000000 ) ) ;
#44269 = VERTEX_POINT ( 'NONE', #49702 ) ;
#44270 = DIRECTION ( 'NONE',  ( 0.000000000000000000, 0.000000000000000000, 1.000000000000000000 ) ) ;
#44271 = B_SPLINE_CURVE_WITH_KNOTS ( 'NONE', 3,
 ( #43558, #28816, #284, #48536 ),
 .UNSPECIFIED., .F., .F.,
 ( 4, 4 ),
 ( 1.058181320345852328E-16, 0.005004948556313925864 ),
 .UNSPECIFIED. ) ;
#44272 = CARTESIAN_POINT ( 'NONE',  ( 0.8744876279028263033, 41.62483489565955352, -26.03311679934954626 ) ) ;
#44273 = ORIENTED_EDGE ( 'NONE', *, *, #4020, .T. ) ;
#44274 = CARTESIAN_POINT ( 'NONE',  ( 0.1365634738349418009, 37.32273229751332622, -23.53457612686919020 ) ) ;
#44275 = LINE ( 'NONE', #15754, #8977 ) ;
#44276 = VERTEX_POINT ( 'NONE', #30906 ) ;
#44277 = EDGE_LOOP ( 'NONE', ( #33350, #28905, #8905, #1880 ) ) ;
#44278 = CARTESIAN_POINT ( 'NONE',  ( 0.5804410086790514622, 23.01644811389207135, 40.86273324284501030 ) ) ;
#44279 = CARTESIAN_POINT ( 'NONE',  ( 47.93443732600252360, 12.48232846285511677, -0.6858480285855463876 ) ) ;
#44280 = CARTESIAN_POINT ( 'NONE',  ( 0.1092565886968784594, -30.27341312544135477, 30.71235995742688374 ) ) ;
#44281 = CARTESIAN_POINT ( 'NONE',  ( 0.9790724872846775506, 36.03764935392171509, 21.39212563129806810 ) ) ;
#44282 = EDGE_CURVE ( 'NONE', #30382, #1638, #44956, .T. ) ;
#44283 = VERTEX_POINT ( 'NONE', #54692 ) ;
#44284 = CARTESIAN_POINT ( 'NONE',  ( 0.6009453534118439633, -12.87216801774577668, 46.35353704332089819 ) ) ;
#44285 = CIRCLE ( 'NONE', #48288, 15.14599999999999369 ) ;
#44286 = CARTESIAN_POINT ( 'NONE',  ( 4.833616638992205949, -3.476827473558217640, 46.11947910922901883 ) ) ;
#44287 = EDGE_CURVE ( 'NONE', #29776, #50801, #5644, .T. ) ;
#44288 = VECTOR ( 'NONE', #1622, 999.9999999999998863 ) ;
#44289 = CARTESIAN_POINT ( 'NONE',  ( -6.078075953587585900, -18.90195907099236905, -3.675747206441904780 ) ) ;
#44290 = CARTESIAN_POINT ( 'NONE',  ( 3.680882792899939027, 30.65151321162949571, 36.90742604464134757 ) ) ;
#44291 = ORIENTED_EDGE ( 'NONE', *, *, #13610, .F. ) ;
#44292 = CARTESIAN_POINT ( 'NONE',  ( 1.112077966505211624, -42.89240287839150056, -10.16228815013172770 ) ) ;
#44293 = FACE_OUTER_BOUND ( 'NONE', #47031, .T. ) ;
#44294 = EDGE_CURVE ( 'NONE', #21415, #5530, #10904, .T. ) ;
#44295 = CARTESIAN_POINT ( 'NONE',  ( 0.9762797500689124330, 41.46413394121043439, -6.086902470967093137 ) ) ;
#44296 = CARTESIAN_POINT ( 'NONE',  ( 0.9268187852002115479, -6.055792169277320447, 43.67014671501740963 ) ) ;
#44297 = VERTEX_POINT ( 'NONE', #54381 ) ;
#44298 = ORIENTED_EDGE ( 'NONE', *, *, #34175, .T. ) ;
#44299 = CARTESIAN_POINT ( 'NONE',  ( 0.9784957157296381158, -39.66552991218980395, -13.52696543122457662 ) ) ;
#44300 = CARTESIAN_POINT ( 'NONE',  ( 0.9722240741986378776, -20.94823706911174099, -37.44729083276446602 ) ) ;
#44301 = CARTESIAN_POINT ( 'NONE',  ( 0.9783242366443558602, 15.31217352658830855, -39.01117573334813216 ) ) ;
#44302 = CARTESIAN_POINT ( 'NONE',  ( -6.079354080745853928, -12.94495173828241441, -14.25556662296175148 ) ) ;
#44303 = B_SPLINE_CURVE_WITH_KNOTS ( 'NONE', 3,
 ( #27273, #3441, #41398, #26344, #45790, #22580, #41705, #36694, #55760, #55453, #17886, #36391, #59852, #12578, #31666, #60768 ),
 .UNSPECIFIED., .F., .F.,
 ( 4, 3, 3, 3, 3, 4 ),
 ( 1.551621725782133898E-17, 0.0002724568934985577696, 0.0004086836638483767317, 0.0005449104342063555619, 0.0008173270854453671070, 0.001089761613562691828 ),
 .UNSPECIFIED. ) ;
#44304 = CARTESIAN_POINT ( 'NONE',  ( 0.1098349054025746369, 34.34238705454303897, -26.08296594991503881 ) ) ;
#44305 = CARTESIAN_POINT ( 'NONE',  ( 0.1157506346131639274, -31.63194487325750259, 30.76297650322595700 ) ) ;
#44306 = B_SPLINE_CURVE_WITH_KNOTS ( 'NONE', 3,
 ( #15832, #1386, #11434, #21136, #7317, #54939, #11133, #20834, #16755, #44971, #2007, #1695, #6691, #53694, #35870, #54009 ),
 .UNSPECIFIED., .F., .F.,
 ( 4, 3, 3, 3, 3, 4 ),
 ( 2.081781105835003155E-17, 0.0002612764279487734338, 0.0003919131003184793535, 0.0005225497727000639548, 0.0007837925190632447038, 0.001045051706266716951 ),
 .UNSPECIFIED. ) ;
#44307 = CARTESIAN_POINT ( 'NONE',  ( 5.960721111146673579, 14.50930005614996610, 14.51823969584104645 ) ) ;
#44308 = CARTESIAN_POINT ( 'NONE',  ( 1.088313998177383279, 37.54798835078488395, -20.77783415101586328 ) ) ;
#44309 = CARTESIAN_POINT ( 'NONE',  ( 2.526552050251861914, -12.29062829844006721, 41.18423939305560566 ) ) ;
#44310 = ADVANCED_FACE ( 'NONE', ( #40339 ), #16125, .F. ) ;
#44311 = CARTESIAN_POINT ( 'NONE',  ( 0.6009453534118440743, -18.00606795643245306, -44.61081284455525520 ) ) ;
#44312 = CARTESIAN_POINT ( 'NONE',  ( -6.077587904424778920, -12.94128980615197477, 14.25899854643086329 ) ) ;
#44313 = EDGE_CURVE ( 'NONE', #27771, #26826, #2070, .T. ) ;
#44314 = CARTESIAN_POINT ( 'NONE',  ( 0.1139756605157203756, -7.434439534098977731, -43.49349754283792890 ) ) ;
#44315 = CARTESIAN_POINT ( 'NONE',  ( 1.227938101723748288, -41.66816631169199070, 10.28900963485366127 ) ) ;
#44316 = CARTESIAN_POINT ( 'NONE',  ( 0.8560838555295158248, 17.70877843982841782, -43.43698884880027578 ) ) ;
#44317 = CARTESIAN_POINT ( 'NONE',  ( 0.5832366564991512403, -41.34220239953998544, 24.18352361336810574 ) ) ;
#44318 = CARTESIAN_POINT ( 'NONE',  ( 0.5988103622719992414, -44.21009254328991744, -18.96890139669977771 ) ) ;
#44319 = ITEM_DEFINED_TRANSFORMATION ( 'NONE', 'NONE', #3883,  #14677 ) ;
#44320 = CARTESIAN_POINT ( 'NONE',  ( 0.9730545539215883499, -26.52009130076794108, 33.73144377768549163 ) ) ;
#44321 = EDGE_CURVE ( 'NONE', #24670, #55943, #25090, .T. ) ;
#44322 = CARTESIAN_POINT ( 'NONE',  ( 0.6028777368367060907, -30.68600655816066336, 38.33939006848692088 ) ) ;
#44323 = CARTESIAN_POINT ( 'NONE',  ( 0.7246131072078555446, -47.57651137777910577, -7.091231226024629741 ) ) ;
#44324 = CARTESIAN_POINT ( 'NONE',  ( 0.5807400328401637335, -24.41979442053141014, -41.20655774452994535 ) ) ;
#44326 = ORIENTED_EDGE ( 'NONE', *, *, #9120, .T. ) ;
#44325 = LINE ( 'NONE', #19897, #58320 ) ;
#44327 = VERTEX_POINT ( 'NONE', #26513 ) ;
#44328 = CARTESIAN_POINT ( 'NONE',  ( 4.553261556744873317, -43.07273893850290136, 8.618510669437750238 ) ) ;
#44329 = CARTESIAN_POINT ( 'NONE',  ( 1.112077966505211846, 43.90950196486499379, -3.871170666099937652 ) ) ;
#44330 = CARTESIAN_POINT ( 'NONE',  ( 2.526464513654346433, 40.15570173027691681, 15.32058692775006037 ) ) ;
#44331 = VERTEX_POINT ( 'NONE', #46262 ) ;
#44332 = EDGE_CURVE ( 'NONE', #28177, #55165, #41532, .T. ) ;
#44333 = ORIENTED_EDGE ( 'NONE', *, *, #7100, .T. ) ;
#44334 = CARTESIAN_POINT ( 'NONE',  ( -6.078726893082806448, 0.6137717894417996645, 19.24622886331775717 ) ) ;
#44335 = FACE_OUTER_BOUND ( 'NONE', #54157, .T. ) ;
#44336 = CARTESIAN_POINT ( 'NONE',  ( 0.1095718737110178698, -37.47471772507234533, 21.33933464366355537 ) ) ;
#44337 = VECTOR ( 'NONE', #13983, 1000.000000000000114 ) ;
#44338 = B_SPLINE_CURVE_WITH_KNOTS ( 'NONE', 3,
 ( #22969, #17965, #56456, #13570, #51142, #56762, #51441, #28266, #8228, #18572, #33300, #57066, #47090, #47383, #23569, #47693 ),
 .UNSPECIFIED., .F., .F.,
 ( 4, 3, 3, 3, 3, 4 ),
 ( 1.962735358247463844E-17, 0.0002612764279487806980, 0.0003919131003184837445, 0.0005225497727000715442, 0.0007837925190632499079, 0.001045051706266720637 ),
 .UNSPECIFIED. ) ;
#44339 = ORIENTED_EDGE ( 'NONE', *, *, #12175, .T. ) ;
#44340 = VERTEX_POINT ( 'NONE', #60318 ) ;
#44341 =( BOUNDED_SURFACE ( )  B_SPLINE_SURFACE ( 3, 1, ( 
 ( #53496, #58199 ),
 ( #53797, #53199 ),
 ( #48212, #15323 ),
 ( #10614, #24394 ) ),
 .UNSPECIFIED., .F., .F., .F. ) 
 B_SPLINE_SURFACE_WITH_KNOTS ( ( 4, 4 ),
 ( 2, 2 ),
 ( 0.000000000000000000, 1.000000000000000000 ),
 ( 0.000000000000000000, 1.000000000000000000 ),
 .UNSPECIFIED. ) 
 GEOMETRIC_REPRESENTATION_ITEM ( )  RATIONAL_B_SPLINE_SURFACE ( (
 ( 1.000000000000000000, 1.000000000000000000),
 ( 0.7282232189291693025, 0.9929344683865674037),
 ( 0.7282232189291693025, 0.9929344683865674037),
 ( 1.000000000000000000, 1.000000000000000000) ) ) 
 REPRESENTATION_ITEM ( '' )  SURFACE ( )  );
#44342 = CARTESIAN_POINT ( 'NONE',  ( 0.6001305935487422083, 46.60388846085722037, -11.94532529598331649 ) ) ;
#44343 = CARTESIAN_POINT ( 'NONE',  ( 2.281448460670572054, -47.71650330356583680, -4.956513608981671482 ) ) ;
#44344 = CARTESIAN_POINT ( 'NONE',  ( 0.9754292589017198312, -41.18084051786591715, -7.775978468165505753 ) ) ;
#44345 = CARTESIAN_POINT ( 'NONE',  ( 0.7948884756798514362, 36.81796298084067587, 32.48286081215135823 ) ) ;
#44346 = CARTESIAN_POINT ( 'NONE',  ( 0.3676999524040323597, -2.238562284876542741, 44.05609404179593724 ) ) ;
#44347 = CARTESIAN_POINT ( 'NONE',  ( -6.078457390727109555, 5.483070842475943785, 18.45888526357694559 ) ) ;
#44348 = B_SPLINE_CURVE_WITH_KNOTS ( 'NONE', 3,
 ( #58586, #44243, #6263, #977 ),
 .UNSPECIFIED., .F., .F.,
 ( 4, 4 ),
 ( 0.000000000000000000, 0.004445488388166994251 ),
 .UNSPECIFIED. ) ;
#44349 = VECTOR ( 'NONE', #48610, 999.9999999999998863 ) ;
#44350 = CARTESIAN_POINT ( 'NONE',  ( 0.9745511491811735816, 42.49552597049459735, 5.938142320543482455 ) ) ;
#44351 = ORIENTED_EDGE ( 'NONE', *, *, #42033, .F. ) ;
#44352 = VERTEX_POINT ( 'NONE', #7077 ) ;
#44353 = CARTESIAN_POINT ( 'NONE',  ( -6.078726893082806448, 7.797636468844896918, -17.60655862934208216 ) ) ;
#44354 = DIRECTION ( 'NONE',  ( 0.000000000000000000, 0.000000000000000000, 1.000000000000000000 ) ) ;
#44355 = ORIENTED_EDGE ( 'NONE', *, *, #8804, .T. ) ;
#44356 = CARTESIAN_POINT ( 'NONE',  ( 0.8744876279028306332, -8.712669995481570950, -48.31603700562917680 ) ) ;
#44357 = CARTESIAN_POINT ( 'NONE',  ( 0.1064266379913942628, 37.62465837278045200, 21.07422113734176961 ) ) ;
#44358 = DIRECTION ( 'NONE',  ( -1.000000000000000000, -0.000000000000000000, -0.000000000000000000 ) ) ;
#44359 = DIRECTION ( 'NONE',  ( 0.000000000000000000, 0.000000000000000000, 1.000000000000000000 ) ) ;
#44360 = EDGE_CURVE ( 'NONE', #32791, #46412, #13912, .T. ) ;
#44361 = ORIENTED_EDGE ( 'NONE', *, *, #46681, .F. ) ;
#44362 = CARTESIAN_POINT ( 'NONE',  ( 0.8551540677456739292, -46.03951182599418246, -13.28067116677249615 ) ) ;
#44363 = DIRECTION ( 'NONE',  ( -1.000000000000000000, -0.000000000000000000, -0.000000000000000000 ) ) ;
#44364 = ADVANCED_FACE ( 'NONE', ( #12138 ), #43780, .F. ) ;
#44365 = DIRECTION ( 'NONE',  ( -1.000000000000000000, 0.000000000000000000, 0.000000000000000000 ) ) ;
#44366 = CARTESIAN_POINT ( 'NONE',  ( 0.9756008150404603674, -21.57722292874432668, -37.08855330282523255 ) ) ;
#44367 = EDGE_LOOP ( 'NONE', ( #59242, #17911, #34219, #19143 ) ) ;
#44368 = CARTESIAN_POINT ( 'NONE',  ( 0.5850706913938533704, 24.10530971368346442, -41.38834827854183374 ) ) ;
#44369 = DIRECTION ( 'NONE',  ( 0.000000000000000000, 0.7071067811865421326, 0.7071067811865527908 ) ) ;
#44371 = VERTEX_POINT ( 'NONE', #49387 ) ;
#44370 = EDGE_CURVE ( 'NONE', #26859, #9792, #36323, .T. ) ;
#44372 = CARTESIAN_POINT ( 'NONE',  ( 0.5988103564986355654, 48.10388392110854738, -0.6065102550368329792 ) ) ;
#44373 = CARTESIAN_POINT ( 'NONE',  ( 0.8760168074887076939, -42.09738177923939162, -23.27577685234582816 ) ) ;
#44374 = EDGE_CURVE ( 'NONE', #52485, #9403, #47512, .T. ) ;
#44375 = EDGE_LOOP ( 'NONE', ( #25934, #16346, #53837, #10357 ) ) ;
#44376 = B_SPLINE_CURVE_WITH_KNOTS ( 'NONE', 3,
 ( #59636, #54000, #58389, #20517, #31139, #7310, #26436, #49625, #15823, #34938, #39645, #53687, #2622, #39331, #15514, #34621, #29905, #11126, #39966 ),
 .UNSPECIFIED., .F., .F.,
 ( 4, 3, 3, 3, 3, 3, 4 ),
 ( 0.000000000000000000, 0.0002612768053151710585, 0.0003919133833142919012, 0.0005225499612322616208, 0.0006531865391693383437, 0.0008112755173415223510, 0.0009693688056799709468 ),
 .UNSPECIFIED. ) ;
#44377 = CARTESIAN_POINT ( 'NONE',  ( 4.553261556744875094, -39.67390170502071811, 18.85526688551479424 ) ) ;
#44378 = ADVANCED_FACE ( 'NONE', ( #30899 ), #20286, .F. ) ;
#44379 = CARTESIAN_POINT ( 'NONE',  ( 0.6023143664670691511, -47.72938193173976629, 6.019611522082517041 ) ) ;
#44380 = CARTESIAN_POINT ( 'NONE',  ( 4.549368137175248350, 2.596185425821331272, 42.84816078363931524 ) ) ;
#44381 = VECTOR ( 'NONE', #2738, 1000.000000000000000 ) ;
#44382 = DIRECTION ( 'NONE',  ( 0.1011922191286468153, 0.7658109114536828521, 0.6350541572860533002 ) ) ;
#44383 = CARTESIAN_POINT ( 'NONE',  ( 1.657374760986086715, 21.46677708116468253, 38.47165097834802339 ) ) ;
#44384 = ADVANCED_FACE ( 'NONE', ( #6442 ), #37739, .F. ) ;
#44385 = CARTESIAN_POINT ( 'NONE',  ( 5.895881250540457863, -7.232970327322216342, 18.76730726162859142 ) ) ;
#44386 = B_SPLINE_CURVE_WITH_KNOTS ( 'NONE', 3,
 ( #30656, #2766, #36319, #16264 ),
 .UNSPECIFIED., .F., .F.,
 ( 4, 4 ),
 ( 0.000000000000000000, 0.005004948556313800964 ),
 .UNSPECIFIED. ) ;
#44387 = CARTESIAN_POINT ( 'NONE',  ( 1.827326673878744145, -9.946825761454215709, -41.88502433275000669 ) ) ;
#44388 = ORIENTED_EDGE ( 'NONE', *, *, #26726, .T. ) ;
#44389 = CARTESIAN_POINT ( 'NONE',  ( -31.75000000000000000, 0.000000000000000000, 0.000000000000000000 ) ) ;
#44390 = EDGE_CURVE ( 'NONE', #50838, #28664, #15894, .T. ) ;
#44391 = CARTESIAN_POINT ( 'NONE',  ( 16.98648177666931502, -7.159091074317975867, -9.346835372692149838E-16 ) ) ;
#44392 = CARTESIAN_POINT ( 'NONE',  ( 2.281448460670565392, 47.95523685111403722, -1.314143534316070339 ) ) ;
#44393 = VERTEX_POINT ( 'NONE', #40642 ) ;
#44394 = CARTESIAN_POINT ( 'NONE',  ( 0.5988103622719990193, -0.6065097949916992137, 48.10388392585941375 ) ) ;
#44395 = DIRECTION ( 'NONE',  ( 1.000000000000000000, 0.000000000000000000, 0.000000000000000000 ) ) ;
#44396 = CARTESIAN_POINT ( 'NONE',  ( 3.783198216974389627, -3.901161703631771172, -42.86118135813608632 ) ) ;
#44397 = CIRCLE ( 'NONE', #12362, 4.000000000000000888 ) ;
#44398 = CARTESIAN_POINT ( 'NONE',  ( 4.967162193818130511, 36.06913038482831979, -23.56777426397140118 ) ) ;
#44400 = B_SPLINE_CURVE_WITH_KNOTS ( 'NONE', 3,
 ( #46451, #37059, #17942, #13238 ),
 .UNSPECIFIED., .F., .F.,
 ( 4, 4 ),
 ( 0.000000000000000000, 0.004444878191957685187 ),
 .UNSPECIFIED. ) ;
#44399 = CARTESIAN_POINT ( 'NONE',  ( 0.9972139404380317984, 41.27214627875024888, -11.74016833743876731 ) ) ;
#44401 = CARTESIAN_POINT ( 'NONE',  ( 3.270143674763207553, 2.058141141425795073, -13.53222904135351889 ) ) ;
#44402 =( BOUNDED_SURFACE ( )  B_SPLINE_SURFACE ( 3, 1, ( 
 ( #47900, #19094 ),
 ( #37276, #61955 ),
 ( #27855, #241 ),
 ( #38508, #14697 ) ),
 .UNSPECIFIED., .F., .F., .F. ) 
 B_SPLINE_SURFACE_WITH_KNOTS ( ( 4, 4 ),
 ( 2, 2 ),
 ( 0.000000000000000000, 1.000000000000000000 ),
 ( 0.000000000000000000, 1.000000000000000000 ),
 .UNSPECIFIED. ) 
 GEOMETRIC_REPRESENTATION_ITEM ( )  RATIONAL_B_SPLINE_SURFACE ( (
 ( 1.000000000000000000, 1.000000000000000000),
 ( 0.7282232189291693025, 0.9929344683865674037),
 ( 0.7282232189291693025, 0.9929344683865674037),
 ( 1.000000000000000000, 1.000000000000000000) ) ) 
 REPRESENTATION_ITEM ( '' )  SURFACE ( )  );
#44403 = CARTESIAN_POINT ( 'NONE',  ( -5.272380000000000067, 0.000000000000000000, 15.38217999999999996 ) ) ;
#44404 = CARTESIAN_POINT ( 'NONE',  ( 5.894904586330512508, 8.467339502218703018, 18.24372697164177026 ) ) ;
#44406 = ORIENTED_EDGE ( 'NONE', *, *, #28719, .T. ) ;
#44405 = CARTESIAN_POINT ( 'NONE',  ( 4.967162193818130511, 0.000000000000000000, 0.000000000000000000 ) ) ;
#44407 = VERTEX_POINT ( 'NONE', #40333 ) ;
#44408 = CARTESIAN_POINT ( 'NONE',  ( 0.000000000000000000, 0.6959691356230525150, -1.199999999999999956 ) ) ;
#44409 = CARTESIAN_POINT ( 'NONE',  ( 4.975610109902397937, 48.43414999183889336, 6.825138951393308950 ) ) ;
#44410 = CARTESIAN_POINT ( 'NONE',  ( 0.1104177457020373149, 16.50753524010242401, 39.83992599038892024 ) ) ;
#44411 = EDGE_CURVE ( 'NONE', #36353, #10343, #1891, .T. ) ;
#44412 = PRODUCT_DEFINITION_SHAPE ( 'NONE', 'NONE',  #61996 ) ;
#44413 = CARTESIAN_POINT ( 'NONE',  ( 3.407937589446178528, -13.51415833181189718, 2.242416846335549607 ) ) ;
#44414 = CARTESIAN_POINT ( 'NONE',  ( 0.8560838555295158248, 31.94705745926175311, 34.34761059777461867 ) ) ;
#44415 = CARTESIAN_POINT ( 'NONE',  ( 0.1129192098497455998, 10.29049805561888498, -42.90754522869442411 ) ) ;
#44416 =( BOUNDED_SURFACE ( )  B_SPLINE_SURFACE ( 3, 1, ( 
 ( #39949, #15500 ),
 ( #59311, #16418 ),
 ( #3150, #51068 ),
 ( #24896, #44037 ) ),
 .UNSPECIFIED., .F., .F., .F. ) 
 B_SPLINE_SURFACE_WITH_KNOTS ( ( 4, 4 ),
 ( 2, 2 ),
 ( 0.000000000000000000, 1.000000000000000000 ),
 ( 0.000000000000000000, 1.000000000000000000 ),
 .UNSPECIFIED. ) 
 GEOMETRIC_REPRESENTATION_ITEM ( )  RATIONAL_B_SPLINE_SURFACE ( (
 ( 1.000000000000000000, 1.000000000000000000),
 ( 0.7211978278499968642, 0.9934217856018975334),
 ( 0.7211978278499968642, 0.9934217856018975334),
 ( 1.000000000000000000, 1.000000000000000000) ) ) 
 REPRESENTATION_ITEM ( '' )  SURFACE ( )  );
#44418 = EDGE_CURVE ( 'NONE', #18802, #22171, #55691, .T. ) ;
#44417 = ORIENTED_EDGE ( 'NONE', *, *, #973, .T. ) ;
#44419 = ORIENTED_EDGE ( 'NONE', *, *, #60668, .T. ) ;
#44420 = CARTESIAN_POINT ( 'NONE',  ( 3.376099380956842921, -12.50537924370754261, 4.829479641029207571 ) ) ;
#44421 = CARTESIAN_POINT ( 'NONE',  ( 0.1092565886968784733, -39.95965440403635682, -16.21587544131310210 ) ) ;
#44422 = CARTESIAN_POINT ( 'NONE',  ( 0.6008122571543325074, 37.67355775107387217, 31.50012058455996211 ) ) ;
#44423 = VERTEX_POINT ( 'NONE', #20586 ) ;
#44424 = PRODUCT_RELATED_PRODUCT_CATEGORY ( 'part', '', ( #54756 ) ) ;
#44425 = CIRCLE ( 'NONE', #41424, 43.08621763946400307 ) ;
#44426 = CARTESIAN_POINT ( 'NONE',  ( 0.1064266379913939020, 37.06314005629914021, -22.04679939086795670 ) ) ;
#44427 = CARTESIAN_POINT ( 'NONE',  ( 2.624215991343620935, 47.98682984381861161, -1.411420423865646034 ) ) ;
#44428 = VERTEX_POINT ( 'NONE', #21197 ) ;
#44429 =( REPRESENTATION_RELATIONSHIP ('NONE','NONE', #44881, #16880 ) REPRESENTATION_RELATIONSHIP_WITH_TRANSFORMATION ( #59684 )SHAPE_REPRESENTATION_RELATIONSHIP( ) );
#44430 = CARTESIAN_POINT ( 'NONE',  ( 4.834790513006555379, -21.44535528597729979, 42.10327870347612134 ) ) ;
#44431 = ORIENTED_EDGE ( 'NONE', *, *, #202, .T. ) ;
#44432 = CARTESIAN_POINT ( 'NONE',  ( 1.154321713695927398, -33.53917066545405845, -26.77578845938217711 ) ) ;
#44433 = ORIENTED_EDGE ( 'NONE', *, *, #9749, .T. ) ;
#44434 = CARTESIAN_POINT ( 'NONE',  ( 5.917102823773431552, -17.29995091781572114, -10.25677416602847281 ) ) ;
#44435 = CARTESIAN_POINT ( 'NONE',  ( 4.956445790444002242, -32.34643101787113295, 34.22347806032784234 ) ) ;
#44436 = CARTESIAN_POINT ( 'NONE',  ( 0.5987334363312695196, 22.17584323994378082, 43.81546397186176023 ) ) ;
#44437 = CARTESIAN_POINT ( 'NONE',  ( 0.08486401232817714080, 1.224646799147353256E-15, -10.00000000000000000 ) ) ;
#44438 = B_SPLINE_CURVE_WITH_KNOTS ( 'NONE', 3,
 ( #50057, #27476, #55659, #32187 ),
 .UNSPECIFIED., .F., .F.,
 ( 4, 4 ),
 ( 0.000000000000000000, 0.005014147105413710795 ),
 .UNSPECIFIED. ) ;
#44439 = VECTOR ( 'NONE', #3707, 1000.000000000000114 ) ;
#44440 = ORIENTED_EDGE ( 'NONE', *, *, #700, .T. ) ;
#44441 = CARTESIAN_POINT ( 'NONE',  ( 5.917102823773431552, 14.91028373222390080, 13.49715366572972286 ) ) ;
#44442 = DIRECTION ( 'NONE',  ( 0.000000000000000000, 0.000000000000000000, 1.000000000000000000 ) ) ;
#44443 = EDGE_CURVE ( 'NONE', #49823, #26123, #35932, .T. ) ;
#44444 = ORIENTED_EDGE ( 'NONE', *, *, #28831, .T. ) ;
#44445 = DIRECTION ( 'NONE',  ( 0.1011922191286468153, 0.4715280952439158124, 0.8760259072558667093 ) ) ;
#44446 = ORIENTED_EDGE ( 'NONE', *, *, #45373, .T. ) ;
#44447 = ORIENTED_EDGE ( 'NONE', *, *, #23142, .F. ) ;
#44448 = CARTESIAN_POINT ( 'NONE',  ( 1.092182651088182688, -31.60377597355978097, -27.53111927719848140 ) ) ;
#44449 = CARTESIAN_POINT ( 'NONE',  ( 0.5997462898726536595, -30.20781297212564454, -38.71743361310750231 ) ) ;
#44450 = EDGE_CURVE ( 'NONE', #47109, #22114, #30294, .T. ) ;
#44451 = CARTESIAN_POINT ( 'NONE',  ( 0.6000166863083090663, -42.53190469623903880, -24.55321902762434050 ) ) ;
#44452 = ORIENTED_EDGE ( 'NONE', *, *, #59609, .T. ) ;
#44453 = CARTESIAN_POINT ( 'NONE',  ( 0.5834872094924171693, 6.026535573894117981, 47.51530820063769056 ) ) ;
#44454 = EDGE_CURVE ( 'NONE', #9995, #46120, #32536, .T. ) ;
#44455 = LINE ( 'NONE', #1482, #50636 ) ;
#44456 = CARTESIAN_POINT ( 'NONE',  ( 0.8760168074887090262, 38.69913431881784049, 28.57146030081993970 ) ) ;
#44457 = EDGE_LOOP ( 'NONE', ( #6859, #6302, #23222, #35574 ) ) ;
#44458 = B_SPLINE_CURVE_WITH_KNOTS ( 'NONE', 3,
 ( #38771, #10867, #40011, #510 ),
 .UNSPECIFIED., .F., .F.,
 ( 4, 4 ),
 ( 0.000000000000000000, 0.005004948556313794893 ),
 .UNSPECIFIED. ) ;
#44459 = ORIENTED_EDGE ( 'NONE', *, *, #28056, .T. ) ;
#44460 = CARTESIAN_POINT ( 'NONE',  ( 0.8760168074886965917, 5.394043284318857268, 47.80016357497251533 ) ) ;
#44461 = CARTESIAN_POINT ( 'NONE',  ( 1.088313998177381281, -42.90642884828984194, -0.7798619649925772057 ) ) ;
#44462 = CARTESIAN_POINT ( 'NONE',  ( 0.5980271706414711508, -19.23780022038679505, -45.18801041783260075 ) ) ;
#44463 = CARTESIAN_POINT ( 'NONE',  ( 0.1102144999581332885, 30.40435207217186075, 30.58258619461932071 ) ) ;
#44464 = CARTESIAN_POINT ( 'NONE',  ( 0.9772918015221170318, -27.37292454379962692, -31.73420642886996745 ) ) ;
#44465 = CARTESIAN_POINT ( 'NONE',  ( 0.9775691876210972353, 38.43414426860777411, 16.70779049814292705 ) ) ;
#44466 = ORIENTED_EDGE ( 'NONE', *, *, #20822, .F. ) ;
#44467 = CARTESIAN_POINT ( 'NONE',  ( 4.958415959904818315, -42.01301765298939017, -17.26587100357933124 ) ) ;
#44468 = VERTEX_POINT ( 'NONE', #20891 ) ;
#44469 = CARTESIAN_POINT ( 'NONE',  ( 0.5830082357119558134, 36.63400490284909239, 29.27766588572876927 ) ) ;
#44470 = CARTESIAN_POINT ( 'NONE',  ( 4.967162193818130511, 43.02067033766018511, 2.375726030842731706 ) ) ;
#44471 = CARTESIAN_POINT ( 'NONE',  ( 4.549368137175248350, 0.000000000000000000, 0.000000000000000000 ) ) ;
#44472 = CIRCLE ( 'NONE', #11437, 47.91270532121795611 ) ;
#44473 = CARTESIAN_POINT ( 'NONE',  ( 2.281351352603294913, -47.71649595778612252, 4.956540261593589847 ) ) ;
#44474 = CARTESIAN_POINT ( 'NONE',  ( 3.680974057930775700, -20.05478739720764025, 43.58300585207889100 ) ) ;
#44475 = DIRECTION ( 'NONE',  ( -1.000000000000000000, -0.000000000000000000, -0.000000000000000000 ) ) ;
#44476 = B_SPLINE_CURVE_WITH_KNOTS ( 'NONE', 3,
 ( #16006, #59506, #34189, #48576 ),
 .UNSPECIFIED., .F., .F.,
 ( 4, 4 ),
 ( 8.673617379884035472E-19, 0.004048833967417089959 ),
 .UNSPECIFIED. ) ;
#44477 = CARTESIAN_POINT ( 'NONE',  ( 0.1152809850208375841, 20.60499082682811434, -39.01768362571110060 ) ) ;
#44478 = CARTESIAN_POINT ( 'NONE',  ( 5.896782393890504181, 8.471952691971054605, 18.24149403045202078 ) ) ;
#44479 = CARTESIAN_POINT ( 'NONE',  ( 0.1158516988532803244, 29.70113990798797943, 32.63103502800547062 ) ) ;
#44480 = CARTESIAN_POINT ( 'NONE',  ( 3.661921753702006566, -37.68385958972724126, 28.15240398715106096 ) ) ;
#44481 = CARTESIAN_POINT ( 'NONE',  ( 3.678834586032787346, -5.985442328740523621, -48.60850594039765582 ) ) ;
#44482 = CARTESIAN_POINT ( 'NONE',  ( 0.5827359174754822568, -23.63273677570887799, -41.65957726278062268 ) ) ;
#44483 = CARTESIAN_POINT ( 'NONE',  ( 0.9268187852002115479, -18.74830179125902774, -39.90307648355574344 ) ) ;
#44484 = CARTESIAN_POINT ( 'NONE',  ( 3.270143674763207553, -3.277085381513020756, -13.28976595685396944 ) ) ;
#44485 = EDGE_CURVE ( 'NONE', #4004, #5670, #7900, .T. ) ;
#44486 = ORIENTED_EDGE ( 'NONE', *, *, #6040, .F. ) ;
#44487 = DIRECTION ( 'NONE',  ( -1.000000000000000000, -0.000000000000000000, -0.000000000000000000 ) ) ;
#44488 = CARTESIAN_POINT ( 'NONE',  ( 0.8753041380234471980, -14.82204010568781172, 46.81287702094758174 ) ) ;
#44489 = CARTESIAN_POINT ( 'NONE',  ( 0.6001305935487422083, 11.94532529598315129, 46.60388846085726300 ) ) ;
#44490 = CARTESIAN_POINT ( 'NONE',  ( 3.050102900204245682, 40.38856827381131609, 17.44100920158413359 ) ) ;
#44491 = FACE_OUTER_BOUND ( 'NONE', #31369, .T. ) ;
#44492 = VERTEX_POINT ( 'NONE', #55307 ) ;
#44493 = CARTESIAN_POINT ( 'NONE',  ( 5.860006189529246790, -36.27483683749458976, 31.78942168514550204 ) ) ;
#44494 = CARTESIAN_POINT ( 'NONE',  ( 43.00000000000000000, 0.000000000000000000, 75.00000000000001421 ) ) ;
#44495 = DIRECTION ( 'NONE',  ( -0.1024043820194934368, 0.9878630899050878655, -0.1167898032637170735 ) ) ;
#44496 = ORIENTED_EDGE ( 'NONE', *, *, #40789, .F. ) ;
#44497 = CARTESIAN_POINT ( 'NONE',  ( 0.7242003506640029009, 43.87790776620104083, -22.03953003552434708 ) ) ;
#44498 = CIRCLE ( 'NONE', #449, 12.50000000000000000 ) ;
#44499 = CARTESIAN_POINT ( 'NONE',  ( 1.154321713695928731, -41.23280394713385277, -11.90271797554057542 ) ) ;
#44500 = ORIENTED_EDGE ( 'NONE', *, *, #20106, .F. ) ;
#44501 = CARTESIAN_POINT ( 'NONE',  ( 3.783278058412225864, -40.39104487792931764, -14.86148287637775844 ) ) ;
#44502 = B_SPLINE_CURVE_WITH_KNOTS ( 'NONE', 3,
 ( #36908, #21860, #2423, #31881, #50966, #26864 ),
 .UNSPECIFIED., .F., .F.,
 ( 4, 2, 4 ),
 ( 1.964591557601686678E-17, 0.0002293755540694308577, 0.0004587511081388420371 ),
 .UNSPECIFIED. ) ;
#44503 = ORIENTED_EDGE ( 'NONE', *, *, #5112, .T. ) ;
#44504 = CARTESIAN_POINT ( 'NONE',  ( 0.8751705887134423323, -46.67919521768896374, 11.58504748649118810 ) ) ;
#44505 = ORIENTED_EDGE ( 'NONE', *, *, #59677, .T. ) ;
#44506 = CARTESIAN_POINT ( 'NONE',  ( 0.1157991065609915715, 29.72493506311960942, -32.60936370171949505 ) ) ;
#44507 = CARTESIAN_POINT ( 'NONE',  ( 0.5998501479064708430, -28.86886762351098312, -38.48283596222019298 ) ) ;
#44508 =( BOUNDED_SURFACE ( )  B_SPLINE_SURFACE ( 3, 1, ( 
 ( #58484, #38818 ),
 ( #24075, #43203 ),
 ( #43514, #233 ),
 ( #19384, #38502 ) ),
 .UNSPECIFIED., .F., .F., .F. ) 
 B_SPLINE_SURFACE_WITH_KNOTS ( ( 4, 4 ),
 ( 2, 2 ),
 ( 0.000000000000000000, 1.000000000000000000 ),
 ( 0.000000000000000000, 1.000000000000000000 ),
 .UNSPECIFIED. ) 
 GEOMETRIC_REPRESENTATION_ITEM ( )  RATIONAL_B_SPLINE_SURFACE ( (
 ( 1.000000000000000000, 1.000000000000000000),
 ( 0.7282232189291694135, 0.9929344683865672927),
 ( 0.7282232189291694135, 0.9929344683865672927),
 ( 1.000000000000000000, 1.000000000000000000) ) ) 
 REPRESENTATION_ITEM ( '' )  SURFACE ( )  );
#44509 = ORIENTED_EDGE ( 'NONE', *, *, #29289, .T. ) ;
#44510 = VERTEX_POINT ( 'NONE', #46256 ) ;
#44511 = CARTESIAN_POINT ( 'NONE',  ( 3.270143674763207553, -6.605065939546904019, 11.98875605389977395 ) ) ;
#44512 = EDGE_CURVE ( 'NONE', #46085, #26923, #43637, .T. ) ;
#44513 = DIRECTION ( 'NONE',  ( -0.07439287786467650709, 0.3937848822959368333, 0.9161872986448712508 ) ) ;
#44514 = B_SPLINE_CURVE_WITH_KNOTS ( 'NONE', 3,
 ( #58832, #31901, #27192, #55992, #46625, #50373 ),
 .UNSPECIFIED., .F., .F.,
 ( 4, 2, 4 ),
 ( 0.000000000000000000, 0.0002291459268755701806, 0.0004582918537511403612 ),
 .UNSPECIFIED. ) ;
#44515 = AXIS2_PLACEMENT_3D ( 'NONE', #59569, #3473, #11999 ) ;
#44516 = EDGE_CURVE ( 'NONE', #58767, #50035, #25751, .T. ) ;
#44517 = ORIENTED_EDGE ( 'NONE', *, *, #21284, .T. ) ;
#44518 = CARTESIAN_POINT ( 'NONE',  ( 0.8554163680231720024, -39.19027442586699550, -25.79395013442211848 ) ) ;
#44519 = CARTESIAN_POINT ( 'NONE',  ( 1.227938101723757836, 39.96870412324336996, 15.63977281655856366 ) ) ;
#44520 = B_SPLINE_CURVE_WITH_KNOTS ( 'NONE', 3,
 ( #10200, #34022, #13994, #28070 ),
 .UNSPECIFIED., .F., .F.,
 ( 4, 4 ),
 ( 0.000000000000000000, 0.004445488388166992516 ),
 .UNSPECIFIED. ) ;
#44521 = VECTOR ( 'NONE', #54283, 999.9999999999998863 ) ;
#44522 = CARTESIAN_POINT ( 'NONE',  ( 0.6029303876144825880, 23.94027529185494885, 41.72757124235830162 ) ) ;
#44523 = CARTESIAN_POINT ( 'NONE',  ( 0.7044674535453004927, -45.19827881396748381, 19.20724642070708654 ) ) ;
#44524 = ORIENTED_EDGE ( 'NONE', *, *, #11230, .T. ) ;
#44525 = ADVANCED_FACE ( 'NONE', ( #41254 ), #41559, .F. ) ;
#44526 = LINE ( 'NONE', #39511, #7761 ) ;
#44527 = CARTESIAN_POINT ( 'NONE',  ( 0.5832367798473370168, -44.35360901387662125, 18.07699868820174771 ) ) ;
#44528 = CIRCLE ( 'NONE', #27450, 42.08604991992415023 ) ;
#44529 = ORIENTED_EDGE ( 'NONE', *, *, #43024, .F. ) ;
#44530 = CARTESIAN_POINT ( 'NONE',  ( 0.8557997880470697982, 47.37054680076715840, -7.156447707085226817 ) ) ;
#44531 = ORIENTED_EDGE ( 'NONE', *, *, #23837, .F. ) ;
#44532 = CARTESIAN_POINT ( 'NONE',  ( -6.015611763856276717, 13.32857883366833462, 13.31979030221804017 ) ) ;
#44533 = DIRECTION ( 'NONE',  ( -0.1011922191286467321, 0.8604626000150104037, 0.4993638440688594193 ) ) ;
#44534 = ORIENTED_EDGE ( 'NONE', *, *, #8391, .F. ) ;
#44535 = CARTESIAN_POINT ( 'NONE',  ( 0.7048096507298579061, 13.26491767067515504, -46.24547838151354995 ) ) ;
#44536 = CARTESIAN_POINT ( 'NONE',  ( 0.6000166863083090663, -14.47337940799656764, -46.92914627628159252 ) ) ;
#44537 = CARTESIAN_POINT ( 'NONE',  ( 51.67535452159865628, 12.27124677633248240, 2.381404722338403168 ) ) ;
#44538 = CARTESIAN_POINT ( 'NONE',  ( -18.52118801082394839, -12.33374936220940477, 2.032088317440561731 ) ) ;
#44539 = EDGE_CURVE ( 'NONE', #472, #23307, #23913, .T. ) ;
#44540 = VERTEX_POINT ( 'NONE', #27750 ) ;
#44541 = CARTESIAN_POINT ( 'NONE',  ( 4.975610109902397937, 45.11887670192734134, 18.88746601040093154 ) ) ;
#44542 = EDGE_CURVE ( 'NONE', #50113, #31710, #13055, .T. ) ;
#44543 = FACE_OUTER_BOUND ( 'NONE', #2641, .T. ) ;
#44544 = CARTESIAN_POINT ( 'NONE',  ( 0.9791128995231621612, 41.53406868334494817, -5.590936670482719251 ) ) ;
#44545 = B_SPLINE_CURVE_WITH_KNOTS ( 'NONE', 3,
 ( #44979, #40287, #29925, #59651, #59339, #44366, #54631, #26149, #35573, #49962, #45285, #2326, #21451, #40590, #13611, #41821, #51798, #7642, #13301 ),
 .UNSPECIFIED., .F., .F.,
 ( 4, 3, 3, 3, 3, 3, 4 ),
 ( 3.469446951953614189E-18, 0.0002724573126191772734, 0.0004086839781548497782, 0.0005449106435901813778, 0.0006811373090491465790, 0.0008459866663933634113, 0.001010840725717218353 ),
 .UNSPECIFIED. ) ;
#44546 = CARTESIAN_POINT ( 'NONE',  ( 0.8554163680231738898, -42.27859581856526461, 20.34025095032544073 ) ) ;
#44547 = AXIS2_PLACEMENT_3D ( 'NONE', #12419, #51525, #33080 ) ;
#44548 = DIRECTION ( 'NONE',  ( 0.000000000000000000, 0.000000000000000000, 1.000000000000000000 ) ) ;
#44549 = CARTESIAN_POINT ( 'NONE',  ( 0.1313383488274121325, 6.260443365526796811, 42.66669366003524999 ) ) ;
#44550 = CARTESIAN_POINT ( 'NONE',  ( -17.83428622022626087, -7.719455939378113030, 2.099999999999994316 ) ) ;
#44551 = DIRECTION ( 'NONE',  ( 0.09722883295013592941, -0.4097642837406412220, -0.9069949205004809167 ) ) ;
#44552 = CARTESIAN_POINT ( 'NONE',  ( 0.7954190325252782356, 47.56618055754175600, -7.138712176114947461 ) ) ;
#44553 = CARTESIAN_POINT ( 'NONE',  ( 0.1140933569871963454, -43.71187804725383330, -6.018443957196380367 ) ) ;
#44554 = FACE_OUTER_BOUND ( 'NONE', #21413, .T. ) ;
#44555 = ADVANCED_FACE ( 'NONE', ( #60015 ), #3906, .T. ) ;
#44556 = CARTESIAN_POINT ( 'NONE',  ( 0.9730545539215883499, 5.099196237954877198, 42.60426903087355299 ) ) ;
#44557 = CARTESIAN_POINT ( 'NONE',  ( 0.1156867017252034557, 36.91162943948151565, 24.17590576167908267 ) ) ;
#44558 = EDGE_LOOP ( 'NONE', ( #29614, #31119, #55115, #56347 ) ) ;
#44559 = CARTESIAN_POINT ( 'NONE',  ( 0.3622758884714600280, -41.42293301073617329, -11.95365414648482627 ) ) ;
#44560 = CARTESIAN_POINT ( 'NONE',  ( 0.5549461598389362482, 19.61782105380045849, -39.50137709710722334 ) ) ;
#44561 = CARTESIAN_POINT ( 'NONE',  ( 5.894904586330512508, -20.11291651039286066, 0.001227847351200775502 ) ) ;
#44562 = ORIENTED_EDGE ( 'NONE', *, *, #16524, .T. ) ;
#44563 = CARTESIAN_POINT ( 'NONE',  ( 3.238741278300274029, 38.98370040185400143, 18.12697907494908378 ) ) ;
#44564 = CARTESIAN_POINT ( 'NONE',  ( 0.1129192098497447394, 4.719118110134695954, 43.87119455916095490 ) ) ;
#44565 = DIRECTION ( 'NONE',  ( 1.000000000000000000, 1.836909530733573776E-16, -1.925929944387235853E-32 ) ) ;
#44566 = VERTEX_POINT ( 'NONE', #56240 ) ;
#44567 = ORIENTED_EDGE ( 'NONE', *, *, #7905, .T. ) ;
#44568 = CARTESIAN_POINT ( 'NONE',  ( 0.7242003506640006805, 37.91427066463845819, 31.20127808431195149 ) ) ;
#44569 = ORIENTED_EDGE ( 'NONE', *, *, #5543, .F. ) ;
#44570 = CARTESIAN_POINT ( 'NONE',  ( 3.376099380956842921, 6.842217874692535062, 11.52789825541954727 ) ) ;
#44571 = EDGE_LOOP ( 'NONE', ( #2612, #36967, #27469, #54785 ) ) ;
#44572 = ORIENTED_EDGE ( 'NONE', *, *, #34255, .T. ) ;
#44573 = CARTESIAN_POINT ( 'NONE',  ( 0.7044674535453004927, -20.64605418817839677, -44.55943412196466369 ) ) ;
#44574 = ORIENTED_EDGE ( 'NONE', *, *, #57561, .F. ) ;
#44575 = FACE_OUTER_BOUND ( 'NONE', #52861, .T. ) ;
#44576 = CARTESIAN_POINT ( 'NONE',  ( 3.783278058412224976, -18.05212641201942247, -39.06943705276849954 ) ) ;
#44577 = ORIENTED_EDGE ( 'NONE', *, *, #6875, .T. ) ;
#44578 = LINE ( 'NONE', #20143, #30711 ) ;
#44579 =( BOUNDED_SURFACE ( )  B_SPLINE_SURFACE ( 3, 1, ( 
 ( #52974, #10077 ),
 ( #657, #17786 ),
 ( #51277, #27481 ),
 ( #46302, #50361 ) ),
 .UNSPECIFIED., .F., .F., .F. ) 
 B_SPLINE_SURFACE_WITH_KNOTS ( ( 4, 4 ),
 ( 2, 2 ),
 ( 0.000000000000000000, 1.000000000000000000 ),
 ( 0.000000000000000000, 1.000000000000000000 ),
 .UNSPECIFIED. ) 
 GEOMETRIC_REPRESENTATION_ITEM ( )  RATIONAL_B_SPLINE_SURFACE ( (
 ( 1.000000000000000000, 1.000000000000000000),
 ( 0.9953390228620291325, 0.8624445117760984880),
 ( 0.9953390228620291325, 0.8624445117760984880),
 ( 1.000000000000000000, 1.000000000000000000) ) ) 
 REPRESENTATION_ITEM ( '' )  SURFACE ( )  );
#44580 = CARTESIAN_POINT ( 'NONE',  ( 0.7048096507298635682, -5.442192462019818322, 47.80151517212777890 ) ) ;
#44581 = EDGE_CURVE ( 'NONE', #5328, #42400, #51149, .T. ) ;
#44582 = VERTEX_POINT ( 'NONE', #55616 ) ;
#44583 = CARTESIAN_POINT ( 'NONE',  ( 0.6029303876144825880, -18.53079182983373130, 44.39523326884606291 ) ) ;
#44584 = CARTESIAN_POINT ( 'NONE',  ( -6.015611763856276717, -17.40650793417838571, -7.216738110653465377 ) ) ;
#44585 = CARTESIAN_POINT ( 'NONE',  ( 5.901463166500146684, -4.648441909663684868, 19.56808263865213604 ) ) ;
#44586 = CARTESIAN_POINT ( 'NONE',  ( 5.959547316686252039, 16.28624005235082350, 12.49238070347981910 ) ) ;
#44587 = ORIENTED_EDGE ( 'NONE', *, *, #3237, .F. ) ;
#44588 = EDGE_CURVE ( 'NONE', #25309, #1809, #28747, .T. ) ;
#44589 = ORIENTED_EDGE ( 'NONE', *, *, #19455, .F. ) ;
#44590 = CARTESIAN_POINT ( 'NONE',  ( 0.7057020205114953315, -37.48480537461314555, -29.82342581815244742 ) ) ;
#44591 = ADVANCED_FACE ( 'NONE', ( #48097 ), #50154, .F. ) ;
#44592 = CARTESIAN_POINT ( 'NONE',  ( 0.8760168074887090262, 42.09738177923922819, 23.27577685234613014 ) ) ;
#44593 = CARTESIAN_POINT ( 'NONE',  ( 0.6000166863083106206, -25.90381862410858460, -41.72308308835457069 ) ) ;
#44594 = AXIS2_PLACEMENT_3D ( 'NONE', #60030, #37485, #17436 ) ;
#44595 = VERTEX_POINT ( 'NONE', #38717 ) ;
#44596 = CARTESIAN_POINT ( 'NONE',  ( 2.526464513654347321, 42.75268905308553968, 4.405490210168531817 ) ) ;
#44597 = DIRECTION ( 'NONE',  ( 0.000000000000000000, 1.000000000000000000, 0.000000000000000000 ) ) ;
#44598 = CARTESIAN_POINT ( 'NONE',  ( 4.967162193818130511, 2.375726030843182457, -43.02067033766016380 ) ) ;
#44600 = EDGE_LOOP ( 'NONE', ( #17147, #51757, #41189, #8738 ) ) ;
#44599 = CIRCLE ( 'NONE', #25570, 42.08604991992415023 ) ;
#44601 = EDGE_LOOP ( 'NONE', ( #11341, #29748, #46353, #49116 ) ) ;
#44602 = CARTESIAN_POINT ( 'NONE',  ( 0.8551540677456834771, -38.56334384152411587, -28.44084013485158735 ) ) ;
#44603 = CARTESIAN_POINT ( 'NONE',  ( 4.390527457369401532, 42.41450209547013372, 11.45405380736354850 ) ) ;
#44604 = CARTESIAN_POINT ( 'NONE',  ( 0.1103310638050661735, -39.87325896099753919, 16.42686748615336256 ) ) ;
#44605 = EDGE_CURVE ( 'NONE', #12545, #3716, #10188, .T. ) ;
#44606 = VECTOR ( 'NONE', #54182, 1000.000000000000114 ) ;
#44607 = CARTESIAN_POINT ( 'NONE',  ( -6.078457390727109555, -19.21618051603929445, 1.238110420156431246 ) ) ;
#44608 = CARTESIAN_POINT ( 'NONE',  ( 3.238018933889920792, -12.74072440564274977, -4.132969149063681513 ) ) ;
#44609 = CARTESIAN_POINT ( 'NONE',  ( 0.8751705887134423323, 28.56654290188602019, 38.69254731947842885 ) ) ;
#44610 = CARTESIAN_POINT ( 'NONE',  ( 1.834102595619085507, -13.77633997718277392, -41.83790388739330979 ) ) ;
#44611 = DIRECTION ( 'NONE',  ( 1.000000000000000000, 0.000000000000000000, 0.000000000000000000 ) ) ;
#44612 = CARTESIAN_POINT ( 'NONE',  ( 0.6027935024548037868, -6.452291758825078105, 47.67281620606621573 ) ) ;
#44613 = CARTESIAN_POINT ( 'NONE',  ( 3.680882792899938138, 36.90742604464125520, -30.65151321162960940 ) ) ;
#44614 = CARTESIAN_POINT ( 'NONE',  ( 0.6008122571543326185, 41.39240437578163068, 26.42391739423000274 ) ) ;
#44615 = CARTESIAN_POINT ( 'NONE',  ( 0.5782707292762442330, -34.29472224813873282, -31.99388034656996282 ) ) ;
#44616 = CARTESIAN_POINT ( 'NONE',  ( 4.553261556744875094, 0.000000000000000000, 0.000000000000000000 ) ) ;
#44617 = CARTESIAN_POINT ( 'NONE',  ( 0.5836750258453343720, -41.56963612796205609, 23.79054009282533144 ) ) ;
#44618 = DIRECTION ( 'NONE',  ( -1.000000000000000000, -0.000000000000000000, -0.000000000000000000 ) ) ;
#44619 = CARTESIAN_POINT ( 'NONE',  ( 0.3622758884714600280, -43.10531414739104861, -0.8252992914326565677 ) ) ;
#44620 = CARTESIAN_POINT ( 'NONE',  ( 0.1100053167205930632, -0.1794603581041471496, -43.12409768020066281 ) ) ;
#44621 = LINE ( 'NONE', #11400, #53229 ) ;
#44622 = DIRECTION ( 'NONE',  ( 0.000000000000000000, 0.000000000000000000, 1.000000000000000000 ) ) ;
#44624 = EDGE_LOOP ( 'NONE', ( #58123, #36051, #55229, #20183 ) ) ;
#44623 = CARTESIAN_POINT ( 'NONE',  ( 4.975610109902397937, 7.237810502494805398, -48.37420290059309025 ) ) ;
#44625 = ORIENTED_EDGE ( 'NONE', *, *, #33721, .T. ) ;
#44626 = CARTESIAN_POINT ( 'NONE',  ( 0.1310142868023714269, -37.66054729763607867, 21.00772081177013462 ) ) ;
#44627 = CARTESIAN_POINT ( 'NONE',  ( 1.834102595619085729, 43.85446432522261517, -4.121128923664326038 ) ) ;
#44628 = CARTESIAN_POINT ( 'NONE',  ( 0.1129192098497447394, 42.02659449688918869, 13.44310763102032702 ) ) ;
#44629 = EDGE_CURVE ( 'NONE', #55688, #11233, #58565, .T. ) ;
#44630 = VERTEX_POINT ( 'NONE', #37802 ) ;
#44631 = ORIENTED_EDGE ( 'NONE', *, *, #12603, .T. ) ;
#44632 = CARTESIAN_POINT ( 'NONE',  ( 0.1103744047535531458, -11.19884698423395797, 41.64495780681018999 ) ) ;
#44633 = CARTESIAN_POINT ( 'NONE',  ( 4.956653778116992370, 26.26162724282429650, -40.28700667097652399 ) ) ;
#44634 = CARTESIAN_POINT ( 'NONE',  ( 0.1092565886968784872, -37.19081526480840694, 21.83052579204398214 ) ) ;
#44635 = EDGE_CURVE ( 'NONE', #9930, #42917, #36992, .T. ) ;
#44636 = EDGE_LOOP ( 'NONE', ( #49723, #9996 ) ) ;
#44637 = ORIENTED_EDGE ( 'NONE', *, *, #55948, .T. ) ;
#44638 = DIRECTION ( 'NONE',  ( -1.000000000000000000, -0.000000000000000000, -0.000000000000000000 ) ) ;
#44639 = EDGE_CURVE ( 'NONE', #19741, #30901, #33204, .T. ) ;
#44640 = CARTESIAN_POINT ( 'NONE',  ( 0.8551540677456715978, 29.88829867897868553, -37.45266983663464089 ) ) ;
#44641 = CARTESIAN_POINT ( 'NONE',  ( 0.6001305935487315502, -6.798494447611894920, -47.62765676940940551 ) ) ;
#44642 = CARTESIAN_POINT ( 'NONE',  ( -6.078726893082806448, -19.21623043802544828, -1.237145513439781075 ) ) ;
#44643 = VERTEX_POINT ( 'NONE', #9249 ) ;
#44645 = CARTESIAN_POINT ( 'NONE',  ( 1.827119703190778877, -41.24693285842936774, 12.32825544177764954 ) ) ;
#44644 = AXIS2_PLACEMENT_3D ( 'NONE', #34667, #59062, #11474 ) ;
#44646 = CARTESIAN_POINT ( 'NONE',  ( 0.8560838555295158248, -29.58154842764465542, -36.40473632241614155 ) ) ;
#44647 = LINE ( 'NONE', #59018, #55961 ) ;
#44648 = ORIENTED_EDGE ( 'NONE', *, *, #47368, .T. ) ;
#44649 = EDGE_CURVE ( 'NONE', #52565, #19604, #39991, .T. ) ;
#44650 = AXIS2_PLACEMENT_3D ( 'NONE', #26570, #36300, #31899 ) ;
#44651 = ORIENTED_EDGE ( 'NONE', *, *, #28499, .F. ) ;
#44652 = CARTESIAN_POINT ( 'NONE',  ( 0.8560838555295158248, 27.08392101972004440, 38.29926965725714894 ) ) ;
#44653 = CARTESIAN_POINT ( 'NONE',  ( 0.5987334308729317378, -19.32301376689503769, 45.14625173294140126 ) ) ;
#44654 = ORIENTED_EDGE ( 'NONE', *, *, #17002, .T. ) ;
#44655 = CARTESIAN_POINT ( 'NONE',  ( 0.5832367798473397924, 44.35360901387671362, -18.07699868820141376 ) ) ;
#44656 = CARTESIAN_POINT ( 'NONE',  ( 0.1129192098497447394, 37.24220309526806005, 23.66368729500878842 ) ) ;
#44657 = FACE_OUTER_BOUND ( 'NONE', #43422, .T. ) ;
#44658 = CARTESIAN_POINT ( 'NONE',  ( 0.5839254288179557273, 12.48406597209104696, -46.24038938821421851 ) ) ;
#44659 = EDGE_CURVE ( 'NONE', #45260, #4680, #27196, .T. ) ;
#44660 = VERTEX_POINT ( 'NONE', #1372 ) ;
#44661 = FACE_OUTER_BOUND ( 'NONE', #45218, .T. ) ;
#44662 = CYLINDRICAL_SURFACE ( 'NONE', #50734, 2.649999999999992806 ) ;
#44663 = EDGE_CURVE ( 'NONE', #9163, #47555, #15509, .T. ) ;
#44664 = DIRECTION ( 'NONE',  ( -1.000000000000000000, -0.000000000000000000, -0.000000000000000000 ) ) ;
#44665 = DIRECTION ( 'NONE',  ( 0.9848077530122077983, 0.1736481776669316079, -1.387778780781445367E-17 ) ) ;
#44666 = EDGE_LOOP ( 'NONE', ( #41081, #60011, #56574, #58314 ) ) ;
#44667 = CARTESIAN_POINT ( 'NONE',  ( 0.7057020205115001055, -46.47981817772235047, 11.58334423512220823 ) ) ;
#44668 = CARTESIAN_POINT ( 'NONE',  ( 0.6846871229502932144, -5.395516691086876371, -47.60345020167356012 ) ) ;
#44669 = ORIENTED_EDGE ( 'NONE', *, *, #56975, .T. ) ;
#44670 = CARTESIAN_POINT ( 'NONE',  ( 3.238741278300276694, 24.69738534405263763, 35.19027457370187051 ) ) ;
#44671 = CARTESIAN_POINT ( 'NONE',  ( 4.303969348037246512, -43.57722561725945098, -20.38638383586165759 ) ) ;
#44672 = B_SPLINE_CURVE_WITH_KNOTS ( 'NONE', 3,
 ( #23105, #13098, #42844, #56289, #13715, #43152 ),
 .UNSPECIFIED., .F., .F.,
 ( 4, 2, 4 ),
 ( 0.000000000000000000, 0.0002293801035737121909, 0.0004587602071474243819 ),
 .UNSPECIFIED. ) ;
#44673 = ORIENTED_EDGE ( 'NONE', *, *, #45925, .T. ) ;
#44674 = CARTESIAN_POINT ( 'NONE',  ( 5.895596859100789899, 0.6684898708301673098, 20.10177366565161705 ) ) ;
#44675 = CARTESIAN_POINT ( 'NONE',  ( 0.8554163680231708922, 27.08908797599144336, 38.30648490452777821 ) ) ;
#44676 = B_SPLINE_CURVE_WITH_KNOTS ( 'NONE', 3,
 ( #2719, #50339, #36574, #7408, #60649, #8046 ),
 .UNSPECIFIED., .F., .F.,
 ( 4, 2, 4 ),
 ( 0.000000000000000000, 0.0002450742804987306525, 0.0004901485609974613050 ),
 .UNSPECIFIED. ) ;
#44677 = CARTESIAN_POINT ( 'NONE',  ( 4.553261556744873317, -9.994631851593151595, -42.77437199977056537 ) ) ;
#44678 = ADVANCED_FACE ( 'NONE', ( #20820 ), #18501, .F. ) ;
#44679 = CARTESIAN_POINT ( 'NONE',  ( 0.6009453534118439633, -41.87889766923471768, 23.67490308139332456 ) ) ;
#44680 = CARTESIAN_POINT ( 'NONE',  ( 0.2940135542859018680, -31.12576111067042106, 31.26383763988192754 ) ) ;
#44681 = CARTESIAN_POINT ( 'NONE',  ( 0.1368894036331279318, -41.13355190018849328, -15.96534478167740900 ) ) ;
#44682 = CARTESIAN_POINT ( 'NONE',  ( 0.1103878639767399555, -41.66755962011272629, -11.11454059769185854 ) ) ;
#44683 = CARTESIAN_POINT ( 'NONE',  ( 4.958415959904816539, 28.93810772186895619, -35.01128211448620675 ) ) ;
#44684 = VECTOR ( 'NONE', #50646, 1000.000000000000114 ) ;
#44685 = CARTESIAN_POINT ( 'NONE',  ( 0.9780106845699483298, 41.49170912070719908, 5.896551593775888556 ) ) ;
#44686 = CARTESIAN_POINT ( 'NONE',  ( 4.553261556744873317, 17.57396821678933563, -40.25785894628420181 ) ) ;
#44687 = ORIENTED_EDGE ( 'NONE', *, *, #39147, .F. ) ;
#44688 = CIRCLE ( 'NONE', #28653, 72.00000000000002842 ) ;
#44689 = VECTOR ( 'NONE', #5555, 1000.000000000000114 ) ;
#44690 = CARTESIAN_POINT ( 'NONE',  ( 0.7954196712028469562, -0.8690072546828989664, 48.09103417491924404 ) ) ;
#44691 = CARTESIAN_POINT ( 'NONE',  ( 0.8760168074887090262, -11.58706983520358769, 46.68716261866156003 ) ) ;
#44692 = CARTESIAN_POINT ( 'NONE',  ( 0.6021448801613057400, 22.48212995651498858, 43.65884757120048221 ) ) ;
#44693 = CARTESIAN_POINT ( 'NONE',  ( 3.238931869106853600, -38.98364358950757946, 18.12707634097755260 ) ) ;
#44694 = B_SPLINE_CURVE_WITH_KNOTS ( 'NONE', 3,
 ( #61597, #8996, #27181, #17790, #36917, #41924 ),
 .UNSPECIFIED., .F., .F.,
 ( 4, 2, 4 ),
 ( 0.000000000000000000, 0.0002291966416970798916, 0.0004583932833941597833 ),
 .UNSPECIFIED. ) ;
#44695 = CARTESIAN_POINT ( 'NONE',  ( 1.227938101723748288, -42.65467462194921922, 4.762198645644287076 ) ) ;
#44696 = CARTESIAN_POINT ( 'NONE',  ( 0.8560838555295223751, -14.76796170096679894, -44.52280473286144513 ) ) ;
#44697 = CARTESIAN_POINT ( 'NONE',  ( 2.281448460670572942, -7.562315317391437475, -47.37344300043620393 ) ) ;
#44698 = CARTESIAN_POINT ( 'NONE',  ( 3.238018933889920792, -10.11627964985454575, -8.778859744499381890 ) ) ;
#44699 = B_SPLINE_CURVE_WITH_KNOTS ( 'NONE', 3,
 ( #11572, #7772, #41325, #26896, #60381, #21577 ),
 .UNSPECIFIED., .F., .F.,
 ( 4, 2, 4 ),
 ( 1.138360651264128102E-17, 0.0002291978881530160788, 0.0004583957763060207734 ),
 .UNSPECIFIED. ) ;
#44700 = VECTOR ( 'NONE', #24252, 1000.000000000000000 ) ;
#44701 = CARTESIAN_POINT ( 'NONE',  ( 4.975801465491695552, -31.15993731089151808, 36.39623109580413285 ) ) ;
#44702 = EDGE_CURVE ( 'NONE', #36162, #22620, #50378, .T. ) ;
#44704 = EDGE_LOOP ( 'NONE', ( #23377, #39369, #59704, #47104 ) ) ;
#44703 = CARTESIAN_POINT ( 'NONE',  ( 0.6252788684277211795, 48.32745661275763638, 8.712133407822351572 ) ) ;
#44705 = ORIENTED_EDGE ( 'NONE', *, *, #8320, .T. ) ;
#44706 = CARTESIAN_POINT ( 'NONE',  ( 0.8751705887134423323, 0.8911681664088411114, -48.08707113907595243 ) ) ;
#44707 = FACE_BOUND ( 'NONE', #28148, .T. ) ;
#44708 = CARTESIAN_POINT ( 'NONE',  ( 0.3676999524040366896, -42.87209381266877983, -10.38913641457107673 ) ) ;
#44709 = ADVANCED_FACE ( 'NONE', ( #16124 ), #20917, .T. ) ;
#44710 = ORIENTED_EDGE ( 'NONE', *, *, #46344, .T. ) ;
#44711 = CARTESIAN_POINT ( 'NONE',  ( -6.016104459813371719, -16.31603998697576685, 9.426230926598584858 ) ) ;
#44712 = FACE_OUTER_BOUND ( 'NONE', #3466, .T. ) ;
#44713 = EDGE_CURVE ( 'NONE', #1001, #58998, #55575, .T. ) ;
#44714 = ORIENTED_EDGE ( 'NONE', *, *, #60835, .F. ) ;
#44715 = ORIENTED_EDGE ( 'NONE', *, *, #2945, .T. ) ;
#44716 = CARTESIAN_POINT ( 'NONE',  ( 2.500000000000000000, 2.357898499370431722, -2.818925648462311528E-15 ) ) ;
#44717 = EDGE_CURVE ( 'NONE', #56156, #22549, #54299, .T. ) ;
#44718 = EDGE_CURVE ( 'NONE', #50189, #33142, #28914, .T. ) ;
#44719 = CARTESIAN_POINT ( 'NONE',  ( 0.1100053167205930216, -11.33468317718527096, -41.60823192620004107 ) ) ;
#44720 = CARTESIAN_POINT ( 'NONE',  ( 4.303969348037258058, -16.39840148505124162, 45.22910199346969762 ) ) ;
#44721 = ORIENTED_EDGE ( 'NONE', *, *, #55849, .T. ) ;
#44722 = DIRECTION ( 'NONE',  ( 0.07500201931887537365, 0.3083113411842569040, -0.9483242135447431664 ) ) ;
#44723 = CARTESIAN_POINT ( 'NONE',  ( 0.5988103564986356764, -11.86435738293476128, 46.62176022926367835 ) ) ;
#44724 = EDGE_LOOP ( 'NONE', ( #7685, #16434, #14852, #45257 ) ) ;
#44725 = EDGE_CURVE ( 'NONE', #57409, #18802, #39204, .T. ) ;
#44726 = CARTESIAN_POINT ( 'NONE',  ( 0.5806925824938502512, 32.20670061096268455, -34.08739940358283604 ) ) ;
#44727 = AXIS2_PLACEMENT_3D ( 'NONE', #53500, #53202, #20937 ) ;
#44728 = ORIENTED_EDGE ( 'NONE', *, *, #54437, .F. ) ;
#44729 = EDGE_CURVE ( 'NONE', #30775, #2222, #17556, .T. ) ;
#44730 = CARTESIAN_POINT ( 'NONE',  ( 5.860006189529246790, 15.48781697582048089, 45.67886430272036336 ) ) ;
#44731 = TOROIDAL_SURFACE ( 'NONE', #36728, 5.100000000000000533, 0.1000000000000005884 ) ;
#44732 = ORIENTED_EDGE ( 'NONE', *, *, #45503, .T. ) ;
#44733 = AXIS2_PLACEMENT_3D ( 'NONE', #24200, #9796, #28285 ) ;
#44734 = FACE_OUTER_BOUND ( 'NONE', #49388, .T. ) ;
#44735 = CARTESIAN_POINT ( 'NONE',  ( 0.8557997880470690211, 19.17299735372009550, 43.90420959842187187 ) ) ;
#44736 = CARTESIAN_POINT ( 'NONE',  ( 0.5827357941260209451, 41.29633147056645726, -24.26189667804958461 ) ) ;
#44737 = CYLINDRICAL_SURFACE ( 'NONE', #24374, 6.728125000000022560 ) ;
#44738 = B_SPLINE_CURVE_WITH_KNOTS ( 'NONE', 3,
 ( #59863, #28203, #47319, #27592, #27284, #56694, #8788, #17903, #23820, #32927, #61087, #47026, #17585, #28502, #13504, #14133, #13824, #4365, #8169 ),
 .UNSPECIFIED., .F., .F.,
 ( 4, 3, 3, 3, 3, 3, 4 ),
 ( 1.734776414728241573E-18, 0.0002612768053151701911, 0.0003919133833142903834, 0.0005225499612322601030, 0.0006531865391693342238, 0.0008112755173415183395, 0.0009693688056799714889 ),
 .UNSPECIFIED. ) ;
#44739 = VERTEX_POINT ( 'NONE', #28505 ) ;
#44740 = CARTESIAN_POINT ( 'NONE',  ( 4.833616638992208614, 8.578242093415751057, -45.44786513329589894 ) ) ;
#44741 = CARTESIAN_POINT ( 'NONE',  ( 0.1156867017252034696, 39.80856523685828563, -19.03210290687776762 ) ) ;
#44742 = ORIENTED_EDGE ( 'NONE', *, *, #24738, .F. ) ;
#44743 = EDGE_CURVE ( 'NONE', #43892, #5799, #30173, .T. ) ;
#44744 = ORIENTED_EDGE ( 'NONE', *, *, #27977, .F. ) ;
#44745 = CARTESIAN_POINT ( 'NONE',  ( 0.8551540677456715978, 34.52115452272975205, -33.23105123575864184 ) ) ;
#44746 = ORIENTED_EDGE ( 'NONE', *, *, #56835, .T. ) ;
#44747 = CARTESIAN_POINT ( 'NONE',  ( 1.154321485836934169, 26.77578840293035611, 33.53917069757662972 ) ) ;
#44748 = CARTESIAN_POINT ( 'NONE',  ( 2.299652685299201860, 40.37736489803184980, 27.81995917950526476 ) ) ;
#44749 = B_SPLINE_CURVE_WITH_KNOTS ( 'NONE', 3,
 ( #30231, #1709, #29615, #19625 ),
 .UNSPECIFIED., .F., .F.,
 ( 4, 4 ),
 ( 2.177303646125455536E-17, 0.004559932413162186803 ),
 .UNSPECIFIED. ) ;
#44750 = FACE_OUTER_BOUND ( 'NONE', #24749, .T. ) ;
#44751 = ORIENTED_EDGE ( 'NONE', *, *, #52051, .T. ) ;
#44752 = CARTESIAN_POINT ( 'NONE',  ( 0.3676999524040366896, -38.02468164711607557, 22.36233818182511257 ) ) ;
#44753 = CARTESIAN_POINT ( 'NONE',  ( 0.5848930533535030563, 16.68483824254223791, 43.82795061610521969 ) ) ;
#44755 = VERTEX_POINT ( 'NONE', #4677 ) ;
#44754 = EDGE_CURVE ( 'NONE', #2809, #30005, #59350, .T. ) ;
#44756 =( BOUNDED_SURFACE ( )  B_SPLINE_SURFACE ( 3, 1, ( 
 ( #52189, #32807 ),
 ( #4254, #28702 ),
 ( #32488, #55965 ),
 ( #51885, #28090 ) ),
 .UNSPECIFIED., .F., .F., .F. ) 
 B_SPLINE_SURFACE_WITH_KNOTS ( ( 4, 4 ),
 ( 2, 2 ),
 ( 0.000000000000000000, 1.000000000000000000 ),
 ( 0.000000000000000000, 1.000000000000000000 ),
 .UNSPECIFIED. ) 
 GEOMETRIC_REPRESENTATION_ITEM ( )  RATIONAL_B_SPLINE_SURFACE ( (
 ( 1.000000000000000000, 1.000000000000000000),
 ( 0.9754377213608244057, 0.9999580625633939235),
 ( 0.9754377213608244057, 0.9999580625633939235),
 ( 1.000000000000000000, 1.000000000000000000) ) ) 
 REPRESENTATION_ITEM ( '' )  SURFACE ( )  );
#44757 = B_SPLINE_CURVE_WITH_KNOTS ( 'NONE', 3,
 ( #18560, #55833, #60836, #27032, #31736, #3508 ),
 .UNSPECIFIED., .F., .F.,
 ( 4, 2, 4 ),
 ( 2.059984127722458810E-18, 0.0002447193893791709549, 0.0004894387787583398498 ),
 .UNSPECIFIED. ) ;
#44758 = EDGE_LOOP ( 'NONE', ( #19856, #13841, #18362, #36333 ) ) ;
#44759 = CARTESIAN_POINT ( 'NONE',  ( 0.5839254288179546171, 18.24509008251478193, 44.28478521851629068 ) ) ;
#44760 = CARTESIAN_POINT ( 'NONE',  ( 1.479689385636123067, 30.48353183614671735, 31.81726154247598615 ) ) ;
#44762 = EDGE_CURVE ( 'NONE', #50474, #61383, #36950, .T. ) ;
#44761 = DIRECTION ( 'NONE',  ( -1.000000000000000000, -0.000000000000000000, -0.000000000000000000 ) ) ;
#44763 = CARTESIAN_POINT ( 'NONE',  ( 0.1102847568649952675, -5.720244683738307856, -42.74337176234127611 ) ) ;
#44764 = DIRECTION ( 'NONE',  ( 0.09722883295013598492, -0.8021136117729557036, 0.5892031125611089104 ) ) ;
#44765 = CARTESIAN_POINT ( 'NONE',  ( 0.5809828226811617480, -47.89273459658653564, -0.5448590168537535972 ) ) ;
#44766 = ORIENTED_EDGE ( 'NONE', *, *, #14661, .F. ) ;
#44767 = CARTESIAN_POINT ( 'NONE',  ( 0.9754292580325143458, -40.94879473734659570, -8.917604861321258625 ) ) ;
#44768 = CARTESIAN_POINT ( 'NONE',  ( 0.8751705887134423323, -46.67919521768896374, 11.58504748649118810 ) ) ;
#44769 = ORIENTED_EDGE ( 'NONE', *, *, #33550, .F. ) ;
#44770 = CARTESIAN_POINT ( 'NONE',  ( 0.6001305935487315502, -28.87057754790910735, -38.48510059944037920 ) ) ;
#44771 = CARTESIAN_POINT ( 'NONE',  ( 0.6024113833632039894, -19.67861259707041910, -44.99215570913765561 ) ) ;
#44772 = CARTESIAN_POINT ( 'NONE',  ( 0.5817217712918331118, 45.10732654355952320, 12.82825187237387610 ) ) ;
#44773 = B_SPLINE_CURVE_WITH_KNOTS ( 'NONE', 3,
 ( #29920, #1391, #57790, #5476, #20531, #58709, #20838, #14924, #39978, #34030, #53102, #31463, #40899, #55560, #21448, #21140 ),
 .UNSPECIFIED., .F., .F.,
 ( 4, 3, 3, 3, 3, 4 ),
 ( 1.551621725782133898E-17, 0.0002732102107931891864, 0.0004098135523333867381, 0.0005464168938825064064, 0.0008195847345945496236, 0.001092771384553108734 ),
 .UNSPECIFIED. ) ;
#44774 = DIRECTION ( 'NONE',  ( 1.000000000000000000, -0.000000000000000000, -0.000000000000000000 ) ) ;
#44775 = CARTESIAN_POINT ( 'NONE',  ( 0.8560838555295223751, 39.88643293834682879, -24.68694597426934223 ) ) ;
#44776 = B_SPLINE_CURVE_WITH_KNOTS ( 'NONE', 3,
 ( #45646, #8028, #55940, #17745 ),
 .UNSPECIFIED., .F., .F.,
 ( 4, 4 ),
 ( 0.000000000000000000, 0.004446090762761359047 ),
 .UNSPECIFIED. ) ;
#44777 = CARTESIAN_POINT ( 'NONE',  ( 5.960721111146673579, -19.82454228767749527, 5.318514366754590661 ) ) ;
#44778 =( BOUNDED_SURFACE ( )  B_SPLINE_SURFACE ( 3, 1, ( 
 ( #42625, #22894 ),
 ( #23196, #19134 ),
 ( #12893, #18819 ),
 ( #17894, #51373 ) ),
 .UNSPECIFIED., .F., .F., .F. ) 
 B_SPLINE_SURFACE_WITH_KNOTS ( ( 4, 4 ),
 ( 2, 2 ),
 ( 0.000000000000000000, 1.000000000000000000 ),
 ( 0.000000000000000000, 1.000000000000000000 ),
 .UNSPECIFIED. ) 
 GEOMETRIC_REPRESENTATION_ITEM ( )  RATIONAL_B_SPLINE_SURFACE ( (
 ( 1.000000000000000000, 1.000000000000000000),
 ( 0.7269869731126821222, 0.9931720237060910339),
 ( 0.7269869731126821222, 0.9931720237060910339),
 ( 1.000000000000000000, 1.000000000000000000) ) ) 
 REPRESENTATION_ITEM ( '' )  SURFACE ( )  );
#44779 = CARTESIAN_POINT ( 'NONE',  ( 0.1157991065609915576, 20.48126240941084930, -39.08273603081740077 ) ) ;
#44780 = CARTESIAN_POINT ( 'NONE',  ( 0.5980894510889457338, -46.28687279963700973, 13.12879507229208009 ) ) ;
#44781 = CIRCLE ( 'NONE', #58716, 42.92674063221959813 ) ;
#44782 = CARTESIAN_POINT ( 'NONE',  ( 0.5786265663353196143, 47.89572889566445468, 0.7221568112308146548 ) ) ;
#44783 = CARTESIAN_POINT ( 'NONE',  ( -3.345653888883671989, 2.687187980154694511, -0.1391502195351393412 ) ) ;
#44784 = CIRCLE ( 'NONE', #46790, 47.09074272231896430 ) ;
#44785 = VECTOR ( 'NONE', #27606, 1000.000000000000000 ) ;
#44786 = SURFACE_STYLE_USAGE ( .BOTH. , #36308 ) ;
#44787 = CARTESIAN_POINT ( 'NONE',  ( 0.2940135542859017570, -17.11870284647595852, 40.65944615394406014 ) ) ;
#44788 = ADVANCED_FACE ( 'NONE', ( #18510 ), #14126, .F. ) ;
#44789 = CARTESIAN_POINT ( 'NONE',  ( 0.1139756605157203756, -6.649460940698757483, 43.62040679421897238 ) ) ;
#44790 = CARTESIAN_POINT ( 'NONE',  ( 5.958863334805807099, -20.52565293643016275, -0.001220270596097471809 ) ) ;
#44791 = FACE_OUTER_BOUND ( 'NONE', #51935, .T. ) ;
#44792 = ADVANCED_FACE ( 'NONE', ( #27286 ), #7304, .F. ) ;
#44793 = APPLICATION_CONTEXT ( 'automotive_design' ) ;
#44794 = ORIENTED_EDGE ( 'NONE', *, *, #50182, .T. ) ;
#44795 =( NAMED_UNIT ( * ) SI_UNIT ( $, .STERADIAN. ) SOLID_ANGLE_UNIT ( ) );
#44796 = EDGE_CURVE ( 'NONE', #22554, #4396, #48176, .T. ) ;
#44797 = EDGE_CURVE ( 'NONE', #41488, #35221, #41423, .T. ) ;
#44798 = CARTESIAN_POINT ( 'NONE',  ( 0.1103878639767399555, 43.12442673975421314, -0.04853618198075116547 ) ) ;
#44799 = CARTESIAN_POINT ( 'NONE',  ( 5.860006189529246790, -47.30964106197865249, 9.393028332204574227 ) ) ;
#44800 = CARTESIAN_POINT ( 'NONE',  ( 0.5848930533535030563, 32.47085631013434437, -33.83661586025067436 ) ) ;
#44801 = CARTESIAN_POINT ( 'NONE',  ( 1.231276596079881935, 35.62927148397020005, 22.08691432816306133 ) ) ;
#44802 = ADVANCED_FACE ( 'NONE', ( #4367 ), #59276, .F. ) ;
#44803 = ORIENTED_EDGE ( 'NONE', *, *, #14169, .T. ) ;
#44804 = B_SPLINE_CURVE_WITH_KNOTS ( 'NONE', 3,
 ( #3101, #16926, #3400, #22539 ),
 .UNSPECIFIED., .F., .F.,
 ( 4, 4 ),
 ( 0.000000000000000000, 0.005014147105413706458 ),
 .UNSPECIFIED. ) ;
#44805 = LINE ( 'NONE', #15971, #56296 ) ;
#44806 = CARTESIAN_POINT ( 'NONE',  ( 0.5997462898726536595, 28.52220283460682282, -39.97543715340528081 ) ) ;
#44807 = CARTESIAN_POINT ( 'NONE',  ( 4.694002226626921015, 23.92658369670245833, -38.80468224391004384 ) ) ;
#44808 = VERTEX_POINT ( 'NONE', #18207 ) ;
#44809 = CARTESIAN_POINT ( 'NONE',  ( 4.956445790443989807, 42.27038699792205279, 20.75457619864928205 ) ) ;
#44810 = EDGE_CURVE ( 'NONE', #59514, #59308, #16002, .T. ) ;
#44811 = CARTESIAN_POINT ( 'NONE',  ( 0.3622758884714600280, 41.42293301073608802, 11.95365414648511582 ) ) ;
#44812 = ORIENTED_EDGE ( 'NONE', *, *, #28427, .T. ) ;
#44813 = CARTESIAN_POINT ( 'NONE',  ( 0.9754292580325127915, -26.60990431517644339, -32.37654180484936006 ) ) ;
#44814 = ORIENTED_EDGE ( 'NONE', *, *, #40193, .F. ) ;
#44815 = CARTESIAN_POINT ( 'NONE',  ( -6.077587904424778920, 9.976910903712887801, 16.46988980574263906 ) ) ;
#44816 = ORIENTED_EDGE ( 'NONE', *, *, #28422, .T. ) ;
#44817 = CARTESIAN_POINT ( 'NONE',  ( 0.8560838555295158248, -0.6537497281619772949, -46.90357604036880446 ) ) ;
#44818 = CARTESIAN_POINT ( 'NONE',  ( 0.8744876279028306332, -49.08725279547490317, 0.8897546699139438076 ) ) ;
#44819 = VERTEX_POINT ( 'NONE', #52005 ) ;
#44820 = EDGE_LOOP ( 'NONE', ( #51518, #37412 ) ) ;
#44821 = CARTESIAN_POINT ( 'NONE',  ( 0.9762797500689124330, -34.83496347773955648, 23.29914386174426255 ) ) ;
#44822 = CARTESIAN_POINT ( 'NONE',  ( 0.5850706913938534814, -12.22095376872069394, 46.31100969101484566 ) ) ;
#44823 = ORIENTED_EDGE ( 'NONE', *, *, #30571, .T. ) ;
#44824 = ORIENTED_EDGE ( 'NONE', *, *, #4918, .T. ) ;
#44825 = FACE_OUTER_BOUND ( 'NONE', #27550, .T. ) ;
#44827 = FACE_OUTER_BOUND ( 'NONE', #13976, .T. ) ;
#44826 = B_SPLINE_CURVE_WITH_KNOTS ( 'NONE', 3,
 ( #45397, #51291, #61001, #18108 ),
 .UNSPECIFIED., .F., .F.,
 ( 4, 4 ),
 ( 4.336808689942017736E-19, 0.004041751736740985604 ),
 .UNSPECIFIED. ) ;
#44828 = CARTESIAN_POINT ( 'NONE',  ( 0.7413678028165011646, -35.88962831636828099, -25.62070785679388152 ) ) ;
#44829 = CIRCLE ( 'NONE', #52788, 0.7500000000000015543 ) ;
#44830 = CARTESIAN_POINT ( 'NONE',  ( 4.956445790444005794, -40.23882117934059011, -24.46171131046819625 ) ) ;
#44831 = FACE_OUTER_BOUND ( 'NONE', #14058, .T. ) ;
#44832 = ORIENTED_EDGE ( 'NONE', *, *, #59974, .T. ) ;
#44833 = CARTESIAN_POINT ( 'NONE',  ( 0.8753041380234530822, 46.87455897190329068, 14.62580080072681099 ) ) ;
#44834 = FACE_OUTER_BOUND ( 'NONE', #6363, .T. ) ;
#44835 = ORIENTED_EDGE ( 'NONE', *, *, #17678, .T. ) ;
#44836 = DIRECTION ( 'NONE',  ( -1.000000000000000000, -0.000000000000000000, -0.000000000000000000 ) ) ;
#44837 = ORIENTED_EDGE ( 'NONE', *, *, #58896, .T. ) ;
#44838 = LINE ( 'NONE', #21313, #1493 ) ;
#44839 = EDGE_CURVE ( 'NONE', #59128, #14410, #9097, .T. ) ;
#44840 = CARTESIAN_POINT ( 'NONE',  ( 0.5835871038041848813, -44.34580925781567373, 15.25397175069270261 ) ) ;
#44841 = ORIENTED_EDGE ( 'NONE', *, *, #19420, .T. ) ;
#44842 = CARTESIAN_POINT ( 'NONE',  ( -6.015611763856276717, -4.870987357968304288, 18.20278301740935234 ) ) ;
#44843 = FACE_OUTER_BOUND ( 'NONE', #26907, .T. ) ;
#44844 = DIRECTION ( 'NONE',  ( 0.000000000000000000, 0.8660254037844380415, -0.5000000000000009992 ) ) ;
#44845 = CARTESIAN_POINT ( 'NONE',  ( 4.975801465491694664, -15.94009207553080643, 45.18341283946430309 ) ) ;
#44846 = AXIS2_PLACEMENT_3D ( 'NONE', #22019, #41144, #51115 ) ;
#44847 = EDGE_LOOP ( 'NONE', ( #33923, #43517, #9071, #2085 ) ) ;
#44848 = DIRECTION ( 'NONE',  ( -1.000000000000000000, -0.000000000000000000, -0.000000000000000000 ) ) ;
#44849 = ORIENTED_EDGE ( 'NONE', *, *, #19122, .F. ) ;
#44850 = CARTESIAN_POINT ( 'NONE',  ( -6.203732170862584994, -1.182048853166489222, 5.744326400484686099E-14 ) ) ;
#44851 = CARTESIAN_POINT ( 'NONE',  ( 2.339468227445713921, 3.268109542640642573, -5.600000000000002309 ) ) ;
#44852 = AXIS2_PLACEMENT_3D ( 'NONE', #3263, #36830, #36512 ) ;
#44853 = CARTESIAN_POINT ( 'NONE',  ( 4.962356264823608143, 26.83784316460287300, 32.41860225448540689 ) ) ;
#44854 = CARTESIAN_POINT ( 'NONE',  ( 2.648799415243696664, -0.1860685961553510681, -49.03552632293368418 ) ) ;
#44855 = AXIS2_PLACEMENT_3D ( 'NONE', #265, #59923, #52592 ) ;
#44856 = CARTESIAN_POINT ( 'NONE',  ( 0.6000166863083090663, -47.63401213562553949, -11.95091500980295507 ) ) ;
#44857 = DIRECTION ( 'NONE',  ( 0.000000000000000000, 1.000000000000000000, 0.000000000000000000 ) ) ;
#44858 = CARTESIAN_POINT ( 'NONE',  ( 2.618530812446111078, 41.14519205294217130, -22.73323470438608851 ) ) ;
#44859 = CARTESIAN_POINT ( 'NONE',  ( 0.5980271706414711508, 32.49685829779699731, 36.82395203688170682 ) ) ;
#44860 = CARTESIAN_POINT ( 'NONE',  ( 5.981074661064941900, -17.77058762078870657, -10.26976685693816727 ) ) ;
#44861 = LINE ( 'NONE', #26040, #16695 ) ;
#44862 = ADVANCED_FACE ( 'NONE', ( #19437 ), #5947, .T. ) ;
#44863 = EDGE_CURVE ( 'NONE', #26211, #24826, #30969, .T. ) ;
#44864 = DIRECTION ( 'NONE',  ( 0.000000000000000000, 0.000000000000000000, 1.000000000000000000 ) ) ;
#44865 = CARTESIAN_POINT ( 'NONE',  ( 0.6026777506516368677, -45.45291013477714159, 18.58976468159541895 ) ) ;
#44866 = CIRCLE ( 'NONE', #33858, 48.91267123290010943 ) ;
#44867 = ORIENTED_EDGE ( 'NONE', *, *, #13395, .F. ) ;
#44868 = EDGE_CURVE ( 'NONE', #61570, #50538, #27972, .T. ) ;
#44869 = AXIS2_PLACEMENT_3D ( 'NONE', #16562, #12191, #35690 ) ;
#44870 = CARTESIAN_POINT ( 'NONE',  ( 0.7413678028165010536, -2.345741242198491339, -44.03389137692570898 ) ) ;
#44871 = DIRECTION ( 'NONE',  ( 0.000000000000000000, 0.000000000000000000, 1.000000000000000000 ) ) ;
#44872 = CARTESIAN_POINT ( 'NONE',  ( 4.553261556744875094, -41.75933753256810377, 13.62707946203756393 ) ) ;
#44873 = EDGE_CURVE ( 'NONE', #43281, #37898, #21199, .T. ) ;
#44874 = ORIENTED_EDGE ( 'NONE', *, *, #59864, .T. ) ;
#44875 = CARTESIAN_POINT ( 'NONE',  ( 0.7954190325252783467, 47.79303692714234586, 5.415566973723409561 ) ) ;
#44876 = CARTESIAN_POINT ( 'NONE',  ( 2.299652685299201860, 26.98654338430133848, 40.93907914237171752 ) ) ;
#44877 = B_SPLINE_CURVE_WITH_KNOTS ( 'NONE', 3,
 ( #15246, #25548, #44683, #53426 ),
 .UNSPECIFIED., .F., .F.,
 ( 4, 4 ),
 ( 0.000000000000000000, 0.005004948556313815709 ),
 .UNSPECIFIED. ) ;
#44878 = DIRECTION ( 'NONE',  ( -1.000000000000000000, -0.000000000000000000, -0.000000000000000000 ) ) ;
#44879 = ORIENTED_EDGE ( 'NONE', *, *, #28016, .F. ) ;
#44880 = CARTESIAN_POINT ( 'NONE',  ( 0.1365634738349403854, 3.602546085856351610, 43.97595117018536826 ) ) ;
#44881 = SHAPE_REPRESENTATION ( 'BR-540', ( #57899, #19889, #9903, #41941, #47920, #8865, #14928, #36936, #27875, #30905, #52907, #5836, #53874, #49916, #39935, #26894, #33922, #22918, #34912, #61872, #4863, #856, #43919, #24882, #45918, #16893, #3883, #60903, #51872, #42923 ), #11941 ) ;
#44882 = CARTESIAN_POINT ( 'NONE',  ( 5.960221823109900008, 16.28072933292548186, -12.49951306783072624 ) ) ;
#44883 = VERTEX_POINT ( 'NONE', #48252 ) ;
#44884 = EDGE_CURVE ( 'NONE', #6088, #7385, #14951, .T. ) ;
#44885 = CARTESIAN_POINT ( 'NONE',  ( 0.5850706913938533704, -47.50996714391786924, 6.071602062250445186 ) ) ;
#44886 = VECTOR ( 'NONE', #14868, 1000.000000000000000 ) ;
#44887 = ORIENTED_EDGE ( 'NONE', *, *, #26645, .T. ) ;
#44888 = ORIENTED_EDGE ( 'NONE', *, *, #4139, .T. ) ;
#44889 = CARTESIAN_POINT ( 'NONE',  ( 4.962356264823602814, -15.53171314616136200, -39.11523340858015274 ) ) ;
#44891 = ORIENTED_EDGE ( 'NONE', *, *, #33249, .T. ) ;
#44890 = ADVANCED_FACE ( 'NONE', ( #20063 ), #5296, .F. ) ;
#44892 = DIRECTION ( 'NONE',  ( 1.000000000000000000, 0.000000000000000000, 0.000000000000000000 ) ) ;
#44893 = CARTESIAN_POINT ( 'NONE',  ( 1.129531546211735016, 6.886005254585696675E-16, 5.612499999999999822 ) ) ;
#44894 = VERTEX_POINT ( 'NONE', #38872 ) ;
#44896 = B_SPLINE_CURVE_WITH_KNOTS ( 'NONE', 3,
 ( #1231, #30057, #6220, #54778 ),
 .UNSPECIFIED., .F., .F.,
 ( 4, 4 ),
 ( 0.000000000000000000, 0.005004948556313797495 ),
 .UNSPECIFIED. ) ;
#44895 = CARTESIAN_POINT ( 'NONE',  ( 0.3676999524040323597, -44.10520818713899871, -0.8253448321555690859 ) ) ;
#44897 = COLOUR_RGB ( '', 0.31764706, 0.68627451, 0.89019608) ;
#44898 = CARTESIAN_POINT ( 'NONE',  ( -2.739355103387248747, -9.100462108390502181, 11.83339158334438324 ) ) ;
#44899 = VERTEX_POINT ( 'NONE', #5599 ) ;
#44900 = CARTESIAN_POINT ( 'NONE',  ( 0.1129192098497447394, 43.21532672376840623, -8.909956450123800664 ) ) ;
#44901 = CARTESIAN_POINT ( 'NONE',  ( -6.001507490154111224, -17.40350523682689854, -7.225628667346763123 ) ) ;
#44902 = CARTESIAN_POINT ( 'NONE',  ( 0.5850706913938533704, 33.99603398296638090, -33.73916126769415769 ) ) ;
#44903 = VECTOR ( 'NONE', #21798, 1000.000000000000000 ) ;
#44904 = LINE ( 'NONE', #21065, #11632 ) ;
#44905 = VERTEX_POINT ( 'NONE', #43566 ) ;
#44906 = VERTEX_POINT ( 'NONE', #610 ) ;
#44907 = CARTESIAN_POINT ( 'NONE',  ( 0.1103878639767399278, 41.66755962011264103, 11.11454059769214808 ) ) ;
#44908 = CARTESIAN_POINT ( 'NONE',  ( -6.077587904424778920, -18.90214787454603851, -3.674891443665424973 ) ) ;
#44909 = EDGE_CURVE ( 'NONE', #50007, #21001, #42203, .T. ) ;
#44910 = CARTESIAN_POINT ( 'NONE',  ( 3.727782113643637096, 13.15907417876901242, -41.94778352504015828 ) ) ;
#44911 = ORIENTED_EDGE ( 'NONE', *, *, #41131, .T. ) ;
#44912 = CARTESIAN_POINT ( 'NONE',  ( 3.783198216974394068, -24.80909581868418101, -35.16829104054195909 ) ) ;
#44913 = FACE_OUTER_BOUND ( 'NONE', #56705, .T. ) ;
#44914 = CARTESIAN_POINT ( 'NONE',  ( 0.6029303876144825880, -41.59667219751865730, -24.16699908817946962 ) ) ;
#44915 = AXIS2_PLACEMENT_3D ( 'NONE', #26416, #31432, #40552 ) ;
#44916 = ORIENTED_EDGE ( 'NONE', *, *, #16319, .F. ) ;
#44917 = VERTEX_POINT ( 'NONE', #9716 ) ;
#44918 = CARTESIAN_POINT ( 'NONE',  ( 5.981074661064941900, -19.82308078259087480, -5.320466518160866798 ) ) ;
#44919 = CARTESIAN_POINT ( 'NONE',  ( 0.8560838555295223751, -20.57050347530454104, -42.15717282805163535 ) ) ;
#44920 = CARTESIAN_POINT ( 'NONE',  ( 4.956445790444026223, 7.299064093731650438, -46.52162629890785439 ) ) ;
#44921 = CARTESIAN_POINT ( 'NONE',  ( 0.2230388203127610103, -43.11276071378622277, 0.7599700551098830248 ) ) ;
#44922 = CARTESIAN_POINT ( 'NONE',  ( 4.553261556744875094, -41.61700166486733110, -14.05577241741153216 ) ) ;
#44923 = CARTESIAN_POINT ( 'NONE',  ( 4.226256110419179812, -14.78729662703991465, -41.37829272035182981 ) ) ;
#44924 = CARTESIAN_POINT ( 'NONE',  ( 5.895596859100789899, 12.98270243688433645, -15.36156309259591701 ) ) ;
#44925 = CARTESIAN_POINT ( 'NONE',  ( 1.139999999999998570, 0.000000000000000000, -6.866799999999992465 ) ) ;
#44926 = CARTESIAN_POINT ( 'NONE',  ( 3.407937589446178528, 13.51415833181191317, -2.242416846335461234 ) ) ;
#44927 = CONICAL_SURFACE ( 'NONE', #50922, 42.92674063221959813, 1.485477209440487556 ) ;
#44928 = CARTESIAN_POINT ( 'NONE',  ( 1.000110580585051867, 15.67476820051338571, -38.86797042079857079 ) ) ;
#44929 = CARTESIAN_POINT ( 'NONE',  ( 0.5997462898726536595, 41.43917033312096265, 26.35046094941977302 ) ) ;
#44930 = CARTESIAN_POINT ( 'NONE',  ( 0.7048096507298635682, 44.11842270945974320, -19.18768066167077180 ) ) ;
#44931 = CARTESIAN_POINT ( 'NONE',  ( 1.296416391601052709, 41.46295787682408474, -14.93755328629393198 ) ) ;
#44932 = CARTESIAN_POINT ( 'NONE',  ( 0.6031356219577718170, -34.07882816221597722, -33.95537057546173543 ) ) ;
#44933 = CARTESIAN_POINT ( 'NONE',  ( 1.227938101723756947, 4.762198645645047357, -42.65467462194912684 ) ) ;
#44934 = FACE_OUTER_BOUND ( 'NONE', #2056, .T. ) ;
#44935 = CARTESIAN_POINT ( 'NONE',  ( 5.974727161628369032, -18.95664195401511876, -7.868887636447555067 ) ) ;
#44936 = B_SPLINE_CURVE_WITH_KNOTS ( 'NONE', 3,
 ( #52513, #4575, #23715, #1122, #53725, #35599 ),
 .UNSPECIFIED., .F., .F.,
 ( 4, 2, 4 ),
 ( 7.007167689862070887E-18, 0.0002448709889506569398, 0.0004897419779013069407 ),
 .UNSPECIFIED. ) ;
#44937 = EDGE_CURVE ( 'NONE', #26085, #10602, #1763, .T. ) ;
#44938 = CARTESIAN_POINT ( 'NONE',  ( 3.680974057930773924, 45.82782223000855026, 14.19449211152953438 ) ) ;
#44939 = CARTESIAN_POINT ( 'NONE',  ( 0.6008122571543326185, 48.97685995893719024, -3.580745596656180307 ) ) ;
#44940 = VERTEX_POINT ( 'NONE', #52619 ) ;
#44941 = ORIENTED_EDGE ( 'NONE', *, *, #47160, .F. ) ;
#44942 = FACE_BOUND ( 'NONE', #50177, .T. ) ;
#44943 = CARTESIAN_POINT ( 'NONE',  ( 0.5804410086790514622, -8.338934868871049844, 46.15172821366630984 ) ) ;
#44944 = FACE_OUTER_BOUND ( 'NONE', #43099, .T. ) ;
#44945 = EDGE_CURVE ( 'NONE', #25014, #29362, #24188, .T. ) ;
#44946 = VERTEX_POINT ( 'NONE', #1531 ) ;
#44947 = ORIENTED_EDGE ( 'NONE', *, *, #54835, .F. ) ;
#44948 = CARTESIAN_POINT ( 'NONE',  ( 0.9754292589017239390, -23.03905100505517822, -35.00756483507158379 ) ) ;
#44949 = CARTESIAN_POINT ( 'NONE',  ( 4.553261556744873317, 1.182159483579998449, -43.91061448874312845 ) ) ;
#44950 = CARTESIAN_POINT ( 'NONE',  ( 0.1081432562775997974, -37.55692207416040418, 21.19449538864492766 ) ) ;
#44951 =( BOUNDED_SURFACE ( )  B_SPLINE_SURFACE ( 3, 1, ( 
 ( #53030, #11066 ),
 ( #30148, #24224 ),
 ( #53945, #1023 ),
 ( #29229, #43359 ) ),
 .UNSPECIFIED., .F., .F., .F. ) 
 B_SPLINE_SURFACE_WITH_KNOTS ( ( 4, 4 ),
 ( 2, 2 ),
 ( 0.000000000000000000, 1.000000000000000000 ),
 ( 0.000000000000000000, 1.000000000000000000 ),
 .UNSPECIFIED. ) 
 GEOMETRIC_REPRESENTATION_ITEM ( )  RATIONAL_B_SPLINE_SURFACE ( (
 ( 1.000000000000000000, 1.000000000000000000),
 ( 0.9751682680413298332, 0.9999560080971552356),
 ( 0.9751682680413298332, 0.9999560080971552356),
 ( 1.000000000000000000, 1.000000000000000000) ) ) 
 REPRESENTATION_ITEM ( '' )  SURFACE ( )  );
#44952 = ORIENTED_EDGE ( 'NONE', *, *, #15553, .T. ) ;
#44953 = VERTEX_POINT ( 'NONE', #5910 ) ;
#44954 = CARTESIAN_POINT ( 'NONE',  ( 0.000000000000000000, 0.000000000000000000, 0.000000000000000000 ) ) ;
#44955 = AXIS2_PLACEMENT_3D ( 'NONE', #6205, #35700, #49771 ) ;
#44956 = CIRCLE ( 'NONE', #45945, 43.92652462719577500 ) ;
#44957 = CARTESIAN_POINT ( 'NONE',  ( 1.231276596079887931, 36.49189576017872128, 20.63051901543724043 ) ) ;
#44958 = CARTESIAN_POINT ( 'NONE',  ( 4.962356264823593044, 27.50309822711036034, 31.85616401534038644 ) ) ;
#44959 = EDGE_LOOP ( 'NONE', ( #49429, #14765, #30273, #10043 ) ) ;
#44960 = EDGE_CURVE ( 'NONE', #34245, #19440, #48857, .T. ) ;
#44961 = CARTESIAN_POINT ( 'NONE',  ( 0.9787464366903565471, -41.03323141156885612, -8.521027685385261563 ) ) ;
#44962 = CARTESIAN_POINT ( 'NONE',  ( 0.6064782688330873084, -29.73181431155118659, -36.26780478829964238 ) ) ;
#44963 = CARTESIAN_POINT ( 'NONE',  ( -4.915099999999999802, 12.80000000000000071, 0.000000000000000000 ) ) ;
#44964 = ORIENTED_EDGE ( 'NONE', *, *, #12647, .T. ) ;
#44965 = ORIENTED_EDGE ( 'NONE', *, *, #1698, .T. ) ;
#44966 = CARTESIAN_POINT ( 'NONE',  ( 0.5797568599927143129, 27.30868314757112003, 38.12428534958486637 ) ) ;
#44967 = FACE_OUTER_BOUND ( 'NONE', #53466, .T. ) ;
#44968 = VECTOR ( 'NONE', #1190, 1000.000000000000000 ) ;
#44969 = ORIENTED_EDGE ( 'NONE', *, *, #54444, .T. ) ;
#44970 = CARTESIAN_POINT ( 'NONE',  ( 5.880360259849752858, 45.44137230084881907, -15.37531919565188865 ) ) ;
#44971 = CARTESIAN_POINT ( 'NONE',  ( 0.6029443199889047422, -7.837513239273773635, 48.47794372782958305 ) ) ;
#44972 = CARTESIAN_POINT ( 'NONE',  ( 0.8554163680231708922, -20.57434774096721952, 42.16517150618003029 ) ) ;
#44973 = CARTESIAN_POINT ( 'NONE',  ( 0.5832367798473380160, 12.65931911325669113, -46.19266341874884318 ) ) ;
#44974 = B_SPLINE_CURVE_WITH_KNOTS ( 'NONE', 3,
 ( #5759, #59323, #10189, #29286, #5457, #43731 ),
 .UNSPECIFIED., .F., .F.,
 ( 4, 2, 4 ),
 ( 1.738108305489988542E-18, 0.0002291966416970807861, 0.0004583932833941598375 ),
 .UNSPECIFIED. ) ;
#44975 = ORIENTED_EDGE ( 'NONE', *, *, #6004, .T. ) ;
#44976 = LINE ( 'NONE', #55250, #20878 ) ;
#44977 = LINE ( 'NONE', #39659, #19771 ) ;
#44978 = EDGE_CURVE ( 'NONE', #19158, #5605, #21976, .T. ) ;
#44979 = CARTESIAN_POINT ( 'NONE',  ( 0.9730545539215883499, -21.89037132892409687, -36.90443313492354349 ) ) ;
#44980 = EDGE_CURVE ( 'NONE', #50421, #59514, #32417, .T. ) ;
#44981 = VERTEX_POINT ( 'NONE', #35713 ) ;
#44982 = CARTESIAN_POINT ( 'NONE',  ( 5.959547316686252039, -10.26589671991375674, 17.77392908783916070 ) ) ;
#44983 = CARTESIAN_POINT ( 'NONE',  ( 4.833616638992208614, 46.17873762321149655, 2.572717262758150270 ) ) ;
#44984 = ORIENTED_EDGE ( 'NONE', *, *, #6121, .T. ) ;
#44985 = CARTESIAN_POINT ( 'NONE',  ( 4.958415959904816539, 13.93965400761555706, 43.23066041561943962 ) ) ;
#44986 = CARTESIAN_POINT ( 'NONE',  ( 4.553261556744873317, -9.554252317234828595, 42.87488575474283437 ) ) ;
#44987 = B_SPLINE_CURVE_WITH_KNOTS ( 'NONE', 3,
 ( #13222, #47345, #12080, #37658 ),
 .UNSPECIFIED., .F., .F.,
 ( 4, 4 ),
 ( 0.000000000000000000, 0.005014147105413702989 ),
 .UNSPECIFIED. ) ;
#44988 = VERTEX_POINT ( 'NONE', #54147 ) ;
#44989 = CARTESIAN_POINT ( 'NONE',  ( 5.901764892641288895, -41.01701952799378859, 26.75061824481547035 ) ) ;
#44990 = CARTESIAN_POINT ( 'NONE',  ( 0.5998501479064708430, 37.84527566984816360, 29.69975237324626605 ) ) ;
#44991 = CARTESIAN_POINT ( 'NONE',  ( 0.2885700199627511675, 25.60460887553377773, -34.69058524452987768 ) ) ;
#44992 = EDGE_CURVE ( 'NONE', #47400, #51041, #7151, .T. ) ;
#44993 = CARTESIAN_POINT ( 'NONE',  ( 1.231276596079881047, -23.26513148155264332, 34.87134107206281186 ) ) ;
#44994 = CARTESIAN_POINT ( 'NONE',  ( 1.112077966505211846, 21.31368232310758515, 38.58441746298893804 ) ) ;
#44995 = CARTESIAN_POINT ( 'NONE',  ( -6.001507490154111224, 18.19774963328908157, 4.892199142591368677 ) ) ;
#44996 = CARTESIAN_POINT ( 'NONE',  ( 0.9730545539215883499, 34.34678117142591702, -25.71816799638743944 ) ) ;
#44997 = CARTESIAN_POINT ( 'NONE',  ( 0.1102847568649952675, -41.67876919128915603, -11.07236323260738686 ) ) ;
#44998 = EDGE_CURVE ( 'NONE', #46130, #28495, #18217, .T. ) ;
#44999 = DIRECTION ( 'NONE',  ( 0.07500201931887538753, -0.3457612750068233542, -0.9353201792989109808 ) ) ;
#45000 = CARTESIAN_POINT ( 'NONE',  ( -6.016761891674564211, 2.462934516563804355, 18.68153697670642543 ) ) ;
#45001 = DIRECTION ( 'NONE',  ( 0.000000000000000000, 0.000000000000000000, 1.000000000000000000 ) ) ;
#45002 = ORIENTED_EDGE ( 'NONE', *, *, #37344, .F. ) ;
#45003 = AXIS2_PLACEMENT_3D ( 'NONE', #27062, #7628, #51783 ) ;
#45004 = CARTESIAN_POINT ( 'NONE',  ( 2.526552050251864134, 42.43615142762125458, 6.809858322089185734 ) ) ;
#45005 = CARTESIAN_POINT ( 'NONE',  ( 4.975610109902397937, -4.123593823331679786, -48.73854102369041641 ) ) ;
#45006 = CARTESIAN_POINT ( 'NONE',  ( -4.000000000000000000, 0.000000000000000000, -5.599999999999999645 ) ) ;
#45007 = CARTESIAN_POINT ( 'NONE',  ( 0.1154773475650540115, 44.02163660921988964, -3.006516304947005391 ) ) ;
#45008 = DIRECTION ( 'NONE',  ( -1.000000000000000000, -0.000000000000000000, -0.000000000000000000 ) ) ;
#45009 = CARTESIAN_POINT ( 'NONE',  ( 4.975610109902397937, 45.55079628452135410, -17.82061629079668919 ) ) ;
#45010 = DIRECTION ( 'NONE',  ( -1.000000000000000000, -3.673819061467635166E-16, 6.982962677686265133E-15 ) ) ;
#45011 = LINE ( 'NONE', #50292, #44903 ) ;
#45012 = B_SPLINE_CURVE_WITH_KNOTS ( 'NONE', 3,
 ( #1294, #30124, #30742, #21359, #2223, #39879, #20430, #49539, #58613, #16664, #15742, #35162, #1603, #35473, #6596, #20743 ),
 .UNSPECIFIED., .F., .F.,
 ( 4, 3, 3, 3, 3, 4 ),
 ( 2.194378057379452319E-17, 0.0002612764279487727291, 0.0003919131003184784861, 0.0005225497727000646053, 0.0007837925190632442701, 0.001045051706266716951 ),
 .UNSPECIFIED. ) ;
#45013 = CARTESIAN_POINT ( 'NONE',  ( 2.359973842542475442, 36.05128472766631376, -25.26738538347871454 ) ) ;
#45014 = EDGE_CURVE ( 'NONE', #20551, #25364, #30245, .T. ) ;
#45015 = CARTESIAN_POINT ( 'NONE',  ( 0.1129192098497455998, 24.84520063729130612, 36.46461014570008530 ) ) ;
#45017 = ORIENTED_EDGE ( 'NONE', *, *, #1734, .F. ) ;
#45016 = CARTESIAN_POINT ( 'NONE',  ( 3.376099380956842921, 13.39763462305342401, -0.4601848967830201032 ) ) ;
#45018 = ORIENTED_EDGE ( 'NONE', *, *, #42060, .T. ) ;
#45020 = VECTOR ( 'NONE', #35681, 999.9999999999998863 ) ;
#45019 = CARTESIAN_POINT ( 'NONE',  ( 0.8557997880470606944, -11.51622788066425684, -46.50333260518571876 ) ) ;
#45021 = CARTESIAN_POINT ( 'NONE',  ( 0.5980894510889457338, 0.7015180095998205800, 48.10766805928369649 ) ) ;
#45022 = FACE_OUTER_BOUND ( 'NONE', #9198, .T. ) ;
#45023 = EDGE_CURVE ( 'NONE', #7371, #21985, #25710, .T. ) ;
#45024 = ORIENTED_EDGE ( 'NONE', *, *, #43307, .F. ) ;
#45025 = CARTESIAN_POINT ( 'NONE',  ( 0.1139756605157203617, -22.53279618253801786, 37.93716272853338012 ) ) ;
#45026 = CARTESIAN_POINT ( 'NONE',  ( 3.376099380956842921, -9.001307264897979721, -9.934024922203580132 ) ) ;
#45027 = DIRECTION ( 'NONE',  ( 0.000000000000000000, 0.000000000000000000, -1.000000000000000000 ) ) ;
#45028 = EDGE_CURVE ( 'NONE', #26582, #35321, #48127, .T. ) ;
#45029 = VERTEX_POINT ( 'NONE', #17207 ) ;
#45030 = ORIENTED_EDGE ( 'NONE', *, *, #38478, .T. ) ;
#45031 = FACE_BOUND ( 'NONE', #8035, .T. ) ;
#45032 =( BOUNDED_SURFACE ( )  B_SPLINE_SURFACE ( 3, 1, ( 
 ( #14971, #6133 ),
 ( #5825, #34683 ),
 ( #10256, #19353 ),
 ( #5525, #20578 ) ),
 .UNSPECIFIED., .F., .F., .F. ) 
 B_SPLINE_SURFACE_WITH_KNOTS ( ( 4, 4 ),
 ( 2, 2 ),
 ( 0.000000000000000000, 1.000000000000000000 ),
 ( 0.000000000000000000, 1.000000000000000000 ),
 .UNSPECIFIED. ) 
 GEOMETRIC_REPRESENTATION_ITEM ( )  RATIONAL_B_SPLINE_SURFACE ( (
 ( 1.000000000000000000, 1.000000000000000000),
 ( 0.7223157951917480446, 0.9931996967497186413),
 ( 0.7223157951917480446, 0.9931996967497186413),
 ( 1.000000000000000000, 1.000000000000000000) ) ) 
 REPRESENTATION_ITEM ( '' )  SURFACE ( )  );
#45033 = CARTESIAN_POINT ( 'NONE',  ( -6.079354080745853928, -18.90066517279539582, 3.682093327720148412 ) ) ;
#45034 = CARTESIAN_POINT ( 'NONE',  ( 0.6029443449137436017, 37.36442650921991770, 31.86595627971074052 ) ) ;
#45035 = ORIENTED_EDGE ( 'NONE', *, *, #12400, .T. ) ;
#45036 = EDGE_CURVE ( 'NONE', #9174, #18062, #11908, .T. ) ;
#45037 = ORIENTED_EDGE ( 'NONE', *, *, #49220, .T. ) ;
#45038 = LINE ( 'NONE', #16825, #23599 ) ;
#45039 = DIRECTION ( 'NONE',  ( -1.000000000000000000, -0.000000000000000000, -0.000000000000000000 ) ) ;
#45040 = ORIENTED_EDGE ( 'NONE', *, *, #39060, .F. ) ;
#45041 = CARTESIAN_POINT ( 'NONE',  ( 0.7044674535453004927, 28.78324386660388257, 39.79104918604833330 ) ) ;
#45042 = CARTESIAN_POINT ( 'NONE',  ( 3.376099380956842921, -13.39845304004336413, -0.4357060543759550542 ) ) ;
#45043 = ORIENTED_EDGE ( 'NONE', *, *, #1472, .F. ) ;
#45044 = CARTESIAN_POINT ( 'NONE',  ( 5.960721111146673579, -5.306302591836445259, -19.82781442290496443 ) ) ;
#45046 = CARTESIAN_POINT ( 'NONE',  ( 0.6039202388192953519, -39.25113122883277583, 29.51122515426866499 ) ) ;
#45045 = AXIS2_PLACEMENT_3D ( 'NONE', #32627, #8806, #33253 ) ;
#45047 = VERTEX_POINT ( 'NONE', #20976 ) ;
#45048 = CARTESIAN_POINT ( 'NONE',  ( 0.6254311100348632912, 23.45480814408369952, 42.00127298835432299 ) ) ;
#45049 = CARTESIAN_POINT ( 'NONE',  ( 0.5997462898726536595, 11.43624519451716992, -47.75734421002901797 ) ) ;
#45050 = CARTESIAN_POINT ( 'NONE',  ( 0.9730545539215883499, 16.88610103448612065, -39.44597740938043273 ) ) ;
#45051 = SURFACE_SIDE_STYLE ('',( #3316 ) ) ;
#45052 = ORIENTED_EDGE ( 'NONE', *, *, #23406, .F. ) ;
#45053 = CARTESIAN_POINT ( 'NONE',  ( 0.8551540677456739292, 19.17641535420911936, -43.91216198251520808 ) ) ;
#45054 = CARTESIAN_POINT ( 'NONE',  ( 0.6027935024548037868, 44.51201578381226653, -18.24855952726183617 ) ) ;
#45055 = ORIENTED_EDGE ( 'NONE', *, *, #32906, .T. ) ;
#45056 = DIRECTION ( 'NONE',  ( -0.07500201931887527651, 0.9580968512853041963, -0.2764509371575298857 ) ) ;
#45057 = AXIS2_PLACEMENT_3D ( 'NONE', #21045, #41110, #30738 ) ;
#45058 = ORIENTED_EDGE ( 'NONE', *, *, #16358, .F. ) ;
#45059 = CARTESIAN_POINT ( 'NONE',  ( 0.5786265663353196143, 13.09387673186399859, -46.07681357296471703 ) ) ;
#45060 = VERTEX_POINT ( 'NONE', #35091 ) ;
#45061 = CARTESIAN_POINT ( 'NONE',  ( 0.6001305935487422083, -0.5236757026892572275, 48.10757715638247589 ) ) ;
#45062 = CARTESIAN_POINT ( 'NONE',  ( 0.9787464366903551038, 24.71660722148015310, 33.84410318429993936 ) ) ;
#45063 = B_SPLINE_CURVE_WITH_KNOTS ( 'NONE', 3,
 ( #45587, #60574, #17379, #7970 ),
 .UNSPECIFIED., .F., .F.,
 ( 4, 4 ),
 ( 2.380737582480036903E-07, 0.002336974151641604130 ),
 .UNSPECIFIED. ) ;
#45064 = CONICAL_SURFACE ( 'NONE', #6992, 5.453125000000000000, 0.4883339510563931007 ) ;
#45065 = CARTESIAN_POINT ( 'NONE',  ( 0.1156867017252034141, -43.77771965051793757, 5.518520587606961847 ) ) ;
#45066 = ORIENTED_EDGE ( 'NONE', *, *, #33396, .F. ) ;
#45067 = CARTESIAN_POINT ( 'NONE',  ( 5.439999999999997726, 15.14599999999999902, 0.000000000000000000 ) ) ;
#45068 = EDGE_CURVE ( 'NONE', #56628, #3699, #4824, .T. ) ;
#45069 = LINE ( 'NONE', #50343, #58625 ) ;
#45070 = DIRECTION ( 'NONE',  ( 0.000000000000000000, 1.000000000000000000, 0.000000000000000000 ) ) ;
#45071 = ORIENTED_EDGE ( 'NONE', *, *, #18696, .T. ) ;
#45072 = ADVANCED_FACE ( 'NONE', ( #7462 ), #56538, .F. ) ;
#45073 = ORIENTED_EDGE ( 'NONE', *, *, #40870, .F. ) ;
#45074 = CARTESIAN_POINT ( 'NONE',  ( 0.2279481005628716528, 29.09488030924818247, 33.16611865840550166 ) ) ;
#45075 = CARTESIAN_POINT ( 'NONE',  ( 0.9268187852002115479, 30.36697088607808936, 31.96250009171234296 ) ) ;
#45076 = CARTESIAN_POINT ( 'NONE',  ( 4.549368137175248350, 23.67244292351589507, 35.80950303116109268 ) ) ;
#45077 = LINE ( 'NONE', #21546, #33962 ) ;
#45078 = CARTESIAN_POINT ( 'NONE',  ( 0.9790724872846759963, 38.56739429505658734, 16.39790557574631436 ) ) ;
#45079 = ORIENTED_EDGE ( 'NONE', *, *, #5955, .F. ) ;
#45080 = EDGE_CURVE ( 'NONE', #35096, #42568, #51881, .T. ) ;
#45081 = LINE ( 'NONE', #2109, #52692 ) ;
#45082 = CARTESIAN_POINT ( 'NONE',  ( 5.901463166500145796, 5.945065151443557738, 19.21390305705033441 ) ) ;
#45083 = VERTEX_POINT ( 'NONE', #59168 ) ;
#45084 = CARTESIAN_POINT ( 'NONE',  ( 4.975610109902397937, 20.32389311291233724, -44.49032227207044343 ) ) ;
#45085 = FACE_OUTER_BOUND ( 'NONE', #30128, .T. ) ;
#45086 = LINE ( 'NONE', #35060, #45020 ) ;
#45087 = CARTESIAN_POINT ( 'NONE',  ( 5.974727161628367256, -18.96851388233653068, -7.840226266082476414 ) ) ;
#45088 = DIRECTION ( 'NONE',  ( -0.1024043820194934507, 0.9641676559171120653, -0.2447326578667160801 ) ) ;
#45089 = CARTESIAN_POINT ( 'NONE',  ( 0.3622758884714730732, -17.25816669464967035, -39.50828911766992491 ) ) ;
#45090 = B_SPLINE_CURVE_WITH_KNOTS ( 'NONE', 3,
 ( #1313, #16679, #59573, #1624, #35489, #6615 ),
 .UNSPECIFIED., .F., .F.,
 ( 4, 2, 4 ),
 ( 1.764953265579307567E-18, 0.0002450742804987342304, 0.0004901485609974666176 ),
 .UNSPECIFIED. ) ;
#45091 = CARTESIAN_POINT ( 'NONE',  ( 0.9752570700956794125, -39.72995844664867349, 16.20701641182904851 ) ) ;
#45092 = CARTESIAN_POINT ( 'NONE',  ( 5.917102823773431552, 8.473612197389305933, 18.23972626932754082 ) ) ;
#45093 = EDGE_CURVE ( 'NONE', #47712, #8823, #20671, .T. ) ;
#45094 = CARTESIAN_POINT ( 'NONE',  ( 4.956445790443988031, 0.000000000000000000, 0.000000000000000000 ) ) ;
#45095 = CARTESIAN_POINT ( 'NONE',  ( 0.6001305935487315502, 46.33281397023063874, -12.95698906763762359 ) ) ;
#45096 = EDGE_CURVE ( 'NONE', #58621, #35726, #42930, .T. ) ;
#45097 = CARTESIAN_POINT ( 'NONE',  ( 0.9762797500689124330, 9.222352665238359393, 40.88120590813919364 ) ) ;
#45098 = DIRECTION ( 'NONE',  ( -1.000000000000000000, -0.000000000000000000, -0.000000000000000000 ) ) ;
#45099 = CARTESIAN_POINT ( 'NONE',  ( 2.299652685299203192, -34.31474700355062879, -35.02541738424348949 ) ) ;
#45100 = EDGE_CURVE ( 'NONE', #26391, #52654, #32486, .T. ) ;
#45101 = AXIS2_PLACEMENT_3D ( 'NONE', #37063, #55510, #26707 ) ;
#45102 = ORIENTED_EDGE ( 'NONE', *, *, #966, .T. ) ;
#45103 = DIRECTION ( 'NONE',  ( 0.000000000000000000, 0.000000000000000000, -1.000000000000000000 ) ) ;
#45104 = CARTESIAN_POINT ( 'NONE',  ( 0.1087620492084205304, 37.16461718700635686, 21.87505161834429757 ) ) ;
#45105 = B_SPLINE_CURVE_WITH_KNOTS ( 'NONE', 3,
 ( #50626, #7085, #7715, #54389 ),
 .UNSPECIFIED., .F., .F.,
 ( 4, 4 ),
 ( 3.469446951953614189E-18, 0.004050076154993004218 ),
 .UNSPECIFIED. ) ;
#45106 = CARTESIAN_POINT ( 'NONE',  ( 0.9757892942422810023, -39.66188497122482204, -16.37293303864347394 ) ) ;
#45107 = CARTESIAN_POINT ( 'NONE',  ( -4.000000000000000000, 1.935983797701054998, -0.2494693066162268769 ) ) ;
#45108 = DIRECTION ( 'NONE',  ( 0.000000000000000000, 0.000000000000000000, -1.000000000000000000 ) ) ;
#45109 = ORIENTED_EDGE ( 'NONE', *, *, #6685, .F. ) ;
#45110 = CARTESIAN_POINT ( 'NONE',  ( 3.680974057930773924, 30.65154904503179267, -36.90739001595142099 ) ) ;
#45111 = CARTESIAN_POINT ( 'NONE',  ( 0.9741495583595168872, 16.78504838919937825, -39.48917442789103660 ) ) ;
#45112 = EDGE_CURVE ( 'NONE', #39282, #44660, #45160, .T. ) ;
#45113 = B_SPLINE_CURVE_WITH_KNOTS ( 'NONE', 3,
 ( #54362, #58144, #49685, #29967, #15269, #43798, #5822, #24657, #44410, #6130, #16186, #54060, #29654, #10252, #11484, #49076, #6739, #25572, #1748 ),
 .UNSPECIFIED., .F., .F.,
 ( 4, 3, 3, 3, 3, 3, 4 ),
 ( 1.153344816771540786E-16, 0.0002618519381806258626, 0.0003927759815485975473, 0.0005237000248299470079, 0.0006546240681324973915, 0.0007855481115631335765, 0.0009699050456655115924 ),
 .UNSPECIFIED. ) ;
#45114 = DIRECTION ( 'NONE',  ( 0.09722883295013597105, 0.5631913828983523551, 0.8205863880617298989 ) ) ;
#45115 = VERTEX_POINT ( 'NONE', #32858 ) ;
#45116 = ADVANCED_FACE ( 'NONE', ( #37560 ), #22529, .F. ) ;
#45117 = CARTESIAN_POINT ( 'NONE',  ( 4.956445790444004018, -40.78973928653763181, -23.53157918788973291 ) ) ;
#45118 = ORIENTED_EDGE ( 'NONE', *, *, #25639, .F. ) ;
#45119 = CARTESIAN_POINT ( 'NONE',  ( 1.157644175074336035, -26.42675002938718976, -32.53658184818230836 ) ) ;
#45120 = CARTESIAN_POINT ( 'NONE',  ( 0.6025881611877910160, -29.45877655626822289, 38.03302298778292112 ) ) ;
#45121 = ORIENTED_EDGE ( 'NONE', *, *, #9870, .T. ) ;
#45122 = CARTESIAN_POINT ( 'NONE',  ( -6.079354080745853928, 13.83333621898001375, -13.39521423124011612 ) ) ;
#45123 = ORIENTED_EDGE ( 'NONE', *, *, #41286, .T. ) ;
#45124 = CARTESIAN_POINT ( 'NONE',  ( 0.8551540677456739292, -34.52115452272951757, 33.23105123575888342 ) ) ;
#45125 = CARTESIAN_POINT ( 'NONE',  ( 0.1100053167205930493, -26.39466280306244883, -34.10339839758277236 ) ) ;
#45126 = EDGE_LOOP ( 'NONE', ( #36009, #51459 ) ) ;
#45127 = VERTEX_POINT ( 'NONE', #56629 ) ;
#45128 = CARTESIAN_POINT ( 'NONE',  ( 0.9790320750461898314, 20.21589195895753832, -36.71041875062102378 ) ) ;
#45129 = B_SPLINE_CURVE_WITH_KNOTS ( 'NONE', 3,
 ( #8744, #28780, #19098, #28163 ),
 .UNSPECIFIED., .F., .F.,
 ( 4, 4 ),
 ( 0.000000000000000000, 0.005004948556313813107 ),
 .UNSPECIFIED. ) ;
#45130 =( BOUNDED_SURFACE ( )  B_SPLINE_SURFACE ( 3, 1, ( 
 ( #41760, #27632 ),
 ( #3495, #61426 ),
 ( #52044, #32970 ),
 ( #7904, #28242 ) ),
 .UNSPECIFIED., .F., .F., .F. ) 
 B_SPLINE_SURFACE_WITH_KNOTS ( ( 4, 4 ),
 ( 2, 2 ),
 ( 0.000000000000000000, 1.000000000000000000 ),
 ( 0.000000000000000000, 1.000000000000000000 ),
 .UNSPECIFIED. ) 
 GEOMETRIC_REPRESENTATION_ITEM ( )  RATIONAL_B_SPLINE_SURFACE ( (
 ( 1.000000000000000000, 1.000000000000000000),
 ( 0.9953390228620291325, 0.8624445117760984880),
 ( 0.9953390228620291325, 0.8624445117760984880),
 ( 1.000000000000000000, 1.000000000000000000) ) ) 
 REPRESENTATION_ITEM ( '' )  SURFACE ( )  );
#45131 = VERTEX_POINT ( 'NONE', #36626 ) ;
#45132 = ORIENTED_EDGE ( 'NONE', *, *, #60745, .T. ) ;
#45133 = DIRECTION ( 'NONE',  ( 0.000000000000000000, 0.000000000000000000, 1.000000000000000000 ) ) ;
#45134 = CARTESIAN_POINT ( 'NONE',  ( 0.6845945791218023269, -39.15688516782633855, -25.82914757919060378 ) ) ;
#45135 = CARTESIAN_POINT ( 'NONE',  ( 0.6008123274975392114, -25.08365429764632282, -42.21806293797273213 ) ) ;
#45136 = CARTESIAN_POINT ( 'NONE',  ( 4.335381028904201628, -33.67825942593249522, -35.57431221687826906 ) ) ;
#45137 = CARTESIAN_POINT ( 'NONE',  ( 4.962356264823603702, -10.17958088187380739, -40.83640203215431086 ) ) ;
#45138 = ORIENTED_EDGE ( 'NONE', *, *, #25236, .T. ) ;
#45139 = EDGE_CURVE ( 'NONE', #28235, #1532, #3945, .T. ) ;
#45140 = DIRECTION ( 'NONE',  ( -0.07906939808003035641, -0.6497517485244272972, -0.7560229464617532757 ) ) ;
#45141 = DIRECTION ( 'NONE',  ( 1.000000000000000000, 0.000000000000000000, 0.000000000000000000 ) ) ;
#45142 = ORIENTED_EDGE ( 'NONE', *, *, #1619, .F. ) ;
#45143 = CARTESIAN_POINT ( 'NONE',  ( 2.528100132419517365, -21.55886359172174949, 36.02039948786813284 ) ) ;
#45144 = EDGE_CURVE ( 'NONE', #49823, #25214, #45928, .T. ) ;
#45145 = ORIENTED_EDGE ( 'NONE', *, *, #6139, .F. ) ;
#45146 =( BOUNDED_SURFACE ( )  B_SPLINE_SURFACE ( 3, 1, ( 
 ( #4111, #16167 ),
 ( #23250, #59051 ),
 ( #35279, #11462 ),
 ( #51118, #30546 ) ),
 .UNSPECIFIED., .F., .F., .F. ) 
 B_SPLINE_SURFACE_WITH_KNOTS ( ( 4, 4 ),
 ( 2, 2 ),
 ( 0.000000000000000000, 1.000000000000000000 ),
 ( 0.000000000000000000, 1.000000000000000000 ),
 .UNSPECIFIED. ) 
 GEOMETRIC_REPRESENTATION_ITEM ( )  RATIONAL_B_SPLINE_SURFACE ( (
 ( 1.000000000000000000, 1.000000000000000000),
 ( 0.7211978278499968642, 0.9934217856018975334),
 ( 0.7211978278499968642, 0.9934217856018975334),
 ( 1.000000000000000000, 1.000000000000000000) ) ) 
 REPRESENTATION_ITEM ( '' )  SURFACE ( )  );
#45147 = CARTESIAN_POINT ( 'NONE',  ( 4.553261556744873317, 38.38432632180467863, 21.35844232721216684 ) ) ;
#45148 = CARTESIAN_POINT ( 'NONE',  ( -6.078457390727109555, 13.82950465835804188, -13.39922803529968931 ) ) ;
#45149 = CARTESIAN_POINT ( 'NONE',  ( 5.965394784446458765, 17.76824826579354877, -10.27521535480968140 ) ) ;
#45150 = ORIENTED_EDGE ( 'NONE', *, *, #48881, .F. ) ;
#45151 = CARTESIAN_POINT ( 'NONE',  ( 1.231276596079887264, 35.62927148397050559, -22.08691432816256395 ) ) ;
#45152 = CARTESIAN_POINT ( 'NONE',  ( 4.962356264823608143, 0.000000000000000000, 0.000000000000000000 ) ) ;
#45153 = DIRECTION ( 'NONE',  ( -0.07836865515943411409, 0.9608836331491580340, -0.2656332009267214356 ) ) ;
#45154 = CARTESIAN_POINT ( 'NONE',  ( 2.301529144917014325, -17.18548816179652405, 44.85388898586996476 ) ) ;
#45155 = EDGE_CURVE ( 'NONE', #33056, #5641, #12001, .T. ) ;
#45156 = EDGE_CURVE ( 'NONE', #55623, #28664, #18437, .T. ) ;
#45157 = ORIENTED_EDGE ( 'NONE', *, *, #14457, .F. ) ;
#45158 = FACE_OUTER_BOUND ( 'NONE', #20603, .T. ) ;
#45159 = ORIENTED_EDGE ( 'NONE', *, *, #49753, .F. ) ;
#45160 = B_SPLINE_CURVE_WITH_KNOTS ( 'NONE', 3,
 ( #11584, #30989, #50096, #16908, #13431, #61621 ),
 .UNSPECIFIED., .F., .F.,
 ( 4, 2, 4 ),
 ( 1.738108305489988542E-18, 0.0002291966416970796477, 0.0004583932833941575607 ),
 .UNSPECIFIED. ) ;
#45161 = EDGE_CURVE ( 'NONE', #28569, #5258, #22711, .T. ) ;
#45162 = CARTESIAN_POINT ( 'NONE',  ( 0.1365634738349413013, 39.47324950736464189, 19.71611505729723746 ) ) ;
#45163 = DIRECTION ( 'NONE',  ( 0.000000000000000000, 0.000000000000000000, 1.000000000000000000 ) ) ;
#45164 =( LENGTH_UNIT ( ) NAMED_UNIT ( * ) SI_UNIT ( .MILLI., .METRE. ) );
#45165 = ADVANCED_FACE ( 'NONE', ( #60390 ), #29986, .T. ) ;
#45166 = ORIENTED_EDGE ( 'NONE', *, *, #34050, .F. ) ;
#45167 = CARTESIAN_POINT ( 'NONE',  ( 0.1064266379913938743, -25.80493164505229586, 34.55203636557764924 ) ) ;
#45168 = CARTESIAN_POINT ( 'NONE',  ( -11.40403086437694569, 0.6959691356230539583, 0.000000000000000000 ) ) ;
#45169 = CARTESIAN_POINT ( 'NONE',  ( 0.1152809850208375703, -35.49359372161672610, 26.21354778000421959 ) ) ;
#45170 = B_SPLINE_CURVE_WITH_KNOTS ( 'NONE', 3,
 ( #17557, #56668, #25783, #11703, #41381, #17869, #36994, #30782, #37290, #3128, #22257, #60435, #36674, #55745, #31966, #51046, #8144, #27260, #46685, #3734, #22868, #42000, #61063, #18175, #47290 ),
 .UNSPECIFIED., .F., .F.,
 ( 4, 3, 3, 3, 3, 3, 3, 3, 4 ),
 ( 4.670885906470169154E-18, 0.0005656085177311388811, 0.001131215744874498755, 0.001696821861372765049, 0.002262427090022497284, 0.002828031679238745925, 0.003393635864401604862, 0.003977030878808131623, 0.004561030005651159000 ),
 .UNSPECIFIED. ) ;
#45171 = CARTESIAN_POINT ( 'NONE',  ( 0.9757892942422824456, 37.13414688883494108, -21.49867881049906870 ) ) ;
#45172 = CARTESIAN_POINT ( 'NONE',  ( 4.553261556744873317, 22.96401893593727550, 37.44587293859699173 ) ) ;
#45173 = CARTESIAN_POINT ( 'NONE',  ( 0.9730545539215883499, -37.40983423658487794, 21.01499094264535472 ) ) ;
#45174 = FACE_OUTER_BOUND ( 'NONE', #23701, .T. ) ;
#45175 = DIRECTION ( 'NONE',  ( 0.000000000000000000, 0.000000000000000000, 1.000000000000000000 ) ) ;
#45176 = B_SPLINE_CURVE_WITH_KNOTS ( 'NONE', 3,
 ( #34268, #25155, #53955, #44001, #53343, #35197, #11378, #10454, #29546, #5712, #24861, #58337, #53637, #30462, #44301, #1331, #39596, #34890, #30159 ),
 .UNSPECIFIED., .F., .F.,
 ( 4, 3, 3, 3, 3, 3, 4 ),
 ( 8.674294979774128197E-18, 0.0002732106629380666061, 0.0004098138914053808530, 0.0005464171197651462560, 0.0006830203481512559828, 0.0008196235766963627656, 0.001011968216111142679 ),
 .UNSPECIFIED. ) ;
#45177 = DIRECTION ( 'NONE',  ( 0.000000000000000000, 0.000000000000000000, 1.000000000000000000 ) ) ;
#45178 = CARTESIAN_POINT ( 'NONE',  ( 0.1149546198390367924, 36.82985107031473859, 24.30038343651506949 ) ) ;
#45179 = ORIENTED_EDGE ( 'NONE', *, *, #41614, .F. ) ;
#45180 = B_SPLINE_CURVE_WITH_KNOTS ( 'NONE', 3,
 ( #57797, #24304, #18691, #33725 ),
 .UNSPECIFIED., .F., .F.,
 ( 4, 4 ),
 ( 0.000000000000000000, 0.005004741218457404127 ),
 .UNSPECIFIED. ) ;
#45181 = CARTESIAN_POINT ( 'NONE',  ( 2.533389852662419894, -2.991380632221138924, -43.91471477360168052 ) ) ;
#45182 = CARTESIAN_POINT ( 'NONE',  ( 0.5827359174754830340, 46.16863801597762773, 12.74690115177623717 ) ) ;
#45183 = DIRECTION ( 'NONE',  ( -1.000000000000000000, -0.000000000000000000, -0.000000000000000000 ) ) ;
#45184 = VERTEX_POINT ( 'NONE', #52236 ) ;
#45185 = CARTESIAN_POINT ( 'NONE',  ( 0.5997462898726536595, -20.35457962188229430, 44.69052157405150183 ) ) ;
#45186 = CARTESIAN_POINT ( 'NONE',  ( 0.1129192098497447394, -31.35755906439637641, 31.04279751098549056 ) ) ;
#45187 = EDGE_CURVE ( 'NONE', #23359, #43044, #28967, .T. ) ;
#45188 = CARTESIAN_POINT ( 'NONE',  ( 0.5806925824938502512, -14.41498975133575300, -44.62544602368080859 ) ) ;
#45189 = AXIS2_PLACEMENT_3D ( 'NONE', #3446, #9087, #46712 ) ;
#45191 = VERTEX_POINT ( 'NONE', #538 ) ;
#45190 = AXIS2_PLACEMENT_3D ( 'NONE', #29418, #19729, #33838 ) ;
#45192 = CARTESIAN_POINT ( 'NONE',  ( 4.967162193818130511, 0.000000000000000000, 0.000000000000000000 ) ) ;
#45193 = EDGE_CURVE ( 'NONE', #39295, #52389, #28699, .T. ) ;
#45194 = CARTESIAN_POINT ( 'NONE',  ( 0.6001305935487315502, -33.64689939321917933, -34.38748867424702382 ) ) ;
#45195 = ORIENTED_EDGE ( 'NONE', *, *, #8855, .T. ) ;
#45196 = CARTESIAN_POINT ( 'NONE',  ( 5.958863334805807099, 20.34989385289157582, -2.680345151634403233 ) ) ;
#45197 = VERTEX_POINT ( 'NONE', #48469 ) ;
#45198 = EDGE_LOOP ( 'NONE', ( #36771, #35409, #51683, #11148 ) ) ;
#45199 = CARTESIAN_POINT ( 'NONE',  ( 0.9757787079277442377, -5.639827755376935592, 42.53619983261575754 ) ) ;
#45200 = ORIENTED_EDGE ( 'NONE', *, *, #400, .T. ) ;
#45201 = CARTESIAN_POINT ( 'NONE',  ( 0.5807400328401637335, 5.711437504335951765, 47.55718917606844798 ) ) ;
#45202 = CARTESIAN_POINT ( 'NONE',  ( 4.975801465491695552, 35.64402118370958306, -32.01766832630274706 ) ) ;
#45203 = ORIENTED_EDGE ( 'NONE', *, *, #48881, .T. ) ;
#45204 = CARTESIAN_POINT ( 'NONE',  ( 0.1102847568649952675, 0.09217763870840627038, 43.12433804869904463 ) ) ;
#45205 = CARTESIAN_POINT ( 'NONE',  ( 0.5804410086790514622, 46.40460073163232124, -6.792119168064288282 ) ) ;
#45206 = ORIENTED_EDGE ( 'NONE', *, *, #38363, .T. ) ;
#45207 = CARTESIAN_POINT ( 'NONE',  ( 4.553261556744873317, 35.06776520399894537, -26.45357082552063233 ) ) ;
#45208 = CARTESIAN_POINT ( 'NONE',  ( 49.64102424810503322, 12.24500408462137813, -2.512856703132412495 ) ) ;
#45209 = CARTESIAN_POINT ( 'NONE',  ( 0.5850706913938534814, 33.73916126769498192, -33.99603398296554957 ) ) ;
#45210 = CARTESIAN_POINT ( 'NONE',  ( 0.9762797500689124330, 35.79768877047958853, 21.79105926469807741 ) ) ;
#45211 = ORIENTED_EDGE ( 'NONE', *, *, #57680, .T. ) ;
#45212 = B_SPLINE_CURVE_WITH_KNOTS ( 'NONE', 3,
 ( #11158, #58732, #44084, #59049 ),
 .UNSPECIFIED., .F., .F.,
 ( 4, 4 ),
 ( 0.000000000000000000, 0.005014147105413707325 ),
 .UNSPECIFIED. ) ;
#45213 = ORIENTED_EDGE ( 'NONE', *, *, #22659, .F. ) ;
#45214 = CARTESIAN_POINT ( 'NONE',  ( 4.956653778116991482, -9.917440902360828758, -47.05699031914960528 ) ) ;
#45215 = EDGE_CURVE ( 'NONE', #13981, #60643, #13082, .T. ) ;
#45216 = CARTESIAN_POINT ( 'NONE',  ( 0.6000166863083106206, 17.45040302316649061, -45.90541270958705411 ) ) ;
#45217 = CARTESIAN_POINT ( 'NONE',  ( 2.185380717157383135, 13.84901153640016425, -41.79742435284565971 ) ) ;
#45218 = EDGE_LOOP ( 'NONE', ( #32889, #6508, #29667, #21526 ) ) ;
#45219 = CARTESIAN_POINT ( 'NONE',  ( 5.965394784446458765, -17.78272165951794292, -10.25014670152108742 ) ) ;
#45220 = CARTESIAN_POINT ( 'NONE',  ( 5.917102823773431552, -2.004558746498583677, 20.01178308606152356 ) ) ;
#45221 = EDGE_CURVE ( 'NONE', #38956, #48507, #48997, .T. ) ;
#45222 = CARTESIAN_POINT ( 'NONE',  ( 3.783198216974387851, 1.726720072276576978, -43.00370179234475643 ) ) ;
#45223 = CARTESIAN_POINT ( 'NONE',  ( 0.6067375320500753011, 29.71715680108788149, -37.56348932307230370 ) ) ;
#45224 =( BOUNDED_SURFACE ( )  B_SPLINE_SURFACE ( 3, 1, ( 
 ( #13056, #32455 ),
 ( #32150, #27134 ),
 ( #13356, #60315 ),
 ( #20974, #8021 ) ),
 .UNSPECIFIED., .F., .F., .F. ) 
 B_SPLINE_SURFACE_WITH_KNOTS ( ( 4, 4 ),
 ( 2, 2 ),
 ( 0.000000000000000000, 1.000000000000000000 ),
 ( 0.000000000000000000, 1.000000000000000000 ),
 .UNSPECIFIED. ) 
 GEOMETRIC_REPRESENTATION_ITEM ( )  RATIONAL_B_SPLINE_SURFACE ( (
 ( 1.000000000000000000, 1.000000000000000000),
 ( 0.9953390228620291325, 0.8624445117760984880),
 ( 0.9953390228620291325, 0.8624445117760984880),
 ( 1.000000000000000000, 1.000000000000000000) ) ) 
 REPRESENTATION_ITEM ( '' )  SURFACE ( )  );
#45225 = ADVANCED_FACE ( 'NONE', ( #38798 ), #34094, .F. ) ;
#45226 = ORIENTED_EDGE ( 'NONE', *, *, #55372, .F. ) ;
#45227 = ORIENTED_EDGE ( 'NONE', *, *, #60378, .F. ) ;
#45228 = CARTESIAN_POINT ( 'NONE',  ( 2.624215991343620935, 46.71702075422651745, 11.05657803851061693 ) ) ;
#45229 = EDGE_CURVE ( 'NONE', #10490, #61767, #18285, .T. ) ;
#45230 = CARTESIAN_POINT ( 'NONE',  ( 3.727782113643637096, 42.34800052025986616, 11.80782062203034322 ) ) ;
#45231 = CARTESIAN_POINT ( 'NONE',  ( 4.958415959904820092, 42.74072562871883463, 15.37642112304467190 ) ) ;
#45232 = CONICAL_SURFACE ( 'NONE', #58194, 42.08604991992415023, 1.569615340895231137 ) ;
#45233 = CARTESIAN_POINT ( 'NONE',  ( 0.9730545539215883499, 21.89037132892435622, 36.90443313492338717 ) ) ;
#45234 = CARTESIAN_POINT ( 'NONE',  ( 2.706805983486680223, -14.09998663259384344, -41.68892527135270143 ) ) ;
#45235 = CARTESIAN_POINT ( 'NONE',  ( 0.2940135542859007023, 25.89542279162153093, 35.71648956902944150 ) ) ;
#45236 = CARTESIAN_POINT ( 'NONE',  ( -6.015611763856276717, -18.19956619163654565, -4.882992715191491584 ) ) ;
#45237 = DIRECTION ( 'NONE',  ( 0.000000000000000000, -0.5000000000000013323, -0.8660254037844380415 ) ) ;
#45238 = ADVANCED_FACE ( 'NONE', ( #15285 ), #14363, .T. ) ;
#45239 = DIRECTION ( 'NONE',  ( -1.000000000000000000, -0.000000000000000000, -0.000000000000000000 ) ) ;
#45240 = CARTESIAN_POINT ( 'NONE',  ( 4.958415959904818315, 37.15973263041131958, -26.12198737958080130 ) ) ;
#45241 = DIRECTION ( 'NONE',  ( -0.1024043820194934645, 0.1167898032637269823, 0.9878630899050867553 ) ) ;
#45242 = DIRECTION ( 'NONE',  ( -1.000000000000000000, -0.000000000000000000, -0.000000000000000000 ) ) ;
#45243 = CARTESIAN_POINT ( 'NONE',  ( 0.6027935024548037868, -33.89348162668954245, -34.14031893787213079 ) ) ;
#45244 = CARTESIAN_POINT ( 'NONE',  ( 0.5998501479064699549, -18.89267974119636406, -44.24259072156078787 ) ) ;
#45245 = CARTESIAN_POINT ( 'NONE',  ( 0.5807400328401574052, 6.791881299636263414, -47.41494605191436307 ) ) ;
#45246 =( BOUNDED_SURFACE ( )  B_SPLINE_SURFACE ( 3, 1, ( 
 ( #12363, #53011 ),
 ( #27988, #8878 ),
 ( #38040, #57382 ),
 ( #10113, #61779 ) ),
 .UNSPECIFIED., .F., .F., .F. ) 
 B_SPLINE_SURFACE_WITH_KNOTS ( ( 4, 4 ),
 ( 2, 2 ),
 ( 0.000000000000000000, 1.000000000000000000 ),
 ( 0.000000000000000000, 1.000000000000000000 ),
 .UNSPECIFIED. ) 
 GEOMETRIC_REPRESENTATION_ITEM ( )  RATIONAL_B_SPLINE_SURFACE ( (
 ( 1.000000000000000000, 1.000000000000000000),
 ( 0.7223157951917480446, 0.9931996967497186413),
 ( 0.7223157951917480446, 0.9931996967497186413),
 ( 1.000000000000000000, 1.000000000000000000) ) ) 
 REPRESENTATION_ITEM ( '' )  SURFACE ( )  );
#45247 = CARTESIAN_POINT ( 'NONE',  ( 3.376099380956838925, 6.035099650301207319, 11.97021118623232105 ) ) ;
#45248 = DIRECTION ( 'NONE',  ( 0.000000000000000000, 0.000000000000000000, 1.000000000000000000 ) ) ;
#45249 = CARTESIAN_POINT ( 'NONE',  ( 5.959828726073459926, 10.25888482581834893, 17.77796293532176719 ) ) ;
#45251 = VERTEX_POINT ( 'NONE', #24988 ) ;
#45250 = DIRECTION ( 'NONE',  ( -0.000000000000000000, 1.000000000000000000, -0.000000000000000000 ) ) ;
#45252 = ORIENTED_EDGE ( 'NONE', *, *, #50444, .F. ) ;
#45253 = FACE_BOUND ( 'NONE', #739, .T. ) ;
#45254 = CARTESIAN_POINT ( 'NONE',  ( 4.390527457369401532, 1.728762144854961935, -43.89984872496869883 ) ) ;
#45255 = CARTESIAN_POINT ( 'NONE',  ( 0.8760168074886965917, -47.56749362999708808, -7.161346975773540180 ) ) ;
#45256 = ORIENTED_EDGE ( 'NONE', *, *, #54707, .F. ) ;
#45257 = ORIENTED_EDGE ( 'NONE', *, *, #11911, .F. ) ;
#45258 = FACE_OUTER_BOUND ( 'NONE', #55159, .T. ) ;
#45259 = CARTESIAN_POINT ( 'NONE',  ( 0.1092355843206037486, -37.49628696754474078, 21.30139719602306059 ) ) ;
#45260 = VERTEX_POINT ( 'NONE', #39409 ) ;
#45261 = ORIENTED_EDGE ( 'NONE', *, *, #12026, .T. ) ;
#45262 = ADVANCED_FACE ( 'NONE', ( #43814 ), #52968, .T. ) ;
#45263 = CARTESIAN_POINT ( 'NONE',  ( 1.091591847532193960, -37.75421764082017262, 18.20379194798224276 ) ) ;
#45264 = DIRECTION ( 'NONE',  ( -0.1024043820194934368, -0.9641676559171102889, 0.2447326578667227415 ) ) ;
#45265 = FACE_OUTER_BOUND ( 'NONE', #16722, .T. ) ;
#45266 = VERTEX_POINT ( 'NONE', #29063 ) ;
#45267 = AXIS2_PLACEMENT_3D ( 'NONE', #5130, #38695, #27495 ) ;
#45268 = DIRECTION ( 'NONE',  ( 0.000000000000000000, 0.000000000000000000, 1.000000000000000000 ) ) ;
#45269 = CIRCLE ( 'NONE', #18252, 47.91270532121795611 ) ;
#45270 = FACE_OUTER_BOUND ( 'NONE', #22909, .T. ) ;
#45271 = VERTEX_POINT ( 'NONE', #48180 ) ;
#45272 = EDGE_LOOP ( 'NONE', ( #13482, #13727, #32704, #41181, #26228, #45889 ) ) ;
#45273 = DIRECTION ( 'NONE',  ( 0.000000000000000000, 0.000000000000000000, 1.000000000000000000 ) ) ;
#45274 = CARTESIAN_POINT ( 'NONE',  ( 0.7948878604505662526, -19.07805348859470129, 45.24076173523978639 ) ) ;
#45275 = VERTEX_POINT ( 'NONE', #24366 ) ;
#45276 = CARTESIAN_POINT ( 'NONE',  ( 0.6008123274975389894, -48.75817511408605043, 5.847641464947805012 ) ) ;
#45277 = LINE ( 'NONE', #41500, #4606 ) ;
#45278 = CARTESIAN_POINT ( 'NONE',  ( 0.5998501479064699549, 46.60114184914301205, 11.94461217097485672 ) ) ;
#45279 = CARTESIAN_POINT ( 'NONE',  ( 0.5819845901640485764, 12.83441129068598308, -46.14435291605016687 ) ) ;
#45280 = ORIENTED_EDGE ( 'NONE', *, *, #15808, .T. ) ;
#45281 = CARTESIAN_POINT ( 'NONE',  ( 0.9757402383260939116, -30.28078671294506563, -30.40085236181982253 ) ) ;
#45282 = CARTESIAN_POINT ( 'NONE',  ( 4.549368137175248350, 35.57418903283081590, 24.02461520945284690 ) ) ;
#45283 = EDGE_CURVE ( 'NONE', #18653, #24624, #31702, .T. ) ;
#45284 = CARTESIAN_POINT ( 'NONE',  ( 0.5848930533535030563, -34.65838163711151765, 31.59224057713996103 ) ) ;
#45285 = CARTESIAN_POINT ( 'NONE',  ( 0.9757402383260949108, -21.38067434779554432, -37.20221273948030927 ) ) ;
#45286 = ORIENTED_EDGE ( 'NONE', *, *, #46334, .T. ) ;
#45287 = DIRECTION ( 'NONE',  ( 0.000000000000000000, 0.000000000000000000, -1.000000000000000000 ) ) ;
#45288 = ADVANCED_FACE ( 'NONE', ( #10895 ), #33006, .F. ) ;
#45289 = CARTESIAN_POINT ( 'NONE',  ( 0.1064266379913939575, -5.071708164747380287, 42.82540706760014615 ) ) ;
#45290 = CARTESIAN_POINT ( 'NONE',  ( 0.8751705887134553219, 48.08707113907595243, -0.8911681664083408450 ) ) ;
#45291 = CARTESIAN_POINT ( 'NONE',  ( 0.1073791018717483448, 41.52698815987167791, -11.62916352156108779 ) ) ;
#45292 = ORIENTED_EDGE ( 'NONE', *, *, #24397, .F. ) ;
#45293 = FACE_BOUND ( 'NONE', #3012, .T. ) ;
#45294 = EDGE_CURVE ( 'NONE', #2310, #44540, #29668, .T. ) ;
#45295 = CARTESIAN_POINT ( 'NONE',  ( 0.08486401232817714080, 0.000000000000000000, 0.000000000000000000 ) ) ;
#45296 = LINE ( 'NONE', #30539, #40865 ) ;
#45297 = CARTESIAN_POINT ( 'NONE',  ( 0.5987334308729317378, -14.55165157869310377, -46.90215712418830663 ) ) ;
#45298 = FACE_OUTER_BOUND ( 'NONE', #50238, .T. ) ;
#45299 = CARTESIAN_POINT ( 'NONE',  ( 0.9756008150404595902, 42.90824081423206593, -0.1421465480004359683 ) ) ;
#45300 = CARTESIAN_POINT ( 'NONE',  ( 0.8557997880470697982, -47.60865952216995822, -5.347802024197736870 ) ) ;
#45301 = CARTESIAN_POINT ( 'NONE',  ( 0.3676999524040366896, -32.25712563511761743, -30.09033780274121739 ) ) ;
#45302 = LINE ( 'NONE', #56129, #13862 ) ;
#45303 = CARTESIAN_POINT ( 'NONE',  ( 0.5834872094924165031, 37.85980081020222343, 29.33699246747713119 ) ) ;
#45304 = CARTESIAN_POINT ( 'NONE',  ( 0.9769922540276043676, 14.64910982633380421, 39.26493520155273131 ) ) ;
#45306 = VERTEX_POINT ( 'NONE', #1156 ) ;
#45305 = EDGE_CURVE ( 'NONE', #14671, #17907, #42878, .T. ) ;
#45307 = FACE_OUTER_BOUND ( 'NONE', #49464, .T. ) ;
#45308 = CARTESIAN_POINT ( 'NONE',  ( 0.9968887458511649369, -17.02616470386906755, 39.38692798189856603 ) ) ;
#45310 = ADVANCED_FACE ( 'NONE', ( #10271 ), #13764, .F. ) ;
#45309 = DIRECTION ( 'NONE',  ( 0.000000000000000000, 0.000000000000000000, 1.000000000000000000 ) ) ;
#45311 = CARTESIAN_POINT ( 'NONE',  ( 0.5830082357119558134, -34.59666430896329103, -31.65916697626838783 ) ) ;
#45312 = CARTESIAN_POINT ( 'NONE',  ( 5.896782393890504181, -11.92541098582135994, 16.19600752337635541 ) ) ;
#45313 = COLOUR_RGB ( '', 0.09019608, 0.27058824, 0.51372549) ;
#45314 = CARTESIAN_POINT ( 'NONE',  ( 0.5988103564986356764, 17.84821699813482709, -44.67429521517314583 ) ) ;
#45315 = B_SPLINE_CURVE_WITH_KNOTS ( 'NONE', 3,
 ( #7805, #35732, #36350, #31314 ),
 .UNSPECIFIED., .F., .F.,
 ( 4, 4 ),
 ( 0.000000000000000000, 0.004446090762761383333 ),
 .UNSPECIFIED. ) ;
#45316 = APPLICATION_PROTOCOL_DEFINITION ( 'draft international standard', 'automotive_design', 1998, #36008 ) ;
#45317 = CARTESIAN_POINT ( 'NONE',  ( 0.2224561200757630419, 36.95704201588763027, 22.21411683958066163 ) ) ;
#45318 =( BOUNDED_SURFACE ( )  B_SPLINE_SURFACE ( 3, 1, ( 
 ( #43387, #19569 ),
 ( #53056, #38686 ),
 ( #48673, #5728 ),
 ( #23640, #48069 ) ),
 .UNSPECIFIED., .F., .F., .F. ) 
 B_SPLINE_SURFACE_WITH_KNOTS ( ( 4, 4 ),
 ( 2, 2 ),
 ( 0.000000000000000000, 1.000000000000000000 ),
 ( 0.000000000000000000, 1.000000000000000000 ),
 .UNSPECIFIED. ) 
 GEOMETRIC_REPRESENTATION_ITEM ( )  RATIONAL_B_SPLINE_SURFACE ( (
 ( 1.000000000000000000, 1.000000000000000000),
 ( 0.9953040768229013402, 0.8617119497784988535),
 ( 0.9953040768229013402, 0.8617119497784988535),
 ( 1.000000000000000000, 1.000000000000000000) ) ) 
 REPRESENTATION_ITEM ( '' )  SURFACE ( )  );
#45319 = B_SPLINE_CURVE_WITH_KNOTS ( 'NONE', 3,
 ( #41635, #28130, #31602, #3685 ),
 .UNSPECIFIED., .F., .F.,
 ( 4, 4 ),
 ( 0.000000000000000000, 0.005004741218457404127 ),
 .UNSPECIFIED. ) ;
#45320 = CARTESIAN_POINT ( 'NONE',  ( 0.5998501479064699549, 41.39809967730487017, -24.50586714782561160 ) ) ;
#45321 = CARTESIAN_POINT ( 'NONE',  ( 4.691466044806102076, 39.84135254923108249, 20.01963481131674172 ) ) ;
#45323 = VERTEX_POINT ( 'NONE', #35015 ) ;
#45322 = LINE ( 'NONE', #45016, #28350 ) ;
#45324 = ORIENTED_EDGE ( 'NONE', *, *, #31678, .F. ) ;
#45325 = CARTESIAN_POINT ( 'NONE',  ( 0.3622758884714600280, -34.70015533914845918, 25.58609868863709380 ) ) ;
#45326 = DIRECTION ( 'NONE',  ( -1.000000000000000000, -0.000000000000000000, -0.000000000000000000 ) ) ;
#45327 = CARTESIAN_POINT ( 'NONE',  ( 3.783198216974389627, -1.726720072276277218, 43.00370179234475643 ) ) ;
#45328 = B_SPLINE_CURVE_WITH_KNOTS ( 'NONE', 3,
 ( #13695, #32484, #19858, #27463 ),
 .UNSPECIFIED., .F., .F.,
 ( 4, 4 ),
 ( 0.000000000000000000, 0.004447772540403782497 ),
 .UNSPECIFIED. ) ;
#45329 = CARTESIAN_POINT ( 'NONE',  ( 0.5850706913938533704, -12.22095376872004202, -46.31100969101499487 ) ) ;
#45330 = DIRECTION ( 'NONE',  ( -0.07500201931887529039, -0.6540624036680577902, -0.7527131387228827020 ) ) ;
#45331 = CARTESIAN_POINT ( 'NONE',  ( 0.1097557419366048670, 41.59672960874312508, -11.37678103520293149 ) ) ;
#45332 = VERTEX_POINT ( 'NONE', #50318 ) ;
#45333 = ORIENTED_EDGE ( 'NONE', *, *, #60812, .T. ) ;
#45334 = EDGE_CURVE ( 'NONE', #11680, #48862, #40964, .T. ) ;
#45335 = DIRECTION ( 'NONE',  ( -1.000000000000000000, -0.000000000000000000, -0.000000000000000000 ) ) ;
#45336 = CARTESIAN_POINT ( 'NONE',  ( 0.1087620492084205442, -10.81135549499751747, -41.74735017127127179 ) ) ;
#45337 = CARTESIAN_POINT ( 'NONE',  ( 0.5997462898726536595, 37.05192695178125462, 32.22896739432052016 ) ) ;
#45338 = VERTEX_POINT ( 'NONE', #35320 ) ;
#45339 = VERTEX_POINT ( 'NONE', #1455 ) ;
#45340 = CARTESIAN_POINT ( 'NONE',  ( 0.6846871229502932144, -0.8641397935262891128, 47.90045233486063836 ) ) ;
#45341 = CARTESIAN_POINT ( 'NONE',  ( 0.7954196712028467342, 0.8690072546825631239, -48.09103417491925825 ) ) ;
#45342 = ORIENTED_EDGE ( 'NONE', *, *, #52746, .F. ) ;
#45343 = CARTESIAN_POINT ( 'NONE',  ( 3.661933894777872567, -28.90718021623337819, -37.10803278129762361 ) ) ;
#45344 = CARTESIAN_POINT ( 'NONE',  ( 0.9741495583595175534, 41.54695848110013401, -10.72301204857613222 ) ) ;
#45345 = ORIENTED_EDGE ( 'NONE', *, *, #16051, .T. ) ;
#45346 = CARTESIAN_POINT ( 'NONE',  ( -2.569797478183790229, -14.01151037928420173, -4.218948559326200609 ) ) ;
#45347 = CARTESIAN_POINT ( 'NONE',  ( 0.2940135542859018680, -6.245378429118067842, 43.67191084631547682 ) ) ;
#45348 = ORIENTED_EDGE ( 'NONE', *, *, #57907, .F. ) ;
#45349 = CARTESIAN_POINT ( 'NONE',  ( 5.910764540655177868, -17.29668172820417027, -10.26284754161198087 ) ) ;
#45350 = CARTESIAN_POINT ( 'NONE',  ( 5.974727161628369032, 12.50710176110007588, -16.27409205901363265 ) ) ;
#45351 = CARTESIAN_POINT ( 'NONE',  ( 0.5832367798473389042, 41.61463593465337851, -23.71165515427673043 ) ) ;
#45352 = CARTESIAN_POINT ( 'NONE',  ( 5.880360259849752858, -39.91356965504166254, 26.61251048557179644 ) ) ;
#45353 = EDGE_LOOP ( 'NONE', ( #30315, #60336, #39865, #54913 ) ) ;
#45354 = DIRECTION ( 'NONE',  ( -1.000000000000000000, -0.000000000000000000, -0.000000000000000000 ) ) ;
#45355 = DIRECTION ( 'NONE',  ( -1.000000000000000000, -0.000000000000000000, -0.000000000000000000 ) ) ;
#45356 = ORIENTED_EDGE ( 'NONE', *, *, #42873, .F. ) ;
#45357 = DIRECTION ( 'NONE',  ( 0.07906939808003037029, -0.5978040102392425670, 0.7977332860230550438 ) ) ;
#45358 = B_SPLINE_CURVE_WITH_KNOTS ( 'NONE', 3,
 ( #58119, #25544, #6714, #54032, #11155, #1718, #35273, #6103, #49971, #49654, #25854, #2029, #39992, #11457, #39063, #30541, #26161, #44383, #11778, #1411, #44994, #58422, #34348, #21159, #39675 ),
 .UNSPECIFIED., .F., .F.,
 ( 4, 3, 3, 3, 3, 3, 3, 3, 4 ),
 ( 6.254634441385502288E-18, 0.0005656085177311393148, 0.001131215744874498755, 0.001696821861372764615, 0.002262427090022497284, 0.002828031679238743323, 0.003393635864401603128, 0.003977030878808130755, 0.004561030005651158133 ),
 .UNSPECIFIED. ) ;
#45359 = EDGE_LOOP ( 'NONE', ( #47883, #44714, #45043, #7180 ) ) ;
#45360 = CARTESIAN_POINT ( 'NONE',  ( 0.8551540677456715978, 13.28067116677266846, -46.03951182599413272 ) ) ;
#45361 = EDGE_CURVE ( 'NONE', #56157, #41236, #11007, .T. ) ;
#45362 = EDGE_LOOP ( 'NONE', ( #44198, #13160, #5878, #25986 ) ) ;
#45363 = CARTESIAN_POINT ( 'NONE',  ( -6.017396004339686577, -0.001173774848850273316, -18.84316306185412415 ) ) ;
#45364 = LINE ( 'NONE', #22155, #48427 ) ;
#45365 = CARTESIAN_POINT ( 'NONE',  ( 0.1158403557922069033, -43.76671389845916593, 5.604914068408183958 ) ) ;
#45366 = ORIENTED_EDGE ( 'NONE', *, *, #60511, .T. ) ;
#45367 = CARTESIAN_POINT ( 'NONE',  ( 2.618530812446115519, -33.90288491188699993, 32.56257336037101169 ) ) ;
#45368 = ADVANCED_FACE ( 'NONE', ( #12139 ), #21512, .T. ) ;
#45369 = LINE ( 'NONE', #21537, #6608 ) ;
#45370 = CARTESIAN_POINT ( 'NONE',  ( 5.895596859100789899, -7.225383168024946734, -18.77024297359278293 ) ) ;
#45371 = ORIENTED_EDGE ( 'NONE', *, *, #5146, .F. ) ;
#45372 = VECTOR ( 'NONE', #15567, 1000.000000000000000 ) ;
#45373 = EDGE_CURVE ( 'NONE', #30367, #35775, #7387, .T. ) ;
#45374 = VERTEX_POINT ( 'NONE', #59713 ) ;
#45375 = DIRECTION ( 'NONE',  ( 0.000000000000000000, 0.000000000000000000, -1.000000000000000000 ) ) ;
#45376 = CARTESIAN_POINT ( 'NONE',  ( 0.3676999524040366896, 30.26295534861856495, 32.09523511193457068 ) ) ;
#45377 = LINE ( 'NONE', #16541, #22953 ) ;
#45378 = CARTESIAN_POINT ( 'NONE',  ( 0.5848930533535030563, -30.13830825645530354, 35.92986860296647933 ) ) ;
#45379 = CARTESIAN_POINT ( 'NONE',  ( 0.2885700199627521112, 41.84838128711407990, 10.38006184593217185 ) ) ;
#45380 = ORIENTED_EDGE ( 'NONE', *, *, #21703, .F. ) ;
#45381 = CARTESIAN_POINT ( 'NONE',  ( 4.303969348037258058, 8.413118729224057901, 47.36875205922775933 ) ) ;
#45382 = DIRECTION ( 'NONE',  ( -1.000000000000000000, 0.000000000000000000, -0.000000000000000000 ) ) ;
#45383 = VERTEX_POINT ( 'NONE', #2696 ) ;
#45384 = FACE_OUTER_BOUND ( 'NONE', #12629, .T. ) ;
#45385 = CARTESIAN_POINT ( 'NONE',  ( 0.5832655196449136881, 36.66244123469611083, 29.24210296277925281 ) ) ;
#45387 = EDGE_CURVE ( 'NONE', #14444, #30313, #30907, .T. ) ;
#45386 = CARTESIAN_POINT ( 'NONE',  ( 5.910764540655178756, 16.57257352145957086, -11.39522028505724904 ) ) ;
#45388 = CARTESIAN_POINT ( 'NONE',  ( 4.963659409799324962, -42.22332985082299928, -14.83726297270324856 ) ) ;
#45389 = FACE_OUTER_BOUND ( 'NONE', #21790, .T. ) ;
#45390 = CARTESIAN_POINT ( 'NONE',  ( 0.6021447746440204973, 4.975436559605085129, 48.85474562547464217 ) ) ;
#45391 = SURFACE_STYLE_USAGE ( .BOTH. , #59449 ) ;
#45392 = CARTESIAN_POINT ( 'NONE',  ( 0.1129192098497447394, -13.01845098534572820, -42.16007260106777466 ) ) ;
#45393 = CARTESIAN_POINT ( 'NONE',  ( 1.231276596079881935, -34.07446381689681658, -24.41736444846283405 ) ) ;
#45394 = CARTESIAN_POINT ( 'NONE',  ( 5.958863334805807099, -2.680345151634473400, -20.34989385289156871 ) ) ;
#45395 =( BOUNDED_SURFACE ( )  B_SPLINE_SURFACE ( 3, 1, ( 
 ( #32159, #27442 ),
 ( #41883, #60951 ),
 ( #47802, #42804 ),
 ( #42496, #14294 ) ),
 .UNSPECIFIED., .F., .F., .F. ) 
 B_SPLINE_SURFACE_WITH_KNOTS ( ( 4, 4 ),
 ( 2, 2 ),
 ( 0.000000000000000000, 1.000000000000000000 ),
 ( 0.000000000000000000, 1.000000000000000000 ),
 .UNSPECIFIED. ) 
 GEOMETRIC_REPRESENTATION_ITEM ( )  RATIONAL_B_SPLINE_SURFACE ( (
 ( 1.000000000000000000, 1.000000000000000000),
 ( 0.7211978278499970862, 0.9934217856018976445),
 ( 0.7211978278499970862, 0.9934217856018976445),
 ( 1.000000000000000000, 1.000000000000000000) ) ) 
 REPRESENTATION_ITEM ( '' )  SURFACE ( )  );
#45396 = CARTESIAN_POINT ( 'NONE',  ( 0.8557997880470697982, 47.37054680076715840, -7.156447707085226817 ) ) ;
#45397 = CARTESIAN_POINT ( 'NONE',  ( 1.231276596079881935, 35.62927148397020005, 22.08691432816306133 ) ) ;
#45398 = CARTESIAN_POINT ( 'NONE',  ( 0.5809828226811553087, -24.41822904836894637, -41.20389530892332886 ) ) ;
#45399 = CIRCLE ( 'NONE', #13370, 85.00000000000001421 ) ;
#45400 = CARTESIAN_POINT ( 'NONE',  ( 0.7242486021783829386, 40.69929259474984207, 27.46960219335028697 ) ) ;
#45401 = CARTESIAN_POINT ( 'NONE',  ( 1.000433927950264756, 38.83647759869904803, 15.75267232499282244 ) ) ;
#45402 = ORIENTED_EDGE ( 'NONE', *, *, #25635, .T. ) ;
#45403 = CARTESIAN_POINT ( 'NONE',  ( 0.1100247026804066219, 11.32523219034908202, -41.61078157869240357 ) ) ;
#45404 = CARTESIAN_POINT ( 'NONE',  ( 0.7762777257811903642, 5.369627942761623807, 47.60264404062380095 ) ) ;
#45405 = CARTESIAN_POINT ( 'NONE',  ( 0.9756008150404600343, -26.23365443298895272, -33.95486284030252477 ) ) ;
#45406 = CARTESIAN_POINT ( 'NONE',  ( 0.8557997880470697982, 28.43566216845025352, -38.55640757422408882 ) ) ;
#45407 = CARTESIAN_POINT ( 'NONE',  ( 5.895596859100789899, -19.93295055289972950, -2.684337063064522244 ) ) ;
#45408 = VERTEX_POINT ( 'NONE', #31220 ) ;
#45409 = EDGE_CURVE ( 'NONE', #4875, #50598, #11504, .T. ) ;
#45410 = CARTESIAN_POINT ( 'NONE',  ( 0.8751705887134423323, 29.98056538504960855, -37.60752970653798855 ) ) ;
#45411 = CARTESIAN_POINT ( 'NONE',  ( 4.960156602257182357, -46.35381625054458254, 2.524999074837397828 ) ) ;
#45412 = CIRCLE ( 'NONE', #53377, 47.09074272231896430 ) ;
#45413 = ADVANCED_FACE ( 'NONE', ( #26514 ), #58772, .F. ) ;
#45414 = CARTESIAN_POINT ( 'NONE',  ( 0.6028777368367060907, -14.05586561488587272, 47.05286889369597247 ) ) ;
#45415 = ORIENTED_EDGE ( 'NONE', *, *, #49081, .T. ) ;
#45416 = EDGE_CURVE ( 'NONE', #27464, #28142, #50021, .T. ) ;
#45417 = CARTESIAN_POINT ( 'NONE',  ( 3.238741278300274029, 42.95313747363661605, 1.828728677531976210 ) ) ;
#45418 = ORIENTED_EDGE ( 'NONE', *, *, #51184, .F. ) ;
#45419 = DIRECTION ( 'NONE',  ( -1.000000000000000000, -0.000000000000000000, -0.000000000000000000 ) ) ;
#45420 = CARTESIAN_POINT ( 'NONE',  ( 5.838029081930955932, -10.93035914537670905, -45.95206531926502436 ) ) ;
#45421 = ORIENTED_EDGE ( 'NONE', *, *, #14435, .F. ) ;
#45422 = CARTESIAN_POINT ( 'NONE',  ( 5.880360259849739535, -43.04573319267431231, -21.17507050419500558 ) ) ;
#45423 = VERTEX_POINT ( 'NONE', #6762 ) ;
#45424 = CARTESIAN_POINT ( 'NONE',  ( 0.9762797500689124330, 35.79768877047958853, 21.79105926469807741 ) ) ;
#45425 = CARTESIAN_POINT ( 'NONE',  ( 0.1158816050234199313, 20.41415249631641515, 39.11782738295033823 ) ) ;
#45426 = ORIENTED_EDGE ( 'NONE', *, *, #53932, .F. ) ;
#45427 = ORIENTED_EDGE ( 'NONE', *, *, #44635, .T. ) ;
#45429 = B_SPLINE_CURVE_WITH_KNOTS ( 'NONE', 3,
 ( #61775, #38038, #9798, #56474, #38637, #47404 ),
 .UNSPECIFIED., .F., .F.,
 ( 4, 2, 4 ),
 ( 1.553373257785006303E-17, 0.0002293755540694304511, 0.0004587511081388453982 ),
 .UNSPECIFIED. ) ;
#45428 = CARTESIAN_POINT ( 'NONE',  ( 5.910764540655178756, -9.679148173056805859, -17.62995544841716367 ) ) ;
#45430 = ORIENTED_EDGE ( 'NONE', *, *, #34604, .F. ) ;
#45431 = CARTESIAN_POINT ( 'NONE',  ( 0.5827359174754834781, -37.77623182210375319, -29.44457394064658828 ) ) ;
#45432 = VERTEX_POINT ( 'NONE', #44726 ) ;
#45433 = ADVANCED_FACE ( 'NONE', ( #35636 ), #25971, .F. ) ;
#45434 = EDGE_LOOP ( 'NONE', ( #4782, #43267, #35580, #19533 ) ) ;
#45435 = CARTESIAN_POINT ( 'NONE',  ( 2.648799415243696664, 12.25810282899351300, -47.47900987092526748 ) ) ;
#45436 = CARTESIAN_POINT ( 'NONE',  ( 0.7057020205115018818, 43.92641219669830832, 19.10543569325809798 ) ) ;
#45437 = CARTESIAN_POINT ( 'NONE',  ( 4.975801465491694664, -3.702618843597810905, 47.76942479135478692 ) ) ;
#45438 = CARTESIAN_POINT ( 'NONE',  ( 2.618530812446115519, -43.92476656374616084, 16.74340680741547160 ) ) ;
#45439 = CARTESIAN_POINT ( 'NONE',  ( 0.6029303876144825880, 44.39523326884611265, 18.53079182983359985 ) ) ;
#45440 = ORIENTED_EDGE ( 'NONE', *, *, #2554, .T. ) ;
#45441 = CARTESIAN_POINT ( 'NONE',  ( 4.963659409799330291, -36.94443854030240004, 25.25989740981486165 ) ) ;
#45442 = CARTESIAN_POINT ( 'NONE',  ( 5.860006189529246790, -3.171667470662847599, 48.12869875779307449 ) ) ;
#45443 = CARTESIAN_POINT ( 'NONE',  ( 0.5827359174754803695, -44.38786494726110732, 17.99288944686878722 ) ) ;
#45444 = B_SPLINE_CURVE_WITH_KNOTS ( 'NONE', 3,
 ( #13292, #32400, #51471, #8565 ),
 .UNSPECIFIED., .F., .F.,
 ( 4, 4 ),
 ( 0.000000000000000000, 0.005014147105413701254 ),
 .UNSPECIFIED. ) ;
#45445 = ORIENTED_EDGE ( 'NONE', *, *, #15908, .T. ) ;
#45446 = EDGE_CURVE ( 'NONE', #54914, #42575, #16724, .T. ) ;
#45447 = ORIENTED_EDGE ( 'NONE', *, *, #43734, .T. ) ;
#45448 = CARTESIAN_POINT ( 'NONE',  ( 0.8744876279028306332, 11.79038800009151089, 47.65854384249261244 ) ) ;
#45449 = CARTESIAN_POINT ( 'NONE',  ( 4.322998006666165516, -8.359821156456828106, 47.25487450103521070 ) ) ;
#45450 = CARTESIAN_POINT ( 'NONE',  ( 4.956445790443991584, 29.98832127573247774, 36.30755619981999871 ) ) ;
#45451 = ORIENTED_EDGE ( 'NONE', *, *, #419, .T. ) ;
#45452 = CARTESIAN_POINT ( 'NONE',  ( 1.827119703190778432, -29.55676396270206041, 31.30004882613791750 ) ) ;
#45453 = CARTESIAN_POINT ( 'NONE',  ( 1.231276596079887931, 8.892602616354244205, -40.96581977363174332 ) ) ;
#45454 = CARTESIAN_POINT ( 'NONE',  ( 0.6030672727741701600, -29.21669544497223470, -38.21927534816974514 ) ) ;
#45455 = B_SPLINE_CURVE_WITH_KNOTS ( 'NONE', 3,
 ( #30631, #21250, #41605, #50363, #35989, #21559, #59763, #31892, #12178, #41010, #11553, #16874, #46304, #2114, #40382, #16552 ),
 .UNSPECIFIED., .F., .F.,
 ( 4, 3, 3, 3, 3, 4 ),
 ( 2.194378057379452319E-17, 0.0002612764279487742470, 0.0003919131003184743662, 0.0005225497727000644969, 0.0007837925190632463301, 0.001045051706266715650 ),
 .UNSPECIFIED. ) ;
#45456 = ORIENTED_EDGE ( 'NONE', *, *, #52188, .T. ) ;
#45457 = CARTESIAN_POINT ( 'NONE',  ( 0.8760168074887076939, 38.69913431881784049, 28.57146030081993615 ) ) ;
#45458 = ORIENTED_EDGE ( 'NONE', *, *, #21042, .T. ) ;
#45459 = CARTESIAN_POINT ( 'NONE',  ( -6.078726893082806448, 18.62710865126535253, -4.881072071038842886 ) ) ;
#45461 = EDGE_CURVE ( 'NONE', #23080, #12149, #21271, .T. ) ;
#45460 = CARTESIAN_POINT ( 'NONE',  ( 0.9757402383260946888, -34.09320464257829286, 26.05362288587352637 ) ) ;
#45462 = VECTOR ( 'NONE', #41827, 999.9999999999998863 ) ;
#45463 = CARTESIAN_POINT ( 'NONE',  ( 5.959828726073459926, 17.77343634131841910, -10.26672511661737452 ) ) ;
#45464 = CARTESIAN_POINT ( 'NONE',  ( 0.5999999999999994227, -11.64055411052240352, 0.000000000000000000 ) ) ;
#45465 = EDGE_LOOP ( 'NONE', ( #2165, #24620, #54605, #26420 ) ) ;
#45466 = CARTESIAN_POINT ( 'NONE',  ( 0.9747592971366241255, 21.17324310849283719, -37.32069240268748445 ) ) ;
#45467 = CARTESIAN_POINT ( 'NONE',  ( -6.077587904424778920, 0.6233693561568425245, 19.24597183931575373 ) ) ;
#45468 = CARTESIAN_POINT ( 'NONE',  ( 0.1365634738349421895, 9.196489050310102442, 43.15422585067162942 ) ) ;
#45469 = CARTESIAN_POINT ( 'NONE',  ( 0.9762797500689124330, 14.58899758184696971, -39.28722355604386252 ) ) ;
#45470 = CARTESIAN_POINT ( 'NONE',  ( 0.8560838555295158248, -38.14845555156047396, -27.29593693413630362 ) ) ;
#45471 = FACE_OUTER_BOUND ( 'NONE', #17170, .T. ) ;
#45472 = CARTESIAN_POINT ( 'NONE',  ( 3.660176727303410260, -43.62748706623509065, -20.10773453922334042 ) ) ;
#45473 = B_SPLINE_CURVE_WITH_KNOTS ( 'NONE', 3,
 ( #4979, #42619, #33531, #27889 ),
 .UNSPECIFIED., .F., .F.,
 ( 4, 4 ),
 ( 6.505213034913026604E-19, 0.004048833967417085622 ),
 .UNSPECIFIED. ) ;
#45474 = CARTESIAN_POINT ( 'NONE',  ( 2.618530812446115519, 45.68928551531443105, 11.05513357215908599 ) ) ;
#45475 = DIRECTION ( 'NONE',  ( 0.000000000000000000, 0.000000000000000000, 1.000000000000000000 ) ) ;
#45476 = ORIENTED_EDGE ( 'NONE', *, *, #33498, .T. ) ;
#45477 = DIRECTION ( 'NONE',  ( 0.07439287786467665975, -0.9971416435352943308, -0.01320009283086585709 ) ) ;
#45478 = DIRECTION ( 'NONE',  ( 0.000000000000000000, 0.000000000000000000, 1.000000000000000000 ) ) ;
#45479 = CARTESIAN_POINT ( 'NONE',  ( 0.5549461598389365813, -42.43107887862065297, 12.03416971224342014 ) ) ;
#45480 = VERTEX_POINT ( 'NONE', #51235 ) ;
#45481 = EDGE_CURVE ( 'NONE', #52654, #16193, #22131, .T. ) ;
#45482 = CARTESIAN_POINT ( 'NONE',  ( 0.8551540677456739292, -11.51835730326447838, -46.51172240253133339 ) ) ;
#45483 = CARTESIAN_POINT ( 'NONE',  ( 0.8744876279028263033, 44.61213666265857825, -20.49651952824592982 ) ) ;
#45484 = ADVANCED_FACE ( 'NONE', ( #60626 ), #28920, .F. ) ;
#45485 =( BOUNDED_SURFACE ( )  B_SPLINE_SURFACE ( 3, 1, ( 
 ( #48375, #61305 ),
 ( #41618, #22804 ),
 ( #51595, #13114 ),
 ( #18421, #37542 ) ),
 .UNSPECIFIED., .F., .F., .F. ) 
 B_SPLINE_SURFACE_WITH_KNOTS ( ( 4, 4 ),
 ( 2, 2 ),
 ( 0.000000000000000000, 1.000000000000000000 ),
 ( 0.000000000000000000, 1.000000000000000000 ),
 .UNSPECIFIED. ) 
 GEOMETRIC_REPRESENTATION_ITEM ( )  RATIONAL_B_SPLINE_SURFACE ( (
 ( 1.000000000000000000, 1.000000000000000000),
 ( 0.9953390228620291325, 0.8624445117760984880),
 ( 0.9953390228620291325, 0.8624445117760984880),
 ( 1.000000000000000000, 1.000000000000000000) ) ) 
 REPRESENTATION_ITEM ( '' )  SURFACE ( )  );
#45486 = VERTEX_POINT ( 'NONE', #60319 ) ;
#45487 = CARTESIAN_POINT ( 'NONE',  ( 0.5987334363312687424, -45.28813410862901634, -18.98809667741633334 ) ) ;
#45488 = CARTESIAN_POINT ( 'NONE',  ( -6.016489644550737204, -13.32104266208090060, -13.32727118274452138 ) ) ;
#45489 = TOROIDAL_SURFACE ( 'NONE', #59452, 5.100000000000000533, 0.09999999999999982514 ) ;
#45490 = EDGE_CURVE ( 'NONE', #60982, #10029, #29473, .T. ) ;
#45491 = EDGE_LOOP ( 'NONE', ( #50254, #51276, #51065, #57534, #52801, #11612, #33882, #7964, #34940, #42553, #60733, #60380, #2322, #35014, #60702, #35787 ) ) ;
#45492 = CARTESIAN_POINT ( 'NONE',  ( 0.7044674535453004927, 11.74740322167597029, 47.68439199946104878 ) ) ;
#45493 = ADVANCED_FACE ( 'NONE', ( #31848 ), #46150, .F. ) ;
#45494 = ORIENTED_EDGE ( 'NONE', *, *, #44332, .F. ) ;
#45495 = ORIENTED_EDGE ( 'NONE', *, *, #17089, .T. ) ;
#45496 = CARTESIAN_POINT ( 'NONE',  ( 0.9754642270333695464, -5.774842730422326653, 42.51806607596982701 ) ) ;
#45497 = ORIENTED_EDGE ( 'NONE', *, *, #7195, .T. ) ;
#45498 = CARTESIAN_POINT ( 'NONE',  ( 0.6254311100348659558, 42.00127298835423773, -23.45480814408383807 ) ) ;
#45499 = AXIS2_PLACEMENT_3D ( 'NONE', #13392, #33118, #61885 ) ;
#45500 = ORIENTED_EDGE ( 'NONE', *, *, #34820, .T. ) ;
#45501 = CARTESIAN_POINT ( 'NONE',  ( 4.956445790444004018, -47.08764048036452721, 0.5405220916596411573 ) ) ;
#45502 =( BOUNDED_SURFACE ( )  B_SPLINE_SURFACE ( 3, 1, ( 
 ( #25529, #11761 ),
 ( #50264, #39661 ),
 ( #21145, #34953 ),
 ( #15531, #45585 ) ),
 .UNSPECIFIED., .F., .F., .F. ) 
 B_SPLINE_SURFACE_WITH_KNOTS ( ( 4, 4 ),
 ( 2, 2 ),
 ( 0.000000000000000000, 1.000000000000000000 ),
 ( 0.000000000000000000, 1.000000000000000000 ),
 .UNSPECIFIED. ) 
 GEOMETRIC_REPRESENTATION_ITEM ( )  RATIONAL_B_SPLINE_SURFACE ( (
 ( 1.000000000000000000, 1.000000000000000000),
 ( 0.9952954269826590483, 0.8620686068821307169),
 ( 0.9952954269826590483, 0.8620686068821307169),
 ( 1.000000000000000000, 1.000000000000000000) ) ) 
 REPRESENTATION_ITEM ( '' )  SURFACE ( )  );
#45503 = EDGE_CURVE ( 'NONE', #35346, #57844, #11508, .T. ) ;
#45504 = CARTESIAN_POINT ( 'NONE',  ( 0.9741495583595169983, 16.05424148287325892, 39.79188455996722951 ) ) ;
#45505 = ADVANCED_FACE ( 'NONE', ( #56556 ), #27280, .F. ) ;
#45506 = ORIENTED_EDGE ( 'NONE', *, *, #35747, .T. ) ;
#45507 = DIRECTION ( 'NONE',  ( 0.000000000000000000, 1.000000000000000000, 0.000000000000000000 ) ) ;
#45508 = CARTESIAN_POINT ( 'NONE',  ( 3.407937589446174087, -10.58239600294632865, -8.699069120706878877 ) ) ;
#45509 = CARTESIAN_POINT ( 'NONE',  ( 2.009741617377216460, -37.68148372272431601, 22.79495255702692091 ) ) ;
#45510 = CARTESIAN_POINT ( 'NONE',  ( 0.5817217712918331118, -30.62363249491660966, 35.51658889624201265 ) ) ;
#45511 = VERTEX_POINT ( 'NONE', #28064 ) ;
#45512 = ORIENTED_EDGE ( 'NONE', *, *, #40163, .F. ) ;
#45513 = CARTESIAN_POINT ( 'NONE',  ( 0.1098349054025745952, 41.59932877996182299, 11.36734385884019360 ) ) ;
#45514 = CARTESIAN_POINT ( 'NONE',  ( 0.9756008150404602564, 26.23365443298915878, 33.95486284030234714 ) ) ;
#45515 = CONICAL_SURFACE ( 'NONE', #9446, 42.92674063221959813, 1.485477209440487556 ) ;
#45516 = CARTESIAN_POINT ( 'NONE',  ( 4.226256110419179812, 12.89805166227863253, -42.00556526585945960 ) ) ;
#45517 = VERTEX_POINT ( 'NONE', #8632 ) ;
#45518 = DIRECTION ( 'NONE',  ( 2.168404344971009361E-16, -1.000000000000000000, 0.000000000000000000 ) ) ;
#45519 = CARTESIAN_POINT ( 'NONE',  ( 2.706805983486679779, 8.171905273964574334, -43.24345126736654521 ) ) ;
#45520 = CARTESIAN_POINT ( 'NONE',  ( 2.643462169533600914, 28.13401304854668084, 38.93558293168548090 ) ) ;
#45521 = ORIENTED_EDGE ( 'NONE', *, *, #42372, .F. ) ;
#45522 = ORIENTED_EDGE ( 'NONE', *, *, #21466, .F. ) ;
#45523 = CARTESIAN_POINT ( 'NONE',  ( 0.5782707292762423457, -0.8434722838406086831, 46.89376193284147121 ) ) ;
#45524 = CARTESIAN_POINT ( 'NONE',  ( 1.296416391601052709, 42.16328716573016777, 12.82827305042783550 ) ) ;
#45525 = CARTESIAN_POINT ( 'NONE',  ( -5.272380000000000067, 0.000000000000000000, 0.000000000000000000 ) ) ;
#45527 = EDGE_CURVE ( 'NONE', #17512, #3481, #42161, .T. ) ;
#45526 = CARTESIAN_POINT ( 'NONE',  ( 0.6009453534118438522, 6.711694149738223203, -47.63713118507420319 ) ) ;
#45528 = EDGE_CURVE ( 'NONE', #60472, #45275, #7945, .T. ) ;
#45529 = FACE_OUTER_BOUND ( 'NONE', #1362, .T. ) ;
#45530 = VECTOR ( 'NONE', #1878, 1000.000000000000000 ) ;
#45531 = FACE_OUTER_BOUND ( 'NONE', #35474, .T. ) ;
#45532 = CARTESIAN_POINT ( 'NONE',  ( 0.6023142530420679819, 12.19802990522800812, -46.53533807097419128 ) ) ;
#45533 = CARTESIAN_POINT ( 'NONE',  ( 0.5806925824938494740, 46.54710689580857519, 5.708695295225819422 ) ) ;
#45534 = CIRCLE ( 'NONE', #21500, 48.09070567114147110 ) ;
#45535 = CARTESIAN_POINT ( 'NONE',  ( 1.088313998177381725, 4.827222641555231064, 42.64115081428565190 ) ) ;
#45536 = CARTESIAN_POINT ( 'NONE',  ( 0.9762797500689124330, -6.471194619075845367, 41.40589843715202534 ) ) ;
#45537 = CARTESIAN_POINT ( 'NONE',  ( 5.880360259849739535, 36.09847387447815947, 31.59460303415995241 ) ) ;
#45538 = AXIS2_PLACEMENT_3D ( 'NONE', #54387, #1773, #35641 ) ;
#45539 = DIRECTION ( 'NONE',  ( 0.000000000000000000, 0.000000000000000000, 1.000000000000000000 ) ) ;
#45540 = CARTESIAN_POINT ( 'NONE',  ( 0.8744876279028263033, 10.05549467470504865, 48.05452192277508061 ) ) ;
#45541 = CARTESIAN_POINT ( 'NONE',  ( 4.975610109902397937, 47.16372689271652519, 12.96272628450595832 ) ) ;
#45542 = CARTESIAN_POINT ( 'NONE',  ( 0.9762797500689124330, -22.12212327108638377, 35.59405072711678741 ) ) ;
#45543 = B_SPLINE_CURVE_WITH_KNOTS ( 'NONE', 3,
 ( #8805, #54935, #27921, #35866, #9110, #18845 ),
 .UNSPECIFIED., .F., .F.,
 ( 4, 2, 4 ),
 ( 1.084202172485504314E-19, 0.0002291966416970794037, 0.0004583932833941586991 ),
 .UNSPECIFIED. ) ;
#45544 = CARTESIAN_POINT ( 'NONE',  ( 5.981074661064941900, -18.95903134304784032, -7.862380442164075056 ) ) ;
#45545 = CARTESIAN_POINT ( 'NONE',  ( 0.7057020205115008826, -43.92641219669816621, -19.10543569325839286 ) ) ;
#45546 = CARTESIAN_POINT ( 'NONE',  ( 3.407937589446178528, 12.47329436636636935, -5.663729899984937255 ) ) ;
#45548 = ORIENTED_EDGE ( 'NONE', *, *, #25512, .T. ) ;
#45547 = CARTESIAN_POINT ( 'NONE',  ( 5.895596859100789899, 17.95274561709302930, 9.067916410093047830 ) ) ;
#45549 = ORIENTED_EDGE ( 'NONE', *, *, #7696, .T. ) ;
#45550 = CARTESIAN_POINT ( 'NONE',  ( 1.157643937452369265, -11.62785187674113097, 40.27152015168191213 ) ) ;
#45551 = CARTESIAN_POINT ( 'NONE',  ( 1.112077966505211624, 3.186402742498017027, -43.96449889048157189 ) ) ;
#45552 = CARTESIAN_POINT ( 'NONE',  ( 0.8760168074887090262, 34.63873394077441503, 33.37827814204137411 ) ) ;
#45553 = VERTEX_POINT ( 'NONE', #38723 ) ;
#45554 = VERTEX_POINT ( 'NONE', #5155 ) ;
#45555 = CARTESIAN_POINT ( 'NONE',  ( 3.238931869106854489, 42.34694073502591039, -7.419701784410695389 ) ) ;
#45556 = CARTESIAN_POINT ( 'NONE',  ( 0.1097557419366048670, -37.23482781437660805, 21.75515245866060354 ) ) ;
#45557 = EDGE_CURVE ( 'NONE', #55904, #46829, #30913, .T. ) ;
#45558 = ORIENTED_EDGE ( 'NONE', *, *, #11551, .F. ) ;
#45559 = VERTEX_POINT ( 'NONE', #34016 ) ;
#45560 = CARTESIAN_POINT ( 'NONE',  ( 0.5839254288179548391, 47.89590036163257736, 0.09078831291240967161 ) ) ;
#45561 = ADVANCED_FACE ( 'NONE', ( #42799 ), #12119, .F. ) ;
#45562 = ADVANCED_FACE ( 'NONE', ( #38112 ), #23979, .F. ) ;
#45563 = CARTESIAN_POINT ( 'NONE',  ( 4.956653778116975495, -9.917440902361487787, 47.05699031914946318 ) ) ;
#45564 = CARTESIAN_POINT ( 'NONE',  ( 0.5980271706414711508, 46.82647351461041296, -14.80981502339418476 ) ) ;
#45565 = EDGE_CURVE ( 'NONE', #47165, #18280, #9279, .T. ) ;
#45566 = VERTEX_POINT ( 'NONE', #13989 ) ;
#45567 = CARTESIAN_POINT ( 'NONE',  ( -6.016489644550736315, -2.455165042129866748, 18.68257207665195452 ) ) ;
#45568 = DIRECTION ( 'NONE',  ( -1.000000000000000000, -0.000000000000000000, -0.000000000000000000 ) ) ;
#45569 = VECTOR ( 'NONE', #17513, 1000.000000000000114 ) ;
#45570 = EDGE_LOOP ( 'NONE', ( #15058, #21535, #44746, #15227 ) ) ;
#45571 = VERTEX_POINT ( 'NONE', #9256 ) ;
#45572 = DIRECTION ( 'NONE',  ( -0.1011922191286467460, 0.2707140367831962213, 0.9573265091265185101 ) ) ;
#45573 = CARTESIAN_POINT ( 'NONE',  ( 4.967162193818130511, -7.970725651239513709, -42.34252806656601820 ) ) ;
#45574 = AXIS2_PLACEMENT_3D ( 'NONE', #49309, #44638, #30499 ) ;
#45575 = ORIENTED_EDGE ( 'NONE', *, *, #25500, .F. ) ;
#45576 = CARTESIAN_POINT ( 'NONE',  ( 0.5809828226811556418, 44.03860873105722362, -18.83114015454650314 ) ) ;
#45577 = DIRECTION ( 'NONE',  ( -1.000000000000000000, -0.000000000000000000, -0.000000000000000000 ) ) ;
#45578 = CARTESIAN_POINT ( 'NONE',  ( 2.282816707992318506, 15.64995451397235904, -44.28968153101309468 ) ) ;
#45579 = CARTESIAN_POINT ( 'NONE',  ( 2.185380717157383135, -43.83117064034907173, -4.200985999000810267 ) ) ;
#45580 = CONICAL_SURFACE ( 'NONE', #19556, 43.08621763946400307, 1.568696531533066763 ) ;
#45581 = ORIENTED_EDGE ( 'NONE', *, *, #17535, .F. ) ;
#45582 = FACE_OUTER_BOUND ( 'NONE', #27529, .T. ) ;
#45583 = CARTESIAN_POINT ( 'NONE',  ( 5.895596859100789899, 5.962379729972213660, -19.20880556328539512 ) ) ;
#45584 = CARTESIAN_POINT ( 'NONE',  ( 4.956445790443988031, 0.000000000000000000, 0.000000000000000000 ) ) ;
#45585 = CARTESIAN_POINT ( 'NONE',  ( 0.5804410086790514622, -42.10186154173658224, -20.66284362269237462 ) ) ;
#45586 = VERTEX_POINT ( 'NONE', #24917 ) ;
#45587 = CARTESIAN_POINT ( 'NONE',  ( -7.459310946700270506E-14, -4.618802153517020948, -5.242734410091827613 ) ) ;
#45588 = CARTESIAN_POINT ( 'NONE',  ( 5.959828726073459926, 2.683617577144109756, 20.34941966491240350 ) ) ;
#45589 = CARTESIAN_POINT ( 'NONE',  ( 0.3622758884714600280, 25.58609868863721459, 34.70015533914837391 ) ) ;
#45590 = CARTESIAN_POINT ( 'NONE',  ( 0.9968887458511644928, 36.82760690604627030, 22.02152923727763678 ) ) ;
#45591 = VERTEX_POINT ( 'NONE', #38408 ) ;
#45592 = LINE ( 'NONE', #54641, #25883 ) ;
#45593 = CARTESIAN_POINT ( 'NONE',  ( 4.962356264823608143, 7.429277797797782412, -41.42513040734446861 ) ) ;
#45594 = CARTESIAN_POINT ( 'NONE',  ( -6.077587904424778920, 0.6110050725292486273, -19.24636833782607681 ) ) ;
#45595 = CARTESIAN_POINT ( 'NONE',  ( 5.895596859100789899, -13.97974974393952508, -14.46010996878344201 ) ) ;
#45596 = CARTESIAN_POINT ( 'NONE',  ( -31.75000000000000000, -16.00000000000000000, 1.959434878635765131E-15 ) ) ;
#45597 =( REPRESENTATION_RELATIONSHIP ('NONE','NONE', #44881, #53251 ) REPRESENTATION_RELATIONSHIP_WITH_TRANSFORMATION ( #20191 )SHAPE_REPRESENTATION_RELATIONSHIP( ) );
#45598 = CARTESIAN_POINT ( 'NONE',  ( 0.8554163680231720024, 16.00619315955243849, -44.10223637924629259 ) ) ;
#45599 =( BOUNDED_SURFACE ( )  B_SPLINE_SURFACE ( 3, 1, ( 
 ( #51379, #8465 ),
 ( #37318, #61390 ),
 ( #13505, #27594 ),
 ( #46720, #3763 ) ),
 .UNSPECIFIED., .F., .F., .F. ) 
 B_SPLINE_SURFACE_WITH_KNOTS ( ( 4, 4 ),
 ( 2, 2 ),
 ( 0.000000000000000000, 1.000000000000000000 ),
 ( 0.000000000000000000, 1.000000000000000000 ),
 .UNSPECIFIED. ) 
 GEOMETRIC_REPRESENTATION_ITEM ( )  RATIONAL_B_SPLINE_SURFACE ( (
 ( 1.000000000000000000, 1.000000000000000000),
 ( 0.9953040768229005630, 0.8617119497784937465),
 ( 0.9953040768229005630, 0.8617119497784937465),
 ( 1.000000000000000000, 1.000000000000000000) ) ) 
 REPRESENTATION_ITEM ( '' )  SURFACE ( )  );
#45600 = EDGE_CURVE ( 'NONE', #31908, #9596, #48898, .T. ) ;
#45601 = CARTESIAN_POINT ( 'NONE',  ( 0.9752132459055834479, -5.831562321021290352, -42.51031254975327300 ) ) ;
#45602 = CARTESIAN_POINT ( 'NONE',  ( 1.479689385636123067, -32.45943909685134798, -29.79880297571515513 ) ) ;
#45603 = CARTESIAN_POINT ( 'NONE',  ( 0.5819845901640493535, 37.72030663501157477, 29.51612926147629778 ) ) ;
#45604 = CARTESIAN_POINT ( 'NONE',  ( 0.5850706913938533704, -23.79070617305352542, -41.56998471741253098 ) ) ;
#45605 = ORIENTED_EDGE ( 'NONE', *, *, #50084, .T. ) ;
#45606 = CARTESIAN_POINT ( 'NONE',  ( 0.7764139734771250412, -46.73184009015370322, -4.021889194790254862 ) ) ;
#45607 = CARTESIAN_POINT ( 'NONE',  ( 4.322998006666179727, 47.80838462754059748, 4.155494336618874129 ) ) ;
#45608 = CYLINDRICAL_SURFACE ( 'NONE', #45851, 2.649999999999992806 ) ;
#45609 = CARTESIAN_POINT ( 'NONE',  ( 2.526464513654346877, -37.81242626108682714, -20.43088802552603056 ) ) ;
#45610 = CARTESIAN_POINT ( 'NONE',  ( 0.6039202388192953519, -47.54548494440594197, -12.28782219314147639 ) ) ;
#45611 = CARTESIAN_POINT ( 'NONE',  ( 0.5807400328401637335, -47.55718917606846929, 5.711437504335787452 ) ) ;
#45612 = PRODUCT_CONTEXT ( 'NONE', #57535, 'mechanical' ) ;
#45613 = CARTESIAN_POINT ( 'NONE',  ( 1.227938101723748288, 4.762198645644436290, 42.65467462194920500 ) ) ;
#45614 = CARTESIAN_POINT ( 'NONE',  ( 5.838029081930955932, 7.876159563729716595, -46.57285871276948797 ) ) ;
#45615 = CARTESIAN_POINT ( 'NONE',  ( 0.6017667736363749853, 0.3491025323180517170, -48.10631678344241635 ) ) ;
#45617 = ORIENTED_EDGE ( 'NONE', *, *, #41395, .F. ) ;
#45616 = CARTESIAN_POINT ( 'NONE',  ( 4.834790513006555379, 24.09885983197582249, -40.64276437108040341 ) ) ;
#45618 = EDGE_LOOP ( 'NONE', ( #35671, #54065, #862, #55344 ) ) ;
#45619 = CARTESIAN_POINT ( 'NONE',  ( 0.000000000000000000, 0.6959691356230525150, 0.000000000000000000 ) ) ;
#45620 = VECTOR ( 'NONE', #39329, 1000.000000000000114 ) ;
#45621 = CARTESIAN_POINT ( 'NONE',  ( 0.5837800005270551429, -7.800150850987738416, 46.24276057226276748 ) ) ;
#45622 = DIRECTION ( 'NONE',  ( -0.1011922191286467598, -0.4715280952439284690, 0.8760259072558600479 ) ) ;
#45623 = EDGE_CURVE ( 'NONE', #30625, #50534, #40719, .T. ) ;
#45624 = VECTOR ( 'NONE', #55362, 999.9999999999998863 ) ;
#45625 = VERTEX_POINT ( 'NONE', #11745 ) ;
#45626 = CARTESIAN_POINT ( 'NONE',  ( -2.601141883200662974, 8.903211435100862658, 11.98032777561940776 ) ) ;
#45627 = CARTESIAN_POINT ( 'NONE',  ( 5.901463166500146684, 14.90686821212722357, -13.50196839156822648 ) ) ;
#45628 = CARTESIAN_POINT ( 'NONE',  ( -90.00000000000000000, 0.000000000000000000, 0.000000000000000000 ) ) ;
#45629 = EDGE_CURVE ( 'NONE', #40414, #29428, #42990, .T. ) ;
#45630 = ORIENTED_EDGE ( 'NONE', *, *, #57053, .F. ) ;
#45631 = EDGE_LOOP ( 'NONE', ( #10172, #34386, #27116, #39521 ) ) ;
#45632 = EDGE_CURVE ( 'NONE', #49021, #60939, #57078, .T. ) ;
#45633 = CARTESIAN_POINT ( 'NONE',  ( 0.7056555295713249354, -43.92642606846689546, 19.10539864320384495 ) ) ;
#45634 = VECTOR ( 'NONE', #56674, 1000.000000000000114 ) ;
#45635 = CARTESIAN_POINT ( 'NONE',  ( 0.8557997880470697982, -23.15977007032352475, 41.93815086860250574 ) ) ;
#45636 = CARTESIAN_POINT ( 'NONE',  ( 0.5998501479064699549, 41.92175333043586960, 23.59887241503369282 ) ) ;
#45637 = VERTEX_POINT ( 'NONE', #50249 ) ;
#45638 = ADVANCED_FACE ( 'NONE', ( #45270 ), #20513, .F. ) ;
#45639 = B_SPLINE_CURVE_WITH_KNOTS ( 'NONE', 3,
 ( #48241, #52924, #10028, #29122 ),
 .UNSPECIFIED., .F., .F.,
 ( 4, 4 ),
 ( 6.254634441385501517E-18, 0.004050076154993004218 ),
 .UNSPECIFIED. ) ;
#45640 = CARTESIAN_POINT ( 'NONE',  ( 0.6029443199889047422, 49.00651436223474633, 3.146298129307232294 ) ) ;
#45641 = CARTESIAN_POINT ( 'NONE',  ( 0.5988103622719989083, 0.6065097949913632602, -48.10388392585942796 ) ) ;
#45642 = ORIENTED_EDGE ( 'NONE', *, *, #28496, .T. ) ;
#45643 = CARTESIAN_POINT ( 'NONE',  ( 0.2940135542859022566, 33.06489085126945326, -29.20536837098717342 ) ) ;
#45644 = CARTESIAN_POINT ( 'NONE',  ( 3.270143674763207553, -2.058141141425694265, 13.53222904135353311 ) ) ;
#45645 = ORIENTED_EDGE ( 'NONE', *, *, #22806, .F. ) ;
#45646 = CARTESIAN_POINT ( 'NONE',  ( 4.956653778116975495, -35.79382859084138602, 32.11725092155030836 ) ) ;
#45647 = EDGE_CURVE ( 'NONE', #26055, #7202, #44376, .T. ) ;
#45648 = CARTESIAN_POINT ( 'NONE',  ( 0.3676999524040366896, -6.224421213753956295, 43.67158302462379282 ) ) ;
#45649 = ORIENTED_EDGE ( 'NONE', *, *, #51749, .T. ) ;
#45650 = CARTESIAN_POINT ( 'NONE',  ( 0.6039202388192953519, -8.009480623389540810, -48.45009734760640896 ) ) ;
#45651 = CARTESIAN_POINT ( 'NONE',  ( 3.783278058412227640, 24.80906179324491845, -35.16831859152105721 ) ) ;
#45652 = CARTESIAN_POINT ( 'NONE',  ( 5.860006189529246790, 43.26650951066899609, -21.31760477694535894 ) ) ;
#45653 = EDGE_CURVE ( 'NONE', #44540, #51774, #30210, .T. ) ;
#45654 = ORIENTED_EDGE ( 'NONE', *, *, #28104, .T. ) ;
#45655 = FACE_OUTER_BOUND ( 'NONE', #35757, .T. ) ;
#45656 = LINE ( 'NONE', #11516, #16015 ) ;
#45657 = B_SPLINE_CURVE_WITH_KNOTS ( 'NONE', 3,
 ( #28824, #47635, #10347, #5602 ),
 .UNSPECIFIED., .F., .F.,
 ( 4, 4 ),
 ( 6.992893892674702526E-18, 0.004050076154993007688 ),
 .UNSPECIFIED. ) ;
#45658 = ORIENTED_EDGE ( 'NONE', *, *, #44762, .F. ) ;
#45659 = CARTESIAN_POINT ( 'NONE',  ( 0.9972139404380298000, -15.81078898082016337, 39.89035676513732653 ) ) ;
#45660 = ORIENTED_EDGE ( 'NONE', *, *, #12560, .T. ) ;
#45661 = CARTESIAN_POINT ( 'NONE',  ( -4.908599999999998964, 0.000000000000000000, 0.000000000000000000 ) ) ;
#45662 = CIRCLE ( 'NONE', #31655, 42.08604991992415023 ) ;
#45663 = ORIENTED_EDGE ( 'NONE', *, *, #43504, .F. ) ;
#45664 = CARTESIAN_POINT ( 'NONE',  ( 0.5998501479064708430, 46.33007877220720871, 12.95623334615518374 ) ) ;
#45665 = CARTESIAN_POINT ( 'NONE',  ( 0.9772918015221165877, 25.19218625365867581, 33.49164981770307747 ) ) ;
#45666 = VECTOR ( 'NONE', #8326, 1000.000000000000227 ) ;
#45667 = CARTESIAN_POINT ( 'NONE',  ( 4.960156602257181468, 46.35381625054450438, 2.524999074837726010 ) ) ;
#45668 = ORIENTED_EDGE ( 'NONE', *, *, #43239, .F. ) ;
#45669 = CARTESIAN_POINT ( 'NONE',  ( 0.8760168074887076939, -44.09317760313766144, 19.22870327415225589 ) ) ;
#45670 = AXIS2_PLACEMENT_3D ( 'NONE', #9206, #37428, #27387 ) ;
#45671 = CARTESIAN_POINT ( 'NONE',  ( 0.5817216825391123836, -41.64824101621195496, 21.55594981583921310 ) ) ;
#45672 = ORIENTED_EDGE ( 'NONE', *, *, #22149, .F. ) ;
#45673 = VERTEX_POINT ( 'NONE', #49318 ) ;
#45674 =( BOUNDED_SURFACE ( )  B_SPLINE_SURFACE ( 3, 1, ( 
 ( #51968, #28167 ),
 ( #9676, #47285 ),
 ( #29095, #19708 ),
 ( #23781, #38833 ) ),
 .UNSPECIFIED., .F., .F., .F. ) 
 B_SPLINE_SURFACE_WITH_KNOTS ( ( 4, 4 ),
 ( 2, 2 ),
 ( 0.000000000000000000, 1.000000000000000000 ),
 ( 0.000000000000000000, 1.000000000000000000 ),
 .UNSPECIFIED. ) 
 GEOMETRIC_REPRESENTATION_ITEM ( )  RATIONAL_B_SPLINE_SURFACE ( (
 ( 1.000000000000000000, 1.000000000000000000),
 ( 0.9953390228620291325, 0.8624445117761032620),
 ( 0.9953390228620291325, 0.8624445117761032620),
 ( 1.000000000000000000, 1.000000000000000000) ) ) 
 REPRESENTATION_ITEM ( '' )  SURFACE ( )  );
#45675 = CARTESIAN_POINT ( 'NONE',  ( 4.975801465491694664, 35.64402118370912120, 32.01766832630325155 ) ) ;
#45676 = CARTESIAN_POINT ( 'NONE',  ( 4.956653778116992370, 14.93973939759951541, -45.71126949320233734 ) ) ;
#45677 = CARTESIAN_POINT ( 'NONE',  ( 0.9785694773339250752, 38.66954382086642994, -16.15554970902462983 ) ) ;
#45678 = CARTESIAN_POINT ( 'NONE',  ( 3.238741278300274473, -36.28414388564879545, -23.06029422818990682 ) ) ;
#45679 = EDGE_CURVE ( 'NONE', #59715, #19827, #2001, .T. ) ;
#45680 = CARTESIAN_POINT ( 'NONE',  ( 0.7056555295713263787, -44.57023068418414624, -17.55111680842085775 ) ) ;
#45681 = DIRECTION ( 'NONE',  ( 0.1011922191286468153, 0.9400526519483254351, -0.3256703031483533795 ) ) ;
#45682 = ORIENTED_EDGE ( 'NONE', *, *, #59158, .F. ) ;
#45683 = AXIS2_PLACEMENT_3D ( 'NONE', #39002, #44618, #24880 ) ;
#45684 = CARTESIAN_POINT ( 'NONE',  ( 4.975801465491695552, 46.87746200127456575, -9.906103548667728020 ) ) ;
#45685 = CARTESIAN_POINT ( 'NONE',  ( 1.399999999999999023, 0.000000000000000000, 0.000000000000000000 ) ) ;
#45686 = ORIENTED_EDGE ( 'NONE', *, *, #5865, .T. ) ;
#45687 = B_SPLINE_CURVE_WITH_KNOTS ( 'NONE', 3,
 ( #319, #52644, #34187, #42979, #53264, #9741 ),
 .UNSPECIFIED., .F., .F.,
 ( 4, 2, 4 ),
 ( 9.660965348001701796E-18, 0.0002448709889506563977, 0.0004897419779013031460 ),
 .UNSPECIFIED. ) ;
#45688 = CARTESIAN_POINT ( 'NONE',  ( 0.9754402186311934564, -30.20795797590421117, 30.47320128434250464 ) ) ;
#45689 = CARTESIAN_POINT ( 'NONE',  ( 30.00000000000001421, -18.99999999999999289, 2.326828918379969393E-15 ) ) ;
#45690 = CARTESIAN_POINT ( 'NONE',  ( 3.660087539127315992, 45.06758728829470328, 16.63102164621050960 ) ) ;
#45691 = CARTESIAN_POINT ( 'NONE',  ( 0.6846871229502932144, 24.69859318104546375, -41.05093867799160989 ) ) ;
#45692 = CARTESIAN_POINT ( 'NONE',  ( 0.8751705887134423323, -47.55935879196466232, -7.160166390004136794 ) ) ;
#45693 = CARTESIAN_POINT ( 'NONE',  ( 4.958415959904820092, 44.61026793747956276, -8.551488079212832716 ) ) ;
#45694 = CARTESIAN_POINT ( 'NONE',  ( 2.282803330402974673, 37.66448333203771170, -28.06926437916816397 ) ) ;
#45695 = SURFACE_STYLE_USAGE ( .BOTH. , #31269 ) ;
#45696 = CARTESIAN_POINT ( 'NONE',  ( 0.5806925824938499181, 10.33919002968644385, 45.74192291403583965 ) ) ;
#45697 = CARTESIAN_POINT ( 'NONE',  ( -6.078726893082806448, -11.01948708261720178, -15.79129335123480971 ) ) ;
#45698 = CARTESIAN_POINT ( 'NONE',  ( 0.2940133293163018635, 30.25014500077257651, -32.11182456682082176 ) ) ;
#45699 = CARTESIAN_POINT ( 'NONE',  ( 0.5987334363312688534, 4.112662775261645365, 48.93515005973777932 ) ) ;
#45700 = CARTESIAN_POINT ( 'NONE',  ( -6.077587904424778920, -18.27702681447043886, -6.061873655649631765 ) ) ;
#45701 = B_SPLINE_CURVE_WITH_KNOTS ( 'NONE', 3,
 ( #22499, #60688, #51294, #45704 ),
 .UNSPECIFIED., .F., .F.,
 ( 4, 4 ),
 ( 1.939025188362721105E-17, 0.004444306975806117631 ),
 .UNSPECIFIED. ) ;
#45702 = FACE_OUTER_BOUND ( 'NONE', #25445, .T. ) ;
#45703 = CARTESIAN_POINT ( 'NONE',  ( 0.5827357941260199459, -24.26189667804973027, -41.29633147056638620 ) ) ;
#45704 = CARTESIAN_POINT ( 'NONE',  ( 4.975801465491694664, -45.18341283946446651, -15.94009207553035523 ) ) ;
#45705 = CARTESIAN_POINT ( 'NONE',  ( 58.00000000000000000, 15.50000000000001066, 1.598617315530391440E-15 ) ) ;
#45706 = VERTEX_POINT ( 'NONE', #25510 ) ;
#45707 = B_SPLINE_CURVE_WITH_KNOTS ( 'NONE', 3,
 ( #58430, #48746, #25250, #10539 ),
 .UNSPECIFIED., .F., .F.,
 ( 4, 4 ),
 ( 0.000000000000000000, 0.005004948556313818311 ),
 .UNSPECIFIED. ) ;
#45708 = EDGE_CURVE ( 'NONE', #19210, #42430, #44647, .T. ) ;
#45709 = VECTOR ( 'NONE', #39360, 999.9999999999998863 ) ;
#45710 = CARTESIAN_POINT ( 'NONE',  ( 0.1081432562775997835, 11.56998286599535852, -41.54352569227150838 ) ) ;
#45711 = B_SPLINE_CURVE_WITH_KNOTS ( 'NONE', 3,
 ( #26317, #2181, #45452, #2501 ),
 .UNSPECIFIED., .F., .F.,
 ( 4, 4 ),
 ( 6.254634441385501517E-18, 0.004566006591234647236 ),
 .UNSPECIFIED. ) ;
#45712 = CARTESIAN_POINT ( 'NONE',  ( -6.077587904424778920, 5.472951620448720078, -18.46192898789718129 ) ) ;
#45713 = VECTOR ( 'NONE', #49855, 1000.000000000000114 ) ;
#45714 = CARTESIAN_POINT ( 'NONE',  ( 0.9730545539215883499, -26.52009130076748278, -33.73144377768585400 ) ) ;
#45715 = CARTESIAN_POINT ( 'NONE',  ( -6.063463321072278589, -12.95783560055447658, 14.24482183210702679 ) ) ;
#45716 = AXIS2_PLACEMENT_3D ( 'NONE', #26511, #45039, #55004 ) ;
#45717 = ORIENTED_EDGE ( 'NONE', *, *, #21092, .T. ) ;
#45718 = EDGE_CURVE ( 'NONE', #10248, #4699, #18957, .T. ) ;
#45719 = CARTESIAN_POINT ( 'NONE',  ( 5.860006189529246790, -48.13093674595587146, 3.137522369585352688 ) ) ;
#45720 = DIRECTION ( 'NONE',  ( 0.9848077530122080203, 0.1736481776669314692, -5.551115123125783935E-17 ) ) ;
#45721 = CARTESIAN_POINT ( 'NONE',  ( 0.1365634738349423560, 43.98722388068600253, 3.462189320886016386 ) ) ;
#45722 = EDGE_LOOP ( 'NONE', ( #28677, #42364, #13176, #51613 ) ) ;
#45723 = CARTESIAN_POINT ( 'NONE',  ( 0.8753041380234471980, 40.66072100792138144, 27.52896828776844629 ) ) ;
#45724 = ORIENTED_EDGE ( 'NONE', *, *, #10126, .T. ) ;
#45725 = CARTESIAN_POINT ( 'NONE',  ( 0.5809828226811617480, 46.40184912890855884, -11.86925843957117799 ) ) ;
#45726 = CARTESIAN_POINT ( 'NONE',  ( -6.017396004339687465, -13.32329839588545717, -13.32495836419638557 ) ) ;
#45727 = ORIENTED_EDGE ( 'NONE', *, *, #15136, .F. ) ;
#45728 = CARTESIAN_POINT ( 'NONE',  ( 5.901764892641307547, 1.612679500413873201, -48.94272910523709896 ) ) ;
#45729 = ORIENTED_EDGE ( 'NONE', *, *, #55858, .T. ) ;
#45730 = DIRECTION ( 'NONE',  ( 0.09722883295013595717, -0.7096678276952366193, -0.6977951908529310687 ) ) ;
#45731 = CARTESIAN_POINT ( 'NONE',  ( 0.1092565886968785149, -26.49813811968561694, -34.02318727879954707 ) ) ;
#45732 = ADVANCED_FACE ( 'NONE', ( #13595 ), #32703, .F. ) ;
#45733 = CIRCLE ( 'NONE', #58696, 15.14599999999999369 ) ;
#45734 = EDGE_LOOP ( 'NONE', ( #38341, #47644, #531, #6919 ) ) ;
#45735 = CARTESIAN_POINT ( 'NONE',  ( -6.015611763856276717, 9.416239407363534042, -16.32183393015586503 ) ) ;
#45736 = ORIENTED_EDGE ( 'NONE', *, *, #8681, .F. ) ;
#45737 = CARTESIAN_POINT ( 'NONE',  ( 4.553261556744875094, 0.000000000000000000, 0.000000000000000000 ) ) ;
#45738 = EDGE_LOOP ( 'NONE', ( #33323, #41482 ) ) ;
#45739 = ORIENTED_EDGE ( 'NONE', *, *, #14953, .T. ) ;
#45740 = CARTESIAN_POINT ( 'NONE',  ( 0.6041374136657475802, 23.90252055111265150, 41.74951251761581972 ) ) ;
#45741 = PLANE ( 'NONE',  #5384 ) ;
#45742 = CARTESIAN_POINT ( 'NONE',  ( 1.000433927950262980, -37.69758855726165336, -18.31148531988220896 ) ) ;
#45743 = CARTESIAN_POINT ( 'NONE',  ( 4.975610109902397937, 0.9924324126403755164, 48.90260202733708894 ) ) ;
#45744 = CARTESIAN_POINT ( 'NONE',  ( 4.963659409799330291, 37.47512675766694201, 24.46566636552837792 ) ) ;
#45745 = VERTEX_POINT ( 'NONE', #3235 ) ;
#45746 = CARTESIAN_POINT ( 'NONE',  ( 1.296416391601052709, 5.336661527168872432, 43.74731326402337572 ) ) ;
#45747 = CARTESIAN_POINT ( 'NONE',  ( 0.5836750258453351492, -44.31929073742205105, 18.16108240858330092 ) ) ;
#45748 = ORIENTED_EDGE ( 'NONE', *, *, #51915, .T. ) ;
#45749 = B_SPLINE_CURVE_WITH_KNOTS ( 'NONE', 3,
 ( #25202, #6369, #20823, #11423, #1998, #44346 ),
 .UNSPECIFIED., .F., .F.,
 ( 4, 2, 4 ),
 ( 1.910620358896493634E-17, 0.0002293755540694310746, 0.0004587511081388430129 ),
 .UNSPECIFIED. ) ;
#45750 = ORIENTED_EDGE ( 'NONE', *, *, #16762, .F. ) ;
#45751 = CARTESIAN_POINT ( 'NONE',  ( 0.6000166863083090663, 44.47108027094633087, -20.83618250168446195 ) ) ;
#45752 = CARTESIAN_POINT ( 'NONE',  ( 6.999999999999991118, 80.00000000000001421, -7.414830285890871171E-32 ) ) ;
#45753 = CARTESIAN_POINT ( 'NONE',  ( 0.8560838555295223751, 36.24009790160352651, -29.78301761346427767 ) ) ;
#45754 = ORIENTED_EDGE ( 'NONE', *, *, #34749, .T. ) ;
#45755 = CARTESIAN_POINT ( 'NONE',  ( 0.1097557419366048670, -42.78407272074154832, -5.407604117549557721 ) ) ;
#45756 = CARTESIAN_POINT ( 'NONE',  ( 0.9268187852002115479, -34.73073342105909944, 27.15751256915762113 ) ) ;
#45757 = AXIS2_PLACEMENT_3D ( 'NONE', #12147, #1775, #40657 ) ;
#45758 =( BOUNDED_SURFACE ( )  B_SPLINE_SURFACE ( 3, 1, ( 
 ( #41945, #17502 ),
 ( #17811, #32223 ),
 ( #32530, #23126 ),
 ( #36939, #8384 ) ),
 .UNSPECIFIED., .F., .F., .F. ) 
 B_SPLINE_SURFACE_WITH_KNOTS ( ( 4, 4 ),
 ( 2, 2 ),
 ( 0.000000000000000000, 1.000000000000000000 ),
 ( 0.000000000000000000, 1.000000000000000000 ),
 .UNSPECIFIED. ) 
 GEOMETRIC_REPRESENTATION_ITEM ( )  RATIONAL_B_SPLINE_SURFACE ( (
 ( 1.000000000000000000, 1.000000000000000000),
 ( 0.7223157951917480446, 0.9931996967497186413),
 ( 0.7223157951917480446, 0.9931996967497186413),
 ( 1.000000000000000000, 1.000000000000000000) ) ) 
 REPRESENTATION_ITEM ( '' )  SURFACE ( )  );
#45759 =( GEOMETRIC_REPRESENTATION_CONTEXT ( 3 ) GLOBAL_UNCERTAINTY_ASSIGNED_CONTEXT ( ( #18581 ) ) GLOBAL_UNIT_ASSIGNED_CONTEXT ( ( #15714, #11014, #7831 ) ) REPRESENTATION_CONTEXT ( 'NONE', 'WORKASPACE' ) );
#45760 = B_SPLINE_CURVE_WITH_KNOTS ( 'NONE', 3,
 ( #14482, #39, #57350, #51741, #38301, #42682 ),
 .UNSPECIFIED., .F., .F.,
 ( 4, 2, 4 ),
 ( 0.000000000000000000, 0.0002447195606305744751, 0.0004894391212611489501 ),
 .UNSPECIFIED. ) ;
#45761 = ORIENTED_EDGE ( 'NONE', *, *, #38552, .T. ) ;
#45763 = CARTESIAN_POINT ( 'NONE',  ( 3.240649175237396484, 26.64593727015325086, -35.00369901014332186 ) ) ;
#45762 = CIRCLE ( 'NONE', #740, 43.08621763946400307 ) ;
#45764 = ORIENTED_EDGE ( 'NONE', *, *, #30191, .T. ) ;
#45765 = CIRCLE ( 'NONE', #4697, 42.92674063221959813 ) ;
#45766 = CARTESIAN_POINT ( 'NONE',  ( 0.1119899015040011353, 39.50795633840085941, 19.64898710253324410 ) ) ;
#45767 = CARTESIAN_POINT ( 'NONE',  ( 0.6845945791218034371, -13.06825445484017933, -45.05138450944092199 ) ) ;
#45768 = CARTESIAN_POINT ( 'NONE',  ( 0.8551540677456715978, -41.94570365541218848, 23.16399837394531147 ) ) ;
#45769 = EDGE_CURVE ( 'NONE', #38058, #51214, #9967, .T. ) ;
#45770 = PRESENTATION_STYLE_ASSIGNMENT (( #2815 ) ) ;
#45771 = LINE ( 'NONE', #41086, #58793 ) ;
#45772 = ORIENTED_EDGE ( 'NONE', *, *, #42111, .F. ) ;
#45773 = CARTESIAN_POINT ( 'NONE',  ( 0.1365634738349407185, 20.97116515538588999, -38.82103620009102940 ) ) ;
#45774 = CARTESIAN_POINT ( 'NONE',  ( 0.2885700199627493356, -25.60460887553402998, 34.69058524452970715 ) ) ;
#45775 = EDGE_CURVE ( 'NONE', #34877, #21245, #964, .T. ) ;
#45776 = CIRCLE ( 'NONE', #18754, 5.612499999999999822 ) ;
#45777 = CARTESIAN_POINT ( 'NONE',  ( 3.783198216974389183, 36.37893817280285447, 22.99723434398804400 ) ) ;
#45778 =( BOUNDED_SURFACE ( )  B_SPLINE_SURFACE ( 3, 1, ( 
 ( #19385, #42282 ),
 ( #48198, #28770 ),
 ( #52256, #32562 ),
 ( #28455, #61042 ) ),
 .UNSPECIFIED., .F., .F., .F. ) 
 B_SPLINE_SURFACE_WITH_KNOTS ( ( 4, 4 ),
 ( 2, 2 ),
 ( 0.000000000000000000, 1.000000000000000000 ),
 ( 0.000000000000000000, 1.000000000000000000 ),
 .UNSPECIFIED. ) 
 GEOMETRIC_REPRESENTATION_ITEM ( )  RATIONAL_B_SPLINE_SURFACE ( (
 ( 1.000000000000000000, 1.000000000000000000),
 ( 0.9953390228620291325, 0.8624445117761032620),
 ( 0.9953390228620291325, 0.8624445117761032620),
 ( 1.000000000000000000, 1.000000000000000000) ) ) 
 REPRESENTATION_ITEM ( '' )  SURFACE ( )  );
#45779 = CARTESIAN_POINT ( 'NONE',  ( 0.1084644655670282121, 21.21700107124048529, -37.54424727804280337 ) ) ;
#45780 = CARTESIAN_POINT ( 'NONE',  ( 0.9757787079277446818, 37.17954582422768084, -21.42002160630781304 ) ) ;
#45781 = CARTESIAN_POINT ( 'NONE',  ( 0.6254087463353934506, -44.17672642933517579, 19.04342133627966405 ) ) ;
#45782 =( BOUNDED_SURFACE ( )  B_SPLINE_SURFACE ( 3, 1, ( 
 ( #29305, #9576 ),
 ( #58404, #5170 ),
 ( #19617, #24929 ),
 ( #19009, #38737 ) ),
 .UNSPECIFIED., .F., .F., .F. ) 
 B_SPLINE_SURFACE_WITH_KNOTS ( ( 4, 4 ),
 ( 2, 2 ),
 ( 0.000000000000000000, 1.000000000000000000 ),
 ( 0.000000000000000000, 1.000000000000000000 ),
 .UNSPECIFIED. ) 
 GEOMETRIC_REPRESENTATION_ITEM ( )  RATIONAL_B_SPLINE_SURFACE ( (
 ( 1.000000000000000000, 1.000000000000000000),
 ( 0.9952954269826590483, 0.8620686068821339365),
 ( 0.9952954269826590483, 0.8620686068821339365),
 ( 1.000000000000000000, 1.000000000000000000) ) ) 
 REPRESENTATION_ITEM ( '' )  SURFACE ( )  );
#45783 = LINE ( 'NONE', #60152, #25042 ) ;
#45784 = CYLINDRICAL_SURFACE ( 'NONE', #20128, 9.500000000000000000 ) ;
#45785 = B_SPLINE_CURVE_WITH_KNOTS ( 'NONE', 3,
 ( #24792, #48903, #25094, #43931, #971, #44237 ),
 .UNSPECIFIED., .F., .F.,
 ( 4, 2, 4 ),
 ( 1.512800854419661994E-16, 0.0002445252820015220629, 0.0004890505640028927712 ),
 .UNSPECIFIED. ) ;
#45786 = B_SPLINE_CURVE_WITH_KNOTS ( 'NONE', 3,
 ( #42542, #4279, #17260, #7208, #21336, #3137, #61605, #13725, #16642, #32837, #26037, #36384, #36686, #2827, #41095, #55447 ),
 .UNSPECIFIED., .F., .F.,
 ( 4, 3, 3, 3, 3, 4 ),
 ( 0.000000000000000000, 0.0002732102107931896201, 0.0004098135523333825097, 0.0005464168938825025032, 0.0008195847345945498404, 0.001092771384553103313 ),
 .UNSPECIFIED. ) ;
#45787 = EDGE_CURVE ( 'NONE', #13848, #45995, #49540, .T. ) ;
#45788 = VECTOR ( 'NONE', #48690, 1000.000000000000000 ) ;
#45789 = CARTESIAN_POINT ( 'NONE',  ( 2.624215991343620935, 17.05978231157464364, -44.87417713512071771 ) ) ;
#45790 = CARTESIAN_POINT ( 'NONE',  ( 0.5834872094924165031, -28.97678700412158648, -38.13619618345241236 ) ) ;
#45791 = ORIENTED_EDGE ( 'NONE', *, *, #52043, .F. ) ;
#45792 = CARTESIAN_POINT ( 'NONE',  ( 0.5806925824938499181, -46.06186276235273169, 8.804950948514585818 ) ) ;
#45793 = CARTESIAN_POINT ( 'NONE',  ( 0.8760168074887076939, -47.56749362999718045, 7.161346975772899803 ) ) ;
#45794 = CARTESIAN_POINT ( 'NONE',  ( 1.479689385636123067, -42.30896271024097643, 12.30997642772440415 ) ) ;
#45795 = ORIENTED_EDGE ( 'NONE', *, *, #2679, .T. ) ;
#45796 = EDGE_CURVE ( 'NONE', #60819, #34095, #24140, .T. ) ;
#45797 = CARTESIAN_POINT ( 'NONE',  ( 2.301430502907646058, 7.543848632415214084, -47.43735983879645346 ) ) ;
#45798 = CARTESIAN_POINT ( 'NONE',  ( 0.6021448801613057400, 44.35700409489896145, -21.07124406275206141 ) ) ;
#45799 = ADVANCED_FACE ( 'NONE', ( #32085, #27683 ), #51162, .T. ) ;
#45800 = LINE ( 'NONE', #20736, #6611 ) ;
#45801 = EDGE_LOOP ( 'NONE', ( #39723, #7662, #39319, #37606 ) ) ;
#45802 = CARTESIAN_POINT ( 'NONE',  ( 5.981074661064941900, 12.50143471347259450, 16.27808421740030553 ) ) ;
#45803 = CARTESIAN_POINT ( 'NONE',  ( 0.9754642270333693244, -41.40054989430071686, -11.27515941577618364 ) ) ;
#45804 = CARTESIAN_POINT ( 'NONE',  ( 0.7044674535453004927, 49.05595398932692319, 2.305667150294545831 ) ) ;
#45805 = ORIENTED_EDGE ( 'NONE', *, *, #18323, .F. ) ;
#45806 = CARTESIAN_POINT ( 'NONE',  ( -5.995132425357893702, 14.94489030678166941, -11.47834865841080720 ) ) ;
#45807 = TOROIDAL_SURFACE ( 'NONE', #9778, 15.71999999999999709, 0.2800000000000011924 ) ;
#45808 = VECTOR ( 'NONE', #55649, 1000.000000000000114 ) ;
#45809 = ORIENTED_EDGE ( 'NONE', *, *, #17307, .F. ) ;
#45810 = VERTEX_POINT ( 'NONE', #22676 ) ;
#45811 = CARTESIAN_POINT ( 'NONE',  ( -6.063463321072278589, 7.780528881867136093, 17.61487504349381794 ) ) ;
#45812 = ORIENTED_EDGE ( 'NONE', *, *, #57972, .T. ) ;
#45813 = EDGE_CURVE ( 'NONE', #49511, #52728, #60744, .T. ) ;
#45814 = PRODUCT_DEFINITION_SHAPE ( 'NONE', 'NONE',  #22195 ) ;
#45815 = ORIENTED_EDGE ( 'NONE', *, *, #30838, .F. ) ;
#45816 = CARTESIAN_POINT ( 'NONE',  ( 5.838029081930955932, 19.86434078293957839, 42.85408992630882352 ) ) ;
#45817 = CARTESIAN_POINT ( 'NONE',  ( 0.9754642270333664378, 16.25787253057936255, 39.70914670678642011 ) ) ;
#45818 = ORIENTED_EDGE ( 'NONE', *, *, #61838, .T. ) ;
#45819 = CARTESIAN_POINT ( 'NONE',  ( 0.1157506346131639274, 15.32596964082831903, 41.37699015601839392 ) ) ;
#45820 = B_SPLINE_CURVE_WITH_KNOTS ( 'NONE', 3,
 ( #51050, #61366, #28178, #24407, #14411, #51668 ),
 .UNSPECIFIED., .F., .F.,
 ( 4, 2, 4 ),
 ( 1.964907063297894324E-17, 0.0002293319059085095475, 0.0004586638118169994167 ),
 .UNSPECIFIED. ) ;
#45821 = CARTESIAN_POINT ( 'NONE',  ( 0.8753041380234524160, 36.80657072176735056, -32.50253343320360244 ) ) ;
#45822 = FACE_OUTER_BOUND ( 'NONE', #8862, .T. ) ;
#45823 = DIRECTION ( 'NONE',  ( 0.1011922191286467876, 0.9788975924247106386, 0.1775377096081985073 ) ) ;
#45824 = ORIENTED_EDGE ( 'NONE', *, *, #46331, .F. ) ;
#45825 = CARTESIAN_POINT ( 'NONE',  ( 0.5827359174754830340, 44.10985444762183505, 18.66406616557994269 ) ) ;
#45826 = VERTEX_POINT ( 'NONE', #24208 ) ;
#45827 = CIRCLE ( 'NONE', #11792, 72.00000000000002842 ) ;
#45828 = DIRECTION ( 'NONE',  ( -1.000000000000000000, -0.000000000000000000, -0.000000000000000000 ) ) ;
#45829 = CARTESIAN_POINT ( 'NONE',  ( 0.9752570700956798566, 25.93764562640103222, 34.18150842933886224 ) ) ;
#45830 = CARTESIAN_POINT ( 'NONE',  ( 1.834102595619085507, 13.98314437153100975, -41.76924009773946267 ) ) ;
#45831 = VERTEX_POINT ( 'NONE', #52090 ) ;
#45832 = CARTESIAN_POINT ( 'NONE',  ( 0.5836750258453357043, -46.21662382526645274, -12.57171936981210436 ) ) ;
#45833 = CARTESIAN_POINT ( 'NONE',  ( 0.8760168074886965917, 11.58706983520260536, 46.68716261866180872 ) ) ;
#45834 = CARTESIAN_POINT ( 'NONE',  ( 0.8551540677456739292, -33.23105123575875552, -34.52115452272963836 ) ) ;
#45835 = FILL_AREA_STYLE ('',( #20773 ) ) ;
#45836 = VECTOR ( 'NONE', #20573, 1000.000000000000000 ) ;
#45837 = ADVANCED_FACE ( 'NONE', ( #53015 ), #22896, .F. ) ;
#45838 = ORIENTED_EDGE ( 'NONE', *, *, #31167, .F. ) ;
#45839 = ORIENTED_EDGE ( 'NONE', *, *, #25746, .T. ) ;
#45840 = CARTESIAN_POINT ( 'NONE',  ( 0.9790320750461907195, -39.56154820336092826, -13.82826946133685730 ) ) ;
#45841 = CARTESIAN_POINT ( 'NONE',  ( 0.5800708057587375954, 13.00144577271105817, -46.09746469244086597 ) ) ;
#45842 = EDGE_CURVE ( 'NONE', #61052, #56419, #9491, .T. ) ;
#45843 = CARTESIAN_POINT ( 'NONE',  ( 0.6041374136657476912, 41.74951251761541471, 23.90252055111336205 ) ) ;
#45844 = CARTESIAN_POINT ( 'NONE',  ( 0.3622758884714730732, 39.50828911766998175, -17.25816669464953534 ) ) ;
#45845 = EDGE_CURVE ( 'NONE', #42917, #30001, #15173, .T. ) ;
#45846 = CARTESIAN_POINT ( 'NONE',  ( 0.5817217712918327788, 5.146885071079491780, -46.61270779598062575 ) ) ;
#45847 = CARTESIAN_POINT ( 'NONE',  ( 3.782542959838397056, -3.127173655629709614, 41.92205431898710799 ) ) ;
#45848 = EDGE_CURVE ( 'NONE', #48557, #16242, #46572, .T. ) ;
#45849 = CARTESIAN_POINT ( 'NONE',  ( 0.1313383488274127153, -6.260443365527081028, -42.66669366003520025 ) ) ;
#45850 = CARTESIAN_POINT ( 'NONE',  ( 0.6000166863083090663, 48.97316450298206547, 3.667784109283304783 ) ) ;
#45851 = AXIS2_PLACEMENT_3D ( 'NONE', #36213, #55278, #9529 ) ;
#45852 = CARTESIAN_POINT ( 'NONE',  ( 0.7762783648524380631, 0.8897020150998180554, 47.89627393592489568 ) ) ;
#45853 = CARTESIAN_POINT ( 'NONE',  ( -1.129531546211690163, 0.000000000000000000, 0.000000000000000000 ) ) ;
#45854 = CARTESIAN_POINT ( 'NONE',  ( 5.959828726073459926, 5.316791119500813068, 19.82504517499715035 ) ) ;
#45855 = CARTESIAN_POINT ( 'NONE',  ( 3.894904216938897434, 40.96222025004743017, -15.94430445842042232 ) ) ;
#45856 = CARTESIAN_POINT ( 'NONE',  ( 0.5998501479064699549, 37.84527566984857572, -29.69975237324574024 ) ) ;
#45857 = CARTESIAN_POINT ( 'NONE',  ( 5.981074661064941900, 20.34795181394748909, -2.687517936919787687 ) ) ;
#45858 = LINE ( 'NONE', #35216, #22878 ) ;
#45859 =( BOUNDED_SURFACE ( )  B_SPLINE_SURFACE ( 3, 1, ( 
 ( #2895, #22027 ),
 ( #17325, #7916 ),
 ( #21093, #50213 ),
 ( #17026, #16392 ) ),
 .UNSPECIFIED., .F., .F., .F. ) 
 B_SPLINE_SURFACE_WITH_KNOTS ( ( 4, 4 ),
 ( 2, 2 ),
 ( 0.000000000000000000, 1.000000000000000000 ),
 ( 0.000000000000000000, 1.000000000000000000 ),
 .UNSPECIFIED. ) 
 GEOMETRIC_REPRESENTATION_ITEM ( )  RATIONAL_B_SPLINE_SURFACE ( (
 ( 1.000000000000000000, 1.000000000000000000),
 ( 0.9953485035131437453, 0.8621029689291515030),
 ( 0.9953485035131437453, 0.8621029689291515030),
 ( 1.000000000000000000, 1.000000000000000000) ) ) 
 REPRESENTATION_ITEM ( '' )  SURFACE ( )  );
#45860 = CARTESIAN_POINT ( 'NONE',  ( 0.6000166863083090663, 11.43688157230968017, -47.76003791465640091 ) ) ;
#45861 = EDGE_CURVE ( 'NONE', #19824, #7010, #48775, .T. ) ;
#45862 = CARTESIAN_POINT ( 'NONE',  ( 5.880360259849739535, 9.405269135694590332, 47.04104239318770198 ) ) ;
#45863 = CARTESIAN_POINT ( 'NONE',  ( 4.956445790444018229, -10.39006634428234577, -45.93021414603951058 ) ) ;
#45865 = ORIENTED_EDGE ( 'NONE', *, *, #21326, .F. ) ;
#45864 = FACE_OUTER_BOUND ( 'NONE', #46546, .T. ) ;
#45866 = ORIENTED_EDGE ( 'NONE', *, *, #28567, .T. ) ;
#45867 = AXIS2_PLACEMENT_3D ( 'NONE', #9212, #23623, #52732 ) ;
#45868 = CARTESIAN_POINT ( 'NONE',  ( 0.6016117650947689910, 16.63268918597161772, -46.20502899779809525 ) ) ;
#45869 = CARTESIAN_POINT ( 'NONE',  ( 3.390910168358336918, 2.257738501152356303, -43.92037970457509033 ) ) ;
#45871 = EDGE_CURVE ( 'NONE', #60330, #26558, #33326, .T. ) ;
#45870 = DIRECTION ( 'NONE',  ( 0.000000000000000000, 0.000000000000000000, 1.000000000000000000 ) ) ;
#45872 = VERTEX_POINT ( 'NONE', #49874 ) ;
#45873 = ORIENTED_EDGE ( 'NONE', *, *, #40620, .T. ) ;
#45874 = DIRECTION ( 'NONE',  ( -1.000000000000000000, -0.000000000000000000, -0.000000000000000000 ) ) ;
#45875 = CARTESIAN_POINT ( 'NONE',  ( -6.078457390727109555, 15.42941986619899097, 11.52074275513744261 ) ) ;
#45876 = EDGE_CURVE ( 'NONE', #18653, #33938, #30754, .T. ) ;
#45877 = EDGE_LOOP ( 'NONE', ( #32784, #17614, #10275, #29512 ) ) ;
#45878 = ORIENTED_EDGE ( 'NONE', *, *, #38630, .T. ) ;
#45879 = CARTESIAN_POINT ( 'NONE',  ( 0.3676999524040366896, -17.09834788623584600, 40.66444494744877858 ) ) ;
#45880 = CARTESIAN_POINT ( 'NONE',  ( 3.660087539127330647, -35.27260502801109965, -32.61167949558423373 ) ) ;
#45881 = CARTESIAN_POINT ( 'NONE',  ( 5.901463166500145796, -11.94204572599471348, 16.18349202795515041 ) ) ;
#45882 = ORIENTED_EDGE ( 'NONE', *, *, #22859, .T. ) ;
#45883 = CARTESIAN_POINT ( 'NONE',  ( 4.694002226626921015, 18.76791414987520668, -41.54575995103530772 ) ) ;
#45884 = EDGE_CURVE ( 'NONE', #37253, #2911, #4695, .T. ) ;
#45885 = B_SPLINE_CURVE_WITH_KNOTS ( 'NONE', 3,
 ( #59685, #36219, #41536, #7673, #17718, #35606, #2981, #7358, #55284, #26484, #2046, #25873, #21177, #55593, #2667, #12723 ),
 .UNSPECIFIED., .F., .F.,
 ( 4, 3, 3, 3, 3, 4 ),
 ( 2.194378057379452319E-17, 0.0002618515315864398084, 0.0003927756766341980454, 0.0005236998216950549626, 0.0007855159896329879472, 0.001047349442285926569 ),
 .UNSPECIFIED. ) ;
#45886 = DIRECTION ( 'NONE',  ( 0.000000000000000000, 0.000000000000000000, 1.000000000000000000 ) ) ;
#45887 = ADVANCED_FACE ( 'NONE', ( #6933 ), #56901, .F. ) ;
#45888 = CARTESIAN_POINT ( 'NONE',  ( 0.6031357023905875581, -48.10744334619843698, -0.04361601114896231091 ) ) ;
#45889 = ORIENTED_EDGE ( 'NONE', *, *, #39489, .F. ) ;
#45890 = VECTOR ( 'NONE', #40730, 999.9999999999998863 ) ;
#45891 = ORIENTED_EDGE ( 'NONE', *, *, #60187, .T. ) ;
#45892 = CARTESIAN_POINT ( 'NONE',  ( 1.227938101723748288, 42.43379953535185933, 6.439911493064710335 ) ) ;
#45893 = CIRCLE ( 'NONE', #6847, 47.09074272231896430 ) ;
#45894 = ORIENTED_EDGE ( 'NONE', *, *, #52376, .F. ) ;
#45895 = CARTESIAN_POINT ( 'NONE',  ( -6.017396004339687465, 4.878103249821321263, -18.20079405513545012 ) ) ;
#45896 = CARTESIAN_POINT ( 'NONE',  ( -6.016761891674565099, -13.32657647165364700, 13.32172022638586917 ) ) ;
#45897 = CARTESIAN_POINT ( 'NONE',  ( -1.200000000000006617, 8.434754829127421589E-16, 6.887500000000022382 ) ) ;
#45898 = CARTESIAN_POINT ( 'NONE',  ( 0.5997462898726536595, 16.46871699354542429, -46.26373299606095202 ) ) ;
#45899 = CARTESIAN_POINT ( 'NONE',  ( 4.956653778116970166, 47.94889704119054130, 3.690426056930153464 ) ) ;
#45900 = VERTEX_POINT ( 'NONE', #6301 ) ;
#45901 = DIRECTION ( 'NONE',  ( -1.000000000000000000, 0.000000000000000000, 0.000000000000000000 ) ) ;
#45902 = CARTESIAN_POINT ( 'NONE',  ( 3.678834586032788234, -47.80915124093738200, 10.62532010103831581 ) ) ;
#45903 = B_SPLINE_CURVE_WITH_KNOTS ( 'NONE', 3,
 ( #15240, #57808, #11154, #48429 ),
 .UNSPECIFIED., .F., .F.,
 ( 4, 4 ),
 ( 0.000000000000000000, 0.004447772540403803314 ),
 .UNSPECIFIED. ) ;
#45904 = CARTESIAN_POINT ( 'NONE',  ( 0.1102144999581333024, 39.88986724628635017, -16.38650952318868903 ) ) ;
#45905 = EDGE_LOOP ( 'NONE', ( #41271, #9487, #26509, #31620 ) ) ;
#45906 = CARTESIAN_POINT ( 'NONE',  ( 0.1100247026804066219, 42.77732815928600019, -5.460606496326462000 ) ) ;
#45907 = CARTESIAN_POINT ( 'NONE',  ( 0.5804410086790514622, -29.86002002114409493, 36.16488706179337953 ) ) ;
#45908 = CARTESIAN_POINT ( 'NONE',  ( 4.967162193818130511, 0.000000000000000000, 0.000000000000000000 ) ) ;
#45909 = CARTESIAN_POINT ( 'NONE',  ( 0.7056759521545049596, -41.47345344194140182, -21.90208868387004060 ) ) ;
#45910 = CONICAL_SURFACE ( 'NONE', #18894, 43.92652462719577500, 1.486293639869522343 ) ;
#45911 = ORIENTED_EDGE ( 'NONE', *, *, #48642, .F. ) ;
#45912 = CARTESIAN_POINT ( 'NONE',  ( 0.1119898979215348395, -12.01552111793010091, 42.45690238955739204 ) ) ;
#45913 = FACE_OUTER_BOUND ( 'NONE', #47855, .T. ) ;
#45914 = ADVANCED_FACE ( 'NONE', ( #11056, #5996 ), #20144, .T. ) ;
#45915 = CARTESIAN_POINT ( 'NONE',  ( 0.6067375320500719704, -0.7090021732337279392, 47.89177856776003495 ) ) ;
#45916 = ADVANCED_FACE ( 'NONE', ( #43975 ), #26920, .F. ) ;
#45917 = DIRECTION ( 'NONE',  ( 0.000000000000000000, 0.000000000000000000, 1.000000000000000000 ) ) ;
#45919 = CARTESIAN_POINT ( 'NONE',  ( 0.5837800304671220131, -46.79431954288349260, 3.086906331265775183 ) ) ;
#45918 = AXIS2_PLACEMENT_3D ( 'NONE', #24960, #39694, #34668 ) ;
#45920 = CARTESIAN_POINT ( 'NONE',  ( 0.7764146366350288542, 40.80384778211000452, 23.13193636173942380 ) ) ;
#45921 = CARTESIAN_POINT ( 'NONE',  ( 0.9754402186311922351, -5.786576363453280081, -42.51649392388765136 ) ) ;
#45922 = CARTESIAN_POINT ( 'NONE',  ( 0.1087620492084205859, -41.55994353650434192, -11.51076657762320643 ) ) ;
#45923 = EDGE_CURVE ( 'NONE', #8537, #29889, #56974, .T. ) ;
#45924 = CARTESIAN_POINT ( 'NONE',  ( 4.967162193818130511, 19.45289607368822615, 38.44485641567079881 ) ) ;
#45925 = EDGE_CURVE ( 'NONE', #12199, #37991, #44275, .T. ) ;
#45926 = DIRECTION ( 'NONE',  ( -1.000000000000000000, -0.000000000000000000, -0.000000000000000000 ) ) ;
#45927 = ORIENTED_EDGE ( 'NONE', *, *, #16479, .F. ) ;
#45928 = B_SPLINE_CURVE_WITH_KNOTS ( 'NONE', 3,
 ( #32231, #37880, #55698, #17511, #46643, #3996 ),
 .UNSPECIFIED., .F., .F.,
 ( 4, 2, 4 ),
 ( 1.180110611199200660E-16, 0.0002448718616795917953, 0.0004897437233590655210 ),
 .UNSPECIFIED. ) ;
#45929 = EDGE_CURVE ( 'NONE', #56169, #9944, #15954, .T. ) ;
#45930 = DIRECTION ( 'NONE',  ( 0.000000000000000000, 0.000000000000000000, 1.000000000000000000 ) ) ;
#45931 = CARTESIAN_POINT ( 'NONE',  ( 0.9762797500689124330, -18.09842611962814019, 37.79909730639167265 ) ) ;
#45932 = CARTESIAN_POINT ( 'NONE',  ( 1.199999999999992628, 0.000000000000000000, -5.612499999999999822 ) ) ;
#45933 = FACE_OUTER_BOUND ( 'NONE', #40352, .T. ) ;
#45934 = LINE ( 'NONE', #33367, #7076 ) ;
#45935 = CARTESIAN_POINT ( 'NONE',  ( 0.9730545539215883499, -21.01499094264522682, -37.40983423658496321 ) ) ;
#45936 = PRODUCT_CONTEXT ( 'NONE', #23534, 'mechanical' ) ;
#45937 = CARTESIAN_POINT ( 'NONE',  ( 0.3622758884714600280, 36.91764744403290166, 22.26738722580180507 ) ) ;
#45938 = EDGE_CURVE ( 'NONE', #58089, #16817, #1010, .T. ) ;
#45939 = CARTESIAN_POINT ( 'NONE',  ( 3.050102900204245682, 35.85168643609029004, -25.49670231356046202 ) ) ;
#45940 = CIRCLE ( 'NONE', #42900, 5.000000000000000000 ) ;
#45941 = CARTESIAN_POINT ( 'NONE',  ( 0.6029443449137436017, -1.617468957629060400, 49.08078373614706891 ) ) ;
#45943 = ORIENTED_EDGE ( 'NONE', *, *, #1898, .F. ) ;
#45942 = CARTESIAN_POINT ( 'NONE',  ( 4.553261556744873317, 22.57774691820481294, -37.68003330573274923 ) ) ;
#45944 = ORIENTED_EDGE ( 'NONE', *, *, #18279, .T. ) ;
#45945 = AXIS2_PLACEMENT_3D ( 'NONE', #31526, #60024, #17432 ) ;
#45946 = CARTESIAN_POINT ( 'NONE',  ( -6.015611763856276717, -18.19956619163661671, 4.882992715191235789 ) ) ;
#45947 = CARTESIAN_POINT ( 'NONE',  ( 5.880360259849739535, -15.46489389606724707, -45.41096578730640942 ) ) ;
#45948 = CARTESIAN_POINT ( 'NONE',  ( -2.569797478183790229, 14.01151037928417153, 4.218948559326298309 ) ) ;
#45949 = ORIENTED_EDGE ( 'NONE', *, *, #4066, .T. ) ;
#45950 = CARTESIAN_POINT ( 'NONE',  ( -2.739355103387248747, 14.87824819718638736, -1.218727834234153207 ) ) ;
#45951 = CARTESIAN_POINT ( 'NONE',  ( 2.891212509699203626, -1.730266096895115631E-16, -41.99381090189411481 ) ) ;
#45952 = FACE_OUTER_BOUND ( 'NONE', #50844, .T. ) ;
#45953 = ORIENTED_EDGE ( 'NONE', *, *, #52615, .F. ) ;
#45954 = ORIENTED_EDGE ( 'NONE', *, *, #21775, .T. ) ;
#45955 = B_SPLINE_CURVE_WITH_KNOTS ( 'NONE', 3,
 ( #467, #56865, #4854, #42808 ),
 .UNSPECIFIED., .F., .F.,
 ( 4, 4 ),
 ( 0.000000000000000000, 0.004445488388166993383 ),
 .UNSPECIFIED. ) ;
#45956 = CIRCLE ( 'NONE', #8903, 7.500000000000022204 ) ;
#45957 = FACE_OUTER_BOUND ( 'NONE', #47743, .T. ) ;
#45958 = DIRECTION ( 'NONE',  ( 0.000000000000000000, 0.000000000000000000, 1.000000000000000000 ) ) ;
#45959 = ORIENTED_EDGE ( 'NONE', *, *, #49940, .T. ) ;
#45960 = CARTESIAN_POINT ( 'NONE',  ( 0.7413678028165009426, -44.08645218430292800, 0.9331803531016585884 ) ) ;
#45961 = CARTESIAN_POINT ( 'NONE',  ( 0.1145239942831223490, -42.59710765884724282, -11.50790596960418100 ) ) ;
#45962 = EDGE_CURVE ( 'NONE', #49832, #20913, #34861, .T. ) ;
#45963 = CARTESIAN_POINT ( 'NONE',  ( 0.6039202388192952409, -13.80541670804725740, -47.12721275830092083 ) ) ;
#45964 = CARTESIAN_POINT ( 'NONE',  ( 0.8760168074887076939, 17.58183840866400516, -44.77533136581864426 ) ) ;
#45965 = ORIENTED_EDGE ( 'NONE', *, *, #18672, .F. ) ;
#45966 = CARTESIAN_POINT ( 'NONE',  ( -6.078457390727109555, 12.00250936636397903, -15.05769836156418684 ) ) ;
#45967 = CARTESIAN_POINT ( 'NONE',  ( 0.8760168074887076939, 48.09529047980637984, -0.8912768426701273006 ) ) ;
#45968 = ORIENTED_EDGE ( 'NONE', *, *, #6790, .T. ) ;
#45969 = DIRECTION ( 'NONE',  ( -1.000000000000000000, -3.135800716341489291E-16, 1.298891185607901956E-16 ) ) ;
#45970 = DIRECTION ( 'NONE',  ( 0.000000000000000000, 0.000000000000000000, 1.000000000000000000 ) ) ;
#45971 = CARTESIAN_POINT ( 'NONE',  ( 0.5549461598389365813, 39.34817863456808595, -19.92331633059426110 ) ) ;
#45972 = CARTESIAN_POINT ( 'NONE',  ( 0.8760168074887090262, -19.22870327415273195, -44.09317760313745538 ) ) ;
#45973 = ORIENTED_EDGE ( 'NONE', *, *, #3588, .T. ) ;
#45974 = VERTEX_POINT ( 'NONE', #20755 ) ;
#45976 = B_SPLINE_CURVE_WITH_KNOTS ( 'NONE', 3,
 ( #20379, #5321, #57945, #29763, #25070, #24765, #39505, #58560, #53255, #39823, #44214, #35108, #10366, #1244, #25377, #24449, #53862, #15690, #43907, #58250, #43587, #948, #44828, #54167, #11286 ),
 .UNSPECIFIED., .F., .F.,
 ( 4, 3, 3, 3, 3, 3, 3, 3, 4 ),
 ( 5.553824967135426632E-18, 0.0005656085177311402905, 0.001131215744874499839, 0.001696821861372766567, 0.002262427090022498585, 0.002828031679238745925, 0.003393635864401606597, 0.003977030878808131623, 0.004561030005651159000 ),
 .UNSPECIFIED. ) ;
#45975 = CARTESIAN_POINT ( 'NONE',  ( 0.6067099128993229673, -33.36330296770416481, 34.36589933408230735 ) ) ;
#45977 = CARTESIAN_POINT ( 'NONE',  ( 0.5998501479064699549, 44.24259072156085182, -18.89267974119621485 ) ) ;
#45978 = VERTEX_POINT ( 'NONE', #40201 ) ;
#45979 = CARTESIAN_POINT ( 'NONE',  ( 0.8554163680231720024, 17.71207986799936052, 43.44522643353847968 ) ) ;
#45980 = B_SPLINE_CURVE_WITH_KNOTS ( 'NONE', 3,
 ( #55310, #12429, #51538, #3922 ),
 .UNSPECIFIED., .F., .F.,
 ( 4, 4 ),
 ( 0.000000000000000000, 0.004442905043737213101 ),
 .UNSPECIFIED. ) ;
#45981 = CIRCLE ( 'NONE', #3937, 2.500000000000000888 ) ;
#45982 =( BOUNDED_SURFACE ( )  B_SPLINE_SURFACE ( 3, 1, ( 
 ( #26054, #45194 ),
 ( #54849, #11983 ),
 ( #31064, #22594 ),
 ( #27907, #52004 ) ),
 .UNSPECIFIED., .F., .F., .F. ) 
 B_SPLINE_SURFACE_WITH_KNOTS ( ( 4, 4 ),
 ( 2, 2 ),
 ( 0.000000000000000000, 1.000000000000000000 ),
 ( 0.000000000000000000, 1.000000000000000000 ),
 .UNSPECIFIED. ) 
 GEOMETRIC_REPRESENTATION_ITEM ( )  RATIONAL_B_SPLINE_SURFACE ( (
 ( 1.000000000000000000, 1.000000000000000000),
 ( 0.9953040768229013402, 0.8617119497784988535),
 ( 0.9953040768229013402, 0.8617119497784988535),
 ( 1.000000000000000000, 1.000000000000000000) ) ) 
 REPRESENTATION_ITEM ( '' )  SURFACE ( )  );
#45983 = ORIENTED_EDGE ( 'NONE', *, *, #24454, .T. ) ;
#45984 = CARTESIAN_POINT ( 'NONE',  ( 0.9754292589017199422, -39.77696748547529637, -13.19546606053464011 ) ) ;
#45985 = ORIENTED_EDGE ( 'NONE', *, *, #49989, .T. ) ;
#45986 = CARTESIAN_POINT ( 'NONE',  ( 3.782542959838391727, -40.81794997429708616, -10.05648115855390934 ) ) ;
#45987 = CARTESIAN_POINT ( 'NONE',  ( 0.6024113833632039894, -48.67596287166193036, -6.495576003516191577 ) ) ;
#45988 = AXIS2_PLACEMENT_3D ( 'NONE', #31645, #1571, #20706 ) ;
#45989 = CARTESIAN_POINT ( 'NONE',  ( 0.2885697896453112699, -20.85752796052987179, -37.73587455644740629 ) ) ;
#45990 = ORIENTED_EDGE ( 'NONE', *, *, #17137, .F. ) ;
#45991 = CARTESIAN_POINT ( 'NONE',  ( 0.1135584504625007235, 43.22593930884824687, 8.858342000793420823 ) ) ;
#45992 = FACE_OUTER_BOUND ( 'NONE', #3524, .T. ) ;
#45993 = CARTESIAN_POINT ( 'NONE',  ( 0.8751705887134553219, 47.55935879196470495, -7.160166390003808168 ) ) ;
#45994 = B_SPLINE_CURVE_WITH_KNOTS ( 'NONE', 3,
 ( #54490, #21010, #1257, #30702 ),
 .UNSPECIFIED., .F., .F.,
 ( 4, 4 ),
 ( 0.000000000000000000, 0.005013413432710151114 ),
 .UNSPECIFIED. ) ;
#45995 = VERTEX_POINT ( 'NONE', #16059 ) ;
#45996 = EDGE_CURVE ( 'NONE', #884, #30413, #57737, .T. ) ;
#45997 = ORIENTED_EDGE ( 'NONE', *, *, #24049, .T. ) ;
#45998 = FACE_OUTER_BOUND ( 'NONE', #50686, .T. ) ;
#45999 = CARTESIAN_POINT ( 'NONE',  ( 0.9762797500689124330, -26.66896101499594707, 32.32787193067817810 ) ) ;
#46000 = CARTESIAN_POINT ( 'NONE',  ( 0.9762797500689124330, 38.77779312671053447, -15.89363222827765831 ) ) ;
#46001 = CARTESIAN_POINT ( 'NONE',  ( 5.838029081930955932, 46.29164171884946910, -9.388768030290036037 ) ) ;
#46002 = CARTESIAN_POINT ( 'NONE',  ( 1.827119703190780653, 36.65069040194709515, -22.58367210012853121 ) ) ;
#46003 = VERTEX_POINT ( 'NONE', #11353 ) ;
#46004 = EDGE_CURVE ( 'NONE', #46173, #15890, #31585, .T. ) ;
#46005 = CARTESIAN_POINT ( 'NONE',  ( 0.7057020205115072109, -23.21851350879788356, -41.89806668505404730 ) ) ;
#46006 = EDGE_CURVE ( 'NONE', #5500, #15172, #13743, .T. ) ;
#46007 = CARTESIAN_POINT ( 'NONE',  ( 0.6064782688330877525, 39.98346752738379450, 24.50830004111699623 ) ) ;
#46008 = CIRCLE ( 'NONE', #53951, 42.92674063221959813 ) ;
#46009 = ORIENTED_EDGE ( 'NONE', *, *, #5616, .T. ) ;
#46010 = EDGE_CURVE ( 'NONE', #36415, #25125, #27925, .T. ) ;
#46011 = DIRECTION ( 'NONE',  ( 0.000000000000000000, 0.000000000000000000, -1.000000000000000000 ) ) ;
#46012 = CARTESIAN_POINT ( 'NONE',  ( 0.8753041380234524160, 43.84722337925243352, -22.10337824412637175 ) ) ;
#46013 = CARTESIAN_POINT ( 'NONE',  ( 0.6064515330803585957, -42.17222881740492824, -20.51432310873376963 ) ) ;
#46014 = CARTESIAN_POINT ( 'NONE',  ( 0.5806925824938502512, 45.37089516811273882, 11.86188155343358197 ) ) ;
#46015 = CARTESIAN_POINT ( 'NONE',  ( 5.958863334805807099, 2.677925489610365251, 20.35021240744035964 ) ) ;
#46016 = DIRECTION ( 'NONE',  ( 0.000000000000000000, 0.000000000000000000, 1.000000000000000000 ) ) ;
#46017 = CARTESIAN_POINT ( 'NONE',  ( 5.960721111146673579, 18.96557324978287085, -7.848955554238317589 ) ) ;
#46018 = CARTESIAN_POINT ( 'NONE',  ( 4.975801465491695552, -43.22084481528207078, -20.67815041659126862 ) ) ;
#46019 = CARTESIAN_POINT ( 'NONE',  ( -6.079354080745853928, -11.01762705387068131, -15.79255677051625817 ) ) ;
#46020 = CARTESIAN_POINT ( 'NONE',  ( 4.956445790444035104, 35.28522167764516837, -31.18479086508480691 ) ) ;
#46021 = CARTESIAN_POINT ( 'NONE',  ( 0.5997462898726536595, 23.17609050332929854, -43.29457771044543080 ) ) ;
#46023 = EDGE_CURVE ( 'NONE', #25242, #26909, #31386, .T. ) ;
#46022 = CARTESIAN_POINT ( 'NONE',  ( 4.999999999999986677, 56.56854249492371878, 56.56854249492391062 ) ) ;
#46024 = CARTESIAN_POINT ( 'NONE',  ( 0.1064266379913941657, 30.88821943652570212, 30.09411261783700908 ) ) ;
#46025 = CARTESIAN_POINT ( 'NONE',  ( 7.000000000000021316, -80.00000000000001421, -1.954818893553044610E-31 ) ) ;
#46026 = CARTESIAN_POINT ( 'NONE',  ( 2.185380717157383579, 16.54900345444415066, 40.80380236855377518 ) ) ;
#46027 = EDGE_CURVE ( 'NONE', #11351, #29999, #6922, .T. ) ;
#46028 = CARTESIAN_POINT ( 'NONE',  ( 1.231276596079887931, -7.805643096901414779, -41.18675402191659174 ) ) ;
#46029 = CARTESIAN_POINT ( 'NONE',  ( 0.9762797500689124330, -41.16654106227479559, 7.851158013551082782 ) ) ;
#46030 = VERTEX_POINT ( 'NONE', #31696 ) ;
#46031 = CARTESIAN_POINT ( 'NONE',  ( 0.1102144999581333440, 11.28312052188147518, -41.62223437741658216 ) ) ;
#46032 = CARTESIAN_POINT ( 'NONE',  ( 5.000000000000012434, -80.00000000000001421, -2.649999999999999467 ) ) ;
#46033 = CARTESIAN_POINT ( 'NONE',  ( 4.291220156522059348, 26.18147253908299632, 39.16528428329022660 ) ) ;
#46034 = CARTESIAN_POINT ( 'NONE',  ( 50.00005079999999680, 1.224646799147353256E-15, -10.00000000000000000 ) ) ;
#46035 = VERTEX_POINT ( 'NONE', #26679 ) ;
#46036 = DIRECTION ( 'NONE',  ( 0.000000000000000000, 0.000000000000000000, -1.000000000000000000 ) ) ;
#46037 = CARTESIAN_POINT ( 'NONE',  ( 5.901463166500145796, 0.6576072425839265545, 20.10187610784470635 ) ) ;
#46038 =( BOUNDED_SURFACE ( )  B_SPLINE_SURFACE ( 3, 1, ( 
 ( #20301, #39424 ),
 ( #58476, #29995 ),
 ( #6157, #25294 ),
 ( #20604, #43507 ) ),
 .UNSPECIFIED., .F., .F., .F. ) 
 B_SPLINE_SURFACE_WITH_KNOTS ( ( 4, 4 ),
 ( 2, 2 ),
 ( 0.000000000000000000, 1.000000000000000000 ),
 ( 0.000000000000000000, 1.000000000000000000 ),
 .UNSPECIFIED. ) 
 GEOMETRIC_REPRESENTATION_ITEM ( )  RATIONAL_B_SPLINE_SURFACE ( (
 ( 1.000000000000000000, 1.000000000000000000),
 ( 0.7211978278499970862, 0.9934217856018976445),
 ( 0.7211978278499970862, 0.9934217856018976445),
 ( 1.000000000000000000, 1.000000000000000000) ) ) 
 REPRESENTATION_ITEM ( '' )  SURFACE ( )  );
#46039 = CARTESIAN_POINT ( 'NONE',  ( 5.895881250540457863, -19.39944854657655782, -5.309338725023076577 ) ) ;
#46040 = ORIENTED_EDGE ( 'NONE', *, *, #42181, .F. ) ;
#46041 = ADVANCED_FACE ( 'NONE', ( #3779 ), #26543, .F. ) ;
#46042 = CARTESIAN_POINT ( 'NONE',  ( -6.077587904424778920, -16.14165210942803341, -10.49967087922893150 ) ) ;
#46043 = ORIENTED_EDGE ( 'NONE', *, *, #57561, .T. ) ;
#46044 = CARTESIAN_POINT ( 'NONE',  ( -6.015611763856276717, -18.84324252354755203, -0.006214430185339674118 ) ) ;
#46045 = AXIS2_PLACEMENT_3D ( 'NONE', #58730, #31170, #40919 ) ;
#46046 = CARTESIAN_POINT ( 'NONE',  ( 0.8551540677456715978, -33.23105123575874842, -34.52115452272964546 ) ) ;
#46047 = ORIENTED_EDGE ( 'NONE', *, *, #40281, .T. ) ;
#46048 = CARTESIAN_POINT ( 'NONE',  ( 2.648799415243696664, 41.83591888777205270, -25.57876764242867296 ) ) ;
#46049 = ORIENTED_EDGE ( 'NONE', *, *, #55415, .F. ) ;
#46050 = CARTESIAN_POINT ( 'NONE',  ( 5.974727161628367256, 14.50236057684845115, -14.52429704002348920 ) ) ;
#46051 = CARTESIAN_POINT ( 'NONE',  ( 0.1157506346131639274, 20.49131570213115694, 39.07744414106975483 ) ) ;
#46052 = ORIENTED_EDGE ( 'NONE', *, *, #34816, .F. ) ;
#46053 = CARTESIAN_POINT ( 'NONE',  ( 1.830465331921978356, 5.457173717480057640, -43.71035702091250386 ) ) ;
#46054 = ORIENTED_EDGE ( 'NONE', *, *, #37386, .F. ) ;
#46055 = CARTESIAN_POINT ( 'NONE',  ( 0.5834872094924182795, -37.85980081020200316, -29.33699246747737988 ) ) ;
#46056 =( BOUNDED_SURFACE ( )  B_SPLINE_SURFACE ( 3, 1, ( 
 ( #44149, #44451 ),
 ( #15616, #1791 ),
 ( #53785, #20919 ),
 ( #35345, #10601 ) ),
 .UNSPECIFIED., .F., .F., .F. ) 
 B_SPLINE_SURFACE_WITH_KNOTS ( ( 4, 4 ),
 ( 2, 2 ),
 ( 0.000000000000000000, 1.000000000000000000 ),
 ( 0.000000000000000000, 1.000000000000000000 ),
 .UNSPECIFIED. ) 
 GEOMETRIC_REPRESENTATION_ITEM ( )  RATIONAL_B_SPLINE_SURFACE ( (
 ( 1.000000000000000000, 1.000000000000000000),
 ( 0.9953485035131437453, 0.8621029689291523912),
 ( 0.9953485035131437453, 0.8621029689291523912),
 ( 1.000000000000000000, 1.000000000000000000) ) ) 
 REPRESENTATION_ITEM ( '' )  SURFACE ( )  );
#46057 = VERTEX_POINT ( 'NONE', #7556 ) ;
#46058 = ORIENTED_EDGE ( 'NONE', *, *, #32038, .F. ) ;
#46059 = CARTESIAN_POINT ( 'NONE',  ( 0.5998501479064699549, 34.38546660123250120, 33.64490850298857083 ) ) ;
#46060 = CARTESIAN_POINT ( 'NONE',  ( -2.708315649062910779, -14.63219292706382824, -0.2635547933243013730 ) ) ;
#46061 = CARTESIAN_POINT ( 'NONE',  ( 0.5997462898726536595, -25.00873172704203640, -42.26245340191634625 ) ) ;
#46062 = CARTESIAN_POINT ( 'NONE',  ( 0.5998501479064708430, 11.94461217097404493, 46.60114184914321811 ) ) ;
#46063 = CARTESIAN_POINT ( 'NONE',  ( 4.975801465491695552, 8.787181743660156030, -47.10002938642133330 ) ) ;
#46064 = ORIENTED_EDGE ( 'NONE', *, *, #7037, .F. ) ;
#46065 = CARTESIAN_POINT ( 'NONE',  ( -6.077587904424778920, -1.855182226446173921, 19.16648951426965652 ) ) ;
#46066 = CARTESIAN_POINT ( 'NONE',  ( 0.7954190325252782356, 7.138712176114802688, 47.56618055754177021 ) ) ;
#46067 = CARTESIAN_POINT ( 'NONE',  ( 4.960156602257182357, 3.546989772330555457, -46.28683144126591742 ) ) ;
#46068 = ORIENTED_EDGE ( 'NONE', *, *, #17706, .T. ) ;
#46069 = EDGE_LOOP ( 'NONE', ( #54533, #11432, #9721, #167 ) ) ;
#46070 = CARTESIAN_POINT ( 'NONE',  ( 1.227938101723748288, -42.91134962331486946, -0.8460948827229646252 ) ) ;
#46071 = CARTESIAN_POINT ( 'NONE',  ( -6.077587904424778920, -8.901182807328710922, -17.07527352707552382 ) ) ;
#46072 = CARTESIAN_POINT ( 'NONE',  ( 0.5837800304671216800, -44.31613230802797432, 15.34007005971153603 ) ) ;
#46073 = ORIENTED_EDGE ( 'NONE', *, *, #44605, .F. ) ;
#46074 = DIRECTION ( 'NONE',  ( -1.000000000000000000, -0.000000000000000000, -0.000000000000000000 ) ) ;
#46075 = CARTESIAN_POINT ( 'NONE',  ( 4.956445790443998689, -17.42806872899825521, 43.74700527484080936 ) ) ;
#46076 = EDGE_CURVE ( 'NONE', #46227, #9975, #43588, .T. ) ;
#46077 = B_SPLINE_CURVE_WITH_KNOTS ( 'NONE', 3,
 ( #53714, #10846, #35272, #29939 ),
 .UNSPECIFIED., .F., .F.,
 ( 4, 4 ),
 ( 0.000000000000000000, 0.005013413432710140706 ),
 .UNSPECIFIED. ) ;
#46078 = ORIENTED_EDGE ( 'NONE', *, *, #45305, .T. ) ;
#46079 = CARTESIAN_POINT ( 'NONE',  ( 0.5819845901640494645, 47.42480841519689250, 6.701564444317855695 ) ) ;
#46080 = EDGE_LOOP ( 'NONE', ( #4133, #9905, #44687, #4091 ) ) ;
#46081 = EDGE_CURVE ( 'NONE', #23235, #31634, #52539, .T. ) ;
#46082 = CARTESIAN_POINT ( 'NONE',  ( 0.5806925824938502512, -44.11884900496080775, 15.89809815106926116 ) ) ;
#46083 = CARTESIAN_POINT ( 'NONE',  ( 5.981074661064941900, 14.50705827991425778, 14.51919955600740764 ) ) ;
#46084 = FACE_OUTER_BOUND ( 'NONE', #49644, .T. ) ;
#46085 = VERTEX_POINT ( 'NONE', #52015 ) ;
#46086 = CARTESIAN_POINT ( 'NONE',  ( 3.238018933889920792, -5.886379020808539586, -12.03154330877955402 ) ) ;
#46087 = CARTESIAN_POINT ( 'NONE',  ( 3.270143674763207553, 11.98875605389979349, 6.605065939546861387 ) ) ;
#46088 = CARTESIAN_POINT ( 'NONE',  ( 0.1064266418746777770, -39.62374465289885705, -17.02047513535218926 ) ) ;
#46090 = EDGE_CURVE ( 'NONE', #41909, #29351, #54752, .T. ) ;
#46089 = CARTESIAN_POINT ( 'NONE',  ( 0.1097557419366048670, -16.70891382096342781, -39.75589591229780950 ) ) ;
#46091 = CARTESIAN_POINT ( 'NONE',  ( -90.00000000000000000, 8.239576745513313235E-16, 6.728125000000022560 ) ) ;
#46092 = CARTESIAN_POINT ( 'NONE',  ( 5.894904586330512508, 19.71013252676734240, -4.005007845049880721 ) ) ;
#46093 = CARTESIAN_POINT ( 'NONE',  ( 0.5806925824938499181, 40.06810415365472977, 24.36738377166168235 ) ) ;
#46094 = EDGE_CURVE ( 'NONE', #19831, #50629, #21015, .T. ) ;
#46095 = CARTESIAN_POINT ( 'NONE',  ( 0.6024113833632039894, -49.10696971218104068, -0.2177034400287303217 ) ) ;
#46096 = CARTESIAN_POINT ( 'NONE',  ( -6.016761891674564211, -11.47373234755493243, -14.94721834528426463 ) ) ;
#46097 = DIRECTION ( 'NONE',  ( 1.000000000000000000, 0.000000000000000000, 0.000000000000000000 ) ) ;
#46098 = CARTESIAN_POINT ( 'NONE',  ( 0.6254311100348675101, 33.52633430496182854, 34.49956326955429375 ) ) ;
#46099 = ORIENTED_EDGE ( 'NONE', *, *, #22448, .F. ) ;
#46100 = CARTESIAN_POINT ( 'NONE',  ( 0.1073791018717578927, 6.109314776652701617, -42.68962945260948061 ) ) ;
#46101 = CARTESIAN_POINT ( 'NONE',  ( 0.8551540677456715978, 43.91216198251566283, -19.17641535420805710 ) ) ;
#46102 = CARTESIAN_POINT ( 'NONE',  ( -6.016761891674565099, 11.47373234755524862, -14.94721834528402660 ) ) ;
#46103 = LINE ( 'NONE', #7856, #13709 ) ;
#46104 = VERTEX_POINT ( 'NONE', #9111 ) ;
#46105 = CARTESIAN_POINT ( 'NONE',  ( 0.7245667037590768356, 47.79072416626837594, 5.464144792999545253 ) ) ;
#46106 = CARTESIAN_POINT ( 'NONE',  ( 0.9772918015221176979, -41.84074903630183684, -2.385073548527663956 ) ) ;
#46107 = SURFACE_SIDE_STYLE ('',( #51694 ) ) ;
#46108 = ORIENTED_EDGE ( 'NONE', *, *, #33129, .F. ) ;
#46109 = DIRECTION ( 'NONE',  ( 0.1305261922200498526, 0.9914448613738106042, -0.000000000000000000 ) ) ;
#46110 = ADVANCED_FACE ( 'NONE', ( #28218 ), #32971, .F. ) ;
#46111 = CARTESIAN_POINT ( 'NONE',  ( 0.7762777257811873666, -41.03453903600416908, -24.71864134625273124 ) ) ;
#46112 = CARTESIAN_POINT ( 'NONE',  ( 0.9268187852002115479, -11.59048861154065513, 42.53721789979185530 ) ) ;
#46113 = ORIENTED_EDGE ( 'NONE', *, *, #35882, .F. ) ;
#46114 = CARTESIAN_POINT ( 'NONE',  ( 5.895881250540457863, -2.008683229082083521, 20.01231803898552286 ) ) ;
#46115 = ORIENTED_EDGE ( 'NONE', *, *, #11958, .T. ) ;
#46116 = ORIENTED_EDGE ( 'NONE', *, *, #11042, .F. ) ;
#46117 = CARTESIAN_POINT ( 'NONE',  ( 0.1152809850208375703, 44.01881950007733479, 3.047755290269537287 ) ) ;
#46118 = ORIENTED_EDGE ( 'NONE', *, *, #19348, .F. ) ;
#46119 = FACE_OUTER_BOUND ( 'NONE', #29295, .T. ) ;
#46120 = VERTEX_POINT ( 'NONE', #39119 ) ;
#46121 = CARTESIAN_POINT ( 'NONE',  ( 4.322998006666179727, -42.57894920390112503, -22.13465289016611948 ) ) ;
#46122 = CIRCLE ( 'NONE', #10063, 48.91267123290010943 ) ;
#46123 = CARTESIAN_POINT ( 'NONE',  ( 2.009741617377216460, -0.04086241258242288843, 44.03978210534519633 ) ) ;
#46124 =( BOUNDED_SURFACE ( )  B_SPLINE_SURFACE ( 3, 1, ( 
 ( #45946, #17412 ),
 ( #17113, #22110 ),
 ( #1512, #3285 ),
 ( #58838, #60606 ) ),
 .UNSPECIFIED., .F., .F., .F. ) 
 B_SPLINE_SURFACE_WITH_KNOTS ( ( 4, 4 ),
 ( 2, 2 ),
 ( 0.000000000000000000, 1.000000000000000000 ),
 ( 0.000000000000000000, 1.000000000000000000 ),
 .UNSPECIFIED. ) 
 GEOMETRIC_REPRESENTATION_ITEM ( )  RATIONAL_B_SPLINE_SURFACE ( (
 ( 1.000000000000000000, 1.000000000000000000),
 ( 0.7223157951917480446, 0.9931996967497186413),
 ( 0.7223157951917480446, 0.9931996967497186413),
 ( 1.000000000000000000, 1.000000000000000000) ) ) 
 REPRESENTATION_ITEM ( '' )  SURFACE ( )  );
#46125 = ORIENTED_EDGE ( 'NONE', *, *, #50075, .T. ) ;
#46126 = CARTESIAN_POINT ( 'NONE',  ( 0.1147471544378676767, 15.52999974506124481, 41.30098420608936749 ) ) ;
#46127 = CARTESIAN_POINT ( 'NONE',  ( 4.335381028904216727, 35.88831783935810193, -33.34344748710841344 ) ) ;
#46128 = CARTESIAN_POINT ( 'NONE',  ( 2.706805983486679779, -37.50615468164787103, 23.02312911652235528 ) ) ;
#46129 = CARTESIAN_POINT ( 'NONE',  ( 0.5830081025819919827, -30.06820310196314594, 35.98798683729531689 ) ) ;
#46130 = VERTEX_POINT ( 'NONE', #23519 ) ;
#46131 = DIRECTION ( 'NONE',  ( 1.000000000000000000, 1.836909530733573776E-16, 0.000000000000000000 ) ) ;
#46132 = B_SPLINE_CURVE_WITH_KNOTS ( 'NONE', 3,
 ( #13957, #55908, #23336, #61522, #27406, #18028, #37452, #56523, #18642, #46533, #33062, #47155, #52134, #26794, #27726, #22717 ),
 .UNSPECIFIED., .F., .F.,
 ( 4, 3, 3, 3, 3, 4 ),
 ( 2.221635811791082109E-17, 0.0002612764279487730002, 0.0003919131003184738241, 0.0005225497727000642800, 0.0007837925190632422101, 0.001045051706266712397 ),
 .UNSPECIFIED. ) ;
#46133 = VERTEX_POINT ( 'NONE', #18523 ) ;
#46134 = DIRECTION ( 'NONE',  ( 0.000000000000000000, 0.000000000000000000, 1.000000000000000000 ) ) ;
#46135 = ORIENTED_EDGE ( 'NONE', *, *, #60258, .T. ) ;
#46136 = CARTESIAN_POINT ( 'NONE',  ( 0.9757402383260938006, 26.05362288587366493, 34.09320464257820049 ) ) ;
#46137 = CARTESIAN_POINT ( 'NONE',  ( 0.9268187852002115479, 14.29204361781913946, -41.70721546848916006 ) ) ;
#46138 = ORIENTED_EDGE ( 'NONE', *, *, #13745, .F. ) ;
#46139 = CARTESIAN_POINT ( 'NONE',  ( 0.5838002273316431623, -46.22850660674012602, -12.52789267095232617 ) ) ;
#46140 = FACE_OUTER_BOUND ( 'NONE', #10616, .T. ) ;
#46141 = CARTESIAN_POINT ( 'NONE',  ( 0.6027444965799114707, 27.98794771890257849, 40.35112511902756438 ) ) ;
#46142 = CARTESIAN_POINT ( 'NONE',  ( -6.079354080745853928, -18.27537090945910947, 6.066611358069499360 ) ) ;
#46143 = ADVANCED_FACE ( 'NONE', ( #42647 ), #29285, .F. ) ;
#46144 =( BOUNDED_SURFACE ( )  B_SPLINE_SURFACE ( 3, 1, ( 
 ( #8531, #27654 ),
 ( #46786, #61149 ),
 ( #18268, #13566 ),
 ( #5920, #34475 ) ),
 .UNSPECIFIED., .F., .F., .F. ) 
 B_SPLINE_SURFACE_WITH_KNOTS ( ( 4, 4 ),
 ( 2, 2 ),
 ( 0.000000000000000000, 1.000000000000000000 ),
 ( 0.000000000000000000, 1.000000000000000000 ),
 .UNSPECIFIED. ) 
 GEOMETRIC_REPRESENTATION_ITEM ( )  RATIONAL_B_SPLINE_SURFACE ( (
 ( 1.000000000000000000, 1.000000000000000000),
 ( 0.9953040768229005630, 0.8617119497784937465),
 ( 0.9953040768229005630, 0.8617119497784937465),
 ( 1.000000000000000000, 1.000000000000000000) ) ) 
 REPRESENTATION_ITEM ( '' )  SURFACE ( )  );
#46145 = VERTEX_POINT ( 'NONE', #27922 ) ;
#46146 = VERTEX_POINT ( 'NONE', #13521 ) ;
#46147 = CARTESIAN_POINT ( 'NONE',  ( 0.9785694773339257413, -39.51624465101048855, -13.95714205688820364 ) ) ;
#46148 = CARTESIAN_POINT ( 'NONE',  ( 0.9780303403264770656, -41.79223983423273836, 3.122227255190472395 ) ) ;
#46149 = ADVANCED_FACE ( 'NONE', ( #47044 ), #24914, .F. ) ;
#46150 =( BOUNDED_SURFACE ( )  B_SPLINE_SURFACE ( 3, 1, ( 
 ( #23367, #56246 ),
 ( #32459, #36869 ),
 ( #27438, #50618 ),
 ( #42493, #61250 ) ),
 .UNSPECIFIED., .F., .F., .F. ) 
 B_SPLINE_SURFACE_WITH_KNOTS ( ( 4, 4 ),
 ( 2, 2 ),
 ( 0.000000000000000000, 1.000000000000000000 ),
 ( 0.000000000000000000, 1.000000000000000000 ),
 .UNSPECIFIED. ) 
 GEOMETRIC_REPRESENTATION_ITEM ( )  RATIONAL_B_SPLINE_SURFACE ( (
 ( 1.000000000000000000, 1.000000000000000000),
 ( 0.7282232189291694135, 0.9929344683865672927),
 ( 0.7282232189291694135, 0.9929344683865672927),
 ( 1.000000000000000000, 1.000000000000000000) ) ) 
 REPRESENTATION_ITEM ( '' )  SURFACE ( )  );
#46151 = CARTESIAN_POINT ( 'NONE',  ( 0.9754642270333696574, -16.58255499746102757, 39.57465882553921688 ) ) ;
#46152 = EDGE_CURVE ( 'NONE', #8500, #61919, #40597, .T. ) ;
#46153 = CARTESIAN_POINT ( 'NONE',  ( 2.225817577893341337, -0.2642321622234031220, 49.03513408093338199 ) ) ;
#46154 = CARTESIAN_POINT ( 'NONE',  ( 4.694002226626920127, 18.76791414987460982, 41.54575995103556352 ) ) ;
#46155 = CARTESIAN_POINT ( 'NONE',  ( 0.5988103622719990193, 38.53259676306921477, -28.80261254779997770 ) ) ;
#46156 = CARTESIAN_POINT ( 'NONE',  ( 0.7242003506639906885, -42.37567836115716347, 24.80551466020780538 ) ) ;
#46157 = CARTESIAN_POINT ( 'NONE',  ( 0.9762797500689124330, 35.79768877047989406, -21.79105926469756938 ) ) ;
#46158 = EDGE_CURVE ( 'NONE', #45408, #6056, #32015, .T. ) ;
#46159 = DIRECTION ( 'NONE',  ( -1.718001593797181987E-16, 1.000000000000000000, 0.000000000000000000 ) ) ;
#46160 = CARTESIAN_POINT ( 'NONE',  ( 0.6031357023905875581, -33.98625823839277160, -34.04794059289636721 ) ) ;
#46161 = FACE_OUTER_BOUND ( 'NONE', #56326, .T. ) ;
#46162 = CARTESIAN_POINT ( 'NONE',  ( 0.6017667736363752073, -5.933018439714995651, -47.74032759880252996 ) ) ;
#46163 = VECTOR ( 'NONE', #20560, 1000.000000000000000 ) ;
#46164 = DIRECTION ( 'NONE',  ( -1.000000000000000000, -1.836909530733573776E-16, 2.465190328815655050E-32 ) ) ;
#46165 = CARTESIAN_POINT ( 'NONE',  ( 0.7762777257811894760, -43.90991299786887225, -19.15108781300977725 ) ) ;
#46166 = CARTESIAN_POINT ( 'NONE',  ( 0.2500000000000002220, 0.000000000000000000, 0.000000000000000000 ) ) ;
#46168 = EDGE_LOOP ( 'NONE', ( #7796, #611, #27619, #61040 ) ) ;
#46167 = CARTESIAN_POINT ( 'NONE',  ( 1.827119703190779765, 43.03226500438895386, -1.232688548475576074 ) ) ;
#46169 = VERTEX_POINT ( 'NONE', #39737 ) ;
#46170 = CARTESIAN_POINT ( 'NONE',  ( 0.6008123274975392114, 17.36800808579142341, -45.93372232130052879 ) ) ;
#46171 = CARTESIAN_POINT ( 'NONE',  ( 5.896782393890504181, 3.339090646272911300, -19.83372281075806853 ) ) ;
#46172 = CARTESIAN_POINT ( 'NONE',  ( 0.6252788684277243991, 44.53702795073676413, 20.68568279001112842 ) ) ;
#46173 = VERTEX_POINT ( 'NONE', #51711 ) ;
#46174 = ORIENTED_EDGE ( 'NONE', *, *, #14308, .F. ) ;
#46175 = CARTESIAN_POINT ( 'NONE',  ( -6.079354080745853928, 12.00682274379690817, -15.05420747987762020 ) ) ;
#46177 = B_SPLINE_CURVE_WITH_KNOTS ( 'NONE', 3,
 ( #13987, #32775, #456, #9562, #19600, #51853 ),
 .UNSPECIFIED., .F., .F.,
 ( 4, 2, 4 ),
 ( 0.000000000000000000, 0.0002450742804987337425, 0.0004901485609974674850 ),
 .UNSPECIFIED. ) ;
#46176 = DIRECTION ( 'NONE',  ( -0.07500201931887526263, 0.2180102369365608250, -0.9730602415518555537 ) ) ;
#46178 = UNCERTAINTY_MEASURE_WITH_UNIT (LENGTH_MEASURE( 1.000000000000000082E-05 ), #18785, 'distance_accuracy_value', 'NONE');
#46179 = ORIENTED_EDGE ( 'NONE', *, *, #42809, .F. ) ;
#46180 = ORIENTED_EDGE ( 'NONE', *, *, #40847, .T. ) ;
#46181 = CARTESIAN_POINT ( 'NONE',  ( 4.553261556744873317, -25.31600221269608397, -35.89762663172042068 ) ) ;
#46182 = CARTESIAN_POINT ( 'NONE',  ( 0.1129192098497447394, 43.40062318508790895, 7.958498283669150020 ) ) ;
#46183 = ADVANCED_FACE ( 'NONE', ( #4382 ), #18024, .F. ) ;
#46184 = ORIENTED_EDGE ( 'NONE', *, *, #54267, .T. ) ;
#46185 = CARTESIAN_POINT ( 'NONE',  ( 4.549368137175248350, 40.58005590356670211, 13.99871866169379508 ) ) ;
#46186 = EDGE_CURVE ( 'NONE', #21995, #50764, #53964, .T. ) ;
#46187 = CARTESIAN_POINT ( 'NONE',  ( 0.7044674535453004927, -42.37103341363683739, 24.82938280085469884 ) ) ;
#46188 = B_SPLINE_CURVE_WITH_KNOTS ( 'NONE', 3,
 ( #44328, #39310, #14891, #14579 ),
 .UNSPECIFIED., .F., .F.,
 ( 4, 4 ),
 ( 0.000000000000000000, 0.005013413432710144176 ),
 .UNSPECIFIED. ) ;
#46189 = CARTESIAN_POINT ( 'NONE',  ( 0.1103936448916665869, 5.228610780659758526E-15, -43.12443171339897674 ) ) ;
#46190 = ORIENTED_EDGE ( 'NONE', *, *, #60317, .F. ) ;
#46191 = EDGE_CURVE ( 'NONE', #16304, #27102, #35018, .T. ) ;
#46192 = ORIENTED_EDGE ( 'NONE', *, *, #13368, .F. ) ;
#46193 = CARTESIAN_POINT ( 'NONE',  ( 0.8560838555295223751, 46.89922841446243496, -0.9138972643637069959 ) ) ;
#46194 = ORIENTED_EDGE ( 'NONE', *, *, #55821, .T. ) ;
#46195 = CARTESIAN_POINT ( 'NONE',  ( 0.6029443199889047422, -48.70423496034977973, 6.279740343473172004 ) ) ;
#46196 = CARTESIAN_POINT ( 'NONE',  ( -5.995132425357893702, -0.008513469642675032187, -18.84415457712583475 ) ) ;
#46197 = CARTESIAN_POINT ( 'NONE',  ( 0.5797568599927139799, -20.30903442135246806, 42.27018369422267341 ) ) ;
#46198 = CARTESIAN_POINT ( 'NONE',  ( 0.8744876279028306332, -29.90976330662902427, 38.93271258621624042 ) ) ;
#46199 = CARTESIAN_POINT ( 'NONE',  ( -6.010958268070873523, 2.445171577615762537, 18.68413620842265033 ) ) ;
#46200 = B_SPLINE_CURVE_WITH_KNOTS ( 'NONE', 3,
 ( #32806, #47826, #42827, #47206, #57180, #4873, #52496, #9280, #42515, #14313 ),
 .UNSPECIFIED., .F., .F.,
 ( 4, 3, 3, 4 ),
 ( 1.095097866269904440E-17, 0.0002724568934985560891, 0.0004086836638483806890, 0.0005448802484326158158 ),
 .UNSPECIFIED. ) ;
#46201 = VERTEX_POINT ( 'NONE', #36261 ) ;
#46202 = CARTESIAN_POINT ( 'NONE',  ( 0.9740398440564311811, -30.63262235044608062, -30.04629765303421607 ) ) ;
#46203 = AXIS2_PLACEMENT_3D ( 'NONE', #9288, #23705, #61583 ) ;
#46204 = CARTESIAN_POINT ( 'NONE',  ( 4.335381028904201628, 6.815065961880899970, -48.51094436928184450 ) ) ;
#46205 = AXIS2_PLACEMENT_3D ( 'NONE', #61915, #38782, #48163 ) ;
#46206 = CARTESIAN_POINT ( 'NONE',  ( 2.301430502907643838, 37.31003439265366239, 30.25184447737447613 ) ) ;
#46207 = VERTEX_POINT ( 'NONE', #59415 ) ;
#46208 = CARTESIAN_POINT ( 'NONE',  ( 1.231276596079887931, -35.03243822710496858, -23.02183839058345072 ) ) ;
#46209 = CARTESIAN_POINT ( 'NONE',  ( 4.962356264823601926, -38.57439820587641321, 16.83007429920694875 ) ) ;
#46210 = CARTESIAN_POINT ( 'NONE',  ( 0.8751705887134553219, -48.08707113907594533, 0.8911681664086766874 ) ) ;
#46211 = CARTESIAN_POINT ( 'NONE',  ( 0.7048096507298635682, 11.63498350884336574, -46.68221792389230984 ) ) ;
#46212 = EDGE_CURVE ( 'NONE', #23179, #19831, #54706, .T. ) ;
#46213 = ORIENTED_EDGE ( 'NONE', *, *, #50062, .T. ) ;
#46214 = CARTESIAN_POINT ( 'NONE',  ( 0.9762797500689124330, -41.77809974471944088, 3.303810967046753255 ) ) ;
#46215 = EDGE_CURVE ( 'NONE', #33056, #35697, #56003, .T. ) ;
#46216 = CYLINDRICAL_SURFACE ( 'NONE', #50679, 85.00000000000001421 ) ;
#46217 = CARTESIAN_POINT ( 'NONE',  ( 0.7048096507298635682, -0.8437160066903991451, -48.10291524268441776 ) ) ;
#46218 = EDGE_CURVE ( 'NONE', #48340, #60124, #45656, .T. ) ;
#46219 = CARTESIAN_POINT ( 'NONE',  ( -2.700785417809989042, -13.56184546075576769, -3.000000000000003997 ) ) ;
#46220 =( BOUNDED_CURVE ( )  B_SPLINE_CURVE ( 3, ( #61652, #30938, #49732, #31245 ),
 .UNSPECIFIED., .F., .F. ) 
 B_SPLINE_CURVE_WITH_KNOTS ( ( 4, 4 ),
 ( 3.141592653589793116, 6.283185307179586232 ),
 .UNSPECIFIED. ) 
 CURVE ( )  GEOMETRIC_REPRESENTATION_ITEM ( )  RATIONAL_B_SPLINE_CURVE ( ( 1.000000000000000000, 0.3333333333333333703, 0.3333333333333333703, 1.000000000000000000 ) ) 
 REPRESENTATION_ITEM ( '' )  );
#46221 = CARTESIAN_POINT ( 'NONE',  ( 0.5817217712918324457, -46.81948268753178155, 2.677871333780827090 ) ) ;
#46222 = CARTESIAN_POINT ( 'NONE',  ( 0.9736507210033064075, 42.90603603725247694, 0.4504567742782497608 ) ) ;
#46223 = CARTESIAN_POINT ( 'NONE',  ( 0.9745511491811744698, -5.262846425219327884, -42.58443036172452167 ) ) ;
#46224 = CARTESIAN_POINT ( 'NONE',  ( 4.975610109902397937, 0.000000000000000000, 0.000000000000000000 ) ) ;
#46225 = CARTESIAN_POINT ( 'NONE',  ( 0.5827359174754817017, 37.77623182210397346, 29.44457394064633959 ) ) ;
#46226 = CARTESIAN_POINT ( 'NONE',  ( 0.6067375320500717484, -18.98242280073596078, 43.97491060910881799 ) ) ;
#46227 = VERTEX_POINT ( 'NONE', #6775 ) ;
#46228 = CARTESIAN_POINT ( 'NONE',  ( 4.335381028904216727, -40.49335964728600601, -27.56890770668824686 ) ) ;
#46229 = B_SPLINE_CURVE_WITH_KNOTS ( 'NONE', 3,
 ( #41194, #45279, #35257, #44973, #6693, #55557, #21138, #44658, #22072, #12074, #40283, #60257, #59335, #16438, #36491, #50258 ),
 .UNSPECIFIED., .F., .F.,
 ( 4, 3, 3, 3, 3, 4 ),
 ( 1.040890552917501732E-17, 0.0002724568934985551675, 0.0004086836638483766233, 0.0005449104342063557788, 0.0008173270854453663480, 0.001089761613562691828 ),
 .UNSPECIFIED. ) ;
#46230 = CARTESIAN_POINT ( 'NONE',  ( -4.000000000000000000, 0.7862748000878172494, -5.565527722372433317 ) ) ;
#46231 = CARTESIAN_POINT ( 'NONE',  ( -6.015611763856276717, 14.95313250337430055, 11.46610900684727952 ) ) ;
#46232 = EDGE_CURVE ( 'NONE', #22826, #19831, #29012, .T. ) ;
#46233 = DIRECTION ( 'NONE',  ( -1.000000000000000000, -5.380183451256670742E-17, 1.298891185607911324E-16 ) ) ;
#46234 = CARTESIAN_POINT ( 'NONE',  ( 0.8744876279028306332, 46.30617036199629410, -16.31222353896820110 ) ) ;
#46235 = SHAPE_DEFINITION_REPRESENTATION ( #46838, #42491 ) ;
#46236 = CARTESIAN_POINT ( 'NONE',  ( 0.5782707292762442330, -42.18185855468866663, 20.50432058322967777 ) ) ;
#46237 = CARTESIAN_POINT ( 'NONE',  ( 2.009741617377216460, 36.14358544831069509, -25.16237883356238569 ) ) ;
#46238 = CARTESIAN_POINT ( 'NONE',  ( 3.238741278300274029, 32.96375560769460122, 27.59904135366547351 ) ) ;
#46240 = ORIENTED_EDGE ( 'NONE', *, *, #40946, .T. ) ;
#46239 = CARTESIAN_POINT ( 'NONE',  ( 5.960721111146673579, -5.318514366754798495, -19.82454228767744198 ) ) ;
#46241 = ORIENTED_EDGE ( 'NONE', *, *, #5166, .F. ) ;
#46242 = CARTESIAN_POINT ( 'NONE',  ( 1.091591847532195514, 3.418266415782475587, 41.77408820867997008 ) ) ;
#46243 = DIRECTION ( 'NONE',  ( 0.000000000000000000, 0.000000000000000000, 1.000000000000000000 ) ) ;
#46244 = CARTESIAN_POINT ( 'NONE',  ( 0.000000000000000000, 1.178949249685212974, -2.042000000000001148 ) ) ;
#46245 = ORIENTED_EDGE ( 'NONE', *, *, #43181, .F. ) ;
#46246 = CARTESIAN_POINT ( 'NONE',  ( 0.7948884756798506590, -47.26562353173273578, -13.29133088733651036 ) ) ;
#46247 = LINE ( 'NONE', #17730, #39194 ) ;
#46248 = CARTESIAN_POINT ( 'NONE',  ( -6.010958268070873523, -13.33459572764748202, -13.31406649671976794 ) ) ;
#46249 = VECTOR ( 'NONE', #59146, 1000.000000000000000 ) ;
#46250 = CIRCLE ( 'NONE', #61196, 15.38217999999999996 ) ;
#46251 = ORIENTED_EDGE ( 'NONE', *, *, #48779, .T. ) ;
#46252 = ORIENTED_EDGE ( 'NONE', *, *, #5792, .F. ) ;
#46253 = B_SPLINE_CURVE_WITH_KNOTS ( 'NONE', 3,
 ( #15728, #34834, #11025, #39862, #29494, #14800, #43946, #34522, #10714, #20117, #21032, #40173, #54204, #48303, #15106, #670 ),
 .UNSPECIFIED., .F., .F.,
 ( 4, 3, 3, 3, 3, 4 ),
 ( 9.813676791237319219E-18, 0.0002724568934985470360, 0.0004086836638483682207, 0.0005449104342063432020, 0.0008173270854453615775, 0.001089761613562694213 ),
 .UNSPECIFIED. ) ;
#46254 = CARTESIAN_POINT ( 'NONE',  ( -5.283180000000052168, 0.000000000000000000, 0.000000000000000000 ) ) ;
#46255 = CARTESIAN_POINT ( 'NONE',  ( 3.390910168358337362, 37.89548767558103748, 22.31656672437592448 ) ) ;
#46256 = CARTESIAN_POINT ( 'NONE',  ( 0.3622758884714600280, -42.62881903538205108, -6.444611261694439541 ) ) ;
#46257 = ORIENTED_EDGE ( 'NONE', *, *, #16572, .F. ) ;
#46258 = EDGE_CURVE ( 'NONE', #33003, #43585, #21944, .T. ) ;
#46259 = CARTESIAN_POINT ( 'NONE',  ( -4.908599999999999852, 0.000000000000000000, 3.000000000000000000 ) ) ;
#46260 = EDGE_CURVE ( 'NONE', #14125, #3786, #18834, .T. ) ;
#46261 = CARTESIAN_POINT ( 'NONE',  ( 0.5848930533535030563, 43.24595201260145672, -18.14003078584298478 ) ) ;
#46262 = CARTESIAN_POINT ( 'NONE',  ( 0.5809828226811553087, 38.32755012159145025, 28.72298383114502229 ) ) ;
#46263 = CARTESIAN_POINT ( 'NONE',  ( -6.078075953587585900, -6.645381366291554848, 18.07302079741184286 ) ) ;
#46264 = EDGE_LOOP ( 'NONE', ( #24611, #4990, #50313, #12254 ) ) ;
#46265 = EDGE_CURVE ( 'NONE', #51250, #50661, #57612, .T. ) ;
#46266 = ADVANCED_FACE ( 'NONE', ( #13374 ), #39375, .F. ) ;
#46267 = PLANE ( 'NONE',  #6802 ) ;
#46268 = CARTESIAN_POINT ( 'NONE',  ( 5.959828726073459926, 20.35060134307031277, 2.674641840416243532 ) ) ;
#46269 = ORIENTED_EDGE ( 'NONE', *, *, #27506, .T. ) ;
#46270 = LINE ( 'NONE', #13365, #30519 ) ;
#46271 = EDGE_CURVE ( 'NONE', #19605, #19530, #10621, .T. ) ;
#46272 = CARTESIAN_POINT ( 'NONE',  ( 5.860006189529234355, -48.13093674595582883, -3.137522369586017934 ) ) ;
#46273 = CARTESIAN_POINT ( 'NONE',  ( 0.8557997880470606944, 38.55640757422477805, -28.43566216844931915 ) ) ;
#46274 = ORIENTED_EDGE ( 'NONE', *, *, #32549, .T. ) ;
#46275 = VERTEX_POINT ( 'NONE', #27769 ) ;
#46276 = CARTESIAN_POINT ( 'NONE',  ( 4.549368137175248350, 0.000000000000000000, 0.000000000000000000 ) ) ;
#46277 = CARTESIAN_POINT ( 'NONE',  ( 0.5839879327111925367, 41.52454255611505829, 23.86931774877311696 ) ) ;
#46278 = ORIENTED_EDGE ( 'NONE', *, *, #20179, .T. ) ;
#46279 = CARTESIAN_POINT ( 'NONE',  ( -6.079354080745853928, -6.649248899792234546, -18.07153685541917909 ) ) ;
#46280 = EDGE_CURVE ( 'NONE', #50174, #51012, #60961, .T. ) ;
#46281 = ORIENTED_EDGE ( 'NONE', *, *, #52915, .T. ) ;
#46282 = DIRECTION ( 'NONE',  ( 0.000000000000000000, 0.000000000000000000, 1.000000000000000000 ) ) ;
#46283 = ORIENTED_EDGE ( 'NONE', *, *, #14675, .T. ) ;
#46284 = CARTESIAN_POINT ( 'NONE',  ( 0.9730545539215883499, 26.52009130076770305, 33.73144377768567637 ) ) ;
#46285 = CARTESIAN_POINT ( 'NONE',  ( 0.9790724872846768845, 24.82680137436399903, 33.76336984809620390 ) ) ;
#46286 = EDGE_CURVE ( 'NONE', #58089, #41630, #21036, .T. ) ;
#46287 = CARTESIAN_POINT ( 'NONE',  ( 0.1073791018717578927, -26.63563652260192427, 33.91564619577761874 ) ) ;
#46288 = VERTEX_POINT ( 'NONE', #3321 ) ;
#46289 = CARTESIAN_POINT ( 'NONE',  ( 0.1140933569871965536, 43.23646427744231602, 8.806708060868194465 ) ) ;
#46290 = CARTESIAN_POINT ( 'NONE',  ( 5.960221823109900008, -14.51763960716788482, 14.50993159119785858 ) ) ;
#46291 = CARTESIAN_POINT ( 'NONE',  ( 2.648799415243708655, -0.1860685961560771262, 49.03552632293369129 ) ) ;
#46292 = ORIENTED_EDGE ( 'NONE', *, *, #46945, .F. ) ;
#46293 = AXIS2_PLACEMENT_3D ( 'NONE', #42283, #4948, #24077 ) ;
#46294 = CARTESIAN_POINT ( 'NONE',  ( 4.834790513006555379, 46.91907382339837085, 5.584787594785887599 ) ) ;
#46295 = CARTESIAN_POINT ( 'NONE',  ( 0.5980894510889448457, -44.71414919659918752, 17.76188940524868443 ) ) ;
#46296 = CARTESIAN_POINT ( 'NONE',  ( 0.6023142530420679819, 47.66103033449098803, -6.538792732869364244 ) ) ;
#46297 = CARTESIAN_POINT ( 'NONE',  ( -2.601141883200665639, 0.9866742854873818969, 14.89368662634428730 ) ) ;
#46298 = ORIENTED_EDGE ( 'NONE', *, *, #49432, .F. ) ;
#46299 = CARTESIAN_POINT ( 'NONE',  ( 5.860006189529246790, 9.393028332204737652, 47.30964106197861696 ) ) ;
#46300 = CARTESIAN_POINT ( 'NONE',  ( 2.643462169533613793, -47.42536612906434357, 7.637863311826802892 ) ) ;
#46301 = ORIENTED_EDGE ( 'NONE', *, *, #23189, .T. ) ;
#46302 = CARTESIAN_POINT ( 'NONE',  ( 5.959547316686252039, -7.858107265727872992, 18.96183906913529782 ) ) ;
#46303 = CARTESIAN_POINT ( 'NONE',  ( 4.967162193818131399, -35.57684288741960899, -24.30453456948146851 ) ) ;
#46304 = CARTESIAN_POINT ( 'NONE',  ( 0.6021447746440204973, 44.35701149669154120, 21.07122849220856153 ) ) ;
#46305 = CARTESIAN_POINT ( 'NONE',  ( -6.017396004339686577, -14.95000090562873396, -11.47005965438154362 ) ) ;
#46307 = ADVANCED_FACE ( 'NONE', ( #23077, #37822 ), #18381, .T. ) ;
#46306 = B_SPLINE_CURVE_WITH_KNOTS ( 'NONE', 3,
 ( #35066, #21567, #16559, #54747, #45698, #39461 ),
 .UNSPECIFIED., .F., .F.,
 ( 4, 2, 4 ),
 ( 2.224307874377020740E-17, 0.0002293755540694337851, 0.0004587511081388452898 ),
 .UNSPECIFIED. ) ;
#46308 = CARTESIAN_POINT ( 'NONE',  ( 0.3622758884714730732, -17.25816669464967035, -39.50828911766992491 ) ) ;
#46309 = CARTESIAN_POINT ( 'NONE',  ( 4.291220156522059348, -41.03139692541890327, -23.14764488353881688 ) ) ;
#46310 = CARTESIAN_POINT ( 'NONE',  ( 5.896782393890504181, -2.019528367549592307, 20.01118667272569951 ) ) ;
#46311 = CARTESIAN_POINT ( 'NONE',  ( 5.981074661064941900, 5.320466518160936076, -19.82308078259086059 ) ) ;
#46312 = EDGE_CURVE ( 'NONE', #55549, #50931, #24003, .T. ) ;
#46313 = CARTESIAN_POINT ( 'NONE',  ( 0.6000166863083106206, 28.52380356231368097, 39.97769518177598513 ) ) ;
#46314 = CARTESIAN_POINT ( 'NONE',  ( 0.8744876279028306332, -39.87136468799875644, -28.64654129726831044 ) ) ;
#46315 = CARTESIAN_POINT ( 'NONE',  ( 0.1368894036331272379, -28.00595822950079494, -34.09585941974172840 ) ) ;
#46316 = DIRECTION ( 'NONE',  ( -1.000000000000000000, -5.380183451256670742E-17, 1.298891185607911324E-16 ) ) ;
#46317 = CARTESIAN_POINT ( 'NONE',  ( 0.3622758884714730732, 31.06363466427686504, 29.89648521331642428 ) ) ;
#46318 = CARTESIAN_POINT ( 'NONE',  ( 0.5806925824938494740, -34.41156632303759011, 31.86010774524702072 ) ) ;
#46319 = CARTESIAN_POINT ( 'NONE',  ( 2.706805983486679779, 16.74203531073313655, 40.69988165798421420 ) ) ;
#46320 = PRODUCT_RELATED_PRODUCT_CATEGORY ( 'part', '', ( #36825 ) ) ;
#46321 = PRODUCT_DEFINITION_SHAPE ( 'NONE', 'NONE',  #8814 ) ;
#46322 = DIRECTION ( 'NONE',  ( -0.07836865515943411409, -0.8672783706145124061, -0.4916162952473585590 ) ) ;
#46323 = CARTESIAN_POINT ( 'NONE',  ( 4.960386119450146403, 0.9915941002490832323, -43.74303608361785223 ) ) ;
#46324 = CARTESIAN_POINT ( 'NONE',  ( 0.6009452777970413218, -37.89911497740590818, 29.63106797105349699 ) ) ;
#46325 = VERTEX_POINT ( 'NONE', #32794 ) ;
#46326 = CARTESIAN_POINT ( 'NONE',  ( 0.9740398440564311811, 10.70454588197344670, -41.55177796653836708 ) ) ;
#46327 = CARTESIAN_POINT ( 'NONE',  ( 3.390910168358337362, -32.93065864425445710, -29.14907987894689612 ) ) ;
#46328 = CARTESIAN_POINT ( 'NONE',  ( 4.834790513006555379, 45.81970208965012148, 11.53881455523459643 ) ) ;
#46329 = CARTESIAN_POINT ( 'NONE',  ( 0.09136607875274982415, 0.000000000000000000, 0.000000000000000000 ) ) ;
#46330 = ORIENTED_EDGE ( 'NONE', *, *, #1458, .T. ) ;
#46331 = EDGE_CURVE ( 'NONE', #12531, #10350, #55633, .T. ) ;
#46332 = CARTESIAN_POINT ( 'NONE',  ( 5.959828726073459926, 14.51059719297116679, -14.51699876360184938 ) ) ;
#46333 =( GEOMETRIC_REPRESENTATION_CONTEXT ( 3 ) GLOBAL_UNCERTAINTY_ASSIGNED_CONTEXT ( ( #41174 ) ) GLOBAL_UNIT_ASSIGNED_CONTEXT ( ( #17423, #10185, #53383 ) ) REPRESENTATION_CONTEXT ( 'NONE', 'WORKASPACE' ) );
#46334 = EDGE_CURVE ( 'NONE', #30625, #17526, #41272, .T. ) ;
#46335 = CARTESIAN_POINT ( 'NONE',  ( 0.6031356755773454870, 24.05369945659533926, -41.66228085015301730 ) ) ;
#46336 = ORIENTED_EDGE ( 'NONE', *, *, #13106, .T. ) ;
#46337 =( BOUNDED_SURFACE ( )  B_SPLINE_SURFACE ( 3, 1, ( 
 ( #12217, #31301 ),
 ( #45122, #16592 ),
 ( #11915, #1852 ),
 ( #40123, #44201 ) ),
 .UNSPECIFIED., .F., .F., .F. ) 
 B_SPLINE_SURFACE_WITH_KNOTS ( ( 4, 4 ),
 ( 2, 2 ),
 ( 0.000000000000000000, 1.000000000000000000 ),
 ( 0.000000000000000000, 1.000000000000000000 ),
 .UNSPECIFIED. ) 
 GEOMETRIC_REPRESENTATION_ITEM ( )  RATIONAL_B_SPLINE_SURFACE ( (
 ( 1.000000000000000000, 1.000000000000000000),
 ( 0.9754377213608244057, 0.9999580625633939235),
 ( 0.9754377213608244057, 0.9999580625633939235),
 ( 1.000000000000000000, 1.000000000000000000) ) ) 
 REPRESENTATION_ITEM ( '' )  SURFACE ( )  );
#46338 = DIRECTION ( 'NONE',  ( 0.000000000000000000, 0.000000000000000000, -1.000000000000000000 ) ) ;
#46339 = ORIENTED_EDGE ( 'NONE', *, *, #23361, .F. ) ;
#46340 = ADVANCED_FACE ( 'NONE', ( #56874 ), #61287, .F. ) ;
#46341 = CARTESIAN_POINT ( 'NONE',  ( 0.5839879327111902052, -0.09083573661678309707, -47.89596760851026858 ) ) ;
#46342 = ORIENTED_EDGE ( 'NONE', *, *, #16407, .T. ) ;
#46343 = CARTESIAN_POINT ( 'NONE',  ( 4.335381028904216727, 2.583895202258514878, -48.91912032373529939 ) ) ;
#46344 = EDGE_CURVE ( 'NONE', #2381, #5855, #13790, .T. ) ;
#46345 = CARTESIAN_POINT ( 'NONE',  ( 0.5839879882012665169, -29.15719377327474859, 37.99844431214160778 ) ) ;
#46346 = ORIENTED_EDGE ( 'NONE', *, *, #26212, .F. ) ;
#46347 = CARTESIAN_POINT ( 'NONE',  ( 0.9749527285493303497, 21.20640438431190233, 37.30179927241184856 ) ) ;
#46348 = DIRECTION ( 'NONE',  ( -0.07500201931887527651, 0.7908860163360004192, 0.6073499866323063268 ) ) ;
#46349 = CONICAL_SURFACE ( 'NONE', #19335, 43.92652462719577500, 1.486293639869522343 ) ;
#46350 = VERTEX_POINT ( 'NONE', #53699 ) ;
#46351 = EDGE_LOOP ( 'NONE', ( #5987, #46174, #18575, #4704 ) ) ;
#46352 = CARTESIAN_POINT ( 'NONE',  ( 0.1129192098497455998, -1.898585089632445433, 44.08341142019953907 ) ) ;
#46353 = ORIENTED_EDGE ( 'NONE', *, *, #33329, .F. ) ;
#46354 = ORIENTED_EDGE ( 'NONE', *, *, #10176, .T. ) ;
#46355 = CARTESIAN_POINT ( 'NONE',  ( -6.077587904424778920, -4.278847002849283321, 18.77465018902185179 ) ) ;
#46356 = CARTESIAN_POINT ( 'NONE',  ( 1.091591847532194182, -7.739709431952981333, 41.19291066269509116 ) ) ;
#46357 = CARTESIAN_POINT ( 'NONE',  ( 0.6021448801613057400, -25.23316997730999134, -42.12871077451965363 ) ) ;
#46358 = CARTESIAN_POINT ( 'NONE',  ( 4.291220156522060236, -43.75057291092651468, 17.47215977695375244 ) ) ;
#46359 = LINE ( 'NONE', #31010, #47706 ) ;
#46360 = EDGE_LOOP ( 'NONE', ( #13210, #34337, #24245, #52511 ) ) ;
#46361 = CARTESIAN_POINT ( 'NONE',  ( 4.967162193818130511, -35.57684288741994294, 24.30453456948097823 ) ) ;
#46362 = CARTESIAN_POINT ( 'NONE',  ( 2.624215991343608501, -46.71702075422659561, 11.05657803851029364 ) ) ;
#46363 = CARTESIAN_POINT ( 'NONE',  ( 0.6064515330803588178, -34.30059540857045164, 31.98129907703317087 ) ) ;
#46364 = ORIENTED_EDGE ( 'NONE', *, *, #52664, .F. ) ;
#46365 = B_SPLINE_CURVE_WITH_KNOTS ( 'NONE', 3,
 ( #56773, #37395, #28583, #23284, #51455, #56467 ),
 .UNSPECIFIED., .F., .F.,
 ( 4, 2, 4 ),
 ( 8.787390050835121380E-18, 0.0002448709889506573735, 0.0004897419779013059650 ),
 .UNSPECIFIED. ) ;
#46366 = ORIENTED_EDGE ( 'NONE', *, *, #42060, .F. ) ;
#46367 = FACE_OUTER_BOUND ( 'NONE', #13649, .T. ) ;
#46368 = CARTESIAN_POINT ( 'NONE',  ( 2.528190830796654964, 28.30160364192409972, 31.00440883888025922 ) ) ;
#46369 = CARTESIAN_POINT ( 'NONE',  ( 0.5806925824938502512, -44.11884900496080775, 15.89809815106926116 ) ) ;
#46370 = VERTEX_POINT ( 'NONE', #159 ) ;
#46371 = CARTESIAN_POINT ( 'NONE',  ( 0.1102144999581332607, -42.73889315046716320, -5.753800096705892209 ) ) ;
#46372 = B_SPLINE_CURVE_WITH_KNOTS ( 'NONE', 3,
 ( #59215, #12263, #16320, #21027 ),
 .UNSPECIFIED., .F., .F.,
 ( 4, 4 ),
 ( 0.000000000000000000, 0.005013413432710150247 ),
 .UNSPECIFIED. ) ;
#46373 = CARTESIAN_POINT ( 'NONE',  ( 0.5848930533535030563, 4.875316827622536486, 46.64230234688099586 ) ) ;
#46374 = ORIENTED_EDGE ( 'NONE', *, *, #34318, .T. ) ;
#46375 = CARTESIAN_POINT ( 'NONE',  ( 1.231276596079881047, -0.5545928549373742023, -41.91621640586514985 ) ) ;
#46376 = CARTESIAN_POINT ( 'NONE',  ( 4.553261556744875094, 0.000000000000000000, 0.000000000000000000 ) ) ;
#46377 = CARTESIAN_POINT ( 'NONE',  ( 0.9754402186311929013, -33.92707563620664502, 26.26956909363305215 ) ) ;
#46378 = CARTESIAN_POINT ( 'NONE',  ( 45.00000000000001421, 0.000000000000000000, 0.000000000000000000 ) ) ;
#46379 = VECTOR ( 'NONE', #58739, 999.9999999999998863 ) ;
#46380 = DIRECTION ( 'NONE',  ( -1.000000000000000000, -0.000000000000000000, -0.000000000000000000 ) ) ;
#46381 = DIRECTION ( 'NONE',  ( 1.000000000000000000, -0.000000000000000000, -0.000000000000000000 ) ) ;
#46382 = EDGE_CURVE ( 'NONE', #51030, #36286, #15829, .T. ) ;
#46383 = ORIENTED_EDGE ( 'NONE', *, *, #39561, .F. ) ;
#46384 = CARTESIAN_POINT ( 'NONE',  ( 0.9741495583595167762, 21.79582154536855754, -36.96045061395513187 ) ) ;
#46385 = CARTESIAN_POINT ( 'NONE',  ( 0.8753041380234471980, 46.87455897190349674, -14.62580080072613242 ) ) ;
#46386 = CARTESIAN_POINT ( 'NONE',  ( 0.8751705887134553219, 46.21789262997757675, -13.30665218149314200 ) ) ;
#46387 = CARTESIAN_POINT ( 'NONE',  ( -6.078457390727109555, -1.853383199521488445, -19.16662416163158156 ) ) ;
#46388 = CARTESIAN_POINT ( 'NONE',  ( 4.975610109902397937, 47.45567470742089000, 11.84940273605495520 ) ) ;
#46389 = CARTESIAN_POINT ( 'NONE',  ( 0.2940135542859016460, 43.14164472089348834, -9.221661426642361548 ) ) ;
#46390 = FACE_OUTER_BOUND ( 'NONE', #61124, .T. ) ;
#46391 = CIRCLE ( 'NONE', #59367, 15.43999999999999417 ) ;
#46392 = B_SPLINE_CURVE_WITH_KNOTS ( 'NONE', 3,
 ( #177, #47212, #19950, #29021, #4259, #52194 ),
 .UNSPECIFIED., .F., .F.,
 ( 4, 2, 4 ),
 ( 8.551243849294126806E-17, 0.0002293366620881463671, 0.0004586733241762071906 ),
 .UNSPECIFIED. ) ;
#46393 = CARTESIAN_POINT ( 'NONE',  ( 5.895881250540457863, -7.224475463584143498, 18.77057899704672295 ) ) ;
#46394 =( BOUNDED_SURFACE ( )  B_SPLINE_SURFACE ( 3, 1, ( 
 ( #29850, #14847 ),
 ( #52724, #4475 ),
 ( #43678, #9825 ),
 ( #42741, #5408 ) ),
 .UNSPECIFIED., .F., .F., .F. ) 
 B_SPLINE_SURFACE_WITH_KNOTS ( ( 4, 4 ),
 ( 2, 2 ),
 ( 0.000000000000000000, 1.000000000000000000 ),
 ( 0.000000000000000000, 1.000000000000000000 ),
 .UNSPECIFIED. ) 
 GEOMETRIC_REPRESENTATION_ITEM ( )  RATIONAL_B_SPLINE_SURFACE ( (
 ( 1.000000000000000000, 1.000000000000000000),
 ( 0.9953040768229013402, 0.8617119497784988535),
 ( 0.9953040768229013402, 0.8617119497784988535),
 ( 1.000000000000000000, 1.000000000000000000) ) ) 
 REPRESENTATION_ITEM ( '' )  SURFACE ( )  );
#46395 = CARTESIAN_POINT ( 'NONE',  ( 0.3622758884714600280, 33.69533458712307095, 26.89560658783397074 ) ) ;
#46396 = CARTESIAN_POINT ( 'NONE',  ( 4.549368137175248350, -2.596185425821630588, -42.84816078363929392 ) ) ;
#46397 = VERTEX_POINT ( 'NONE', #57791 ) ;
#46398 = CARTESIAN_POINT ( 'NONE',  ( 0.7948878604505671408, 46.31693282836004499, -16.29234116606942706 ) ) ;
#46399 = CARTESIAN_POINT ( 'NONE',  ( 0.9762797500689124330, 20.58271139965489738, 36.50584578699993443 ) ) ;
#46400 = CARTESIAN_POINT ( 'NONE',  ( 0.7246131072078559887, -38.65593150731067595, 28.62741613354226544 ) ) ;
#46401 = CARTESIAN_POINT ( 'NONE',  ( 0.7764146366350267447, -45.77880931614775051, 10.21474871276577012 ) ) ;
#46402 = ORIENTED_EDGE ( 'NONE', *, *, #60357, .T. ) ;
#46403 = EDGE_CURVE ( 'NONE', #45625, #46967, #32252, .T. ) ;
#46404 = CARTESIAN_POINT ( 'NONE',  ( -6.001507490154110336, 4.892199142591303840, 18.19774963328910289 ) ) ;
#46405 = CARTESIAN_POINT ( 'NONE',  ( 0.6016118706126976079, 44.39439472474408177, -20.99258849707547725 ) ) ;
#46406 = ADVANCED_FACE ( 'NONE', ( #10207 ), #45782, .F. ) ;
#46407 =( BOUNDED_SURFACE ( )  B_SPLINE_SURFACE ( 3, 1, ( 
 ( #56368, #46385 ),
 ( #3431, #32277 ),
 ( #61367, #4344 ),
 ( #27263, #17563 ) ),
 .UNSPECIFIED., .F., .F., .F. ) 
 B_SPLINE_SURFACE_WITH_KNOTS ( ( 4, 4 ),
 ( 2, 2 ),
 ( 0.000000000000000000, 1.000000000000000000 ),
 ( 0.000000000000000000, 1.000000000000000000 ),
 .UNSPECIFIED. ) 
 GEOMETRIC_REPRESENTATION_ITEM ( )  RATIONAL_B_SPLINE_SURFACE ( (
 ( 1.000000000000000000, 1.000000000000000000),
 ( 0.7211978278499970862, 0.9934217856018976445),
 ( 0.7211978278499970862, 0.9934217856018976445),
 ( 1.000000000000000000, 1.000000000000000000) ) ) 
 REPRESENTATION_ITEM ( '' )  SURFACE ( )  );
#46408 = VERTEX_POINT ( 'NONE', #49031 ) ;
#46409 = LINE ( 'NONE', #18506, #15039 ) ;
#46410 = EDGE_CURVE ( 'NONE', #55732, #13148, #36820, .T. ) ;
#46411 = CARTESIAN_POINT ( 'NONE',  ( 4.962356264823608143, 0.000000000000000000, 0.000000000000000000 ) ) ;
#46412 = VERTEX_POINT ( 'NONE', #34330 ) ;
#46413 = CARTESIAN_POINT ( 'NONE',  ( 0.6017666602106489515, 29.56224131406219158, 37.95277954208646065 ) ) ;
#46414 = B_SPLINE_CURVE_WITH_KNOTS ( 'NONE', 3,
 ( #25034, #1207, #53214, #24410, #57904, #49447 ),
 .UNSPECIFIED., .F., .F.,
 ( 4, 2, 4 ),
 ( 2.949348774913697507E-18, 0.0002447193893791696538, 0.0004894387787583363804 ),
 .UNSPECIFIED. ) ;
#46415 = EDGE_LOOP ( 'NONE', ( #29908, #50551, #14618, #55802 ) ) ;
#46416 = ADVANCED_FACE ( 'NONE', ( #1094 ), #52888, .F. ) ;
#46417 = ORIENTED_EDGE ( 'NONE', *, *, #10726, .F. ) ;
#46418 = CARTESIAN_POINT ( 'NONE',  ( 0.1313383488274124378, -42.83318330237621296, -4.995828979989310525 ) ) ;
#46419 = ORIENTED_EDGE ( 'NONE', *, *, #18216, .F. ) ;
#46420 = CARTESIAN_POINT ( 'NONE',  ( 5.917102823773431552, -13.98784315367467812, 14.45095020958616416 ) ) ;
#46421 = B_SPLINE_CURVE_WITH_KNOTS ( 'NONE', 3,
 ( #27046, #12971, #55222, #12346, #50533, #26735 ),
 .UNSPECIFIED., .F., .F.,
 ( 4, 2, 4 ),
 ( 1.268664800107929448E-16, 0.0002450741128632364079, 0.0004901482257263459642 ),
 .UNSPECIFIED. ) ;
#46422 = VECTOR ( 'NONE', #10156, 1000.000000000000114 ) ;
#46423 = ORIENTED_EDGE ( 'NONE', *, *, #21369, .T. ) ;
#46424 = CARTESIAN_POINT ( 'NONE',  ( 5.901463166500145796, -7.215136289071087283, -18.77390952014966530 ) ) ;
#46425 = CARTESIAN_POINT ( 'NONE',  ( 0.9757892942422817795, 16.46777583825603486, 39.62259979733185133 ) ) ;
#46426 = ORIENTED_EDGE ( 'NONE', *, *, #48210, .T. ) ;
#46427 = CARTESIAN_POINT ( 'NONE',  ( 0.1156495703730067576, 15.36680576975396306, 41.36186932025348995 ) ) ;
#46428 = EDGE_CURVE ( 'NONE', #8350, #36635, #40808, .T. ) ;
#46429 = CARTESIAN_POINT ( 'NONE',  ( 5.960721111146673579, -19.82781442290494311, -5.306302591836510985 ) ) ;
#46430 = CARTESIAN_POINT ( 'NONE',  ( 4.691466044806103852, -29.14742760351135331, 33.74235639413277710 ) ) ;
#46431 = CARTESIAN_POINT ( 'NONE',  ( 0.5824936645240088584, -30.55462678129038068, 35.57601665864742557 ) ) ;
#46432 = ORIENTED_EDGE ( 'NONE', *, *, #29380, .T. ) ;
#46433 = CARTESIAN_POINT ( 'NONE',  ( 1.231276596079887264, -34.07446381689716475, 24.41736444846234733 ) ) ;
#46434 = ADVANCED_FACE ( 'NONE', ( #33719 ), #35723, .F. ) ;
#46435 = AXIS2_PLACEMENT_3D ( 'NONE', #58644, #15771, #28928 ) ;
#46436 = ORIENTED_EDGE ( 'NONE', *, *, #52932, .T. ) ;
#46437 = CARTESIAN_POINT ( 'NONE',  ( 0.9752570700956786354, -42.90785210525872628, -0.2306661201225728430 ) ) ;
#46438 = ORIENTED_EDGE ( 'NONE', *, *, #33336, .F. ) ;
#46439 = CARTESIAN_POINT ( 'NONE',  ( 0.1129192098497455998, -13.01845098534629486, 42.16007260106758281 ) ) ;
#46440 = B_SPLINE_CURVE_WITH_KNOTS ( 'NONE', 3,
 ( #34289, #9233, #53367, #47461 ),
 .UNSPECIFIED., .F., .F.,
 ( 4, 4 ),
 ( 0.000000000000000000, 0.004445488388166992516 ),
 .UNSPECIFIED. ) ;
#46441 = CARTESIAN_POINT ( 'NONE',  ( 0.5817216825391131607, 10.42801594297066892, -45.72189230227252921 ) ) ;
#46442 = ORIENTED_EDGE ( 'NONE', *, *, #36389, .F. ) ;
#46443 = CARTESIAN_POINT ( 'NONE',  ( -2.708315649062916552, 14.06540004355482587, -4.041664582652659377 ) ) ;
#46444 = CARTESIAN_POINT ( 'NONE',  ( 43.00000000000000000, 0.000000000000000000, 0.000000000000000000 ) ) ;
#46445 = CARTESIAN_POINT ( 'NONE',  ( 0.7056555295713347054, 24.67549844185537467, 41.05687446835445087 ) ) ;
#46446 = CARTESIAN_POINT ( 'NONE',  ( -6.078726893082806448, -18.27610589745697567, 6.064486333866907053 ) ) ;
#46447 = VERTEX_POINT ( 'NONE', #49639 ) ;
#46448 = ORIENTED_EDGE ( 'NONE', *, *, #46886, .F. ) ;
#46449 = CARTESIAN_POINT ( 'NONE',  ( 4.694002226626921015, -20.78018001817150306, -40.57670378257112276 ) ) ;
#46450 = CARTESIAN_POINT ( 'NONE',  ( 0.5786265663353153954, -41.11783955080255737, 24.57327059187383611 ) ) ;
#46451 = CARTESIAN_POINT ( 'NONE',  ( 0.8557997880470697982, -13.27832040216607190, -46.03118133706039572 ) ) ;
#46452 = FACE_OUTER_BOUND ( 'NONE', #52400, .T. ) ;
#46453 = CARTESIAN_POINT ( 'NONE',  ( 5.895596859100789899, 20.06773179721815126, -1.346968346846738385 ) ) ;
#46454 = LINE ( 'NONE', #38600, #56836 ) ;
#46455 = EDGE_CURVE ( 'NONE', #17061, #58789, #24035, .T. ) ;
#46456 = FACE_OUTER_BOUND ( 'NONE', #38239, .T. ) ;
#46457 = CARTESIAN_POINT ( 'NONE',  ( 0.5839880159502354173, -46.27569712847338224, 12.35255585954166335 ) ) ;
#46458 = CARTESIAN_POINT ( 'NONE',  ( 3.407937589446174087, 13.63405474014710350, -1.331713209622366501 ) ) ;
#46459 = DIRECTION ( 'NONE',  ( 0.07500201931887538753, 0.04681388819016350789, -0.9960839106072389981 ) ) ;
#46460 = CARTESIAN_POINT ( 'NONE',  ( 0.8751705887134553219, 48.08707113907595243, -0.8911681664083408450 ) ) ;
#46461 = CARTESIAN_POINT ( 'NONE',  ( 6.999999999999991118, 80.00000000000001421, -2.649999999999992806 ) ) ;
#46462 = CARTESIAN_POINT ( 'NONE',  ( -6.015611763856276717, -7.216738110653404981, 17.40650793417841413 ) ) ;
#46463 = CIRCLE ( 'NONE', #54426, 43.08621763946400307 ) ;
#46464 = DIRECTION ( 'NONE',  ( -1.000000000000000000, -0.000000000000000000, -0.000000000000000000 ) ) ;
#46465 = FACE_OUTER_BOUND ( 'NONE', #32572, .T. ) ;
#46466 = CARTESIAN_POINT ( 'NONE',  ( 3.894904216938898323, -20.85496616184445173, 38.69360048980352929 ) ) ;
#46467 = CARTESIAN_POINT ( 'NONE',  ( 0.9756950546413942771, -37.20808764646322686, -21.37039651692535358 ) ) ;
#46468 = AXIS2_PLACEMENT_3D ( 'NONE', #58407, #32251, #8735 ) ;
#46469 = CARTESIAN_POINT ( 'NONE',  ( 1.227938101723756947, 11.92353943227949387, 41.23019537246713639 ) ) ;
#46471 = ORIENTED_EDGE ( 'NONE', *, *, #5521, .F. ) ;
#46470 = CARTESIAN_POINT ( 'NONE',  ( 0.9752132459055872227, 39.73079175141347008, 16.20487516111966997 ) ) ;
#46472 = ORIENTED_EDGE ( 'NONE', *, *, #32433, .T. ) ;
#46473 = DIRECTION ( 'NONE',  ( -1.000000000000000000, -0.000000000000000000, -0.000000000000000000 ) ) ;
#46474 = CARTESIAN_POINT ( 'NONE',  ( 3.407937589446178528, -1.331713209622598315, 13.63405474014708041 ) ) ;
#46475 = CARTESIAN_POINT ( 'NONE',  ( 5.901463166500146684, -2.027578129542785046, -20.01016734735710756 ) ) ;
#46476 = ORIENTED_EDGE ( 'NONE', *, *, #46704, .T. ) ;
#46477 = EDGE_LOOP ( 'NONE', ( #6202, #39408, #10522, #12837 ) ) ;
#46478 = CYLINDRICAL_SURFACE ( 'NONE', #42334, 2.649999999999997691 ) ;
#46479 = CIRCLE ( 'NONE', #53460, 6.728125000000023448 ) ;
#46480 = CARTESIAN_POINT ( 'NONE',  ( 0.7948878604505664747, 5.577371006631278050, 48.78105759362752991 ) ) ;
#46481 = ORIENTED_EDGE ( 'NONE', *, *, #4928, .T. ) ;
#46482 = VERTEX_POINT ( 'NONE', #30221 ) ;
#46483 = EDGE_CURVE ( 'NONE', #12277, #24298, #16145, .T. ) ;
#46484 =( BOUNDED_SURFACE ( )  B_SPLINE_SURFACE ( 3, 1, ( 
 ( #9552, #4830 ),
 ( #53379, #33694 ),
 ( #15195, #29274 ),
 ( #28662, #57146 ) ),
 .UNSPECIFIED., .F., .F., .F. ) 
 B_SPLINE_SURFACE_WITH_KNOTS ( ( 4, 4 ),
 ( 2, 2 ),
 ( 0.000000000000000000, 1.000000000000000000 ),
 ( 0.000000000000000000, 1.000000000000000000 ),
 .UNSPECIFIED. ) 
 GEOMETRIC_REPRESENTATION_ITEM ( )  RATIONAL_B_SPLINE_SURFACE ( (
 ( 1.000000000000000000, 1.000000000000000000),
 ( 0.9953040768229005630, 0.8617119497784937465),
 ( 0.9953040768229005630, 0.8617119497784937465),
 ( 1.000000000000000000, 1.000000000000000000) ) ) 
 REPRESENTATION_ITEM ( '' )  SURFACE ( )  );
#46485 = DIRECTION ( 'NONE',  ( 1.000000000000000000, 1.836909530733573776E-16, -1.925929944387235579E-32 ) ) ;
#46486 = DIRECTION ( 'NONE',  ( -1.000000000000000000, -0.000000000000000000, -0.000000000000000000 ) ) ;
#46487 = ORIENTED_EDGE ( 'NONE', *, *, #34391, .F. ) ;
#46488 = ADVANCED_FACE ( 'NONE', ( #25526 ), #44662, .F. ) ;
#46489 = ORIENTED_EDGE ( 'NONE', *, *, #17549, .F. ) ;
#46490 = CARTESIAN_POINT ( 'NONE',  ( 2.301529144917016101, 25.12312032040453147, 40.93948199333342330 ) ) ;
#46491 = CARTESIAN_POINT ( 'NONE',  ( 3.678748215320120973, -31.95975617982332295, -37.11046751559092627 ) ) ;
#46492 = AXIS2_PLACEMENT_3D ( 'NONE', #44403, #16179, #1430 ) ;
#46493 = CARTESIAN_POINT ( 'NONE',  ( 58.00000000000000000, 8.437969416220405915E-15, -2.995852231480068572E-16 ) ) ;
#46494 = ORIENTED_EDGE ( 'NONE', *, *, #2477, .T. ) ;
#46495 = EDGE_LOOP ( 'NONE', ( #27904, #15617, #19007, #35482 ) ) ;
#46496 = CARTESIAN_POINT ( 'NONE',  ( 0.5807400328401637335, -41.20655774452951903, -24.41979442053213489 ) ) ;
#46497 = VERTEX_POINT ( 'NONE', #45282 ) ;
#46498 = CARTESIAN_POINT ( 'NONE',  ( 0.5806925824938499181, -44.47729014209976128, 14.86583411581871772 ) ) ;
#46499 = CARTESIAN_POINT ( 'NONE',  ( 0.6064782688330843108, -20.38304199076106471, 42.23583840320495852 ) ) ;
#46500 = CARTESIAN_POINT ( 'NONE',  ( 0.8751705887134423323, 33.37254303619506857, 34.63284514348596588 ) ) ;
#46501 = CARTESIAN_POINT ( 'NONE',  ( -2.708315649062910779, -10.16016146078282034, -10.53288422393052315 ) ) ;
#46502 =( BOUNDED_SURFACE ( )  B_SPLINE_SURFACE ( 3, 1, ( 
 ( #56257, #4860 ),
 ( #23992, #47499 ),
 ( #33409, #27453 ),
 ( #43122, #158 ) ),
 .UNSPECIFIED., .F., .F., .F. ) 
 B_SPLINE_SURFACE_WITH_KNOTS ( ( 4, 4 ),
 ( 2, 2 ),
 ( 0.000000000000000000, 1.000000000000000000 ),
 ( 0.000000000000000000, 1.000000000000000000 ),
 .UNSPECIFIED. ) 
 GEOMETRIC_REPRESENTATION_ITEM ( )  RATIONAL_B_SPLINE_SURFACE ( (
 ( 1.000000000000000000, 1.000000000000000000),
 ( 0.9953040768229005630, 0.8617119497784937465),
 ( 0.9953040768229005630, 0.8617119497784937465),
 ( 1.000000000000000000, 1.000000000000000000) ) ) 
 REPRESENTATION_ITEM ( '' )  SURFACE ( )  );
#46503 = EDGE_CURVE ( 'NONE', #43179, #52266, #44977, .T. ) ;
#46504 = ORIENTED_EDGE ( 'NONE', *, *, #52475, .F. ) ;
#46505 = CARTESIAN_POINT ( 'NONE',  ( 0.7764139734771242640, 16.02283686154742881, 44.08298050058667172 ) ) ;
#46506 = CARTESIAN_POINT ( 'NONE',  ( 0.5998501479064708430, 24.50586714782604858, -41.39809967730462859 ) ) ;
#46507 = B_SPLINE_CURVE_WITH_KNOTS ( 'NONE', 3,
 ( #57947, #43911, #15072, #25690 ),
 .UNSPECIFIED., .F., .F.,
 ( 4, 4 ),
 ( 0.000000000000000000, 0.005014147105413702989 ),
 .UNSPECIFIED. ) ;
#46508 = CARTESIAN_POINT ( 'NONE',  ( 0.1103744047535531458, 39.85659247569260089, -16.46720136312940852 ) ) ;
#46509 = EDGE_LOOP ( 'NONE', ( #24933, #59799, #48949, #33517 ) ) ;
#46510 = CARTESIAN_POINT ( 'NONE',  ( 0.3622758884714730732, 42.84426538328725798, 4.808133778522027058 ) ) ;
#46511 = CARTESIAN_POINT ( 'NONE',  ( 1.088313998177380615, -26.73848503423878498, 33.56520876252056240 ) ) ;
#46512 = DIRECTION ( 'NONE',  ( -0.1011922191286467598, 0.1460712814909170820, 0.9840850143719399590 ) ) ;
#46513 = CARTESIAN_POINT ( 'NONE',  ( 0.6253024248130486518, -24.86663011560634118, -42.34495169570114825 ) ) ;
#46515 = VERTEX_POINT ( 'NONE', #21141 ) ;
#46514 = CIRCLE ( 'NONE', #27493, 1.000000000000000666 ) ;
#46516 = CARTESIAN_POINT ( 'NONE',  ( 0.8753041380234471980, -45.17330286263774752, -19.24866323549208502 ) ) ;
#46517 = CARTESIAN_POINT ( 'NONE',  ( 4.549368137175248350, -28.46244473166650479, -32.13400537129916046 ) ) ;
#46518 = CARTESIAN_POINT ( 'NONE',  ( 0.6000166863083090663, -2.096232480232020912, 49.06556115135416007 ) ) ;
#46519 = CIRCLE ( 'NONE', #27498, 2.649999999999997691 ) ;
#46520 = B_SPLINE_CURVE_WITH_KNOTS ( 'NONE', 3,
 ( #33623, #43340, #8554, #5988 ),
 .UNSPECIFIED., .F., .F.,
 ( 4, 4 ),
 ( 4.336808689942017736E-18, 0.004566006591234645501 ),
 .UNSPECIFIED. ) ;
#46521 = DIRECTION ( 'NONE',  ( 0.000000000000000000, 0.000000000000000000, -1.000000000000000000 ) ) ;
#46522 = CARTESIAN_POINT ( 'NONE',  ( 7.999999999999996447, 1.469527624586858429E-15, -1.540743955509788245E-31 ) ) ;
#46523 = CARTESIAN_POINT ( 'NONE',  ( 0.8560838555295223751, 40.81790744942443183, 23.11430867518979326 ) ) ;
#46524 = CARTESIAN_POINT ( 'NONE',  ( 0.3676999524040323597, 36.51379593394458567, 24.75264207750540635 ) ) ;
#46525 = CARTESIAN_POINT ( 'NONE',  ( 0.8554163680231816613, -6.900908941297196009, 46.40671211038057464 ) ) ;
#46526 = CARTESIAN_POINT ( 'NONE',  ( 0.9762797500689124330, 41.90547441298052433, 0.5059638413352746111 ) ) ;
#46527 = CARTESIAN_POINT ( 'NONE',  ( 0.8560838555295158248, 11.76118766017326323, -45.40977096290972526 ) ) ;
#46528 = ORIENTED_EDGE ( 'NONE', *, *, #52039, .T. ) ;
#46529 = EDGE_CURVE ( 'NONE', #462, #60714, #11389, .T. ) ;
#46530 = CARTESIAN_POINT ( 'NONE',  ( -16.39102408640302500, -12.42318157589703631, -1.387175274418403825 ) ) ;
#46531 = CARTESIAN_POINT ( 'NONE',  ( -5.995132425357893702, -18.68182899165009658, -2.468096378288315851 ) ) ;
#46532 = CARTESIAN_POINT ( 'NONE',  ( 0.5998501479064708430, -33.64490850298820845, -34.38546660123286358 ) ) ;
#46533 = CARTESIAN_POINT ( 'NONE',  ( 0.6029443199889047422, -39.35536131004970883, -29.37163900789067839 ) ) ;
#46534 = B_SPLINE_CURVE_WITH_KNOTS ( 'NONE', 3,
 ( #32360, #61750, #42089, #28259, #51748, #37374 ),
 .UNSPECIFIED., .F., .F.,
 ( 4, 2, 4 ),
 ( 1.736890526760486189E-17, 0.0002293755540694303698, 0.0004587511081388433382 ),
 .UNSPECIFIED. ) ;
#46535 = CARTESIAN_POINT ( 'NONE',  ( 4.956445790443993360, 20.31112743693043399, 42.48524629068788983 ) ) ;
#46536 = FACE_OUTER_BOUND ( 'NONE', #25073, .T. ) ;
#46537 = EDGE_CURVE ( 'NONE', #3027, #30298, #15743, .T. ) ;
#46538 = SHAPE_DEFINITION_REPRESENTATION ( #19921, #27649 ) ;
#46539 = CARTESIAN_POINT ( 'NONE',  ( 4.549368137175248350, 0.000000000000000000, 0.000000000000000000 ) ) ;
#46540 = B_SPLINE_CURVE_WITH_KNOTS ( 'NONE', 3,
 ( #31120, #45550, #17041, #22042, #41167, #17340 ),
 .UNSPECIFIED., .F., .F.,
 ( 4, 2, 4 ),
 ( 4.872882708070265673E-18, 0.0002291472222819940739, 0.0004582944445639832690 ),
 .UNSPECIFIED. ) ;
#46541 = CIRCLE ( 'NONE', #20325, 0.09999999999999939493 ) ;
#46542 = CARTESIAN_POINT ( 'NONE',  ( 0.5806925824938511393, 10.33919002968708689, -45.74192291403568333 ) ) ;
#46543 = EDGE_CURVE ( 'NONE', #23728, #24263, #1710, .T. ) ;
#46544 = CARTESIAN_POINT ( 'NONE',  ( 0.6028777368367060907, -1.660990723866983432, 49.07933311615287408 ) ) ;
#46546 = EDGE_LOOP ( 'NONE', ( #18571, #16665, #11769, #49629 ) ) ;
#46545 = CARTESIAN_POINT ( 'NONE',  ( 0.3622758884714730732, -6.444611261694294768, -42.62881903538208661 ) ) ;
#46547 = ORIENTED_EDGE ( 'NONE', *, *, #54153, .F. ) ;
#46548 = LINE ( 'NONE', #4823, #15875 ) ;
#46549 = DIRECTION ( 'NONE',  ( 0.000000000000000000, 0.000000000000000000, 1.000000000000000000 ) ) ;
#46550 = CARTESIAN_POINT ( 'NONE',  ( 0.5998501479064699549, 47.62484632993687939, -6.798102206413639159 ) ) ;
#46551 = ORIENTED_EDGE ( 'NONE', *, *, #20503, .T. ) ;
#46552 = CARTESIAN_POINT ( 'NONE',  ( 0.5817216825391118284, 22.93558720760018943, 40.90469156038248144 ) ) ;
#46553 = CARTESIAN_POINT ( 'NONE',  ( 0.5837157313716020424, -45.97435446094988265, 9.251799580674125778 ) ) ;
#46554 = LINE ( 'NONE', #8617, #57910 ) ;
#46555 = ORIENTED_EDGE ( 'NONE', *, *, #32774, .F. ) ;
#46556 = ORIENTED_EDGE ( 'NONE', *, *, #2157, .T. ) ;
#46557 = CIRCLE ( 'NONE', #29535, 2.649999999999992806 ) ;
#46558 = CARTESIAN_POINT ( 'NONE',  ( 0.9790850452238870627, 24.81859480363789672, -33.76943414148414746 ) ) ;
#46559 = EDGE_CURVE ( 'NONE', #31240, #5597, #21818, .T. ) ;
#46561 = CARTESIAN_POINT ( 'NONE',  ( 0.5980894510889448457, 46.28687279963673973, 13.12879507229304288 ) ) ;
#46560 = AXIS2_PLACEMENT_3D ( 'NONE', #10651, #5596, #57922 ) ;
#46562 = CARTESIAN_POINT ( 'NONE',  ( 0.9791128995231611620, 32.88674391329360702, -25.97690337641515157 ) ) ;
#46563 = EDGE_CURVE ( 'NONE', #18906, #17743, #5363, .T. ) ;
#46565 = CARTESIAN_POINT ( 'NONE',  ( 0.8744876279028263033, -0.6840263623742536270, -49.09055060105834656 ) ) ;
#46564 = CIRCLE ( 'NONE', #35569, 43.92652462719577500 ) ;
#46566 = CARTESIAN_POINT ( 'NONE',  ( 0.5997462898726536595, 49.03735788587799505, 2.624721264559015221 ) ) ;
#46567 = ADVANCED_FACE ( 'NONE', ( #32097 ), #55561, .F. ) ;
#46568 = CARTESIAN_POINT ( 'NONE',  ( 0.3622758884714600280, 11.95365414648497193, -41.42293301073613776 ) ) ;
#46569 = ORIENTED_EDGE ( 'NONE', *, *, #52231, .F. ) ;
#46570 = CARTESIAN_POINT ( 'NONE',  ( 4.975610109902397937, 47.45567470742105343, -11.84940273605426242 ) ) ;
#46571 = FILL_AREA_STYLE ('',( #51860 ) ) ;
#46572 = B_SPLINE_CURVE_WITH_KNOTS ( 'NONE', 3,
 ( #15134, #33628, #34242, #4766 ),
 .UNSPECIFIED., .F., .F.,
 ( 4, 4 ),
 ( 0.000000000000000000, 0.004444103432399266161 ),
 .UNSPECIFIED. ) ;
#46573 = ORIENTED_EDGE ( 'NONE', *, *, #47536, .T. ) ;
#46574 = CARTESIAN_POINT ( 'NONE',  ( 0.6009453534118438522, -47.63713118507423161, -6.711694149738057114 ) ) ;
#46575 = CARTESIAN_POINT ( 'NONE',  ( -6.077587904424778920, 16.77513308702641837, -9.454677747363051665 ) ) ;
#46576 = CARTESIAN_POINT ( 'NONE',  ( 4.390527457369402420, 38.43681538245588314, -21.27901689184964340 ) ) ;
#46577 = CARTESIAN_POINT ( 'NONE',  ( 4.553261556744873317, 38.16266689001211887, -21.75202109381124771 ) ) ;
#46578 = EDGE_CURVE ( 'NONE', #48340, #19272, #42037, .T. ) ;
#46579 = ORIENTED_EDGE ( 'NONE', *, *, #14513, .F. ) ;
#46580 = EDGE_LOOP ( 'NONE', ( #13310, #40898, #26846, #15698 ) ) ;
#46581 = CARTESIAN_POINT ( 'NONE',  ( 1.091591847532199511, -31.60342101358676459, 27.53148690488443862 ) ) ;
#46582 = DIRECTION ( 'NONE',  ( 0.1011922191286468015, 0.9919158664526106506, -0.07657054699678347842 ) ) ;
#46583 = ORIENTED_EDGE ( 'NONE', *, *, #35331, .T. ) ;
#46584 = CARTESIAN_POINT ( 'NONE',  ( 0.6041374136657476912, 6.452348380035281217, 47.67304777898701218 ) ) ;
#46585 =( BOUNDED_SURFACE ( )  B_SPLINE_SURFACE ( 3, 1, ( 
 ( #32653, #56432 ),
 ( #52045, #13546 ),
 ( #38293, #23246 ),
 ( #28243, #334 ) ),
 .UNSPECIFIED., .F., .F., .F. ) 
 B_SPLINE_SURFACE_WITH_KNOTS ( ( 4, 4 ),
 ( 2, 2 ),
 ( 0.000000000000000000, 1.000000000000000000 ),
 ( 0.000000000000000000, 1.000000000000000000 ),
 .UNSPECIFIED. ) 
 GEOMETRIC_REPRESENTATION_ITEM ( )  RATIONAL_B_SPLINE_SURFACE ( (
 ( 1.000000000000000000, 1.000000000000000000),
 ( 0.7223157951917476005, 0.9931996967497186413),
 ( 0.7223157951917476005, 0.9931996967497186413),
 ( 1.000000000000000000, 1.000000000000000000) ) ) 
 REPRESENTATION_ITEM ( '' )  SURFACE ( )  );
#46586 = ORIENTED_EDGE ( 'NONE', *, *, #22838, .T. ) ;
#46587 = CARTESIAN_POINT ( 'NONE',  ( -6.016761891674565099, 13.32657647165373760, -13.32172022638577680 ) ) ;
#46588 = ORIENTED_EDGE ( 'NONE', *, *, #33951, .F. ) ;
#46589 = CARTESIAN_POINT ( 'NONE',  ( 0.6041374136657476912, -0.1745662470641466957, -48.10739871142803992 ) ) ;
#46590 = DIRECTION ( 'NONE',  ( -1.000000000000000000, -5.380183451256670742E-17, 1.298891185607911324E-16 ) ) ;
#46591 = CARTESIAN_POINT ( 'NONE',  ( 0.6026112563231248442, -13.80537458850877641, -47.12698406831444942 ) ) ;
#46592 = VERTEX_POINT ( 'NONE', #4171 ) ;
#46593 = CARTESIAN_POINT ( 'NONE',  ( 0.5997462898726536595, -8.352924653000044941, -48.39194436975655123 ) ) ;
#46594 = CARTESIAN_POINT ( 'NONE',  ( 0.1157991065609915715, -27.57457289024313951, 34.44684739505731841 ) ) ;
#46595 = CARTESIAN_POINT ( 'NONE',  ( 1.000110580585049203, 29.60461236713370070, -29.66453116709677573 ) ) ;
#46596 = ORIENTED_EDGE ( 'NONE', *, *, #26880, .F. ) ;
#46597 = CARTESIAN_POINT ( 'NONE',  ( -19.55451506711360210, -12.42295183846419704, -1.389156475119130318 ) ) ;
#46598 = FACE_OUTER_BOUND ( 'NONE', #60864, .T. ) ;
#46599 = CARTESIAN_POINT ( 'NONE',  ( 0.8557997880470599172, -7.156447707086029730, 47.37054680076704472 ) ) ;
#46600 = CARTESIAN_POINT ( 'NONE',  ( 0.6030672727741701600, 47.70721108823349255, -6.192762795893955285 ) ) ;
#46601 = B_SPLINE_CURVE_WITH_KNOTS ( 'NONE', 3,
 ( #31856, #46576, #22754, #8639, #17752, #56566, #13680, #27764, #32163, #9265, #41888, #8327, #60956, #52172, #22141, #61256, #22446, #41571, #42500, #18065, #46894, #56253, #41268, #45971, #60326 ),
 .UNSPECIFIED., .F., .F.,
 ( 4, 3, 3, 3, 3, 3, 3, 3, 4 ),
 ( 6.254634441385502288E-18, 0.0005656085177311393148, 0.001131215744874500056, 0.001696821861372765266, 0.002262427090022498585, 0.002828031679238745058, 0.003393635864401605296, 0.003977030878808130755, 0.004561030005651158133 ),
 .UNSPECIFIED. ) ;
#46603 = CONICAL_SURFACE ( 'NONE', #28470, 43.92652462719577500, 1.486293639869522343 ) ;
#46602 = CARTESIAN_POINT ( 'NONE',  ( 0.7762783648524399505, 23.17763242108814481, -41.92424098267915866 ) ) ;
#46604 = ORIENTED_EDGE ( 'NONE', *, *, #50835, .T. ) ;
#46605 = CARTESIAN_POINT ( 'NONE',  ( 1.231276596079887264, -13.22565419921979313, -39.77887431816952102 ) ) ;
#46606 = EDGE_CURVE ( 'NONE', #10512, #36411, #39825, .T. ) ;
#46607 = CARTESIAN_POINT ( 'NONE',  ( 4.975610109902397937, 14.46773809681615575, -46.72401910687593585 ) ) ;
#46608 = VERTEX_POINT ( 'NONE', #42138 ) ;
#46609 = CIRCLE ( 'NONE', #61592, 0.2800000000000007483 ) ;
#46610 = ADVANCED_FACE ( 'NONE', ( #8261 ), #36810, .F. ) ;
#46611 = DIRECTION ( 'NONE',  ( 0.000000000000000000, 0.000000000000000000, -1.000000000000000000 ) ) ;
#46612 = CARTESIAN_POINT ( 'NONE',  ( 1.227938101723748288, 42.91134962331487657, 0.8460948827226649760 ) ) ;
#46613 = CARTESIAN_POINT ( 'NONE',  ( 4.291220156522059348, -33.45801620160708012, -33.16549636532965195 ) ) ;
#46614 = CIRCLE ( 'NONE', #55558, 42.92674063221959813 ) ;
#46615 = CARTESIAN_POINT ( 'NONE',  ( 0.2885697896453121025, -11.93479333319053559, 41.43179225254745290 ) ) ;
#46616 = DIRECTION ( 'NONE',  ( 0.07439287786467665975, -0.1170659376278835873, -0.9903339163990677596 ) ) ;
#46617 = CARTESIAN_POINT ( 'NONE',  ( 42.00000000000000711, 0.000000000000000000, 0.000000000000000000 ) ) ;
#46618 = CARTESIAN_POINT ( 'NONE',  ( 0.6016118706126977189, 4.368608851477891797, 48.91284403392140234 ) ) ;
#46619 = ADVANCED_FACE ( 'NONE', ( #51177 ), #33703, .F. ) ;
#46620 = CARTESIAN_POINT ( 'NONE',  ( 0.6025881611877910160, 38.03302298778302770, 29.45877655626806657 ) ) ;
#46621 = CARTESIAN_POINT ( 'NONE',  ( 0.8753041380234524160, -8.714053517583520758, -48.32394436680091587 ) ) ;
#46622 = CARTESIAN_POINT ( 'NONE',  ( 4.975610109902397937, -5.269241389990889424, -48.62802178077758697 ) ) ;
#46623 = ADVANCED_FACE ( 'NONE', ( #50565 ), #33338, .F. ) ;
#46624 = EDGE_CURVE ( 'NONE', #60046, #32260, #38257, .T. ) ;
#46625 = CARTESIAN_POINT ( 'NONE',  ( 1.157644175074336035, 8.912044513555821723, 40.95824383524741563 ) ) ;
#46626 = CARTESIAN_POINT ( 'NONE',  ( 3.376099380956842921, -11.75009321188415967, 6.453192476914109577 ) ) ;
#46627 = CARTESIAN_POINT ( 'NONE',  ( 0.6027444965799114707, -1.443419008004065640, -49.08620027517687845 ) ) ;
#46628 = LINE ( 'NONE', #61003, #17782 ) ;
#46629 = DIRECTION ( 'NONE',  ( 1.000000000000000000, -0.000000000000000000, -0.000000000000000000 ) ) ;
#46630 = CARTESIAN_POINT ( 'NONE',  ( -48.95476116535499500, 0.000000000000000000, 0.000000000000000000 ) ) ;
#46631 = CARTESIAN_POINT ( 'NONE',  ( 4.553261556744875094, 31.71129487083167220, -30.39627186743139831 ) ) ;
#46632 = ORIENTED_EDGE ( 'NONE', *, *, #40245, .F. ) ;
#46633 = CARTESIAN_POINT ( 'NONE',  ( 0.9722240741986379886, -29.92651525529354117, -30.74950262511632104 ) ) ;
#46634 = EDGE_CURVE ( 'NONE', #4388, #5237, #16609, .T. ) ;
#46635 = CARTESIAN_POINT ( 'NONE',  ( 4.226256110419178924, -33.18950264439402531, -28.79729439035807559 ) ) ;
#46636 = CARTESIAN_POINT ( 'NONE',  ( 2.879087469061463622, 28.27730024378419671, -33.71195585702882624 ) ) ;
#46637 = CARTESIAN_POINT ( 'NONE',  ( 0.9730545539215892381, -21.89037132892461912, 36.90443313492323085 ) ) ;
#46638 = ORIENTED_EDGE ( 'NONE', *, *, #42320, .F. ) ;
#46639 = CARTESIAN_POINT ( 'NONE',  ( 0.6023143664670691511, 24.28012784216878117, -41.53077189784239209 ) ) ;
#46640 = EDGE_CURVE ( 'NONE', #47578, #9208, #47127, .T. ) ;
#46641 = EDGE_LOOP ( 'NONE', ( #50710, #59540, #40888, #53952 ) ) ;
#46642 = B_SPLINE_CURVE_WITH_KNOTS ( 'NONE', 3,
 ( #32489, #55966, #17774, #13700, #51263, #61274, #36579, #18392, #12782, #18083, #13085, #51565, #37513, #21852, #45671, #60055 ),
 .UNSPECIFIED., .F., .F.,
 ( 4, 3, 3, 3, 3, 4 ),
 ( 9.813676791237319219E-18, 0.0002732102107931869096, 0.0004098135523333678730, 0.0005464168938824852644, 0.0008195847345945424679, 0.001092771384553108951 ),
 .UNSPECIFIED. ) ;
#46643 = CARTESIAN_POINT ( 'NONE',  ( 0.5797568599927116484, 37.19047634640187994, -28.56735510681254553 ) ) ;
#46644 = VERTEX_POINT ( 'NONE', #3867 ) ;
#46645 = CARTESIAN_POINT ( 'NONE',  ( 0.8760168074887076939, 29.98565522133296213, 37.61398439004543803 ) ) ;
#46646 = CARTESIAN_POINT ( 'NONE',  ( 0.1313383488274112720, 22.11173226734840469, 37.02311703718862645 ) ) ;
#46647 = CONICAL_SURFACE ( 'NONE', #21641, 43.92652462719577500, 1.486293639869522343 ) ;
#46648 = VERTEX_POINT ( 'NONE', #23009 ) ;
#46649 = CARTESIAN_POINT ( 'NONE',  ( 5.960721111146673579, -12.50019045452750355, 16.28018152803671370 ) ) ;
#46650 = FACE_OUTER_BOUND ( 'NONE', #61793, .T. ) ;
#46651 = ORIENTED_EDGE ( 'NONE', *, *, #58797, .F. ) ;
#46652 = CARTESIAN_POINT ( 'NONE',  ( 0.5997462898726536595, -45.31995669577361951, 18.91172004968117903 ) ) ;
#46653 = CARTESIAN_POINT ( 'NONE',  ( 0.5804410086790514622, -30.69452151258693817, -35.45935984995687562 ) ) ;
#46654 = EDGE_CURVE ( 'NONE', #23810, #18917, #35252, .T. ) ;
#46655 = ORIENTED_EDGE ( 'NONE', *, *, #38471, .T. ) ;
#46656 = CARTESIAN_POINT ( 'NONE',  ( 3.240649175237395596, 6.040174043042799035, -43.57500676910334647 ) ) ;
#46657 = ORIENTED_EDGE ( 'NONE', *, *, #35792, .T. ) ;
#46658 = CARTESIAN_POINT ( 'NONE',  ( 0.5807400328401574052, 47.41494605191452649, -6.791881299635100788 ) ) ;
#46659 = EDGE_CURVE ( 'NONE', #51385, #59613, #3727, .T. ) ;
#46660 = ORIENTED_EDGE ( 'NONE', *, *, #55667, .F. ) ;
#46661 = ORIENTED_EDGE ( 'NONE', *, *, #16032, .T. ) ;
#46662 = DIRECTION ( 'NONE',  ( -0.1011922191286467460, -0.4487230644346533737, -0.8879232772217393599 ) ) ;
#46664 = CIRCLE ( 'NONE', #17631, 0.2000000000000000944 ) ;
#46663 = CARTESIAN_POINT ( 'NONE',  ( 1.157644175074335813, -7.784786351351509204, 41.18736914325793919 ) ) ;
#46665 = DIRECTION ( 'NONE',  ( 0.09835009131224552170, 0.8656670924898548503, 0.4908642831975393306 ) ) ;
#46666 = CARTESIAN_POINT ( 'NONE',  ( 0.1100053167205930771, -16.33707796615732377, 39.91014771056750021 ) ) ;
#46667 = FACE_OUTER_BOUND ( 'NONE', #45434, .T. ) ;
#46668 = ORIENTED_EDGE ( 'NONE', *, *, #59210, .F. ) ;
#46669 = CARTESIAN_POINT ( 'NONE',  ( 1.834102595619085285, 5.524616319571569178, 43.69984392854519228 ) ) ;
#46670 = FACE_OUTER_BOUND ( 'NONE', #60000, .T. ) ;
#46671 = CARTESIAN_POINT ( 'NONE',  ( 0.6008122571543327295, 46.46679251165622304, -15.88684185557360351 ) ) ;
#46672 = VERTEX_POINT ( 'NONE', #58023 ) ;
#46673 = ORIENTED_EDGE ( 'NONE', *, *, #52133, .T. ) ;
#46674 = CARTESIAN_POINT ( 'NONE',  ( 0.5997462898726536595, 11.43624519451647714, 47.75734421002918140 ) ) ;
#46675 = LINE ( 'NONE', #4026, #40850 ) ;
#46676 = CARTESIAN_POINT ( 'NONE',  ( 1.000110580585049425, 40.24174505028877036, 11.70553023487029698 ) ) ;
#46677 = CARTESIAN_POINT ( 'NONE',  ( 2.299652685299200972, 5.989079187508338009, -48.66634006522278355 ) ) ;
#46678 = DIRECTION ( 'NONE',  ( 0.07500201931887538753, -0.2180102369365475579, -0.9730602415518585513 ) ) ;
#46679 = ORIENTED_EDGE ( 'NONE', *, *, #57624, .F. ) ;
#46680 = CARTESIAN_POINT ( 'NONE',  ( 0.5809828226811617480, 47.41188724015879785, 6.791453954330491705 ) ) ;
#46681 = EDGE_CURVE ( 'NONE', #12966, #43120, #28609, .T. ) ;
#46682 = FACE_OUTER_BOUND ( 'NONE', #22973, .T. ) ;
#46683 = CARTESIAN_POINT ( 'NONE',  ( 0.9775691876210993447, -41.14243135631965487, 7.977095403749041580 ) ) ;
#46684 = FACE_OUTER_BOUND ( 'NONE', #60235, .T. ) ;
#46685 = CARTESIAN_POINT ( 'NONE',  ( 1.479689385636123067, -43.53577155721767866, 6.798561626215384734 ) ) ;
#46686 = EDGE_CURVE ( 'NONE', #16591, #26419, #45762, .T. ) ;
#46687 = SURFACE_STYLE_FILL_AREA ( #42305 ) ;
#46688 = CARTESIAN_POINT ( 'NONE',  ( 58.00000000000000000, 8.437969416220405915E-15, -2.995852231480068572E-16 ) ) ;
#46689 = EDGE_LOOP ( 'NONE', ( #21485, #53782, #56653, #57553 ) ) ;
#46690 = DIRECTION ( 'NONE',  ( -0.07906939808003035641, -0.4269277467251155200, -0.9008222518141286717 ) ) ;
#46691 = CARTESIAN_POINT ( 'NONE',  ( 0.1073791018717483448, 5.147744207006859973, -42.81622261970989030 ) ) ;
#46692 = CIRCLE ( 'NONE', #1658, 2.649999999999997691 ) ;
#46693 = EDGE_CURVE ( 'NONE', #5101, #13508, #33040, .T. ) ;
#46694 = CARTESIAN_POINT ( 'NONE',  ( -2.708315649062916552, -14.06540004355485252, 4.041664582652561677 ) ) ;
#46695 = EDGE_CURVE ( 'NONE', #58067, #38817, #41253, .T. ) ;
#46696 = CARTESIAN_POINT ( 'NONE',  ( 0.1087620492084205442, 21.87505161834417322, -37.16461718700644923 ) ) ;
#46697 = COLOUR_RGB ( '', 0.66274510, 0.83137255, 0.94901961) ;
#46698 = CIRCLE ( 'NONE', #11676, 42.08604991992415023 ) ;
#46699 = ADVANCED_FACE ( 'NONE', ( #43052 ), #49760, .F. ) ;
#46700 = CARTESIAN_POINT ( 'NONE',  ( 5.965394784446460541, -7.841344330024812237, -18.96850062921631874 ) ) ;
#46701 = CARTESIAN_POINT ( 'NONE',  ( 0.6846871229502932144, -44.58493949244016363, 17.53234844287726091 ) ) ;
#46702 = CARTESIAN_POINT ( 'NONE',  ( 2.643462169533600914, 17.09809940585597232, 44.89050350746158102 ) ) ;
#46703 = CARTESIAN_POINT ( 'NONE',  ( 0.7764146366350282991, 37.35658959738729834, 28.36416202396149799 ) ) ;
#46704 = EDGE_CURVE ( 'NONE', #53253, #22549, #50985, .T. ) ;
#46705 =( BOUNDED_SURFACE ( )  B_SPLINE_SURFACE ( 3, 1, ( 
 ( #82, #19534 ),
 ( #51790, #38649 ),
 ( #57703, #14834 ),
 ( #33943, #61483 ) ),
 .UNSPECIFIED., .F., .F., .F. ) 
 B_SPLINE_SURFACE_WITH_KNOTS ( ( 4, 4 ),
 ( 2, 2 ),
 ( 0.000000000000000000, 1.000000000000000000 ),
 ( 0.000000000000000000, 1.000000000000000000 ),
 .UNSPECIFIED. ) 
 GEOMETRIC_REPRESENTATION_ITEM ( )  RATIONAL_B_SPLINE_SURFACE ( (
 ( 1.000000000000000000, 1.000000000000000000),
 ( 0.7223157951917480446, 0.9931996967497186413),
 ( 0.7223157951917480446, 0.9931996967497186413),
 ( 1.000000000000000000, 1.000000000000000000) ) ) 
 REPRESENTATION_ITEM ( '' )  SURFACE ( )  );
#46706 = B_SPLINE_CURVE_WITH_KNOTS ( 'NONE', 3,
 ( #38546, #57598, #14731, #7776, #45107, #50684 ),
 .UNSPECIFIED., .F., .F.,
 ( 4, 2, 4 ),
 ( 0.006456566858647395761, 0.007625406818786647362, 0.008794246778925899830 ),
 .UNSPECIFIED. ) ;
#46707 = FACE_OUTER_BOUND ( 'NONE', #29496, .T. ) ;
#46708 = CIRCLE ( 'NONE', #9661, 48.09070567114147110 ) ;
#46709 = ORIENTED_EDGE ( 'NONE', *, *, #25322, .F. ) ;
#46710 = CARTESIAN_POINT ( 'NONE',  ( 3.660176727303412925, 14.24118031989659094, -45.87883389004754520 ) ) ;
#46711 = CARTESIAN_POINT ( 'NONE',  ( 0.3622758884714600280, 25.58609868863721459, 34.70015533914837391 ) ) ;
#46712 = DIRECTION ( 'NONE',  ( 0.000000000000000000, 0.000000000000000000, 1.000000000000000000 ) ) ;
#46713 = CARTESIAN_POINT ( 'NONE',  ( 0.8560838555295158248, -2.480523550131575661, 46.84250032821661591 ) ) ;
#46714 = VERTEX_POINT ( 'NONE', #38656 ) ;
#46715 = CARTESIAN_POINT ( 'NONE',  ( 0.8753041380234530822, -13.11588273819849704, 47.31925557181565267 ) ) ;
#46716 = CARTESIAN_POINT ( 'NONE',  ( 0.6029443449137436017, 44.26313014289048198, -21.26769493708410508 ) ) ;
#46717 = B_SPLINE_CURVE_WITH_KNOTS ( 'NONE', 3,
 ( #24941, #39361, #49043, #39990 ),
 .UNSPECIFIED., .F., .F.,
 ( 4, 4 ),
 ( 0.000000000000000000, 0.005013413432710147645 ),
 .UNSPECIFIED. ) ;
#46718 = PRESENTATION_STYLE_ASSIGNMENT (( #12897 ) ) ;
#46719 = ORIENTED_EDGE ( 'NONE', *, *, #9820, .T. ) ;
#46720 = CARTESIAN_POINT ( 'NONE',  ( -6.016761891674565099, 18.68153697670641833, 2.462934516563870080 ) ) ;
#46721 = CARTESIAN_POINT ( 'NONE',  ( 0.8760168074886965917, -5.394043284319169018, -47.80016357497247981 ) ) ;
#46722 = ORIENTED_EDGE ( 'NONE', *, *, #9009, .F. ) ;
#46723 = B_SPLINE_CURVE_WITH_KNOTS ( 'NONE', 3,
 ( #17750, #22444, #55320, #22752, #41886, #27143 ),
 .UNSPECIFIED., .F., .F.,
 ( 4, 2, 4 ),
 ( 1.843143693225357538E-18, 0.0002447193893791662386, 0.0004894387787583306341 ),
 .UNSPECIFIED. ) ;
#46724 = CARTESIAN_POINT ( 'NONE',  ( 0.6023142530420679819, 29.49327578399137195, 38.00626667377531476 ) ) ;
#46725 = ORIENTED_EDGE ( 'NONE', *, *, #35882, .T. ) ;
#46726 = ORIENTED_EDGE ( 'NONE', *, *, #4112, .F. ) ;
#46727 = CARTESIAN_POINT ( 'NONE',  ( 0.5839880159502351953, -6.206687493267375011, -47.49213420504722905 ) ) ;
#46728 = ORIENTED_EDGE ( 'NONE', *, *, #41598, .T. ) ;
#46729 = CARTESIAN_POINT ( 'NONE',  ( -6.016761891674565099, 4.873659902332367011, 18.20201388312097279 ) ) ;
#46730 = ORIENTED_EDGE ( 'NONE', *, *, #37947, .T. ) ;
#46731 = CARTESIAN_POINT ( 'NONE',  ( 5.880360259849752858, -43.00389496650600307, -21.25991003419937542 ) ) ;
#46732 = ADVANCED_FACE ( 'NONE', ( #43987 ), #18741, .T. ) ;
#46733 = CARTESIAN_POINT ( 'NONE',  ( 5.895881250540457863, 8.462078741123132630, 18.24612027219301780 ) ) ;
#46734 = CARTESIAN_POINT ( 'NONE',  ( 0.9757787079277444597, 16.38386580718292507, 39.65734351318506867 ) ) ;
#46735 = AXIS2_PLACEMENT_3D ( 'NONE', #58170, #19683, #38807 ) ;
#46736 = EDGE_LOOP ( 'NONE', ( #41364, #61607, #28746, #1683 ) ) ;
#46737 = CARTESIAN_POINT ( 'NONE',  ( 3.407937589446178528, -3.099921468255096624, 13.34359005742688531 ) ) ;
#46738 =( GEOMETRIC_REPRESENTATION_CONTEXT ( 3 ) GLOBAL_UNCERTAINTY_ASSIGNED_CONTEXT ( ( #46799 ) ) GLOBAL_UNIT_ASSIGNED_CONTEXT ( ( #50445, #58904, #49829 ) ) REPRESENTATION_CONTEXT ( 'NONE', 'WORKASPACE' ) );
#46739 = CARTESIAN_POINT ( 'NONE',  ( -6.079354080745853928, -14.66163526140110385, -12.48316493161096830 ) ) ;
#46740 = CARTESIAN_POINT ( 'NONE',  ( 0.5837800304671209028, -44.28628010941674376, -15.42604052405472359 ) ) ;
#46741 = CIRCLE ( 'NONE', #54700, 48.91267123290010943 ) ;
#46742 = CARTESIAN_POINT ( 'NONE',  ( 0.5809828226811556418, -5.711058609465654357, 47.55412398569204413 ) ) ;
#46743 = VERTEX_POINT ( 'NONE', #15145 ) ;
#46744 = DIRECTION ( 'NONE',  ( 0.000000000000000000, 0.000000000000000000, 1.000000000000000000 ) ) ;
#46745 = CARTESIAN_POINT ( 'NONE',  ( 0.1152339509894530906, -31.85158600912513904, -30.53553928062425271 ) ) ;
#46746 = VERTEX_POINT ( 'NONE', #52410 ) ;
#46747 = CARTESIAN_POINT ( 'NONE',  ( 5.974727161628369032, 12.48248968439907003, 16.29297756969652511 ) ) ;
#46748 = ORIENTED_EDGE ( 'NONE', *, *, #55638, .T. ) ;
#46749 = B_SPLINE_CURVE_WITH_KNOTS ( 'NONE', 3,
 ( #56934, #34090, #19066, #29358, #53160, #10267 ),
 .UNSPECIFIED., .F., .F.,
 ( 4, 2, 4 ),
 ( 1.111611290687706433E-17, 0.0002291978881530163769, 0.0004583957763060216408 ),
 .UNSPECIFIED. ) ;
#46750 = CARTESIAN_POINT ( 'NONE',  ( 0.8560838555295223751, -26.00596412780120303, -39.03924517540328765 ) ) ;
#46751 = CARTESIAN_POINT ( 'NONE',  ( 5.960721111146673579, 10.26825948882901152, 17.77250458025995528 ) ) ;
#46752 = ORIENTED_EDGE ( 'NONE', *, *, #14095, .T. ) ;
#46753 = CARTESIAN_POINT ( 'NONE',  ( 5.895596859100789899, -17.30698493747174993, -10.24677781483592121 ) ) ;
#46754 = FACE_OUTER_BOUND ( 'NONE', #44277, .T. ) ;
#46755 = DIRECTION ( 'NONE',  ( 0.000000000000000000, 0.000000000000000000, 1.000000000000000000 ) ) ;
#46756 = CARTESIAN_POINT ( 'NONE',  ( 0.6000166863083106206, 46.77044519531232680, -14.97828220927686793 ) ) ;
#46757 = CIRCLE ( 'NONE', #59737, 47.09074272231896430 ) ;
#46758 = ORIENTED_EDGE ( 'NONE', *, *, #28786, .F. ) ;
#46759 = CARTESIAN_POINT ( 'NONE',  ( 1.227938101723756947, 41.66816631169191965, 10.28900963485394904 ) ) ;
#46760 = DIRECTION ( 'NONE',  ( 0.000000000000000000, 1.000000000000000000, 0.000000000000000000 ) ) ;
#46761 = CARTESIAN_POINT ( 'NONE',  ( 5.960721111146673579, -12.49016043756459915, -16.28787783074223228 ) ) ;
#46762 = B_SPLINE_CURVE_WITH_KNOTS ( 'NONE', 3,
 ( #27316, #51107, #61121, #13231 ),
 .UNSPECIFIED., .F., .F.,
 ( 4, 4 ),
 ( 0.000000000000000000, 0.005004948556313818311 ),
 .UNSPECIFIED. ) ;
#46763 = CARTESIAN_POINT ( 'NONE',  ( 1.827119703190777988, 39.28489939038887258, -17.60659059422136608 ) ) ;
#46764 = ADVANCED_FACE ( 'NONE', ( #48641 ), #16772, .T. ) ;
#46766 = CARTESIAN_POINT ( 'NONE',  ( 4.960156602257181468, 30.22163187094436054, -35.23783291257134920 ) ) ;
#46765 =( BOUNDED_SURFACE ( )  B_SPLINE_SURFACE ( 3, 1, ( 
 ( #36049, #27241 ),
 ( #50122, #46362 ),
 ( #12236, #36976 ),
 ( #3406, #2173 ) ),
 .UNSPECIFIED., .F., .F., .F. ) 
 B_SPLINE_SURFACE_WITH_KNOTS ( ( 4, 4 ),
 ( 2, 2 ),
 ( 0.000000000000000000, 1.000000000000000000 ),
 ( 0.000000000000000000, 1.000000000000000000 ),
 .UNSPECIFIED. ) 
 GEOMETRIC_REPRESENTATION_ITEM ( )  RATIONAL_B_SPLINE_SURFACE ( (
 ( 1.000000000000000000, 1.000000000000000000),
 ( 0.7269869731126821222, 0.9931720237060910339),
 ( 0.7269869731126821222, 0.9931720237060910339),
 ( 1.000000000000000000, 1.000000000000000000) ) ) 
 REPRESENTATION_ITEM ( '' )  SURFACE ( )  );
#46767 = DIRECTION ( 'NONE',  ( 1.000000000000000000, 1.836909530733573776E-16, 0.000000000000000000 ) ) ;
#46768 = CARTESIAN_POINT ( 'NONE',  ( 1.231276596079881047, 41.91134057782998212, 0.8463462572780127147 ) ) ;
#46769 = CARTESIAN_POINT ( 'NONE',  ( 0.5997462898726536595, 28.52220283460682282, -39.97543715340528081 ) ) ;
#46770 = ADVANCED_FACE ( 'NONE', ( #5402 ), #2701, .F. ) ;
#46771 = CONICAL_SURFACE ( 'NONE', #27884, 43.92652462719577500, 1.486293639869522343 ) ;
#46772 = CYLINDRICAL_SURFACE ( 'NONE', #31852, 4.250000000000000000 ) ;
#46773 = ADVANCED_FACE ( 'NONE', ( #9503 ), #39751, .F. ) ;
#46774 = EDGE_CURVE ( 'NONE', #44981, #57082, #30787, .T. ) ;
#46775 = CARTESIAN_POINT ( 'NONE',  ( 5.965394784446458765, -0.01447339372439073943, -20.52536205633085231 ) ) ;
#46776 = CARTESIAN_POINT ( 'NONE',  ( 0.3622758884714730732, -15.73321244754880688, 40.13994584881756111 ) ) ;
#46777 = CARTESIAN_POINT ( 'NONE',  ( 0.8753041380234465318, -20.68664920503345073, 44.53314352862224013 ) ) ;
#46778 = DIRECTION ( 'NONE',  ( 0.000000000000000000, 0.000000000000000000, 1.000000000000000000 ) ) ;
#46779 = CARTESIAN_POINT ( 'NONE',  ( 4.694002226626921015, 32.98704702821333967, -31.46648216443294999 ) ) ;
#46780 = CARTESIAN_POINT ( 'NONE',  ( 0.9740398440564312921, 37.36539512268019791, 21.09418882170549736 ) ) ;
#46781 = CARTESIAN_POINT ( 'NONE',  ( 3.559346040607745287, -21.01279064855753020, 38.62502958836252986 ) ) ;
#46782 =( BOUNDED_SURFACE ( )  B_SPLINE_SURFACE ( 3, 1, ( 
 ( #6499, #30333 ),
 ( #6192, #12188 ),
 ( #59770, #44780 ),
 ( #35375, #54431 ) ),
 .UNSPECIFIED., .F., .F., .F. ) 
 B_SPLINE_SURFACE_WITH_KNOTS ( ( 4, 4 ),
 ( 2, 2 ),
 ( 0.000000000000000000, 1.000000000000000000 ),
 ( 0.000000000000000000, 1.000000000000000000 ),
 .UNSPECIFIED. ) 
 GEOMETRIC_REPRESENTATION_ITEM ( )  RATIONAL_B_SPLINE_SURFACE ( (
 ( 1.000000000000000000, 1.000000000000000000),
 ( 0.9953040768229005630, 0.8617119497784937465),
 ( 0.9953040768229005630, 0.8617119497784937465),
 ( 1.000000000000000000, 1.000000000000000000) ) ) 
 REPRESENTATION_ITEM ( '' )  SURFACE ( )  );
#46783 = FACE_OUTER_BOUND ( 'NONE', #58604, .T. ) ;
#46784 = LINE ( 'NONE', #9461, #34302 ) ;
#46785 = CARTESIAN_POINT ( 'NONE',  ( 0.9722240750034554235, 11.66659272802858105, 41.29187379046130957 ) ) ;
#46787 = ORIENTED_EDGE ( 'NONE', *, *, #38219, .F. ) ;
#46786 = CARTESIAN_POINT ( 'NONE',  ( -6.016104459813374383, -9.416989654584190461, -16.32137543786092237 ) ) ;
#46788 = ORIENTED_EDGE ( 'NONE', *, *, #20227, .F. ) ;
#46789 = EDGE_CURVE ( 'NONE', #33551, #32792, #57400, .T. ) ;
#46790 = AXIS2_PLACEMENT_3D ( 'NONE', #17304, #8493, #32329 ) ;
#46791 = CARTESIAN_POINT ( 'NONE',  ( 0.1129192098497455998, 33.28205046155587610, 28.96993104685618547 ) ) ;
#46792 = CARTESIAN_POINT ( 'NONE',  ( 5.901764892641288895, 45.37424261077635634, -18.41655708698249683 ) ) ;
#46793 = CARTESIAN_POINT ( 'NONE',  ( 4.967162193818131399, -23.56777426397203357, 36.06913038482792189 ) ) ;
#46794 = ORIENTED_EDGE ( 'NONE', *, *, #4241, .T. ) ;
#46795 = ADVANCED_FACE ( 'NONE', ( #24220 ), #58535, .F. ) ;
#46796 = ORIENTED_EDGE ( 'NONE', *, *, #11790, .T. ) ;
#46797 = CARTESIAN_POINT ( 'NONE',  ( 0.3676999524040366896, -23.56959980820299094, -37.28839696479317212 ) ) ;
#46798 = LINE ( 'NONE', #17347, #14096 ) ;
#46799 = UNCERTAINTY_MEASURE_WITH_UNIT (LENGTH_MEASURE( 1.000000000000000082E-05 ), #50445, 'distance_accuracy_value', 'NONE');
#46800 = VERTEX_POINT ( 'NONE', #1317 ) ;
#46801 = VERTEX_POINT ( 'NONE', #21068 ) ;
#46802 = CARTESIAN_POINT ( 'NONE',  ( 0.9754642270333682141, -10.93570046136878737, -41.49150764699770377 ) ) ;
#46803 = DIRECTION ( 'NONE',  ( 0.000000000000000000, 0.000000000000000000, -1.000000000000000000 ) ) ;
#46804 = LINE ( 'NONE', #33008, #55955 ) ;
#46805 = ORIENTED_EDGE ( 'NONE', *, *, #60703, .T. ) ;
#46806 = ORIENTED_EDGE ( 'NONE', *, *, #37937, .F. ) ;
#46807 = DIRECTION ( 'NONE',  ( 0.000000000000000000, 0.000000000000000000, 1.000000000000000000 ) ) ;
#46808 = ORIENTED_EDGE ( 'NONE', *, *, #39489, .T. ) ;
#46809 = CARTESIAN_POINT ( 'NONE',  ( 0.5263152470540294336, 0.000000000000000000, 0.000000000000000000 ) ) ;
#46810 = CARTESIAN_POINT ( 'NONE',  ( 1.231276596079881047, -16.87422718933157739, -38.37365278131454005 ) ) ;
#46811 = CARTESIAN_POINT ( 'NONE',  ( 3.782625744892853525, 2.488346184749487211, -41.96482142652158842 ) ) ;
#46812 = VERTEX_POINT ( 'NONE', #49885 ) ;
#46813 = ADVANCED_FACE ( 'NONE', ( #30447 ), #40128, .F. ) ;
#46814 = CARTESIAN_POINT ( 'NONE',  ( 3.661933894777873455, -45.68403645958177606, -11.20713958649829500 ) ) ;
#46815 = ORIENTED_EDGE ( 'NONE', *, *, #31136, .T. ) ;
#46816 = AXIS2_PLACEMENT_3D ( 'NONE', #20644, #30035, #30967 ) ;
#46817 = VERTEX_POINT ( 'NONE', #11364 ) ;
#46818 = CARTESIAN_POINT ( 'NONE',  ( 0.8551540677456715978, -41.03346287276411175, -24.74404575822818941 ) ) ;
#46819 = EDGE_LOOP ( 'NONE', ( #11213, #60964, #53394, #29820 ) ) ;
#46820 = CARTESIAN_POINT ( 'NONE',  ( 0.5997462898726536595, 46.43852004798843325, 15.96920429754989890 ) ) ;
#46821 = CARTESIAN_POINT ( 'NONE',  ( -6.017396004339687465, -13.32495836419633761, 13.32329839588550335 ) ) ;
#46822 = CARTESIAN_POINT ( 'NONE',  ( 0.1129192098497455998, -23.28677643606931014, 37.47903188453085477 ) ) ;
#46823 = CARTESIAN_POINT ( 'NONE',  ( 0.5817216825391127166, -38.40350717126904101, 26.91478383999664814 ) ) ;
#46824 = FACE_BOUND ( 'NONE', #48419, .T. ) ;
#46825 = ORIENTED_EDGE ( 'NONE', *, *, #7259, .F. ) ;
#46826 = DIRECTION ( 'NONE',  ( 0.000000000000000000, 0.000000000000000000, 1.000000000000000000 ) ) ;
#46827 = DIRECTION ( 'NONE',  ( 0.1024043820194936449, 0.9844298967354735419, -0.1428674944015972947 ) ) ;
#46828 = CARTESIAN_POINT ( 'NONE',  ( 0.1092565886968785704, 39.72209809039397754, -16.78938711553589158 ) ) ;
#46829 = VERTEX_POINT ( 'NONE', #16071 ) ;
#46830 = CARTESIAN_POINT ( 'NONE',  ( 0.9754292580325127915, -22.05710644602384107, -35.63441485604581516 ) ) ;
#46831 = CARTESIAN_POINT ( 'NONE',  ( 1.231276596079881047, -37.78837162824498819, 18.14705873423338289 ) ) ;
#46832 = CARTESIAN_POINT ( 'NONE',  ( 0.9756950546413939440, 30.40918718457341896, 30.27237962848448660 ) ) ;
#46833 = CARTESIAN_POINT ( 'NONE',  ( 0.5987334363312692975, -24.93754700689008885, -42.30462924729660301 ) ) ;
#46834 = CIRCLE ( 'NONE', #54797, 47.91270532121795611 ) ;
#46835 = EDGE_LOOP ( 'NONE', ( #21357, #3933 ) ) ;
#46836 = FACE_OUTER_BOUND ( 'NONE', #44601, .T. ) ;
#46837 = CARTESIAN_POINT ( 'NONE',  ( 0.8753041380234465318, -2.462982411634898838, 49.04153388213869391 ) ) ;
#46838 = PRODUCT_DEFINITION_SHAPE ( 'NONE', 'NONE',  #61968 ) ;
#46839 = CARTESIAN_POINT ( 'NONE',  ( 5.965394784446460541, -14.50338846149123384, -14.52385693118997700 ) ) ;
#46840 = CARTESIAN_POINT ( 'NONE',  ( 0.9754402186311950107, -42.51649392388755189, 5.786576363453401761 ) ) ;
#46841 = CARTESIAN_POINT ( 'NONE',  ( 0.5830082357119563685, -46.80869808478055916, 2.859688540068253459 ) ) ;
#46842 = CARTESIAN_POINT ( 'NONE',  ( 3.678748215320119197, 20.99750299042923984, -44.24610358513390196 ) ) ;
#46843 = DIRECTION ( 'NONE',  ( -1.000000000000000000, -0.000000000000000000, -0.000000000000000000 ) ) ;
#46844 = CARTESIAN_POINT ( 'NONE',  ( 2.618530812446115519, -6.426312013672279555, 46.56639671588441587 ) ) ;
#46845 = B_SPLINE_CURVE_WITH_KNOTS ( 'NONE', 3,
 ( #43386, #113, #44015, #21334, #15479, #10783, #34588, #40463, #48367, #9851, #423, #29870, #49836, #45169, #5428, #35761, #2196, #24564, #19263 ),
 .UNSPECIFIED., .F., .F.,
 ( 4, 3, 3, 3, 3, 3, 4 ),
 ( 1.355252715606880543E-20, 0.0002612768053151711127, 0.0003919133833142926602, 0.0005225499612322640061, 0.0006531865391693361753, 0.0008112755173415186647, 0.0009693688056799727899 ),
 .UNSPECIFIED. ) ;
#46846 = EDGE_CURVE ( 'NONE', #42831, #28832, #50211, .T. ) ;
#46847 = CARTESIAN_POINT ( 'NONE',  ( 0.9791128995231623833, -1.405476621873006371, -41.88510558314887788 ) ) ;
#46848 = CARTESIAN_POINT ( 'NONE',  ( 0.1365634738349424393, 36.62793384158531040, 24.60197313468367142 ) ) ;
#46849 = VERTEX_POINT ( 'NONE', #35185 ) ;
#46850 = EDGE_CURVE ( 'NONE', #24289, #55598, #47758, .T. ) ;
#46851 = CARTESIAN_POINT ( 'NONE',  ( -2.000000000000009770, 3.464101615137749057, 0.000000000000000000 ) ) ;
#46852 = CARTESIAN_POINT ( 'NONE',  ( 0.8560838555295158248, -26.00596412780176081, 39.03924517540291106 ) ) ;
#46853 = CARTESIAN_POINT ( 'NONE',  ( 0.6253024248130497620, -13.31237246887635628, -47.26758896609333505 ) ) ;
#46854 = CARTESIAN_POINT ( 'NONE',  ( -4.473699999999997345, 1.530808498934191127E-15, 12.50000000000000000 ) ) ;
#46855 = B_SPLINE_CURVE_WITH_KNOTS ( 'NONE', 3,
 ( #36616, #8087, #18112, #37236 ),
 .UNSPECIFIED., .F., .F.,
 ( 4, 4 ),
 ( 0.000000000000000000, 0.005004948556313805301 ),
 .UNSPECIFIED. ) ;
#46856 = CARTESIAN_POINT ( 'NONE',  ( 2.359973842542476330, -24.09890286121120795, -36.84262172428024940 ) ) ;
#46857 = CARTESIAN_POINT ( 'NONE',  ( 0.1073791018717483448, 42.81622261970987608, 5.147744207007008299 ) ) ;
#46858 = CONTEXT_DEPENDENT_SHAPE_REPRESENTATION ( #49973, #11775 ) ;
#46859 = CARTESIAN_POINT ( 'NONE',  ( 0.5837157313716042628, -25.31061043140172728, 39.47923584837779032 ) ) ;
#46860 = STYLED_ITEM ( 'NONE', ( #25954 ), #21278 ) ;
#46861 = DIRECTION ( 'NONE',  ( 0.000000000000000000, 1.000000000000000000, 0.000000000000000000 ) ) ;
#46862 = VECTOR ( 'NONE', #59359, 1000.000000000000114 ) ;
#46863 = FACE_OUTER_BOUND ( 'NONE', #56870, .T. ) ;
#46865 = ORIENTED_EDGE ( 'NONE', *, *, #11036, .F. ) ;
#46864 = CARTESIAN_POINT ( 'NONE',  ( 0.6030672727741701600, -46.44558360017003906, -12.53539249098698427 ) ) ;
#46866 = ORIENTED_EDGE ( 'NONE', *, *, #53867, .T. ) ;
#46867 = DIRECTION ( 'NONE',  ( 0.07836865515943411409, 0.3742079063794837568, 0.9240274869783826617 ) ) ;
#46868 = CARTESIAN_POINT ( 'NONE',  ( 5.838029081930957709, -16.95764376597208667, 44.08518318051211793 ) ) ;
#46869 = CARTESIAN_POINT ( 'NONE',  ( 5.901463166500145796, 17.95741941801110642, -9.058087998373295591 ) ) ;
#46870 = EDGE_CURVE ( 'NONE', #7624, #5090, #6806, .T. ) ;
#46871 = ORIENTED_EDGE ( 'NONE', *, *, #3196, .T. ) ;
#46872 = CARTESIAN_POINT ( 'NONE',  ( 0.6024113833632039894, 11.13957392438117822, -47.82731188227197805 ) ) ;
#46873 = CARTESIAN_POINT ( 'NONE',  ( 0.5832655196449144652, -46.00108932644737081, 9.117837668742486912 ) ) ;
#46875 = CARTESIAN_POINT ( 'NONE',  ( 0.1081432562775997419, 6.048481838666034172, -42.69830087850306199 ) ) ;
#46874 = B_SPLINE_CURVE_WITH_KNOTS ( 'NONE', 3,
 ( #40523, #31722, #54886, #17015, #54254, #59588 ),
 .UNSPECIFIED., .F., .F.,
 ( 4, 2, 4 ),
 ( 1.264432626340127662E-17, 0.0002448709889506591082, 0.0004897419779013056397 ),
 .UNSPECIFIED. ) ;
#46876 = ORIENTED_EDGE ( 'NONE', *, *, #6547, .T. ) ;
#46877 = ORIENTED_EDGE ( 'NONE', *, *, #54010, .T. ) ;
#46878 = SURFACE_STYLE_FILL_AREA ( #4525 ) ;
#46879 = VECTOR ( 'NONE', #8398, 1000.000000000000114 ) ;
#46880 = CIRCLE ( 'NONE', #56852, 47.67072199303260049 ) ;
#46881 = CARTESIAN_POINT ( 'NONE',  ( 1.479689385636123067, 37.55715799008815736, 23.04438606201625817 ) ) ;
#46882 = CARTESIAN_POINT ( 'NONE',  ( 4.691466044806103852, 3.249105306917819735, 44.46979273209136352 ) ) ;
#46883 = CARTESIAN_POINT ( 'NONE',  ( -5.331200000000000827, 1.538011871406776419E-15, -12.55882000000000076 ) ) ;
#46884 = B_SPLINE_CURVE_WITH_KNOTS ( 'NONE', 3,
 ( #8416, #17846, #22235, #56034 ),
 .UNSPECIFIED., .F., .F.,
 ( 4, 4 ),
 ( 2.199414408396618760E-17, 0.004559932413162189405 ),
 .UNSPECIFIED. ) ;
#46885 = CARTESIAN_POINT ( 'NONE',  ( 0.6024113833632039894, 48.99212586890816112, 3.363550497008568119 ) ) ;
#46886 = EDGE_CURVE ( 'NONE', #29827, #34780, #54619, .T. ) ;
#46887 = CARTESIAN_POINT ( 'NONE',  ( 0.1073791018717578927, 11.62916352156150346, -41.52698815987157133 ) ) ;
#46888 = ORIENTED_EDGE ( 'NONE', *, *, #50754, .F. ) ;
#46889 = CARTESIAN_POINT ( 'NONE',  ( 4.967162193818130511, 36.06913038482831979, -23.56777426397140118 ) ) ;
#46890 = CONICAL_SURFACE ( 'NONE', #15892, 42.92674063221959813, 1.485477209440487556 ) ;
#46891 = ORIENTED_EDGE ( 'NONE', *, *, #6820, .F. ) ;
#46892 = CARTESIAN_POINT ( 'NONE',  ( 0.6031356755773454870, -47.69588082432152021, -6.279255973231177457 ) ) ;
#46893 = CARTESIAN_POINT ( 'NONE',  ( -6.077587904424778920, -17.34643006009186195, -8.360465630828942452 ) ) ;
#46894 = CARTESIAN_POINT ( 'NONE',  ( 1.112077966505211402, 39.24773055670718236, -20.06604024905431416 ) ) ;
#46895 = CARTESIAN_POINT ( 'NONE',  ( 3.240649175237396484, 37.83429905813157035, -22.44617411002408147 ) ) ;
#46896 = B_SPLINE_CURVE_WITH_KNOTS ( 'NONE', 3,
 ( #26537, #13078, #50639, #31238, #26851, #12157 ),
 .UNSPECIFIED., .F., .F.,
 ( 4, 2, 4 ),
 ( 1.265278335494562270E-16, 0.0002450741128632358658, 0.0004901482257263452052 ),
 .UNSPECIFIED. ) ;
#46897 = ORIENTED_EDGE ( 'NONE', *, *, #33447, .T. ) ;
#46899 = EDGE_CURVE ( 'NONE', #995, #20273, #3817, .T. ) ;
#46898 = ORIENTED_EDGE ( 'NONE', *, *, #7555, .T. ) ;
#46900 = CARTESIAN_POINT ( 'NONE',  ( 0.1158516988532803521, -44.12414005494260039, 0.04922646246316730867 ) ) ;
#46901 = CARTESIAN_POINT ( 'NONE',  ( 0.5834872094924180574, 41.36515088387913153, 24.14431479207704712 ) ) ;
#46902 = CARTESIAN_POINT ( 'NONE',  ( 0.5806925824938502512, -2.112975627976310111, -46.84824112321764744 ) ) ;
#46903 = PRODUCT_DEFINITION_FORMATION_WITH_SPECIFIED_SOURCE ( 'ANY', '', #31800, .NOT_KNOWN. ) ;
#46904 = VERTEX_POINT ( 'NONE', #45214 ) ;
#46905 = CARTESIAN_POINT ( 'NONE',  ( 5.974727161628367256, -12.48248968439940931, 16.29297756969626576 ) ) ;
#46906 = EDGE_CURVE ( 'NONE', #22913, #35798, #56075, .T. ) ;
#46907 = ORIENTED_EDGE ( 'NONE', *, *, #21862, .F. ) ;
#46908 = CARTESIAN_POINT ( 'NONE',  ( 1.834102595619085507, 43.46554130548571493, 7.137539063206623347 ) ) ;
#46909 = CARTESIAN_POINT ( 'NONE',  ( 0.6029442701453591180, -25.38242846679687048, 42.03900034832199140 ) ) ;
#46910 = CARTESIAN_POINT ( 'NONE',  ( 0.6029443449137436017, -13.93069009245118473, -47.09007763352503417 ) ) ;
#46911 = ORIENTED_EDGE ( 'NONE', *, *, #52001, .T. ) ;
#46913 = CIRCLE ( 'NONE', #13904, 15.38218000000000174 ) ;
#46912 = CARTESIAN_POINT ( 'NONE',  ( 0.8560838555295223751, 37.37287335782406217, 28.34856559090382078 ) ) ;
#46914 = CARTESIAN_POINT ( 'NONE',  ( 0.1149546198390367230, -27.72460785286477858, 34.32626814012978400 ) ) ;
#46915 = CARTESIAN_POINT ( 'NONE',  ( 3.678834586032786014, 44.89638856848508652, -19.56851203172985265 ) ) ;
#46916 = ORIENTED_EDGE ( 'NONE', *, *, #134, .F. ) ;
#46917 = CARTESIAN_POINT ( 'NONE',  ( 4.960156602257181468, -14.43621227656497297, -44.12083041402478756 ) ) ;
#46918 = LINE ( 'NONE', #8352, #35513 ) ;
#46919 = CARTESIAN_POINT ( 'NONE',  ( -6.016761891674564211, 17.40752468084793136, -7.214149619366169830 ) ) ;
#46920 = LINE ( 'NONE', #51894, #25766 ) ;
#46921 = EDGE_LOOP ( 'NONE', ( #36241, #26052, #39054, #5918 ) ) ;
#46922 = EDGE_CURVE ( 'NONE', #13823, #46085, #55737, .T. ) ;
#46923 = CARTESIAN_POINT ( 'NONE',  ( 5.880360259849739535, 21.25991003419893488, 43.00389496650622334 ) ) ;
#46924 = CONICAL_SURFACE ( 'NONE', #53890, 5.453125000000000000, 0.4883339510563931007 ) ;
#46925 = CARTESIAN_POINT ( 'NONE',  ( 1.114299999999999846, 0.000000000000000000, 0.000000000000000000 ) ) ;
#46926 = VERTEX_POINT ( 'NONE', #32639 ) ;
#46927 = AXIS2_PLACEMENT_3D ( 'NONE', #26157, #2960, #21154 ) ;
#46928 = EDGE_CURVE ( 'NONE', #55527, #33684, #39704, .T. ) ;
#46929 = DIRECTION ( 'NONE',  ( 0.000000000000000000, 0.000000000000000000, 1.000000000000000000 ) ) ;
#46930 = CARTESIAN_POINT ( 'NONE',  ( 4.963659409799328515, -36.94443854030204477, -25.25989740981538390 ) ) ;
#46931 = CARTESIAN_POINT ( 'NONE',  ( 5.838029081930957709, -32.85120734338257620, -33.93911068715571133 ) ) ;
#46932 = CARTESIAN_POINT ( 'NONE',  ( 0.9749527285493317930, 5.883724875809718036, -42.50314808877153183 ) ) ;
#46933 = DIRECTION ( 'NONE',  ( 1.000000000000000000, 1.558861125776144859E-16, -3.851859888774471706E-32 ) ) ;
#46934 = CARTESIAN_POINT ( 'NONE',  ( 0.3676999524040366896, 3.413584541509296688, -43.98065510995495941 ) ) ;
#46935 = EDGE_CURVE ( 'NONE', #26853, #42210, #44784, .T. ) ;
#46936 = CARTESIAN_POINT ( 'NONE',  ( 0.5998501479064708430, 47.62484632993678701, 6.798102206414301740 ) ) ;
#46937 = CARTESIAN_POINT ( 'NONE',  ( -6.077587904424778920, 3.067159685105322442, 19.01022232536997691 ) ) ;
#46938 = DIRECTION ( 'NONE',  ( 0.000000000000000000, 0.000000000000000000, 1.000000000000000000 ) ) ;
#46939 = CARTESIAN_POINT ( 'NONE',  ( -1.114299999999999624, 0.000000000000000000, -6.866799999999992465 ) ) ;
#46940 = VERTEX_POINT ( 'NONE', #3180 ) ;
#46941 = VECTOR ( 'NONE', #58350, 1000.000000000000000 ) ;
#46942 = CARTESIAN_POINT ( 'NONE',  ( 0.1365634738349397193, 40.02584797782402859, -18.56863250967517587 ) ) ;
#46943 = CARTESIAN_POINT ( 'NONE',  ( 0.6008123274975392114, -1.138712662034059075, -49.09437732196816029 ) ) ;
#46944 = CARTESIAN_POINT ( 'NONE',  ( 0.6846871229502899947, 47.90045233486064546, -0.8641397935261211360 ) ) ;
#46945 = EDGE_CURVE ( 'NONE', #46672, #31513, #5252, .T. ) ;
#46946 = CARTESIAN_POINT ( 'NONE',  ( 0.9754292580325130135, -17.11069898979941328, -38.25639092994113355 ) ) ;
#46947 = CARTESIAN_POINT ( 'NONE',  ( 0.5824936645240084143, 46.42765496787452406, 6.611432010109767887 ) ) ;
#46948 = CARTESIAN_POINT ( 'NONE',  ( 0.5998501479064699549, -37.84527566984877467, 29.69975237324549155 ) ) ;
#46949 = ORIENTED_EDGE ( 'NONE', *, *, #13038, .T. ) ;
#46950 = CARTESIAN_POINT ( 'NONE',  ( 0.9749527285493296835, 11.38116287125111903, -41.37154756071283401 ) ) ;
#46951 = CARTESIAN_POINT ( 'NONE',  ( 3.559346040607745287, -32.98083365439821080, -29.08083377420432214 ) ) ;
#46952 = CARTESIAN_POINT ( 'NONE',  ( 2.528190830796657629, 30.04139741748772252, -29.32181060844588316 ) ) ;
#46953 = CARTESIAN_POINT ( 'NONE',  ( 0.6021447746440204973, -45.61591350405682732, -18.18597190910877615 ) ) ;
#46954 = ORIENTED_EDGE ( 'NONE', *, *, #60895, .F. ) ;
#46955 = FACE_OUTER_BOUND ( 'NONE', #31540, .T. ) ;
#46956 = CARTESIAN_POINT ( 'NONE',  ( 4.549368137175248350, 0.000000000000000000, 0.000000000000000000 ) ) ;
#46957 =( BOUNDED_SURFACE ( )  B_SPLINE_SURFACE ( 3, 1, ( 
 ( #4185, #23026 ),
 ( #27397, #12706 ),
 ( #51194, #2967 ),
 ( #41838, #59983 ) ),
 .UNSPECIFIED., .F., .F., .F. ) 
 B_SPLINE_SURFACE_WITH_KNOTS ( ( 4, 4 ),
 ( 2, 2 ),
 ( 0.000000000000000000, 1.000000000000000000 ),
 ( 0.000000000000000000, 1.000000000000000000 ),
 .UNSPECIFIED. ) 
 GEOMETRIC_REPRESENTATION_ITEM ( )  RATIONAL_B_SPLINE_SURFACE ( (
 ( 1.000000000000000000, 1.000000000000000000),
 ( 0.9953390228620291325, 0.8624445117760984880),
 ( 0.9953390228620291325, 0.8624445117760984880),
 ( 1.000000000000000000, 1.000000000000000000) ) ) 
 REPRESENTATION_ITEM ( '' )  SURFACE ( )  );
#46958 = VERTEX_POINT ( 'NONE', #36121 ) ;
#46959 = CIRCLE ( 'NONE', #59939, 15.43999999999999240 ) ;
#46960 = CARTESIAN_POINT ( 'NONE',  ( -6.078075953587585900, -6.645381366291293723, -18.07302079741193879 ) ) ;
#46961 = EDGE_LOOP ( 'NONE', ( #18196, #61845, #42626, #8934 ) ) ;
#46962 = LINE ( 'NONE', #13134, #46879 ) ;
#46963 = DIRECTION ( 'NONE',  ( 0.000000000000000000, 0.000000000000000000, 1.000000000000000000 ) ) ;
#46964 = ORIENTED_EDGE ( 'NONE', *, *, #55081, .F. ) ;
#46965 = CARTESIAN_POINT ( 'NONE',  ( 5.860006189529234355, -31.78942168514587507, 36.27483683749426291 ) ) ;
#46966 = CARTESIAN_POINT ( 'NONE',  ( 5.901764892641307547, 39.21882766674595189, 29.32362569474928549 ) ) ;
#46967 = VERTEX_POINT ( 'NONE', #50800 ) ;
#46968 = CARTESIAN_POINT ( 'NONE',  ( 0.5817217712918332229, -7.350851069864205556, -46.31630320477930951 ) ) ;
#46969 = CARTESIAN_POINT ( 'NONE',  ( 0.7044674535452954967, -48.80743866909971018, 5.443955673311092980 ) ) ;
#46970 = EDGE_CURVE ( 'NONE', #47841, #9802, #47117, .T. ) ;
#46971 = ORIENTED_EDGE ( 'NONE', *, *, #51146, .T. ) ;
#46972 = EDGE_CURVE ( 'NONE', #58372, #5948, #42683, .T. ) ;
#46973 = CARTESIAN_POINT ( 'NONE',  ( 0.6016117650947688800, -8.181245532462590120, -48.42125851092740874 ) ) ;
#46974 = EDGE_LOOP ( 'NONE', ( #10004, #12347, #60769, #22598 ) ) ;
#46975 = CARTESIAN_POINT ( 'NONE',  ( 5.959547316686252039, -20.34955788964378698, 2.682663672454569159 ) ) ;
#46976 = EDGE_LOOP ( 'NONE', ( #5063, #48788, #57812, #23116 ) ) ;
#46977 = ADVANCED_FACE ( 'NONE', ( #56418 ), #42135, .F. ) ;
#46978 = VERTEX_POINT ( 'NONE', #17609 ) ;
#46979 = CARTESIAN_POINT ( 'NONE',  ( 0.9754292589017173887, 28.71299572461916583, -30.52689541065851486 ) ) ;
#46980 = CARTESIAN_POINT ( 'NONE',  ( 0.6031356755773454870, -34.01708126935065479, 34.01711753073199418 ) ) ;
#46981 = CONICAL_SURFACE ( 'NONE', #5914, 42.08604991992415023, 1.569615340895231137 ) ;
#46982 = CARTESIAN_POINT ( 'NONE',  ( 0.9757892942422814464, 34.07281211842327906, 26.08029006934548377 ) ) ;
#46983 = CARTESIAN_POINT ( 'NONE',  ( 0.3676999524040366896, -28.14442808720893296, -33.96824621564622504 ) ) ;
#46984 = ORIENTED_EDGE ( 'NONE', *, *, #40365, .F. ) ;
#46985 = CARTESIAN_POINT ( 'NONE',  ( 0.9757954354143114628, 0.01316335317109677827, -42.90846090505964838 ) ) ;
#46986 = CARTESIAN_POINT ( 'NONE',  ( 1.227938101723756947, 0.8460948827225182045, 42.91134962331487657 ) ) ;
#46987 = CARTESIAN_POINT ( 'NONE',  ( 2.706805983486680223, 0.2451503928605884286, 44.00813577742911065 ) ) ;
#46988 = ORIENTED_EDGE ( 'NONE', *, *, #56222, .T. ) ;
#46989 = B_SPLINE_CURVE_WITH_KNOTS ( 'NONE', 3,
 ( #9028, #51623, #61325, #22825 ),
 .UNSPECIFIED., .F., .F.,
 ( 4, 4 ),
 ( 2.294131830766625192E-17, 0.004564976165746188579 ),
 .UNSPECIFIED. ) ;
#46990 = ORIENTED_EDGE ( 'NONE', *, *, #53326, .T. ) ;
#46991 = CARTESIAN_POINT ( 'NONE',  ( 0.9730545539215883499, -41.57420493492393376, 10.61654491617549034 ) ) ;
#46992 = CARTESIAN_POINT ( 'NONE',  ( 4.962356264823591268, 23.01169039590626753, 35.23773124060775785 ) ) ;
#46993 = CARTESIAN_POINT ( 'NONE',  ( -6.077587904424778920, -11.01164173315279271, -15.79682777441781738 ) ) ;
#46994 = CARTESIAN_POINT ( 'NONE',  ( 4.335381028904201628, 43.17230378757372478, 23.14970914153764170 ) ) ;
#46995 = FACE_OUTER_BOUND ( 'NONE', #25380, .T. ) ;
#46996 = EDGE_CURVE ( 'NONE', #16356, #43088, #56717, .T. ) ;
#46997 = VERTEX_POINT ( 'NONE', #41134 ) ;
#46998 = CARTESIAN_POINT ( 'NONE',  ( 2.891212509699203626, -1.730266096895115631E-16, -41.99381090189411481 ) ) ;
#46999 = EDGE_CURVE ( 'NONE', #3847, #23682, #60808, .T. ) ;
#47000 = DIRECTION ( 'NONE',  ( 0.000000000000000000, 0.000000000000000000, 1.000000000000000000 ) ) ;
#47001 = CARTESIAN_POINT ( 'NONE',  ( 4.226256110419178924, 42.60700927045893138, -10.74569732563750968 ) ) ;
#47002 = DIRECTION ( 'NONE',  ( 1.000000000000000000, 0.000000000000000000, 0.000000000000000000 ) ) ;
#47003 = CARTESIAN_POINT ( 'NONE',  ( 4.060580049360325461, -41.54832425072979163, -14.32495885911816380 ) ) ;
#47004 = ADVANCED_FACE ( 'NONE', ( #27618 ), #15760, .F. ) ;
#47005 = CARTESIAN_POINT ( 'NONE',  ( 0.5809828226811544205, -34.25055090842130312, -33.48000389720652947 ) ) ;
#47006 = ORIENTED_EDGE ( 'NONE', *, *, #59864, .F. ) ;
#47007 = CARTESIAN_POINT ( 'NONE',  ( 2.281351352603294913, -22.83955855331488038, -42.18750813859382731 ) ) ;
#47008 = CARTESIAN_POINT ( 'NONE',  ( 4.694002226626920127, 39.55162978021545683, -22.67053932254166781 ) ) ;
#47009 = CARTESIAN_POINT ( 'NONE',  ( 0.5804410086790514622, -7.261380058784682845, 46.33348909263450111 ) ) ;
#47010 = CARTESIAN_POINT ( 'NONE',  ( 0.1073791018717578927, -16.05399293000789385, -40.02496097243051310 ) ) ;
#47011 = AXIS2_PLACEMENT_3D ( 'NONE', #6146, #25908, #40340 ) ;
#47012 = CARTESIAN_POINT ( 'NONE',  ( 0.5850706913938533704, 18.49682194438024752, -44.18063951072202400 ) ) ;
#47013 = CARTESIAN_POINT ( 'NONE',  ( 5.959828726073459926, 16.28681682518064378, -12.49160845136018061 ) ) ;
#47014 = EDGE_CURVE ( 'NONE', #28601, #14851, #23253, .T. ) ;
#47015 = CARTESIAN_POINT ( 'NONE',  ( 4.963659409799328515, -33.33129552235065773, -29.86601237216442684 ) ) ;
#47016 = CARTESIAN_POINT ( 'NONE',  ( 5.959547316686252039, 5.315863417546330183, -19.82530672674356964 ) ) ;
#47017 = CARTESIAN_POINT ( 'NONE',  ( 5.917102823773431552, -13.98784315367447029, -14.45095020958636667 ) ) ;
#47018 = ORIENTED_EDGE ( 'NONE', *, *, #34041, .T. ) ;
#47019 = DIRECTION ( 'NONE',  ( 0.000000000000000000, 0.000000000000000000, 1.000000000000000000 ) ) ;
#47020 = CARTESIAN_POINT ( 'NONE',  ( 0.1129192098497455998, 44.06201484046248140, -2.343210614524073421 ) ) ;
#47021 = CARTESIAN_POINT ( 'NONE',  ( 1.231276596079881047, 40.19859528295886975, 11.88905834349143653 ) ) ;
#47022 = FACE_OUTER_BOUND ( 'NONE', #27678, .T. ) ;
#47023 = ORIENTED_EDGE ( 'NONE', *, *, #7228, .F. ) ;
#47024 = CARTESIAN_POINT ( 'NONE',  ( 0.1152809850208375841, 4.016710468846341975, 43.94099816229958577 ) ) ;
#47025 = ORIENTED_EDGE ( 'NONE', *, *, #32477, .T. ) ;
#47026 = CARTESIAN_POINT ( 'NONE',  ( 0.1156867017252034696, 4.361299308302413635, -43.90810717417215159 ) ) ;
#47027 = B_SPLINE_CURVE_WITH_KNOTS ( 'NONE', 3,
 ( #21410, #56145, #7925, #59610, #41781, #17960 ),
 .UNSPECIFIED., .F., .F.,
 ( 4, 2, 4 ),
 ( 0.004120275011746849653, 0.005288420935197133549, 0.006456566858647417445 ),
 .UNSPECIFIED. ) ;
#47028 = CARTESIAN_POINT ( 'NONE',  ( 0.5806925824938499181, -45.84420715090598009, -9.875780123533834498 ) ) ;
#47029 = CARTESIAN_POINT ( 'NONE',  ( 4.962356264823603702, 26.83784316460332420, -32.41860225448503030 ) ) ;
#47031 = EDGE_LOOP ( 'NONE', ( #43723, #7298, #32622, #31392 ) ) ;
#47030 =( BOUNDED_SURFACE ( )  B_SPLINE_SURFACE ( 3, 1, ( 
 ( #37982, #52646 ),
 ( #38281, #33267 ),
 ( #42660, #27935 ),
 ( #57956, #14465 ) ),
 .UNSPECIFIED., .F., .F., .F. ) 
 B_SPLINE_SURFACE_WITH_KNOTS ( ( 4, 4 ),
 ( 2, 2 ),
 ( 0.000000000000000000, 1.000000000000000000 ),
 ( 0.000000000000000000, 1.000000000000000000 ),
 .UNSPECIFIED. ) 
 GEOMETRIC_REPRESENTATION_ITEM ( )  RATIONAL_B_SPLINE_SURFACE ( (
 ( 1.000000000000000000, 1.000000000000000000),
 ( 0.9953040768229013402, 0.8617119497784988535),
 ( 0.9953040768229013402, 0.8617119497784988535),
 ( 1.000000000000000000, 1.000000000000000000) ) ) 
 REPRESENTATION_ITEM ( '' )  SURFACE ( )  );
#47032 = CARTESIAN_POINT ( 'NONE',  ( 0.7954196712028465122, 46.22745629466055561, 13.28627209367592954 ) ) ;
#47033 = ORIENTED_EDGE ( 'NONE', *, *, #59677, .F. ) ;
#47034 = ORIENTED_EDGE ( 'NONE', *, *, #33316, .F. ) ;
#47035 = CARTESIAN_POINT ( 'NONE',  ( 3.407937589446178528, -3.987184287467695043, -13.10584870154470671 ) ) ;
#47036 = FACE_OUTER_BOUND ( 'NONE', #17136, .T. ) ;
#47037 = EDGE_CURVE ( 'NONE', #53844, #44630, #21696, .T. ) ;
#47038 = ORIENTED_EDGE ( 'NONE', *, *, #51915, .F. ) ;
#47039 = FACE_OUTER_BOUND ( 'NONE', #2244, .T. ) ;
#47040 = ORIENTED_EDGE ( 'NONE', *, *, #22285, .F. ) ;
#47041 = EDGE_CURVE ( 'NONE', #61654, #42964, #58277, .T. ) ;
#47042 = CARTESIAN_POINT ( 'NONE',  ( 5.894904586330512508, -19.39861238634053819, -5.312555839344970998 ) ) ;
#47043 = FACE_OUTER_BOUND ( 'NONE', #26547, .T. ) ;
#47044 = FACE_OUTER_BOUND ( 'NONE', #38627, .T. ) ;
#47045 = ADVANCED_FACE ( 'NONE', ( #28531 ), #20744, .F. ) ;
#47046 = ORIENTED_EDGE ( 'NONE', *, *, #6161, .F. ) ;
#47047 = EDGE_CURVE ( 'NONE', #57756, #31240, #45687, .T. ) ;
#47048 = LINE ( 'NONE', #42649, #25467 ) ;
#47049 = CARTESIAN_POINT ( 'NONE',  ( 5.901463166500145796, 19.71248269111032414, -3.991979019648351112 ) ) ;
#47050 = CARTESIAN_POINT ( 'NONE',  ( 5.895596859100789899, 17.95274561709314654, -9.067916410092799140 ) ) ;
#47051 = CARTESIAN_POINT ( 'NONE',  ( 0.1158516988532803382, -22.91572194069864921, -37.70692040951341539 ) ) ;
#47053 = EDGE_CURVE ( 'NONE', #11266, #56932, #10374, .T. ) ;
#47052 = VERTEX_POINT ( 'NONE', #52027 ) ;
#47054 = CARTESIAN_POINT ( 'NONE',  ( -6.017396004339687465, 9.420565012089426205, 16.31924478664278766 ) ) ;
#47055 = FACE_OUTER_BOUND ( 'NONE', #25802, .T. ) ;
#47056 = EDGE_LOOP ( 'NONE', ( #31061, #13206, #1662, #17723 ) ) ;
#47057 = CARTESIAN_POINT ( 'NONE',  ( 5.960721111146673579, 12.49016043756449434, 16.28787783074231399 ) ) ;
#47058 = ORIENTED_EDGE ( 'NONE', *, *, #52292, .F. ) ;
#47059 = CIRCLE ( 'NONE', #45057, 47.09074272231896430 ) ;
#47060 = LINE ( 'NONE', #28533, #47535 ) ;
#47061 = EDGE_CURVE ( 'NONE', #29140, #31868, #11271, .T. ) ;
#47062 = CARTESIAN_POINT ( 'NONE',  ( 5.959828726073459926, 10.26672511661731058, 17.77343634131845462 ) ) ;
#47063 = ORIENTED_EDGE ( 'NONE', *, *, #4714, .T. ) ;
#47064 = CARTESIAN_POINT ( 'NONE',  ( 0.2885700199627532769, -37.73587457854652882, -20.85752789928049111 ) ) ;
#47065 = CARTESIAN_POINT ( 'NONE',  ( 0.8751705887134553219, 48.08707113907595243, -0.8911681664083408450 ) ) ;
#47066 = CARTESIAN_POINT ( 'NONE',  ( 2.282803330402965347, -35.70555387398805181, 30.52229234524697432 ) ) ;
#47067 = LINE ( 'NONE', #57041, #58419 ) ;
#47068 = AXIS2_PLACEMENT_3D ( 'NONE', #20318, #1795, #11859 ) ;
#47069 = VERTEX_POINT ( 'NONE', #28230 ) ;
#47070 = CARTESIAN_POINT ( 'NONE',  ( 0.8557997880470599172, 5.347802024197243043, 47.60865952217000796 ) ) ;
#47071 = CARTESIAN_POINT ( 'NONE',  ( 0.9789889208857693870, -41.80852869865788080, 2.895138355220653548 ) ) ;
#47072 = CARTESIAN_POINT ( 'NONE',  ( 4.962356264823601926, -41.76635909427990612, -5.177532797579353918 ) ) ;
#47073 = FACE_OUTER_BOUND ( 'NONE', #40940, .T. ) ;
#47074 = B_SPLINE_CURVE_WITH_KNOTS ( 'NONE', 3,
 ( #44398, #14645, #25557, #19648 ),
 .UNSPECIFIED., .F., .F.,
 ( 4, 4 ),
 ( 0.000000000000000000, 0.004050076154992998147 ),
 .UNSPECIFIED. ) ;
#47075 = CARTESIAN_POINT ( 'NONE',  ( 5.895881250540457863, 20.06765451668685785, -1.347933161250387535 ) ) ;
#47076 = CARTESIAN_POINT ( 'NONE',  ( 0.9762797500689124330, -12.89881610234976961, 39.87411852747928265 ) ) ;
#47077 = DIRECTION ( 'NONE',  ( 0.000000000000000000, 0.000000000000000000, 1.000000000000000000 ) ) ;
#47078 = CARTESIAN_POINT ( 'NONE',  ( 0.9790724872846777727, -12.45512225568080567, 40.01506140914315779 ) ) ;
#47079 = CARTESIAN_POINT ( 'NONE',  ( 0.9972139404380323535, 33.63772329383416348, -26.64066783422301654 ) ) ;
#47080 = ADVANCED_FACE ( 'NONE', ( #47348 ), #4938, .F. ) ;
#47081 = CARTESIAN_POINT ( 'NONE',  ( 0.1103878639767399417, -21.52017980327924462, 37.37111717125835497 ) ) ;
#47082 = CARTESIAN_POINT ( 'NONE',  ( -6.017396004339687465, -11.47005965438128783, -14.95000090562892936 ) ) ;
#47083 = CARTESIAN_POINT ( 'NONE',  ( -6.077587904424778920, -17.34643006009186195, -8.360465630828942452 ) ) ;
#47084 = ADVANCED_FACE ( 'NONE', ( #11293 ), #60742, .T. ) ;
#47085 = CARTESIAN_POINT ( 'NONE',  ( 4.975801465491694664, 46.87746200127440943, 9.906103548668390602 ) ) ;
#47086 = CARTESIAN_POINT ( 'NONE',  ( 0.5806925824938499181, 45.37089516811292356, -11.86188155343291584 ) ) ;
#47087 = CARTESIAN_POINT ( 'NONE',  ( 4.553261556744875094, 0.000000000000000000, 0.000000000000000000 ) ) ;
#47089 = EDGE_LOOP ( 'NONE', ( #51773, #48034, #29432, #34540 ) ) ;
#47088 = CARTESIAN_POINT ( 'NONE',  ( -9.500000000000000000, 1.163414459189985485E-15, -1.199999999999999956 ) ) ;
#47090 = CARTESIAN_POINT ( 'NONE',  ( 0.6021447746440204973, -39.19855282349202241, 29.58064562568560163 ) ) ;
#47091 = CARTESIAN_POINT ( 'NONE',  ( 0.5809828226811617480, 23.47450554821709900, 41.74875432577658074 ) ) ;
#47092 = LINE ( 'NONE', #4740, #23711 ) ;
#47093 = ORIENTED_EDGE ( 'NONE', *, *, #30895, .F. ) ;
#47094 = ORIENTED_EDGE ( 'NONE', *, *, #41719, .F. ) ;
#47095 = CARTESIAN_POINT ( 'NONE',  ( 3.390910168358336918, -30.18958311396259830, 31.97946541045958924 ) ) ;
#47096 = CARTESIAN_POINT ( 'NONE',  ( 0.5997462898726536595, 5.235280152387000285, 48.82769165002921596 ) ) ;
#47098 = ORIENTED_EDGE ( 'NONE', *, *, #23530, .F. ) ;
#47097 = AXIS2_PLACEMENT_3D ( 'NONE', #48323, #44892, #38638 ) ;
#47099 = ORIENTED_EDGE ( 'NONE', *, *, #8249, .T. ) ;
#47100 = CARTESIAN_POINT ( 'NONE',  ( 0.6028618097248863439, -38.27229381545031828, -29.14732267129559773 ) ) ;
#47101 = LINE ( 'NONE', #9478, #34998 ) ;
#47102 = CARTESIAN_POINT ( 'NONE',  ( 0.8744876279028263033, 48.92939099258497038, 4.032957658374010101 ) ) ;
#47103 = ORIENTED_EDGE ( 'NONE', *, *, #32694, .T. ) ;
#47104 = ORIENTED_EDGE ( 'NONE', *, *, #11042, .T. ) ;
#47105 = CARTESIAN_POINT ( 'NONE',  ( 0.5839880159502339740, -12.35255585954151236, -46.27569712847346750 ) ) ;
#47106 = ORIENTED_EDGE ( 'NONE', *, *, #35331, .F. ) ;
#47107 = LINE ( 'NONE', #3849, #3023 ) ;
#47108 = CARTESIAN_POINT ( 'NONE',  ( 0.2285344041767099210, 9.075216059588225193, -43.17570640727545594 ) ) ;
#47109 = VERTEX_POINT ( 'NONE', #25696 ) ;
#47110 = EDGE_CURVE ( 'NONE', #22672, #60467, #9045, .T. ) ;
#47111 = CARTESIAN_POINT ( 'NONE',  ( 0.1103310638050661735, 0.08238894504395631591, -43.12437788119554227 ) ) ;
#47112 = EDGE_CURVE ( 'NONE', #1293, #40747, #24774, .T. ) ;
#47113 = ORIENTED_EDGE ( 'NONE', *, *, #49674, .F. ) ;
#47114 = ORIENTED_EDGE ( 'NONE', *, *, #58527, .T. ) ;
#47115 = ADVANCED_FACE ( 'NONE', ( #6552 ), #57736, .T. ) ;
#47116 = CARTESIAN_POINT ( 'NONE',  ( 0.5980894510889448457, -38.59343625445466586, 28.72954109785538890 ) ) ;
#47117 = B_SPLINE_CURVE_WITH_KNOTS ( 'NONE', 3,
 ( #18233, #61114, #51099, #7888 ),
 .UNSPECIFIED., .F., .F.,
 ( 4, 4 ),
 ( 8.673617379884035472E-19, 0.004050076154992998147 ),
 .UNSPECIFIED. ) ;
#47118 = ORIENTED_EDGE ( 'NONE', *, *, #36588, .F. ) ;
#47119 = CARTESIAN_POINT ( 'NONE',  ( 0.6024113833632039894, 46.53665168057906953, 15.68062241944890722 ) ) ;
#47120 = CARTESIAN_POINT ( 'NONE',  ( 0.6001305935487422083, 34.38748867424712330, -33.64689939321907275 ) ) ;
#47121 = CARTESIAN_POINT ( 'NONE',  ( -5.720000000000002416, 16.00000000000000355, 0.000000000000000000 ) ) ;
#47122 = EDGE_CURVE ( 'NONE', #55130, #24670, #26730, .T. ) ;
#47123 = CARTESIAN_POINT ( 'NONE',  ( -6.016104459813374383, 11.46679299034580168, 14.95258000663136499 ) ) ;
#47124 = PLANE ( 'NONE',  #48388 ) ;
#47125 = EDGE_LOOP ( 'NONE', ( #34981, #39967, #3152, #41433 ) ) ;
#47126 = CARTESIAN_POINT ( 'NONE',  ( 0.5806925824938499181, 16.34374012233052653, 43.95571090492437349 ) ) ;
#47127 = LINE ( 'NONE', #37421, #8751 ) ;
#47128 =( BOUNDED_SURFACE ( )  B_SPLINE_SURFACE ( 3, 1, ( 
 ( #12856, #2797 ),
 ( #31320, #59501 ),
 ( #32257, #22546 ),
 ( #60417, #12541 ) ),
 .UNSPECIFIED., .F., .F., .F. ) 
 B_SPLINE_SURFACE_WITH_KNOTS ( ( 4, 4 ),
 ( 2, 2 ),
 ( 0.000000000000000000, 1.000000000000000000 ),
 ( 0.000000000000000000, 1.000000000000000000 ),
 .UNSPECIFIED. ) 
 GEOMETRIC_REPRESENTATION_ITEM ( )  RATIONAL_B_SPLINE_SURFACE ( (
 ( 1.000000000000000000, 1.000000000000000000),
 ( 0.7282232189291693025, 0.9929344683865674037),
 ( 0.7282232189291693025, 0.9929344683865674037),
 ( 1.000000000000000000, 1.000000000000000000) ) ) 
 REPRESENTATION_ITEM ( '' )  SURFACE ( )  );
#47129 = CARTESIAN_POINT ( 'NONE',  ( 0.1087620492084205581, 39.97903073778065419, -16.16798550313382066 ) ) ;
#47130 = ORIENTED_EDGE ( 'NONE', *, *, #846, .T. ) ;
#47131 = CARTESIAN_POINT ( 'NONE',  ( 0.8557997880470690211, -38.55640757422419540, -28.43566216845010075 ) ) ;
#47132 = CARTESIAN_POINT ( 'NONE',  ( 0.9740398440564311811, 30.63262235044629378, 30.04629765303400291 ) ) ;
#47133 = CARTESIAN_POINT ( 'NONE',  ( 3.221118495291109163, -5.149125434531551804, 43.68349719197414061 ) ) ;
#47134 = EDGE_LOOP ( 'NONE', ( #60180, #20590, #22379, #14673 ) ) ;
#47135 = ORIENTED_EDGE ( 'NONE', *, *, #12201, .T. ) ;
#47136 = FACE_OUTER_BOUND ( 'NONE', #36790, .T. ) ;
#47137 = CARTESIAN_POINT ( 'NONE',  ( 0.1103310638050662013, -42.76619676553140437, 5.547176740492814950 ) ) ;
#47138 = CARTESIAN_POINT ( 'NONE',  ( 0.6845945791218034371, 21.77999332122215037, 41.54561844095550782 ) ) ;
#47139 = DIRECTION ( 'NONE',  ( -1.000000000000000000, -0.000000000000000000, -0.000000000000000000 ) ) ;
#47140 = B_SPLINE_CURVE_WITH_KNOTS ( 'NONE', 3,
 ( #12242, #26942, #31327, #16619, #6876, #50431, #44840, #41074, #46072, #3117, #22246, #52268, #55731, #8133, #60424, #46369 ),
 .UNSPECIFIED., .F., .F.,
 ( 4, 3, 3, 3, 3, 4 ),
 ( 8.674294979774126656E-18, 0.0002732102107931889696, 0.0004098135523333802871, 0.0005464168938824911191, 0.0008195847345945437689, 0.001092771384553109385 ),
 .UNSPECIFIED. ) ;
#47141 = CARTESIAN_POINT ( 'NONE',  ( 42.00000000000000711, 6.547216728259810428E-15, -1.617781153285278467E-30 ) ) ;
#47142 = CARTESIAN_POINT ( 'NONE',  ( 0.9757892942422807803, -42.53466646637867399, 5.651566539685677348 ) ) ;
#47143 =( BOUNDED_SURFACE ( )  B_SPLINE_SURFACE ( 3, 1, ( 
 ( #35063, #40091 ),
 ( #21255, #53511 ),
 ( #39773, #6497 ),
 ( #25638, #35373 ) ),
 .UNSPECIFIED., .F., .F., .F. ) 
 B_SPLINE_SURFACE_WITH_KNOTS ( ( 4, 4 ),
 ( 2, 2 ),
 ( 0.000000000000000000, 1.000000000000000000 ),
 ( 0.000000000000000000, 1.000000000000000000 ),
 .UNSPECIFIED. ) 
 GEOMETRIC_REPRESENTATION_ITEM ( )  RATIONAL_B_SPLINE_SURFACE ( (
 ( 1.000000000000000000, 1.000000000000000000),
 ( 0.9952954269826590483, 0.8620686068821307169),
 ( 0.9952954269826590483, 0.8620686068821307169),
 ( 1.000000000000000000, 1.000000000000000000) ) ) 
 REPRESENTATION_ITEM ( '' )  SURFACE ( )  );
#47144 = VECTOR ( 'NONE', #61438, 1000.000000000000000 ) ;
#47145 = CARTESIAN_POINT ( 'NONE',  ( 0.5807400328401574052, -28.72484455891667920, 38.33001520688939934 ) ) ;
#47146 = CARTESIAN_POINT ( 'NONE',  ( 5.917102823773431552, 3.353685953999792968, -19.83034312798663024 ) ) ;
#47147 = B_SPLINE_CURVE_WITH_KNOTS ( 'NONE', 3,
 ( #33836, #52599, #10320, #1210 ),
 .UNSPECIFIED., .F., .F.,
 ( 4, 4 ),
 ( 6.254634441385501517E-18, 0.004566006591234643766 ),
 .UNSPECIFIED. ) ;
#47148 = CARTESIAN_POINT ( 'NONE',  ( -6.001507490154111224, 2.475062734132707387, -18.68062548815622748 ) ) ;
#47149 = B_SPLINE_CURVE_WITH_KNOTS ( 'NONE', 3,
 ( #57614, #57014, #43266, #299 ),
 .UNSPECIFIED., .F., .F.,
 ( 4, 4 ),
 ( 0.000000000000000000, 0.005004948556313799229 ),
 .UNSPECIFIED. ) ;
#47150 = CARTESIAN_POINT ( 'NONE',  ( 4.967162193818131399, -23.56777426397203357, 36.06913038482792189 ) ) ;
#47151 = EDGE_LOOP ( 'NONE', ( #37393, #37811, #22601, #16791 ) ) ;
#47152 = DIRECTION ( 'NONE',  ( 1.000000000000000000, 0.000000000000000000, 0.000000000000000000 ) ) ;
#47153 = CARTESIAN_POINT ( 'NONE',  ( 5.000000000000007994, -56.56854249492331377, -56.56854249492430142 ) ) ;
#47154 = FACE_OUTER_BOUND ( 'NONE', #4392, .T. ) ;
#47155 = CARTESIAN_POINT ( 'NONE',  ( 0.6026777506516367566, -39.45935355539368317, -29.23193130170600540 ) ) ;
#47156 = CARTESIAN_POINT ( 'NONE',  ( 2.879087469061463178, -24.27289634831959475, -36.70052015499387466 ) ) ;
#47157 = CARTESIAN_POINT ( 'NONE',  ( 0.1103878639767399278, 42.76182653383950338, 5.580746265797182026 ) ) ;
#47158 = CONTEXT_DEPENDENT_SHAPE_REPRESENTATION ( #58360, #28834 ) ;
#47159 = CARTESIAN_POINT ( 'NONE',  ( 4.975801465491695552, -21.70134120755170315, -42.71626295676257001 ) ) ;
#47160 = EDGE_CURVE ( 'NONE', #46104, #5234, #17747, .T. ) ;
#47161 = CARTESIAN_POINT ( 'NONE',  ( 2.282803330402963571, -44.78788971279550424, 14.16127969257910912 ) ) ;
#47162 = CARTESIAN_POINT ( 'NONE',  ( 4.975801465491695552, 0.000000000000000000, 0.000000000000000000 ) ) ;
#47164 = EDGE_LOOP ( 'NONE', ( #43976, #39573, #46888, #14399 ) ) ;
#47163 = CARTESIAN_POINT ( 'NONE',  ( 0.8557997880470599172, 33.22501220301901270, 34.51495345639560952 ) ) ;
#47165 = VERTEX_POINT ( 'NONE', #1875 ) ;
#47166 = CARTESIAN_POINT ( 'NONE',  ( 0.1145239942831223490, -7.364426063610032713, 43.50529518872725987 ) ) ;
#47167 = FACE_OUTER_BOUND ( 'NONE', #19104, .T. ) ;
#47168 = CARTESIAN_POINT ( 'NONE',  ( 0.5809828226811617480, 17.82437196699680726, 44.45562576850608139 ) ) ;
#47169 = ORIENTED_EDGE ( 'NONE', *, *, #41295, .F. ) ;
#47170 = CARTESIAN_POINT ( 'NONE',  ( 0.6008122571543326185, 10.50252207146543704, -47.97136208826780290 ) ) ;
#47171 = CARTESIAN_POINT ( 'NONE',  ( 0.1129192098497455998, 9.345467776858411568, 43.12324222292260600 ) ) ;
#47172 = CARTESIAN_POINT ( 'NONE',  ( 0.5998501479064699549, -44.64337787626236320, -17.92509395669093308 ) ) ;
#47173 = ORIENTED_EDGE ( 'NONE', *, *, #56558, .T. ) ;
#47174 = VERTEX_POINT ( 'NONE', #35424 ) ;
#47175 = CARTESIAN_POINT ( 'NONE',  ( 0.9788927965476029724, 24.74514878889634062, -33.82327932130707637 ) ) ;
#47176 = CARTESIAN_POINT ( 'NONE',  ( 0.5997462898726536595, -20.35457962188166192, -44.69052157405179315 ) ) ;
#47177 = CARTESIAN_POINT ( 'NONE',  ( -6.016104459813371719, -18.20253432612963351, -4.871830707673248995 ) ) ;
#47178 = DIRECTION ( 'NONE',  ( -0.07439287786467652097, 0.7144194931003017279, 0.6957517427943097355 ) ) ;
#47179 = CARTESIAN_POINT ( 'NONE',  ( 4.962356264823601926, -41.76635909427990612, -5.177532797579353918 ) ) ;
#47180 = B_SPLINE_CURVE_WITH_KNOTS ( 'NONE', 3,
 ( #39189, #24755, #43271, #43899 ),
 .UNSPECIFIED., .F., .F.,
 ( 4, 4 ),
 ( 6.992893892674702526E-18, 0.004050076154992999881 ),
 .UNSPECIFIED. ) ;
#47181 = AXIS2_PLACEMENT_3D ( 'NONE', #24631, #43770, #813 ) ;
#47182 = DIRECTION ( 'NONE',  ( 1.000000000000000000, -0.000000000000000000, -0.000000000000000000 ) ) ;
#47183 = EDGE_CURVE ( 'NONE', #42042, #61015, #25456, .T. ) ;
#47184 = CARTESIAN_POINT ( 'NONE',  ( 0.1147471544378676350, 33.79869711786884778, 28.36547657995207317 ) ) ;
#47185 = EDGE_CURVE ( 'NONE', #4962, #17422, #12070, .T. ) ;
#47186 = VERTEX_POINT ( 'NONE', #39517 ) ;
#47187 = CARTESIAN_POINT ( 'NONE',  ( 0.9722240750034581991, 15.88116978453036054, -39.86121765932383454 ) ) ;
#47188 =( NAMED_UNIT ( * ) SI_UNIT ( $, .STERADIAN. ) SOLID_ANGLE_UNIT ( ) );
#47189 = ORIENTED_EDGE ( 'NONE', *, *, #52505, .F. ) ;
#47190 = CARTESIAN_POINT ( 'NONE',  ( 0.1129192098497455998, 42.02659449688937343, -13.44310763101974260 ) ) ;
#47191 = FACE_OUTER_BOUND ( 'NONE', #47164, .T. ) ;
#47192 = EDGE_CURVE ( 'NONE', #54683, #28511, #30670, .T. ) ;
#47193 = CARTESIAN_POINT ( 'NONE',  ( 0.9785694773339257413, 4.416269084231816855, -41.67531611266228708 ) ) ;
#47194 = DIRECTION ( 'NONE',  ( 0.9990097760809873995, 0.000000000000000000, -0.04449120468829072944 ) ) ;
#47195 = EDGE_LOOP ( 'NONE', ( #38447, #9022, #7233, #36819 ) ) ;
#47196 = ORIENTED_EDGE ( 'NONE', *, *, #1344, .T. ) ;
#47197 = CARTESIAN_POINT ( 'NONE',  ( 0.8751705887134423323, -38.69254731947852832, 28.56654290188588163 ) ) ;
#47198 = B_SPLINE_CURVE_WITH_KNOTS ( 'NONE', 3,
 ( #19426, #53526, #4662, #33845, #9389, #10641, #52921, #28491, #24113, #29118, #23811, #5897, #42939, #26939, #2764, #30044, #45104, #7140, #30347 ),
 .UNSPECIFIED., .F., .F.,
 ( 4, 3, 3, 3, 3, 3, 4 ),
 ( 1.149162571898268292E-16, 0.0002618519381806242905, 0.0003927759815485966258, 0.0005237000248299457069, 0.0006546240681324996683, 0.0007855481115631327092, 0.0009699050456655109419 ),
 .UNSPECIFIED. ) ;
#47199 = VERTEX_POINT ( 'NONE', #1560 ) ;
#47200 = CARTESIAN_POINT ( 'NONE',  ( 0.6021447746440204973, 4.455320864211258503, -48.90492056107863306 ) ) ;
#47201 = ORIENTED_EDGE ( 'NONE', *, *, #23460, .F. ) ;
#47202 = CARTESIAN_POINT ( 'NONE',  ( 0.9968887458511638267, -4.948372828380487753, -42.62316256128688963 ) ) ;
#47203 = LINE ( 'NONE', #23084, #33466 ) ;
#47204 = ADVANCED_FACE ( 'NONE', ( #20694 ), #33774, .T. ) ;
#47205 = VERTEX_POINT ( 'NONE', #43808 ) ;
#47206 = CARTESIAN_POINT ( 'NONE',  ( 0.5832367798473397924, -0.2724222379463806520, 47.89515946578896433 ) ) ;
#47207 = CARTESIAN_POINT ( 'NONE',  ( 3.782542959838397501, 13.48688832728106846, 39.81634961475020162 ) ) ;
#47208 = ADVANCED_FACE ( 'NONE', ( #29054 ), #53156, .F. ) ;
#47209 = CARTESIAN_POINT ( 'NONE',  ( 0.9756008150404607004, 26.00810955565563631, -34.12792951168081146 ) ) ;
#47210 = CARTESIAN_POINT ( 'NONE',  ( 4.963659409799326738, -13.93274247731990911, -42.53037318521008814 ) ) ;
#47211 = CARTESIAN_POINT ( 'NONE',  ( 1.830465331921978800, -42.90550687857155054, 9.974644623806854682 ) ) ;
#47212 = CARTESIAN_POINT ( 'NONE',  ( 0.2885700199627515561, 26.88157179738457714, 33.71073713194529375 ) ) ;
#47213 = CARTESIAN_POINT ( 'NONE',  ( 0.6028618097248864549, 47.67286800277443604, -6.452328974163124009 ) ) ;
#47214 = CARTESIAN_POINT ( 'NONE',  ( 0.7056759521544957448, 36.27980703839233456, 29.72413884999874156 ) ) ;
#47215 = ORIENTED_EDGE ( 'NONE', *, *, #6926, .T. ) ;
#47216 = CARTESIAN_POINT ( 'NONE',  ( 0.5806925824938502512, -24.77160101449099727, 39.81946942793729249 ) ) ;
#47217 =( BOUNDED_SURFACE ( )  B_SPLINE_SURFACE ( 3, 1, ( 
 ( #21742, #35858 ),
 ( #45567, #50857 ),
 ( #50544, #27060 ),
 ( #40569, #2620 ) ),
 .UNSPECIFIED., .F., .F., .F. ) 
 B_SPLINE_SURFACE_WITH_KNOTS ( ( 4, 4 ),
 ( 2, 2 ),
 ( 0.000000000000000000, 1.000000000000000000 ),
 ( 0.000000000000000000, 1.000000000000000000 ),
 .UNSPECIFIED. ) 
 GEOMETRIC_REPRESENTATION_ITEM ( )  RATIONAL_B_SPLINE_SURFACE ( (
 ( 1.000000000000000000, 1.000000000000000000),
 ( 0.9953040768229013402, 0.8617119497784988535),
 ( 0.9953040768229013402, 0.8617119497784988535),
 ( 1.000000000000000000, 1.000000000000000000) ) ) 
 REPRESENTATION_ITEM ( '' )  SURFACE ( )  );
#47218 = CARTESIAN_POINT ( 'NONE',  ( 4.549368137175248350, 35.80950303116068056, 23.67244292351653101 ) ) ;
#47219 = ORIENTED_EDGE ( 'NONE', *, *, #17289, .F. ) ;
#47220 = DIRECTION ( 'NONE',  ( 0.09835009131224567436, -0.7847759187265501701, -0.6119264800004754479 ) ) ;
#47221 = CARTESIAN_POINT ( 'NONE',  ( 4.960156602257180580, -38.31207700265935756, -26.21519897043469172 ) ) ;
#47222 = CARTESIAN_POINT ( 'NONE',  ( 4.967162193818131399, 18.65818244221258126, 38.83676580803773248 ) ) ;
#47223 = CARTESIAN_POINT ( 'NONE',  ( 0.9745511491811756910, 5.938142320543945196, -42.49552597049449787 ) ) ;
#47224 = CARTESIAN_POINT ( 'NONE',  ( -6.057079549204054558, 5.487289185789351542, 18.45862639773766389 ) ) ;
#47225 = CARTESIAN_POINT ( 'NONE',  ( 0.9730545539215883499, 37.40983423658472873, 21.01499094264562473 ) ) ;
#47226 =( GEOMETRIC_REPRESENTATION_CONTEXT ( 3 ) GLOBAL_UNCERTAINTY_ASSIGNED_CONTEXT ( ( #21735 ) ) GLOBAL_UNIT_ASSIGNED_CONTEXT ( ( #11246, #7441, #6502 ) ) REPRESENTATION_CONTEXT ( 'NONE', 'WORKASPACE' ) );
#47227 = CARTESIAN_POINT ( 'NONE',  ( 0.5819845901640485764, -47.89381229371849003, -0.4540519722835836269 ) ) ;
#47228 = CARTESIAN_POINT ( 'NONE',  ( -5.438558936750501616, -0.4863491397211875955, -0.7223290250795360024 ) ) ;
#47229 = CARTESIAN_POINT ( 'NONE',  ( 0.6017667736363750963, 47.64919355032679249, 6.625250263233795067 ) ) ;
#47230 = AXIS2_PLACEMENT_3D ( 'NONE', #58156, #15277, #209 ) ;
#47231 = EDGE_CURVE ( 'NONE', #46482, #47052, #56854, .T. ) ;
#47232 = CARTESIAN_POINT ( 'NONE',  ( 4.553261556744875094, 38.38432632180499837, -21.35844232721162683 ) ) ;
#47233 = CARTESIAN_POINT ( 'NONE',  ( 0.5804410086790514622, 43.38796872094602008, 17.80460676694675826 ) ) ;
#47234 = CARTESIAN_POINT ( 'NONE',  ( 4.834790513006553603, 43.96797211434409292, -17.30337449969347219 ) ) ;
#47235 = ORIENTED_EDGE ( 'NONE', *, *, #9954, .T. ) ;
#47236 = CARTESIAN_POINT ( 'NONE',  ( 0.8751705887134423323, 28.56654290188602019, 38.69254731947842885 ) ) ;
#47237 = CARTESIAN_POINT ( 'NONE',  ( 5.965394784446458765, -2.664747781316264330, 20.35165389555753279 ) ) ;
#47238 = CARTESIAN_POINT ( 'NONE',  ( 2.648799415243708655, -6.455064903436325885, 48.60915140569751713 ) ) ;
#47239 = CARTESIAN_POINT ( 'NONE',  ( 0.5809828226811553087, -47.89273459658654275, 0.5448590168530708100 ) ) ;
#47240 = CARTESIAN_POINT ( 'NONE',  ( 0.6254087463353918963, -42.00124903776053031, -23.45485308995585072 ) ) ;
#47241 = ORIENTED_EDGE ( 'NONE', *, *, #22745, .T. ) ;
#47242 = DIRECTION ( 'NONE',  ( 1.000000000000000000, 0.000000000000000000, 0.000000000000000000 ) ) ;
#47243 = CARTESIAN_POINT ( 'NONE',  ( 0.8554163680231738898, 27.08908797599145046, 38.30648490452777821 ) ) ;
#47244 = CARTESIAN_POINT ( 'NONE',  ( -20.06020393719607142, -7.996425831208540558, 0.2746589711620047169 ) ) ;
#47245 = VERTEX_POINT ( 'NONE', #15278 ) ;
#47246 = CARTESIAN_POINT ( 'NONE',  ( -6.078726893082806448, -12.94836301907752585, 14.25250631976375004 ) ) ;
#47247 = DIRECTION ( 'NONE',  ( -1.000000000000000000, -0.000000000000000000, -0.000000000000000000 ) ) ;
#47248 = ORIENTED_EDGE ( 'NONE', *, *, #51071, .F. ) ;
#47249 = CARTESIAN_POINT ( 'NONE',  ( 1.657374760986086049, -26.48956948988313087, 35.20217543693708251 ) ) ;
#47250 = ADVANCED_FACE ( 'NONE', ( #52227 ), #48777, .T. ) ;
#47251 = VERTEX_POINT ( 'NONE', #23742 ) ;
#47252 = B_SPLINE_CURVE_WITH_KNOTS ( 'NONE', 3,
 ( #29231, #18616, #13613, #52107 ),
 .UNSPECIFIED., .F., .F.,
 ( 4, 4 ),
 ( 0.000000000000000000, 0.004445488388166994251 ),
 .UNSPECIFIED. ) ;
#47253 = CARTESIAN_POINT ( 'NONE',  ( 51.67657445772706382, 15.31620728304649326, -2.380828478538471238 ) ) ;
#47254 = CARTESIAN_POINT ( 'NONE',  ( 0.5987334308729320709, 17.52678517438131678, 45.87346409440667117 ) ) ;
#47255 = ORIENTED_EDGE ( 'NONE', *, *, #8687, .F. ) ;
#47256 = CARTESIAN_POINT ( 'NONE',  ( 4.958415959904820092, 29.71032706691326908, -34.35841118852379594 ) ) ;
#47257 = CARTESIAN_POINT ( 'NONE',  ( 0.1103878639767399278, 26.29099398937401588, 34.18336104662747488 ) ) ;
#47258 = EDGE_CURVE ( 'NONE', #39651, #22299, #10265, .T. ) ;
#47259 = CARTESIAN_POINT ( 'NONE',  ( 0.5987334308729317378, -43.08218175136362049, -23.56880400258363650 ) ) ;
#47260 = CARTESIAN_POINT ( 'NONE',  ( 3.238741278300274917, 23.06029422819004182, -36.28414388564873150 ) ) ;
#47261 =( REPRESENTATION_RELATIONSHIP ('NONE','NONE', #44881, #40484 ) REPRESENTATION_RELATIONSHIP_WITH_TRANSFORMATION ( #52441 )SHAPE_REPRESENTATION_RELATIONSHIP( ) );
#47262 = VECTOR ( 'NONE', #5660, 1000.000000000000114 ) ;
#47263 = EDGE_LOOP ( 'NONE', ( #14235, #32006, #2867, #14292 ) ) ;
#47264 = CARTESIAN_POINT ( 'NONE',  ( 0.9784957157296357844, -7.200058621843461459, -41.28549639806200844 ) ) ;
#47265 = EDGE_CURVE ( 'NONE', #8115, #35714, #31455, .T. ) ;
#47266 = ORIENTED_EDGE ( 'NONE', *, *, #39779, .F. ) ;
#47267 = CARTESIAN_POINT ( 'NONE',  ( 2.648799415243696664, -45.95403142182595246, 17.10977671892392493 ) ) ;
#47268 = CIRCLE ( 'NONE', #31251, 47.09074272231896430 ) ;
#47269 = ORIENTED_EDGE ( 'NONE', *, *, #21371, .T. ) ;
#47270 = VERTEX_POINT ( 'NONE', #58157 ) ;
#47271 = CARTESIAN_POINT ( 'NONE',  ( 0.6029442701453591180, -42.83094826596455107, -24.02197110556389603 ) ) ;
#47272 = CARTESIAN_POINT ( 'NONE',  ( 5.960221823109900008, -18.96108896995720983, 7.859839668734879048 ) ) ;
#47273 = CARTESIAN_POINT ( 'NONE',  ( 0.1073791018717578927, 5.147744207006301309, 42.81622261970996135 ) ) ;
#47274 = CARTESIAN_POINT ( 'NONE',  ( 1.112077966505211180, -28.29638438491135943, -33.79859399250062069 ) ) ;
#47275 = ORIENTED_EDGE ( 'NONE', *, *, #22362, .T. ) ;
#47276 = CARTESIAN_POINT ( 'NONE',  ( -5.995132425357893702, -7.203480333238950095, -17.41298668506978231 ) ) ;
#47277 = EDGE_CURVE ( 'NONE', #54460, #59959, #42869, .T. ) ;
#47278 = DIRECTION ( 'NONE',  ( 1.000000000000000000, 0.000000000000000000, 0.000000000000000000 ) ) ;
#47279 = ORIENTED_EDGE ( 'NONE', *, *, #57680, .F. ) ;
#47280 = VERTEX_POINT ( 'NONE', #24050 ) ;
#47281 = DIRECTION ( 'NONE',  ( -1.000000000000000000, -0.000000000000000000, -0.000000000000000000 ) ) ;
#47282 = CARTESIAN_POINT ( 'NONE',  ( 0.8551540677456739292, 46.03951182599426772, 13.28067116677217641 ) ) ;
#47283 = CARTESIAN_POINT ( 'NONE',  ( 2.648799415243708655, 29.17954675436460121, 39.40902833741842670 ) ) ;
#47284 = CARTESIAN_POINT ( 'NONE',  ( 0.1064266418746775827, -42.67882141624140502, -6.185136754498182121 ) ) ;
#47285 = CARTESIAN_POINT ( 'NONE',  ( 0.5786265663353196143, -29.72999788434318802, 37.55861529268543109 ) ) ;
#47286 = ORIENTED_EDGE ( 'NONE', *, *, #31249, .F. ) ;
#47287 = CARTESIAN_POINT ( 'NONE',  ( 4.975801465491695552, -14.85979367497206205, 45.55012473237727733 ) ) ;
#47288 = CARTESIAN_POINT ( 'NONE',  ( 48.50459710310596506, 15.40111741581167593, 1.752346893213588386 ) ) ;
#47289 = CARTESIAN_POINT ( 'NONE',  ( 0.7413678028165011646, -38.87127836507679746, -20.82089839644190121 ) ) ;
#47290 = CARTESIAN_POINT ( 'NONE',  ( 0.3676999524040366896, -43.63756228305280160, 6.458617600967457406 ) ) ;
#47291 =( NAMED_UNIT ( * ) SI_UNIT ( $, .STERADIAN. ) SOLID_ANGLE_UNIT ( ) );
#47292 = CARTESIAN_POINT ( 'NONE',  ( 5.860006189529234355, -45.66786516969939669, 15.52021937683260511 ) ) ;
#47293 = ORIENTED_EDGE ( 'NONE', *, *, #12396, .T. ) ;
#47294 = CARTESIAN_POINT ( 'NONE',  ( 5.860006189529246790, 3.137522369585520998, 48.13093674595586435 ) ) ;
#47295 = CARTESIAN_POINT ( 'NONE',  ( 4.553261556744873317, 38.16266689001211887, -21.75202109381124771 ) ) ;
#47296 = CARTESIAN_POINT ( 'NONE',  ( 3.661933894777869902, -9.674350085358240037, 46.03301114827903717 ) ) ;
#47297 = CARTESIAN_POINT ( 'NONE',  ( 5.719999999999997087, 6.938893903907228378E-15, 0.000000000000000000 ) ) ;
#47298 = CARTESIAN_POINT ( 'NONE',  ( 5.860006189529246790, 21.31760477694582789, 43.26650951066876161 ) ) ;
#47299 = EDGE_CURVE ( 'NONE', #57072, #44468, #52294, .T. ) ;
#47300 = CARTESIAN_POINT ( 'NONE',  ( 4.975801465491694664, -39.51822597168476392, -27.09127437476367106 ) ) ;
#47301 = DIRECTION ( 'NONE',  ( 0.000000000000000000, 0.000000000000000000, 1.000000000000000000 ) ) ;
#47302 = B_SPLINE_CURVE_WITH_KNOTS ( 'NONE', 3,
 ( #2680, #50602, #45327, #2990 ),
 .UNSPECIFIED., .F., .F.,
 ( 4, 4 ),
 ( 0.000000000000000000, 0.004048833967417082152 ),
 .UNSPECIFIED. ) ;
#47303 = VECTOR ( 'NONE', #14590, 1000.000000000000000 ) ;
#47304 = CARTESIAN_POINT ( 'NONE',  ( 0.5835871038041858805, 22.65703148838214176, -41.05963196420492523 ) ) ;
#47305 = ADVANCED_FACE ( 'NONE', ( #14354 ), #22162, .F. ) ;
#47306 =( BOUNDED_SURFACE ( )  B_SPLINE_SURFACE ( 3, 1, ( 
 ( #3153, #23498 ),
 ( #42627, #32605 ),
 ( #28195, #32924 ),
 ( #61688, #28497 ) ),
 .UNSPECIFIED., .F., .F., .F. ) 
 B_SPLINE_SURFACE_WITH_KNOTS ( ( 4, 4 ),
 ( 2, 2 ),
 ( 0.000000000000000000, 1.000000000000000000 ),
 ( 0.000000000000000000, 1.000000000000000000 ),
 .UNSPECIFIED. ) 
 GEOMETRIC_REPRESENTATION_ITEM ( )  RATIONAL_B_SPLINE_SURFACE ( (
 ( 1.000000000000000000, 1.000000000000000000),
 ( 0.9952954269826590483, 0.8620686068821307169),
 ( 0.9952954269826590483, 0.8620686068821307169),
 ( 1.000000000000000000, 1.000000000000000000) ) ) 
 REPRESENTATION_ITEM ( '' )  SURFACE ( )  );
#47307 = EDGE_CURVE ( 'NONE', #37486, #49553, #3050, .T. ) ;
#47308 = CARTESIAN_POINT ( 'NONE',  ( 4.291220156522059348, 31.16808953869599463, 35.32618280841457192 ) ) ;
#47309 = ORIENTED_EDGE ( 'NONE', *, *, #21420, .F. ) ;
#47310 = DIRECTION ( 'NONE',  ( 0.000000000000000000, 0.000000000000000000, 1.000000000000000000 ) ) ;
#47311 = CARTESIAN_POINT ( 'NONE',  ( 3.390910168358337362, 23.51971099678612021, -37.16073641844702280 ) ) ;
#47312 = CARTESIAN_POINT ( 'NONE',  ( 0.7048096507298635682, 13.26491767067451200, 46.24547838151373469 ) ) ;
#47313 = DIRECTION ( 'NONE',  ( 0.000000000000000000, 0.000000000000000000, -1.000000000000000000 ) ) ;
#47314 = ORIENTED_EDGE ( 'NONE', *, *, #23346, .F. ) ;
#47315 = CARTESIAN_POINT ( 'NONE',  ( 0.5980271706414734822, -13.30134363210459369, 47.27709276618364953 ) ) ;
#47316 = CARTESIAN_POINT ( 'NONE',  ( 4.975610109902397937, 0.000000000000000000, 0.000000000000000000 ) ) ;
#47317 = B_SPLINE_CURVE_WITH_KNOTS ( 'NONE', 3,
 ( #20104, #20711, #15404, #39851, #16021, #25714 ),
 .UNSPECIFIED., .F., .F.,
 ( 4, 2, 4 ),
 ( 7.757919228897728493E-18, 0.0002291472222819924205, 0.0004582944445639770890 ),
 .UNSPECIFIED. ) ;
#47318 = ORIENTED_EDGE ( 'NONE', *, *, #3639, .T. ) ;
#47319 = CARTESIAN_POINT ( 'NONE',  ( 0.1147471544378677322, 3.927779167740302668, -43.94911534129795427 ) ) ;
#47320 = CIRCLE ( 'NONE', #26297, 2.649999999999997691 ) ;
#47321 = CARTESIAN_POINT ( 'NONE',  ( 0.9762797500689124330, 24.45014227842982635, 34.03697001423955726 ) ) ;
#47322 = DIRECTION ( 'NONE',  ( 8.032841876251139751E-16, -4.551914400963141816E-15, 1.000000000000000000 ) ) ;
#47323 = EDGE_CURVE ( 'NONE', #35039, #47174, #52540, .T. ) ;
#47324 = ORIENTED_EDGE ( 'NONE', *, *, #51546, .T. ) ;
#47325 = ORIENTED_EDGE ( 'NONE', *, *, #42852, .F. ) ;
#47327 = ORIENTED_EDGE ( 'NONE', *, *, #47624, .F. ) ;
#47326 = EDGE_CURVE ( 'NONE', #23299, #28349, #61756, .T. ) ;
#47328 = CARTESIAN_POINT ( 'NONE',  ( 1.157644175074337367, -6.156433857109804286, -41.46203803049500181 ) ) ;
#47329 = CARTESIAN_POINT ( 'NONE',  ( -6.078726893082806448, 19.09835798914753369, -2.459016752095146252 ) ) ;
#47330 = ORIENTED_EDGE ( 'NONE', *, *, #45962, .T. ) ;
#47331 = CARTESIAN_POINT ( 'NONE',  ( 0.8551540677456715978, -47.90804413217341562, 0.9122407826474140391 ) ) ;
#47332 = VERTEX_POINT ( 'NONE', #9633 ) ;
#47333 = CARTESIAN_POINT ( 'NONE',  ( 0.5832366564991502411, 0.2724446024277419331, 47.89515933308369000 ) ) ;
#47334 = EDGE_CURVE ( 'NONE', #4156, #55418, #53457, .T. ) ;
#47335 = CARTESIAN_POINT ( 'NONE',  ( 3.238741278300274917, 42.82436441900173207, -3.793425828152205970 ) ) ;
#47336 = CARTESIAN_POINT ( 'NONE',  ( 5.896782393890504181, -7.234636363571307349, -18.76662259344776018 ) ) ;
#47337 = ORIENTED_EDGE ( 'NONE', *, *, #5891, .F. ) ;
#47338 = CARTESIAN_POINT ( 'NONE',  ( 0.9757787079277443487, -16.38386580718262664, -39.65734351318521078 ) ) ;
#47339 = CARTESIAN_POINT ( 'NONE',  ( 4.291220156522060236, -45.68901888636798247, 11.48488356522638654 ) ) ;
#47340 = CARTESIAN_POINT ( 'NONE',  ( 4.909518593422035337, 0.8656805902944597619, 8.896908036367455278E-17 ) ) ;
#47341 = DIRECTION ( 'NONE',  ( 1.000000000000000000, 1.836909530733573776E-16, 0.000000000000000000 ) ) ;
#47342 = ORIENTED_EDGE ( 'NONE', *, *, #44099, .F. ) ;
#47343 = CARTESIAN_POINT ( 'NONE',  ( 0.8551540677456715978, 13.28067116677202364, 46.03951182599431746 ) ) ;
#47344 = EDGE_CURVE ( 'NONE', #12652, #24696, #10571, .T. ) ;
#47345 = CARTESIAN_POINT ( 'NONE',  ( 4.691466044806103852, -33.30232861642453202, 29.64918311951070606 ) ) ;
#47346 = ORIENTED_EDGE ( 'NONE', *, *, #212, .T. ) ;
#47347 = CIRCLE ( 'NONE', #11310, 15.43999999999999240 ) ;
#47348 = FACE_OUTER_BOUND ( 'NONE', #30584, .T. ) ;
#47349 = ORIENTED_EDGE ( 'NONE', *, *, #39792, .T. ) ;
#47350 = LINE ( 'NONE', #10064, #53498 ) ;
#47351 = CARTESIAN_POINT ( 'NONE',  ( 0.6016118706126976079, 46.71438999114540991, -15.14321044359830992 ) ) ;
#47352 = ORIENTED_EDGE ( 'NONE', *, *, #37861, .T. ) ;
#47353 = CARTESIAN_POINT ( 'NONE',  ( 0.9780106845699469975, -34.37272748497746733, -23.97596404107485668 ) ) ;
#47354 = CARTESIAN_POINT ( 'NONE',  ( 0.6000166863083106206, 49.04012132094737808, -2.624877622902994201 ) ) ;
#47355 = CARTESIAN_POINT ( 'NONE',  ( 0.8560838555295158248, 46.60258007729424889, -5.345312359545362213 ) ) ;
#47356 = CARTESIAN_POINT ( 'NONE',  ( 0.6000166863083106206, 46.44114019838995944, -15.97009639238106438 ) ) ;
#47357 = EDGE_LOOP ( 'NONE', ( #61286, #50308, #57025, #43058 ) ) ;
#47358 = CARTESIAN_POINT ( 'NONE',  ( 4.975610109902397937, -48.77192499014908833, -3.707929326867496655 ) ) ;
#47359 = CARTESIAN_POINT ( 'NONE',  ( 5.895596859100789899, -20.11288567981415909, 0.003583743010676890273 ) ) ;
#47360 = CARTESIAN_POINT ( 'NONE',  ( 4.975801465491694664, -20.67815041659109809, -43.22084481528213473 ) ) ;
#47361 = AXIS2_PLACEMENT_3D ( 'NONE', #42856, #33450, #24341 ) ;
#47362 = CARTESIAN_POINT ( 'NONE',  ( 5.896278296736517710, 20.06757494133108466, -1.348857141599696829 ) ) ;
#47363 = FACE_OUTER_BOUND ( 'NONE', #57694, .T. ) ;
#47364 = CARTESIAN_POINT ( 'NONE',  ( 0.000000000000000000, 0.000000000000000000, -25.03750572909317285 ) ) ;
#47365 = DIRECTION ( 'NONE',  ( -0.9848077530122077983, -0.1736481776669316079, 1.387778780781445367E-17 ) ) ;
#47366 = CARTESIAN_POINT ( 'NONE',  ( 0.5837157313716030416, 40.39573142367531489, -23.82062019193272917 ) ) ;
#47367 = DIRECTION ( 'NONE',  ( -0.07906939808003035641, 0.3507354328807477106, -0.9331305837926522351 ) ) ;
#47368 = EDGE_CURVE ( 'NONE', #3337, #32695, #46834, .T. ) ;
#47369 = CARTESIAN_POINT ( 'NONE',  ( 0.3622758884714600280, -29.89648521331609743, -31.06363466427717412 ) ) ;
#47370 = CARTESIAN_POINT ( 'NONE',  ( 0.5804410086790514622, 42.96136033320072301, -18.81067170986420223 ) ) ;
#47371 = CARTESIAN_POINT ( 'NONE',  ( 1.088313998177381503, -34.51470853099735336, 25.50107284445300948 ) ) ;
#47372 = DIRECTION ( 'NONE',  ( 0.1011922191286468153, 0.9935638751191105955, 0.05090148176739390379 ) ) ;
#47374 = ADVANCED_FACE ( 'NONE', ( #59507 ), #8132, .F. ) ;
#47373 = CARTESIAN_POINT ( 'NONE',  ( 3.390910168358336474, -21.09049067108720621, 38.59129875744557125 ) ) ;
#47375 = CARTESIAN_POINT ( 'NONE',  ( 0.6001305935487315502, -41.40054608060276564, -24.50730504006443411 ) ) ;
#47376 = EDGE_CURVE ( 'NONE', #42648, #5378, #7466, .T. ) ;
#47378 =( BOUNDED_SURFACE ( )  B_SPLINE_SURFACE ( 3, 1, ( 
 ( #7232, #16347 ),
 ( #40807, #59867 ),
 ( #45196, #44885 ),
 ( #31376, #26669 ) ),
 .UNSPECIFIED., .F., .F., .F. ) 
 B_SPLINE_SURFACE_WITH_KNOTS ( ( 4, 4 ),
 ( 2, 2 ),
 ( 0.000000000000000000, 1.000000000000000000 ),
 ( 0.000000000000000000, 1.000000000000000000 ),
 .UNSPECIFIED. ) 
 GEOMETRIC_REPRESENTATION_ITEM ( )  RATIONAL_B_SPLINE_SURFACE ( (
 ( 1.000000000000000000, 1.000000000000000000),
 ( 0.9732289882329797637, 0.9999525324661233672),
 ( 0.9732289882329797637, 0.9999525324661233672),
 ( 1.000000000000000000, 1.000000000000000000) ) ) 
 REPRESENTATION_ITEM ( '' )  SURFACE ( )  );
#47377 = CARTESIAN_POINT ( 'NONE',  ( 2.282816707992307848, -6.514472263567006927, 46.51944343535488002 ) ) ;
#47379 = DIRECTION ( 'NONE',  ( 0.000000000000000000, 0.000000000000000000, 1.000000000000000000 ) ) ;
#47380 = EDGE_CURVE ( 'NONE', #15373, #46397, #59071, .T. ) ;
#47382 = EDGE_LOOP ( 'NONE', ( #33109, #32680, #20100, #46788 ) ) ;
#47381 = DIRECTION ( 'NONE',  ( 0.000000000000000000, 0.000000000000000000, 1.000000000000000000 ) ) ;
#47383 = CARTESIAN_POINT ( 'NONE',  ( 0.6016117650947689910, -39.14611488887053525, 29.65017273730201453 ) ) ;
#47384 = CARTESIAN_POINT ( 'NONE',  ( 0.5832366564991492419, 24.18352361336827983, 41.34220239953996412 ) ) ;
#47385 = EDGE_CURVE ( 'NONE', #56877, #1638, #8252, .T. ) ;
#47386 = CARTESIAN_POINT ( 'NONE',  ( 2.618530812446111078, 3.301668998265828048, 46.89163860459656519 ) ) ;
#47387 = VERTEX_POINT ( 'NONE', #54808 ) ;
#47388 = CARTESIAN_POINT ( 'NONE',  ( 4.553261556744875094, -36.93702150832111641, 23.77385134801386712 ) ) ;
#47389 = CARTESIAN_POINT ( 'NONE',  ( 0.8551540677456715978, 37.45266983663536564, -29.88829867897776893 ) ) ;
#47390 = AXIS2_PLACEMENT_3D ( 'NONE', #44850, #11308, #25711 ) ;
#47391 = UNCERTAINTY_MEASURE_WITH_UNIT (LENGTH_MEASURE( 1.000000000000000082E-05 ), #10315, 'distance_accuracy_value', 'NONE');
#47392 = ORIENTED_EDGE ( 'NONE', *, *, #31753, .T. ) ;
#47393 = VERTEX_POINT ( 'NONE', #36661 ) ;
#47394 = ADVANCED_FACE ( 'NONE', ( #30698 ), #11361, .F. ) ;
#47395 = DIRECTION ( 'NONE',  ( 1.000000000000000000, 0.000000000000000000, 0.000000000000000000 ) ) ;
#47396 = EDGE_CURVE ( 'NONE', #15197, #96, #56808, .T. ) ;
#47397 = ORIENTED_EDGE ( 'NONE', *, *, #13547, .T. ) ;
#47398 = CARTESIAN_POINT ( 'NONE',  ( -1.200000000000006617, 0.000000000000000000, 0.000000000000000000 ) ) ;
#47399 = CARTESIAN_POINT ( 'NONE',  ( 0.8554163680231816613, 27.08908797599198337, -38.30648490452740162 ) ) ;
#47400 = VERTEX_POINT ( 'NONE', #12862 ) ;
#47401 = ORIENTED_EDGE ( 'NONE', *, *, #24867, .F. ) ;
#47402 = CARTESIAN_POINT ( 'NONE',  ( 0.5827359174754830340, -12.04517879102104416, -46.35666395585283794 ) ) ;
#47403 = ORIENTED_EDGE ( 'NONE', *, *, #61810, .F. ) ;
#47404 = CARTESIAN_POINT ( 'NONE',  ( 0.3676999524040323597, -23.56959980820351674, 37.28839696479283106 ) ) ;
#47405 = CARTESIAN_POINT ( 'NONE',  ( 4.962356264823608143, 37.36413190407361640, 19.36897635181929545 ) ) ;
#47406 = B_SPLINE_CURVE_WITH_KNOTS ( 'NONE', 3,
 ( #891, #25022, #24709, #40376, #11232, #35670 ),
 .UNSPECIFIED., .F., .F.,
 ( 4, 2, 4 ),
 ( 1.951563910473907981E-18, 0.0002447193893791709007, 0.0004894387787583398498 ),
 .UNSPECIFIED. ) ;
#47407 = CIRCLE ( 'NONE', #2354, 15.14599999999999369 ) ;
#47408 = CARTESIAN_POINT ( 'NONE',  ( 0.1095718737110178698, -30.31138510522973561, -30.67477146794362497 ) ) ;
#47409 = ORIENTED_EDGE ( 'NONE', *, *, #36380, .T. ) ;
#47410 = CARTESIAN_POINT ( 'NONE',  ( 0.1119898979215349921, -7.595749101251602298, -43.46568651065648226 ) ) ;
#47411 = CARTESIAN_POINT ( 'NONE',  ( 0.9741495583595178864, -33.79932324264165544, -26.43366215195294444 ) ) ;
#47412 = ORIENTED_EDGE ( 'NONE', *, *, #61718, .T. ) ;
#47413 = VERTEX_POINT ( 'NONE', #17239 ) ;
#47414 = FACE_OUTER_BOUND ( 'NONE', #1418, .T. ) ;
#47415 = B_SPLINE_CURVE_WITH_KNOTS ( 'NONE', 3,
 ( #938, #48258, #5001, #15369, #34474, #20070 ),
 .UNSPECIFIED., .F., .F.,
 ( 4, 2, 4 ),
 ( 4.878909776184769953E-19, 0.0002293801035737106731, 0.0004587602071474208582 ),
 .UNSPECIFIED. ) ;
#47416 = ORIENTED_EDGE ( 'NONE', *, *, #15789, .F. ) ;
#47417 = CARTESIAN_POINT ( 'NONE',  ( 0.6016117650947689910, 46.71439353012161178, 15.14319950860553732 ) ) ;
#47418 = CARTESIAN_POINT ( 'NONE',  ( -2.500000000000002220, 0.000000000000000000, -5.574599999999999334 ) ) ;
#47419 = CARTESIAN_POINT ( 'NONE',  ( 0.1098349054025746646, 5.417317591399238630, 42.78286259078964804 ) ) ;
#47420 = CARTESIAN_POINT ( 'NONE',  ( 0.3622758884714730732, 29.89648521331631414, -31.06363466427696807 ) ) ;
#47421 = EDGE_CURVE ( 'NONE', #43089, #15076, #13496, .T. ) ;
#47422 = EDGE_LOOP ( 'NONE', ( #30084, #43958, #22278, #51713 ) ) ;
#47423 = CARTESIAN_POINT ( 'NONE',  ( 3.407937589446178528, 4.815089211105230582, -12.82481284928199017 ) ) ;
#47424 = DIRECTION ( 'NONE',  ( 2.280301054154487250E-31, 0.000000000000000000, -1.000000000000000000 ) ) ;
#47425 = EDGE_CURVE ( 'NONE', #59171, #6735, #16618, .T. ) ;
#47426 = CARTESIAN_POINT ( 'NONE',  ( 0.5804410086790514622, -46.06497594411315077, 8.805557513506689915 ) ) ;
#47427 = ORIENTED_EDGE ( 'NONE', *, *, #52351, .T. ) ;
#47428 = CARTESIAN_POINT ( 'NONE',  ( 0.5809828226811553087, -38.32755012159125840, -28.72298383114528519 ) ) ;
#47429 = FACE_OUTER_BOUND ( 'NONE', #26987, .T. ) ;
#47430 = CARTESIAN_POINT ( 'NONE',  ( 0.7246131072078572100, 46.66866179549018057, -11.65529928397590531 ) ) ;
#47431 = VERTEX_POINT ( 'NONE', #31019 ) ;
#47432 = ORIENTED_EDGE ( 'NONE', *, *, #61415, .T. ) ;
#47433 = CARTESIAN_POINT ( 'NONE',  ( 0.1073791018717578927, -39.65380858626204486, -16.95003405440299460 ) ) ;
#47434 = CARTESIAN_POINT ( 'NONE',  ( 4.967162193818129623, 40.65506779172164897, 14.26841313271295952 ) ) ;
#47435 = CARTESIAN_POINT ( 'NONE',  ( 2.282816707992308736, -31.31875043000178493, -35.00903937429915658 ) ) ;
#47436 = CARTESIAN_POINT ( 'NONE',  ( 0.6064515330803547100, -41.53117911960045916, 21.78291754960180526 ) ) ;
#47437 = VECTOR ( 'NONE', #14040, 1000.000000000000000 ) ;
#47438 = CARTESIAN_POINT ( 'NONE',  ( 0.6064515330803561532, -20.38298978299800623, -42.23586229193488606 ) ) ;
#47439 = CARTESIAN_POINT ( 'NONE',  ( 1.500000000000001332, 0.000000000000000000, 0.000000000000000000 ) ) ;
#47440 = CARTESIAN_POINT ( 'NONE',  ( 0.6027444965799114707, -42.85215455639489335, 23.98398144100112361 ) ) ;
#47441 = CARTESIAN_POINT ( 'NONE',  ( -6.077587904424778920, -14.65844225831517633, 12.48703695652296553 ) ) ;
#47442 = B_SPLINE_CURVE_WITH_KNOTS ( 'NONE', 3,
 ( #25251, #31489, #55586, #7994 ),
 .UNSPECIFIED., .F., .F.,
 ( 4, 4 ),
 ( 0.000000000000000000, 0.004446090762761370323 ),
 .UNSPECIFIED. ) ;
#47443 = CYLINDRICAL_SURFACE ( 'NONE', #13806, 16.00000000000000000 ) ;
#47444 = CARTESIAN_POINT ( 'NONE',  ( 5.896782393890504181, 3.351618377817360273, -19.83160964539916549 ) ) ;
#47445 = CARTESIAN_POINT ( 'NONE',  ( 0.9780106845699487739, 41.90743226373805896, 0.3136359603809434904 ) ) ;
#47446 = CARTESIAN_POINT ( 'NONE',  ( 0.1129192098497447394, 39.96249028893947752, 18.70698152272492365 ) ) ;
#47447 = VERTEX_POINT ( 'NONE', #50127 ) ;
#47448 = DIRECTION ( 'NONE',  ( -1.000000000000000000, -5.380183451256670742E-17, 1.298891185607911324E-16 ) ) ;
#47449 = CARTESIAN_POINT ( 'NONE',  ( 0.5997462898726536595, 40.86908001809322855, 27.22627276398666041 ) ) ;
#47450 = ADVANCED_FACE ( 'NONE', ( #7182 ), #9342, .F. ) ;
#47451 = CARTESIAN_POINT ( 'NONE',  ( 5.974727161628367256, 5.297264154380937562, -19.82959049719570288 ) ) ;
#47452 = CARTESIAN_POINT ( 'NONE',  ( 0.8760168074886965917, 38.69913431881823129, -28.57146030081939259 ) ) ;
#47453 = CARTESIAN_POINT ( 'NONE',  ( 4.958415959904820092, 24.86570830293467438, -38.01184689561937802 ) ) ;
#47454 = DIRECTION ( 'NONE',  ( -1.000000000000000000, -0.000000000000000000, -0.000000000000000000 ) ) ;
#47455 = ITEM_DEFINED_TRANSFORMATION ( 'NONE', 'NONE', #33922,  #14677 ) ;
#47457 = ADVANCED_FACE ( 'NONE', ( #12241 ), #34982, .F. ) ;
#47456 = DIRECTION ( 'NONE',  ( 0.000000000000000000, 0.000000000000000000, -1.000000000000000000 ) ) ;
#47458 = CARTESIAN_POINT ( 'NONE',  ( 0.6027444965799114707, 48.22663320652137742, -9.259069362041273621 ) ) ;
#47459 = CARTESIAN_POINT ( 'NONE',  ( 2.301430502907645170, -34.86297247504497676, 33.04218380901160401 ) ) ;
#47460 = EDGE_CURVE ( 'NONE', #36276, #24805, #20789, .T. ) ;
#47461 = CARTESIAN_POINT ( 'NONE',  ( 0.8751705887134423323, -44.08562551107069538, -19.22545746485646490 ) ) ;
#47462 = EDGE_CURVE ( 'NONE', #32330, #40711, #56349, .T. ) ;
#47464 = VERTEX_POINT ( 'NONE', #32891 ) ;
#47463 = CARTESIAN_POINT ( 'NONE',  ( 0.6027935024548038978, -46.42277558035033991, -12.61964268015540647 ) ) ;
#47465 = ORIENTED_EDGE ( 'NONE', *, *, #52128, .F. ) ;
#47466 = CARTESIAN_POINT ( 'NONE',  ( 0.1129192098497455998, -7.520259262076605999, 43.47870154933683295 ) ) ;
#47467 = CARTESIAN_POINT ( 'NONE',  ( 0.1092565886968784733, 39.95965440403623603, 16.21587544131337921 ) ) ;
#47468 = EDGE_CURVE ( 'NONE', #15890, #16986, #33820, .T. ) ;
#47469 = DIRECTION ( 'NONE',  ( 0.000000000000000000, 0.000000000000000000, -1.000000000000000000 ) ) ;
#47470 = EDGE_LOOP ( 'NONE', ( #54921, #45682, #32293, #58441 ) ) ;
#47471 = CARTESIAN_POINT ( 'NONE',  ( 0.6029443449137436017, 10.96985678109974671, -47.86649956060598043 ) ) ;
#47472 = FACE_OUTER_BOUND ( 'NONE', #5915, .T. ) ;
#47473 = CARTESIAN_POINT ( 'NONE',  ( 0.1104177457020372871, 5.624018123398638380, -42.75615561261995623 ) ) ;
#47474 = EDGE_LOOP ( 'NONE', ( #61893, #42910, #20142, #5379 ) ) ;
#47475 = CIRCLE ( 'NONE', #6421, 10.00000000000000711 ) ;
#47476 = ORIENTED_EDGE ( 'NONE', *, *, #45796, .T. ) ;
#47477 = EDGE_CURVE ( 'NONE', #9430, #42648, #42912, .T. ) ;
#47478 = B_SPLINE_CURVE_WITH_KNOTS ( 'NONE', 3,
 ( #37945, #52295, #28493, #33534 ),
 .UNSPECIFIED., .F., .F.,
 ( 4, 4 ),
 ( 0.000000000000000000, 0.004447772540403792038 ),
 .UNSPECIFIED. ) ;
#47479 = CARTESIAN_POINT ( 'NONE',  ( 3.238018933889920792, 2.836920992588773061, -13.09043053720778715 ) ) ;
#47480 = CARTESIAN_POINT ( 'NONE',  ( 0.6253024248130478746, -7.158632958273170033, -48.58187112068006996 ) ) ;
#47481 = CARTESIAN_POINT ( 'NONE',  ( 0.5830082357119540371, 46.89517470974700331, 0.2731737188040911923 ) ) ;
#47482 = CARTESIAN_POINT ( 'NONE',  ( 4.956445790444004018, -46.73954499432459642, -5.740468958468717631 ) ) ;
#47483 = CARTESIAN_POINT ( 'NONE',  ( 6.189768672335216770, 1.091423221276722755, -1.945113688487589062E-17 ) ) ;
#47484 =( BOUNDED_SURFACE ( )  B_SPLINE_SURFACE ( 3, 1, ( 
 ( #33282, #32043 ),
 ( #52352, #9443 ),
 ( #32348, #8208 ),
 ( #23547, #18250 ) ),
 .UNSPECIFIED., .F., .F., .F. ) 
 B_SPLINE_SURFACE_WITH_KNOTS ( ( 4, 4 ),
 ( 2, 2 ),
 ( 0.000000000000000000, 1.000000000000000000 ),
 ( 0.000000000000000000, 1.000000000000000000 ),
 .UNSPECIFIED. ) 
 GEOMETRIC_REPRESENTATION_ITEM ( )  RATIONAL_B_SPLINE_SURFACE ( (
 ( 1.000000000000000000, 1.000000000000000000),
 ( 0.9953485035131437453, 0.8621029689291515030),
 ( 0.9953485035131437453, 0.8621029689291515030),
 ( 1.000000000000000000, 1.000000000000000000) ) ) 
 REPRESENTATION_ITEM ( '' )  SURFACE ( )  );
#47485 = VECTOR ( 'NONE', #54873, 1000.000000000000000 ) ;
#47486 = CARTESIAN_POINT ( 'NONE',  ( 0.1145239942831223490, 33.38557459180370302, 28.85045735997584515 ) ) ;
#47487 = ORIENTED_EDGE ( 'NONE', *, *, #55301, .F. ) ;
#47488 = DIRECTION ( 'NONE',  ( -1.000000000000000000, -1.836909530733573776E-16, 1.103352205049209901E-32 ) ) ;
#47489 = FACE_OUTER_BOUND ( 'NONE', #40194, .T. ) ;
#47490 = VECTOR ( 'NONE', #20266, 1000.000000000000114 ) ;
#47491 = EDGE_LOOP ( 'NONE', ( #34478, #32023, #17830, #50563 ) ) ;
#47492 = FACE_OUTER_BOUND ( 'NONE', #37348, .T. ) ;
#47493 = CARTESIAN_POINT ( 'NONE',  ( 0.5806925824938494740, -1.020860314013172454, 46.88475452172951918 ) ) ;
#47494 = CARTESIAN_POINT ( 'NONE',  ( 0.8560838555295223751, -13.02223058219873764, 45.06433561859954295 ) ) ;
#47495 = CARTESIAN_POINT ( 'NONE',  ( 0.9722240741986378776, 15.88116971565388802, 39.86121768686890476 ) ) ;
#47496 = AXIS2_PLACEMENT_3D ( 'NONE', #40300, #26160, #45917 ) ;
#47497 = ORIENTED_EDGE ( 'NONE', *, *, #25746, .F. ) ;
#47498 = ORIENTED_EDGE ( 'NONE', *, *, #28082, .T. ) ;
#47499 = CARTESIAN_POINT ( 'NONE',  ( 0.7048096507298635682, 28.61383451045698223, -38.67623024744019489 ) ) ;
#47500 = CARTESIAN_POINT ( 'NONE',  ( 0.2885697896453113254, -42.84523253470164406, 4.828949182955208919 ) ) ;
#47501 = CARTESIAN_POINT ( 'NONE',  ( 0.2885697896453122135, 25.60460893337430477, 34.69058521462543609 ) ) ;
#47502 =( BOUNDED_SURFACE ( )  B_SPLINE_SURFACE ( 3, 1, ( 
 ( #58026, #47426 ),
 ( #29228, #52412 ),
 ( #28610, #34256 ),
 ( #47736, #48045 ) ),
 .UNSPECIFIED., .F., .F., .F. ) 
 B_SPLINE_SURFACE_WITH_KNOTS ( ( 4, 4 ),
 ( 2, 2 ),
 ( 0.000000000000000000, 1.000000000000000000 ),
 ( 0.000000000000000000, 1.000000000000000000 ),
 .UNSPECIFIED. ) 
 GEOMETRIC_REPRESENTATION_ITEM ( )  RATIONAL_B_SPLINE_SURFACE ( (
 ( 1.000000000000000000, 1.000000000000000000),
 ( 0.9952954269826590483, 0.8620686068821339365),
 ( 0.9952954269826590483, 0.8620686068821339365),
 ( 1.000000000000000000, 1.000000000000000000) ) ) 
 REPRESENTATION_ITEM ( '' )  SURFACE ( )  );
#47503 = ADVANCED_FACE ( 'NONE', ( #33503 ), #45807, .T. ) ;
#47504 = ORIENTED_EDGE ( 'NONE', *, *, #47112, .F. ) ;
#47505 = CARTESIAN_POINT ( 'NONE',  ( 4.694002226626920127, -21.39119943673025048, -40.25793534328562373 ) ) ;
#47506 = ORIENTED_EDGE ( 'NONE', *, *, #39033, .T. ) ;
#47507 = CARTESIAN_POINT ( 'NONE',  ( 0.6028777368367060907, -25.53134248582511745, 41.94866362808920002 ) ) ;
#47508 = ORIENTED_EDGE ( 'NONE', *, *, #41489, .T. ) ;
#47509 = CARTESIAN_POINT ( 'NONE',  ( 0.5839879327111920926, -47.49806740880204359, -6.161619650335801168 ) ) ;
#47510 = CARTESIAN_POINT ( 'NONE',  ( 1.231276596079881047, -30.51591784428347154, -28.74118176309054107 ) ) ;
#47511 = CARTESIAN_POINT ( 'NONE',  ( 0.5848930533535030563, -34.90273318373162681, -31.32207366527313397 ) ) ;
#47512 = B_SPLINE_CURVE_WITH_KNOTS ( 'NONE', 3,
 ( #55000, #7378, #50013, #30278 ),
 .UNSPECIFIED., .F., .F.,
 ( 4, 4 ),
 ( 2.302551629917872730E-17, 0.004564976165746187711 ),
 .UNSPECIFIED. ) ;
#47513 = ORIENTED_EDGE ( 'NONE', *, *, #52427, .T. ) ;
#47514 = CARTESIAN_POINT ( 'NONE',  ( 0.1129192098497447394, 24.84520063729181416, -36.46461014569973713 ) ) ;
#47515 = CARTESIAN_POINT ( 'NONE',  ( 1.227938101723756947, 41.23019537246726429, -11.92353943227906399 ) ) ;
#47516 = CARTESIAN_POINT ( 'NONE',  ( 0.6000166863083090663, 22.25084548767497239, 43.78039923061538730 ) ) ;
#47517 = AXIS2_PLACEMENT_3D ( 'NONE', #29969, #44111, #6742 ) ;
#47518 = CARTESIAN_POINT ( 'NONE',  ( -6.077587904424778920, 13.82827771187084664, -13.40055061993000685 ) ) ;
#47519 = CARTESIAN_POINT ( 'NONE',  ( 0.1103310638050662429, 16.57910240621641762, -39.81020119244065114 ) ) ;
#47520 = VERTEX_POINT ( 'NONE', #8745 ) ;
#47521 = CARTESIAN_POINT ( 'NONE',  ( 0.8560838555295158248, -42.27062166135473120, 20.33635607586422012 ) ) ;
#47522 = CARTESIAN_POINT ( 'NONE',  ( 0.5848930533535030563, 36.91687493861158487, -28.92088219875856581 ) ) ;
#47523 = VERTEX_POINT ( 'NONE', #37281 ) ;
#47524 = CARTESIAN_POINT ( 'NONE',  ( 4.975801465491695552, 0.000000000000000000, 0.000000000000000000 ) ) ;
#47525 = CARTESIAN_POINT ( 'NONE',  ( 1.500000000000001332, 0.000000000000000000, 5.453125000000000000 ) ) ;
#47526 = CARTESIAN_POINT ( 'NONE',  ( 0.8744876279028306332, 40.65405044375329879, -27.52450240960324024 ) ) ;
#47527 = CARTESIAN_POINT ( 'NONE',  ( 0.1310142868023694562, -11.77532653407867436, 41.48473022063161153 ) ) ;
#47528 = B_SPLINE_CURVE_WITH_KNOTS ( 'NONE', 3,
 ( #20771, #11687, #40220, #20459 ),
 .UNSPECIFIED., .F., .F.,
 ( 4, 4 ),
 ( 5.421010862427522170E-19, 0.004446298630425085836 ),
 .UNSPECIFIED. ) ;
#47529 = CARTESIAN_POINT ( 'NONE',  ( -6.010958268070873523, 9.409153349053585913, 16.32616437357115657 ) ) ;
#47530 = CARTESIAN_POINT ( 'NONE',  ( 4.549368137175248350, -23.67244292351614376, -35.80950303116092925 ) ) ;
#47531 = CARTESIAN_POINT ( 'NONE',  ( 0.1368894036331293473, 3.601832553117911395, -43.97599490838877756 ) ) ;
#47533 = EDGE_CURVE ( 'NONE', #4551, #36259, #5898, .T. ) ;
#47532 = CARTESIAN_POINT ( 'NONE',  ( -4.214292481396491930, -11.25702090725073035, 0.000000000000000000 ) ) ;
#47534 = DIRECTION ( 'NONE',  ( -1.718001593797181987E-16, 1.000000000000000000, 0.000000000000000000 ) ) ;
#47535 = VECTOR ( 'NONE', #4097, 1000.000000000000114 ) ;
#47536 = EDGE_CURVE ( 'NONE', #37747, #14203, #29119, .T. ) ;
#47537 = CARTESIAN_POINT ( 'NONE',  ( 0.5850706913938533704, -46.31100969101495934, 12.22095376872020367 ) ) ;
#47538 = EDGE_CURVE ( 'NONE', #41116, #12007, #46675, .T. ) ;
#47539 = CARTESIAN_POINT ( 'NONE',  ( 0.2885697896453107703, 22.25146201964144765, -36.93108635218676028 ) ) ;
#47540 = ORIENTED_EDGE ( 'NONE', *, *, #53884, .T. ) ;
#47541 = CIRCLE ( 'NONE', #59496, 10.00000000000000000 ) ;
#47542 = B_SPLINE_CURVE_WITH_KNOTS ( 'NONE', 3,
 ( #59129, #11234, #39145, #6801 ),
 .UNSPECIFIED., .F., .F.,
 ( 4, 4 ),
 ( 4.336808689942017736E-19, 0.004041751736740997747 ),
 .UNSPECIFIED. ) ;
#47543 = FACE_OUTER_BOUND ( 'NONE', #47650, .T. ) ;
#47544 = ADVANCED_FACE ( 'NONE', ( #41989 ), #28544, .F. ) ;
#47545 = DIRECTION ( 'NONE',  ( 1.000000000000000000, 1.836909530733573776E-16, -1.925929944387235579E-32 ) ) ;
#47546 = VECTOR ( 'NONE', #11143, 1000.000000000000000 ) ;
#47547 = DIRECTION ( 'NONE',  ( -1.000000000000000000, -0.000000000000000000, -0.000000000000000000 ) ) ;
#47548 = CARTESIAN_POINT ( 'NONE',  ( 0.9752132459055858904, 42.51031254975323748, -5.831562321021135809 ) ) ;
#47549 = CARTESIAN_POINT ( 'NONE',  ( -2.739355103387247858, 4.908046929417170468, 14.09817868696718257 ) ) ;
#47550 = VERTEX_POINT ( 'NONE', #42595 ) ;
#47551 = CARTESIAN_POINT ( 'NONE',  ( 0.9968887458511681565, -29.87314546208208199, -30.80284987750041736 ) ) ;
#47552 = EDGE_CURVE ( 'NONE', #30367, #2015, #51804, .T. ) ;
#47553 = CARTESIAN_POINT ( 'NONE',  ( 0.6029443199889047422, -45.51848969954281188, -18.42836773366042280 ) ) ;
#47554 = CARTESIAN_POINT ( 'NONE',  ( 3.660176727303409372, -32.61164548483939285, -35.27264088192915636 ) ) ;
#47555 = VERTEX_POINT ( 'NONE', #14090 ) ;
#47556 = EDGE_CURVE ( 'NONE', #57516, #46146, #34356, .T. ) ;
#47557 = CARTESIAN_POINT ( 'NONE',  ( 0.9722240741986373225, -25.65687427836881795, -34.39263045016081577 ) ) ;
#47558 = B_SPLINE_CURVE_WITH_KNOTS ( 'NONE', 3,
 ( #56442, #12954, #51128, #41772 ),
 .UNSPECIFIED., .F., .F.,
 ( 4, 4 ),
 ( 4.336808689942017736E-19, 0.004041751736740994277 ),
 .UNSPECIFIED. ) ;
#47559 = CARTESIAN_POINT ( 'NONE',  ( 0.5806925824938502512, 43.38503874128546300, 17.80339225430713057 ) ) ;
#47560 = DIRECTION ( 'NONE',  ( 0.000000000000000000, 1.000000000000000000, 0.000000000000000000 ) ) ;
#47561 = ORIENTED_EDGE ( 'NONE', *, *, #19611, .T. ) ;
#47562 = B_SPLINE_CURVE_WITH_KNOTS ( 'NONE', 3,
 ( #34689, #1443, #58762, #40031 ),
 .UNSPECIFIED., .F., .F.,
 ( 4, 4 ),
 ( 0.000000000000000000, 0.004042984057420972825 ),
 .UNSPECIFIED. ) ;
#47563 = DIRECTION ( 'NONE',  ( 0.09722883295013595717, -0.9860961158916726754, 0.1347627703281270295 ) ) ;
#47564 = ORIENTED_EDGE ( 'NONE', *, *, #212, .F. ) ;
#47565 = CARTESIAN_POINT ( 'NONE',  ( 0.1119898979215347423, 42.04997231376550815, 13.37015843823037287 ) ) ;
#47566 = CYLINDRICAL_SURFACE ( 'NONE', #38556, 2.099999999999999645 ) ;
#47567 = ORIENTED_EDGE ( 'NONE', *, *, #28990, .F. ) ;
#47568 = DIRECTION ( 'NONE',  ( 0.09722883295013594329, 0.3508110149947656353, -0.9313850899609124045 ) ) ;
#47569 = CARTESIAN_POINT ( 'NONE',  ( 4.553261556744875094, -43.15908619232990873, 8.175135770534621926 ) ) ;
#47570 = CARTESIAN_POINT ( 'NONE',  ( 0.5837157313716019313, -7.710401042972349295, -46.25782938420864099 ) ) ;
#47571 = CARTESIAN_POINT ( 'NONE',  ( 0.5827359174754825899, -38.21848266111689441, 28.86822142608436437 ) ) ;
#47572 = EDGE_LOOP ( 'NONE', ( #21823, #51867, #45102, #29308 ) ) ;
#47573 = CARTESIAN_POINT ( 'NONE',  ( 0.9730545539215883499, -0.5054011016615761465, 42.90536227157002003 ) ) ;
#47574 = EDGE_LOOP ( 'NONE', ( #17245, #33548, #59732, #27075 ) ) ;
#47575 = CARTESIAN_POINT ( 'NONE',  ( 4.956653778116975495, -31.29546495791875316, 36.51451553856407628 ) ) ;
#47576 = ADVANCED_FACE ( 'NONE', ( #47905 ), #24160, .F. ) ;
#47577 = AXIS2_PLACEMENT_3D ( 'NONE', #42863, #61916, #13733 ) ;
#47578 = VERTEX_POINT ( 'NONE', #47592 ) ;
#47579 = ORIENTED_EDGE ( 'NONE', *, *, #15484, .F. ) ;
#47580 = CARTESIAN_POINT ( 'NONE',  ( -4.467299999999999827, 0.000000000000000000, 0.000000000000000000 ) ) ;
#47581 = CARTESIAN_POINT ( 'NONE',  ( 0.9791128995231604959, -37.40198472735112034, 18.90579204109574363 ) ) ;
#47582 = AXIS2_PLACEMENT_3D ( 'NONE', #12357, #22052, #2299 ) ;
#47583 = CARTESIAN_POINT ( 'NONE',  ( 0.1129192098497455998, -41.07894348801367812, 16.10814047907867064 ) ) ;
#47584 = CARTESIAN_POINT ( 'NONE',  ( 0.1129192098497455998, -43.69739906996312584, -6.122834499277253428 ) ) ;
#47585 = ORIENTED_EDGE ( 'NONE', *, *, #16816, .T. ) ;
#47586 = CARTESIAN_POINT ( 'NONE',  ( 4.322998006666179727, -30.86725474310334150, -36.74401119231399093 ) ) ;
#47587 = CARTESIAN_POINT ( 'NONE',  ( -2.271448787322325728E-15, -4.618802153517061804, -5.599999999999999645 ) ) ;
#47588 = CARTESIAN_POINT ( 'NONE',  ( 0.1145239942831223490, -38.60545397981544369, 21.36736773018673929 ) ) ;
#47589 = ORIENTED_EDGE ( 'NONE', *, *, #1987, .T. ) ;
#47590 = ORIENTED_EDGE ( 'NONE', *, *, #21788, .T. ) ;
#47591 = CARTESIAN_POINT ( 'NONE',  ( 0.1087620492084205720, -21.24797679669934070, -37.52665900408511135 ) ) ;
#47592 = CARTESIAN_POINT ( 'NONE',  ( 0.3622758884714730732, 42.62881903538210793, -6.444611261694146442 ) ) ;
#47593 = CARTESIAN_POINT ( 'NONE',  ( -6.072942160501519027, -11.00492040199063304, -15.80176854769334582 ) ) ;
#47594 = CARTESIAN_POINT ( 'NONE',  ( 0.1101816497532063094, -34.13008584880309826, 26.36013219694213916 ) ) ;
#47595 = CARTESIAN_POINT ( 'NONE',  ( 0.1368894036331284314, -42.51402964546802110, 11.80756576215436660 ) ) ;
#47596 = EDGE_LOOP ( 'NONE', ( #23906, #5765, #19876, #60302 ) ) ;
#47597 = EDGE_LOOP ( 'NONE', ( #55486, #60635, #29660, #41436 ) ) ;
#47598 = FACE_OUTER_BOUND ( 'NONE', #50760, .T. ) ;
#47599 = CARTESIAN_POINT ( 'NONE',  ( 2.706805983486680223, 42.85020883812403270, -10.03173543555213243 ) ) ;
#47600 = CARTESIAN_POINT ( 'NONE',  ( 2.185380717157383135, -39.05135512724729097, -20.34235644641046292 ) ) ;
#47601 = CARTESIAN_POINT ( 'NONE',  ( 0.9756950546413950542, -21.37039651692523989, 37.20808764646330502 ) ) ;
#47602 = DIRECTION ( 'NONE',  ( 0.07836865515943411409, -0.4916162952473493997, -0.8672783706145176241 ) ) ;
#47603 =( BOUNDED_SURFACE ( )  B_SPLINE_SURFACE ( 3, 1, ( 
 ( #52999, #10103 ),
 ( #57997, #53302 ),
 ( #15119, #34230 ),
 ( #29816, #25121 ) ),
 .UNSPECIFIED., .F., .F., .F. ) 
 B_SPLINE_SURFACE_WITH_KNOTS ( ( 4, 4 ),
 ( 2, 2 ),
 ( 0.000000000000000000, 1.000000000000000000 ),
 ( 0.000000000000000000, 1.000000000000000000 ),
 .UNSPECIFIED. ) 
 GEOMETRIC_REPRESENTATION_ITEM ( )  RATIONAL_B_SPLINE_SURFACE ( (
 ( 1.000000000000000000, 1.000000000000000000),
 ( 0.7223157951917476005, 0.9931996967497186413),
 ( 0.7223157951917476005, 0.9931996967497186413),
 ( 1.000000000000000000, 1.000000000000000000) ) ) 
 REPRESENTATION_ITEM ( '' )  SURFACE ( )  );
#47604 = ORIENTED_EDGE ( 'NONE', *, *, #15506, .T. ) ;
#47605 = CARTESIAN_POINT ( 'NONE',  ( -6.072942160501519915, -19.21763696748626060, -1.219258657925263112 ) ) ;
#47606 = DIRECTION ( 'NONE',  ( -1.000000000000000000, -0.000000000000000000, -0.000000000000000000 ) ) ;
#47607 = EDGE_CURVE ( 'NONE', #49238, #50555, #1757, .T. ) ;
#47608 = CARTESIAN_POINT ( 'NONE',  ( 4.956445790443998689, -10.39006634428300835, 45.93021414603936847 ) ) ;
#47609 = B_SPLINE_CURVE_WITH_KNOTS ( 'NONE', 3,
 ( #43679, #24229, #33960, #20165, #10449, #34569 ),
 .UNSPECIFIED., .F., .F.,
 ( 4, 2, 4 ),
 ( 6.892149644104416487E-18, 0.0002291472222819936403, 0.0004582944445639803958 ),
 .UNSPECIFIED. ) ;
#47610 = CARTESIAN_POINT ( 'NONE',  ( -6.079354080745853928, -8.905595498587343783, 17.07288271100410526 ) ) ;
#47611 = CARTESIAN_POINT ( 'NONE',  ( 0.8753041380234465318, -0.6841799139044266731, -49.09857661601188994 ) ) ;
#47612 = EDGE_CURVE ( 'NONE', #28131, #16591, #19368, .T. ) ;
#47613 = B_SPLINE_CURVE_WITH_KNOTS ( 'NONE', 3,
 ( #31907, #22808, #41938, #60376, #23121, #56305 ),
 .UNSPECIFIED., .F., .F.,
 ( 4, 2, 4 ),
 ( 1.964907063297894324E-17, 0.0002293319059085081922, 0.0004586638118169967062 ),
 .UNSPECIFIED. ) ;
#47614 = DIRECTION ( 'NONE',  ( 0.1736481776669314414, -0.9848077530122079093, 5.551115123125779004E-17 ) ) ;
#47615 = FACE_OUTER_BOUND ( 'NONE', #38438, .T. ) ;
#47616 = CARTESIAN_POINT ( 'NONE',  ( 4.967162193818130511, 0.000000000000000000, 0.000000000000000000 ) ) ;
#47617 = ORIENTED_EDGE ( 'NONE', *, *, #4992, .F. ) ;
#47618 = CARTESIAN_POINT ( 'NONE',  ( 5.958863334805807099, -12.49425770716475981, -16.28483817244735121 ) ) ;
#47619 = AXIS2_PLACEMENT_3D ( 'NONE', #51855, #24598, #38407 ) ;
#47620 = CARTESIAN_POINT ( 'NONE',  ( 0.9790850452238867296, 20.18493756421641905, 36.72745057571902549 ) ) ;
#47621 = CARTESIAN_POINT ( 'NONE',  ( 0.6067099128993239665, 34.36589933408243525, 33.36330296770405113 ) ) ;
#47622 = CARTESIAN_POINT ( 'NONE',  ( 0.5806925824938499181, -2.112975627976999782, 46.84824112321762613 ) ) ;
#47623 = ORIENTED_EDGE ( 'NONE', *, *, #41476, .F. ) ;
#47624 = EDGE_CURVE ( 'NONE', #30492, #6976, #3691, .T. ) ;
#47625 = CARTESIAN_POINT ( 'NONE',  ( 2.114184763561894886, 5.677447754278171364E-15, -44.03514965515262247 ) ) ;
#47626 = CARTESIAN_POINT ( 'NONE',  ( 4.956445790444029775, 25.79263028817611314, -39.39896284113449809 ) ) ;
#47627 = B_SPLINE_CURVE_WITH_KNOTS ( 'NONE', 3,
 ( #45648, #45347, #20597, #35639, #40344, #35949 ),
 .UNSPECIFIED., .F., .F.,
 ( 4, 2, 4 ),
 ( 8.131516293641283255E-19, 0.0002293801035737088028, 0.0004587602071474167925 ),
 .UNSPECIFIED. ) ;
#47628 = CARTESIAN_POINT ( 'NONE',  ( -6.057079549204054558, -6.642710526269484994, -18.07500008198967834 ) ) ;
#47629 = VERTEX_POINT ( 'NONE', #19705 ) ;
#47630 = CARTESIAN_POINT ( 'NONE',  ( 5.960721111146673579, -19.82781442290501417, 5.306302591836237426 ) ) ;
#47631 = CARTESIAN_POINT ( 'NONE',  ( 4.956653778116970166, -27.17045123668450657, -39.67974989265067620 ) ) ;
#47632 = CARTESIAN_POINT ( 'NONE',  ( 0.7954190325252789018, 24.79809930825928532, 41.21355377862707314 ) ) ;
#47633 = ORIENTED_EDGE ( 'NONE', *, *, #58189, .T. ) ;
#47634 = CONICAL_SURFACE ( 'NONE', #41657, 43.92652462719577500, 1.486293639869522343 ) ;
#47635 = CARTESIAN_POINT ( 'NONE',  ( 3.783278058412227640, -27.54892951149523483, -33.06594414781525160 ) ) ;
#47636 = ORIENTED_EDGE ( 'NONE', *, *, #27510, .F. ) ;
#47637 = CARTESIAN_POINT ( 'NONE',  ( 5.880360259849752858, -43.04573319267461073, 21.17507050419438741 ) ) ;
#47638 = VERTEX_POINT ( 'NONE', #58197 ) ;
#47639 = DIRECTION ( 'NONE',  ( 0.000000000000000000, 1.224646799147343593E-16, 1.000000000000000000 ) ) ;
#47640 = CARTESIAN_POINT ( 'NONE',  ( -5.995132425357893702, 17.41298668506970770, 7.203480333239141942 ) ) ;
#47641 = VERTEX_POINT ( 'NONE', #15320 ) ;
#47642 = CARTESIAN_POINT ( 'NONE',  ( 4.962356264823608143, 39.61238188121388504, 14.21600504921214814 ) ) ;
#47643 = B_SPLINE_CURVE_WITH_KNOTS ( 'NONE', 3,
 ( #8486, #46430, #22611, #51716 ),
 .UNSPECIFIED., .F., .F.,
 ( 4, 4 ),
 ( 0.000000000000000000, 0.005014147105413703856 ),
 .UNSPECIFIED. ) ;
#47644 = ORIENTED_EDGE ( 'NONE', *, *, #15720, .F. ) ;
#47645 = CARTESIAN_POINT ( 'NONE',  ( 0.1129192098497455998, -43.82135468580280957, 5.161459220629533107 ) ) ;
#47646 = CARTESIAN_POINT ( 'NONE',  ( 0.6030672727741701600, -38.21927534817003647, 29.21669544497185100 ) ) ;
#47647 = EDGE_CURVE ( 'NONE', #44468, #23596, #27570, .T. ) ;
#47648 = ORIENTED_EDGE ( 'NONE', *, *, #19519, .F. ) ;
#47649 = CARTESIAN_POINT ( 'NONE',  ( 0.1158403557922069033, -22.84124094437145658, -37.75205980214838775 ) ) ;
#47650 = EDGE_LOOP ( 'NONE', ( #33002, #24448, #56810, #26954 ) ) ;
#47651 = CARTESIAN_POINT ( 'NONE',  ( 5.895596859100789899, 0.6684898708304538584, -20.10177366565161350 ) ) ;
#47652 = CARTESIAN_POINT ( 'NONE',  ( 0.1158516988532803799, -17.81570362517812001, 40.36759669800286332 ) ) ;
#47653 = ORIENTED_EDGE ( 'NONE', *, *, #32346, .T. ) ;
#47654 = CARTESIAN_POINT ( 'NONE',  ( 0.5817217712918341110, 43.35050981640732459, -17.88765643302514263 ) ) ;
#47655 = EDGE_CURVE ( 'NONE', #14894, #12273, #38803, .T. ) ;
#47656 = ORIENTED_EDGE ( 'NONE', *, *, #25088, .T. ) ;
#47657 = CARTESIAN_POINT ( 'NONE',  ( 0.8557997880470599172, -47.60865952217002928, 5.347802024197076065 ) ) ;
#47658 = FACE_OUTER_BOUND ( 'NONE', #4767, .T. ) ;
#47659 = VERTEX_POINT ( 'NONE', #57568 ) ;
#47660 = CARTESIAN_POINT ( 'NONE',  ( 0.8751705887134423323, 13.30665218149362516, -46.21789262997744885 ) ) ;
#47661 = DIRECTION ( 'NONE',  ( -0.1011922191286467460, -0.5585841627631753514, -0.8232520075274534221 ) ) ;
#47662 = EDGE_CURVE ( 'NONE', #34106, #1986, #11963, .T. ) ;
#47663 = CARTESIAN_POINT ( 'NONE',  ( 4.958415959904821868, 12.97383654755002347, -43.53025980924186911 ) ) ;
#47664 = CARTESIAN_POINT ( 'NONE',  ( 0.9791128995231600518, -22.55462118696511098, -35.32175671393865457 ) ) ;
#47665 = TOROIDAL_SURFACE ( 'NONE', #18654, 12.55882000000000076, 0.05882000000000066342 ) ;
#47666 = ORIENTED_EDGE ( 'NONE', *, *, #20595, .T. ) ;
#47667 = CARTESIAN_POINT ( 'NONE',  ( 4.960386119450136633, 32.76426482034204213, 28.99895542006362703 ) ) ;
#47668 = CIRCLE ( 'NONE', #36684, 47.09074272231896430 ) ;
#47669 = CARTESIAN_POINT ( 'NONE',  ( 5.959828726073459926, -12.49160845136023923, -16.28681682518060114 ) ) ;
#47670 = B_SPLINE_CURVE_WITH_KNOTS ( 'NONE', 3,
 ( #25634, #22178, #20943, #31575, #50665, #30632 ),
 .UNSPECIFIED., .F., .F.,
 ( 4, 2, 4 ),
 ( 2.224174099750402954E-17, 0.0002293755540694314540, 0.0004587511081388406277 ),
 .UNSPECIFIED. ) ;
#47671 = CARTESIAN_POINT ( 'NONE',  ( 4.967162193818130511, -40.93989340068619498, 13.42934394584149871 ) ) ;
#47672 = CARTESIAN_POINT ( 'NONE',  ( 0.7057020205115048794, 46.47981817772241442, -11.58334423512187605 ) ) ;
#47673 =( BOUNDED_SURFACE ( )  B_SPLINE_SURFACE ( 3, 1, ( 
 ( #49566, #6624 ),
 ( #21691, #12014 ),
 ( #30151, #25772 ),
 ( #45220, #2255 ) ),
 .UNSPECIFIED., .F., .F., .F. ) 
 B_SPLINE_SURFACE_WITH_KNOTS ( ( 4, 4 ),
 ( 2, 2 ),
 ( 0.000000000000000000, 1.000000000000000000 ),
 ( 0.000000000000000000, 1.000000000000000000 ),
 .UNSPECIFIED. ) 
 GEOMETRIC_REPRESENTATION_ITEM ( )  RATIONAL_B_SPLINE_SURFACE ( (
 ( 1.000000000000000000, 1.000000000000000000),
 ( 0.7282232189291694135, 0.9929344683865672927),
 ( 0.7282232189291694135, 0.9929344683865672927),
 ( 1.000000000000000000, 1.000000000000000000) ) ) 
 REPRESENTATION_ITEM ( '' )  SURFACE ( )  );
#47674 = B_SPLINE_CURVE_WITH_KNOTS ( 'NONE', 3,
 ( #2207, #2833, #16329, #55144, #8157, #46395 ),
 .UNSPECIFIED., .F., .F.,
 ( 4, 2, 4 ),
 ( 1.964907063297894324E-17, 0.0002293319059085101709, 0.0004586638118170006636 ),
 .UNSPECIFIED. ) ;
#47675 = CARTESIAN_POINT ( 'NONE',  ( 4.967162193818130511, 0.000000000000000000, 0.000000000000000000 ) ) ;
#47676 = EDGE_CURVE ( 'NONE', #46030, #14818, #33814, .T. ) ;
#47678 = AXIS2_PLACEMENT_3D ( 'NONE', #50522, #7596, #27034 ) ;
#47677 = B_SPLINE_CURVE_WITH_KNOTS ( 'NONE', 3,
 ( #50532, #45254, #59932, #30803, #31749, #41474, #3217, #45869, #7605, #54595, #17042, #36155, #6979, #55221, #12345, #40252, #50231, #60228, #51143, #36775, #45551, #1984, #40553, #26732, #2604 ),
 .UNSPECIFIED., .F., .F.,
 ( 4, 3, 3, 3, 3, 3, 3, 3, 4 ),
 ( 5.057544569639795705E-18, 0.0005656085177311397484, 0.001131215744874499189, 0.001696821861372765699, 0.002262427090022497284, 0.002828031679238745058, 0.003393635864401604429, 0.003977030878808130755, 0.004561030005651157265 ),
 .UNSPECIFIED. ) ;
#47679 = DIRECTION ( 'NONE',  ( 0.000000000000000000, 0.000000000000000000, -1.000000000000000000 ) ) ;
#47680 = CARTESIAN_POINT ( 'NONE',  ( 4.956445790444005794, -28.36659270909926533, -37.58822246682746737 ) ) ;
#47681 = ADVANCED_FACE ( 'NONE', ( #10300 ), #47780, .F. ) ;
#47682 = DIRECTION ( 'NONE',  ( -1.000000000000000000, 0.000000000000000000, 0.000000000000000000 ) ) ;
#47683 = CARTESIAN_POINT ( 'NONE',  ( 0.6009453534118438522, 48.10564080474284054, 0.4363813339959712878 ) ) ;
#47684 = DIRECTION ( 'NONE',  ( 0.000000000000000000, -0.7071067811865435759, -0.7071067811865514585 ) ) ;
#47685 = CARTESIAN_POINT ( 'NONE',  ( -6.017396004339686577, -11.47192209077577196, -14.94857180792004669 ) ) ;
#47686 = CARTESIAN_POINT ( 'NONE',  ( 0.5807400328401574052, 18.83234461715182562, 44.04145271122570904 ) ) ;
#47687 = DIRECTION ( 'NONE',  ( 0.09835009131224552170, -0.5042575517176627331, -0.8579344853044326147 ) ) ;
#47688 = EDGE_CURVE ( 'NONE', #5258, #1848, #57886, .T. ) ;
#47689 = CARTESIAN_POINT ( 'NONE',  ( 0.5850706913938534814, 47.89601588673689037, -0.1816364388702012000 ) ) ;
#47690 = FACE_OUTER_BOUND ( 'NONE', #55605, .T. ) ;
#47691 = CARTESIAN_POINT ( 'NONE',  ( 0.1368894036331291253, 20.97178701940289258, 38.82068359954699588 ) ) ;
#47692 = VERTEX_POINT ( 'NONE', #25624 ) ;
#47693 = CARTESIAN_POINT ( 'NONE',  ( 0.5997462898726536595, -39.04071682475809268, 29.78882441375220580 ) ) ;
#47694 = CARTESIAN_POINT ( 'NONE',  ( 0.5836750258453363704, 23.79054009282546644, 41.56963612796194951 ) ) ;
#47695 = CARTESIAN_POINT ( 'NONE',  ( 4.962356264823593044, 12.88441948660167391, 40.06528837230087703 ) ) ;
#47696 = EDGE_LOOP ( 'NONE', ( #35916, #1250, #44339, #4263 ) ) ;
#47697 = ADVANCED_FACE ( 'NONE', ( #25315 ), #2752, .F. ) ;
#47698 = CARTESIAN_POINT ( 'NONE',  ( 0.5819845901640493535, -34.18710267837677463, 33.54497622115119526 ) ) ;
#47699 = CARTESIAN_POINT ( 'NONE',  ( 0.3676999524040366896, 25.91024933382758277, 35.70167450949220722 ) ) ;
#47700 = VERTEX_POINT ( 'NONE', #48209 ) ;
#47701 = ORIENTED_EDGE ( 'NONE', *, *, #27235, .F. ) ;
#47702 = FACE_BOUND ( 'NONE', #32235, .T. ) ;
#47703 = AXIS2_PLACEMENT_3D ( 'NONE', #2260, #9137, #46760 ) ;
#47704 = ORIENTED_EDGE ( 'NONE', *, *, #58527, .F. ) ;
#47705 = CARTESIAN_POINT ( 'NONE',  ( 3.407937589446174087, -4.815089211104962352, -12.82481284928208964 ) ) ;
#47706 = VECTOR ( 'NONE', #32254, 1000.000000000000000 ) ;
#47707 = CARTESIAN_POINT ( 'NONE',  ( 0.3622758884714600280, -6.444611261694905835, 42.62881903538198713 ) ) ;
#47708 = VECTOR ( 'NONE', #43337, 1000.000000000000000 ) ;
#47709 = ORIENTED_EDGE ( 'NONE', *, *, #54677, .F. ) ;
#47710 = ORIENTED_EDGE ( 'NONE', *, *, #47122, .F. ) ;
#47711 = FACE_OUTER_BOUND ( 'NONE', #2625, .T. ) ;
#47712 = VERTEX_POINT ( 'NONE', #15627 ) ;
#47713 = CARTESIAN_POINT ( 'NONE',  ( 4.553261556744875094, -41.75933753256810377, 13.62707946203756393 ) ) ;
#47714 = CARTESIAN_POINT ( 'NONE',  ( 1.227938101723748288, 41.66816631169206886, -10.28900963485336995 ) ) ;
#47715 = CARTESIAN_POINT ( 'NONE',  ( -15.25000000000000711, -2.688986455804108555, -9.952330921218299798E-16 ) ) ;
#47716 = ORIENTED_EDGE ( 'NONE', *, *, #18254, .T. ) ;
#47717 = DIRECTION ( 'NONE',  ( 0.09722883295013598492, 0.4536333312076149538, 0.8858687006891241555 ) ) ;
#47718 = CARTESIAN_POINT ( 'NONE',  ( 2.618530812446111078, 23.81615347600983768, -40.52798567416525088 ) ) ;
#47719 = VERTEX_POINT ( 'NONE', #5261 ) ;
#47720 = CONICAL_SURFACE ( 'NONE', #54716, 43.08621763946400307, 1.568696531533066763 ) ;
#47721 = ORIENTED_EDGE ( 'NONE', *, *, #15426, .T. ) ;
#47722 = ADVANCED_FACE ( 'NONE', ( #250 ), #41391, .F. ) ;
#47723 = DIRECTION ( 'NONE',  ( 0.000000000000000000, 0.000000000000000000, -1.000000000000000000 ) ) ;
#47724 = VERTEX_POINT ( 'NONE', #39443 ) ;
#47725 = CARTESIAN_POINT ( 'NONE',  ( 2.359973842542476330, 34.48061513594045380, 27.37193954544789420 ) ) ;
#47726 = CARTESIAN_POINT ( 'NONE',  ( 0.8753041380234465318, -24.68967207985765455, -42.44476905888495111 ) ) ;
#47727 = FACE_OUTER_BOUND ( 'NONE', #36426, .T. ) ;
#47728 = CARTESIAN_POINT ( 'NONE',  ( 4.967162193818130511, -14.26841313271309808, 40.65506779172159924 ) ) ;
#47729 = EDGE_CURVE ( 'NONE', #21005, #16278, #53753, .T. ) ;
#47730 = B_SPLINE_CURVE_WITH_KNOTS ( 'NONE', 3,
 ( #49833, #45774, #21024, #41090, #45167, #26030 ),
 .UNSPECIFIED., .F., .F.,
 ( 4, 2, 4 ),
 ( 8.440430351524944310E-17, 0.0002293366620881473158, 0.0004586733241762102264 ),
 .UNSPECIFIED. ) ;
#47731 = VERTEX_POINT ( 'NONE', #59124 ) ;
#47732 = CARTESIAN_POINT ( 'NONE',  ( -6.057079549204054558, 11.99988366729722244, -15.06101002825082169 ) ) ;
#47733 = CONICAL_SURFACE ( 'NONE', #55708, 42.92674063221959813, 1.485477209440487556 ) ;
#47734 = CARTESIAN_POINT ( 'NONE',  ( 4.967162193818130511, 0.000000000000000000, 0.000000000000000000 ) ) ;
#47735 = EDGE_CURVE ( 'NONE', #2365, #22119, #13829, .T. ) ;
#47736 = CARTESIAN_POINT ( 'NONE',  ( 5.896782393890504181, 19.70854070425251692, -4.012419492878830596 ) ) ;
#47737 = VERTEX_POINT ( 'NONE', #36280 ) ;
#47738 = CARTESIAN_POINT ( 'NONE',  ( 4.962356264823593044, 18.10963840443015016, 37.99048031708913697 ) ) ;
#47739 = EDGE_CURVE ( 'NONE', #46120, #41724, #14952, .T. ) ;
#47740 = CARTESIAN_POINT ( 'NONE',  ( 4.000000000000003553, 2.309401076758524685, -0.3572655899081733644 ) ) ;
#47741 = CARTESIAN_POINT ( 'NONE',  ( 2.533389852662419894, -5.458459604331522996, 43.67671863225876194 ) ) ;
#47742 = ORIENTED_EDGE ( 'NONE', *, *, #44258, .F. ) ;
#47743 = EDGE_LOOP ( 'NONE', ( #47854, #47337, #24634, #34541 ) ) ;
#47744 = CARTESIAN_POINT ( 'NONE',  ( 5.910764540655178756, -15.77444817831471013, 12.47669920847764580 ) ) ;
#47745 = FACE_OUTER_BOUND ( 'NONE', #24043, .T. ) ;
#47746 = CARTESIAN_POINT ( 'NONE',  ( 4.975610109902397937, -43.81605102859442979, -21.73943604138302987 ) ) ;
#47747 = CARTESIAN_POINT ( 'NONE',  ( 4.694002226626920127, -45.47116547585236646, 3.264641130933999325 ) ) ;
#47748 = B_SPLINE_CURVE_WITH_KNOTS ( 'NONE', 3,
 ( #55951, #54705, #45975, #16519, #7087, #40353 ),
 .UNSPECIFIED., .F., .F.,
 ( 4, 2, 4 ),
 ( 9.851335625380350225E-18, 0.0002445244328975374566, 0.0004890488657950650469 ),
 .UNSPECIFIED. ) ;
#47749 = CARTESIAN_POINT ( 'NONE',  ( -6.017396004339687465, -11.47192209077597447, 14.94857180791989215 ) ) ;
#47750 = CARTESIAN_POINT ( 'NONE',  ( 0.1158516988532803660, -17.90573022250301349, -40.32774459391125532 ) ) ;
#47751 = CARTESIAN_POINT ( 'NONE',  ( 4.549368137175248350, 0.000000000000000000, 0.000000000000000000 ) ) ;
#47752 = CARTESIAN_POINT ( 'NONE',  ( 4.694002226626920127, 1.805541223687672447, 45.55244002614677612 ) ) ;
#47753 = EDGE_CURVE ( 'NONE', #61317, #28755, #51519, .T. ) ;
#47754 = CARTESIAN_POINT ( 'NONE',  ( 0.9791128995231609400, 41.90867939003388187, -0.005101912726580280430 ) ) ;
#47755 =( BOUNDED_SURFACE ( )  B_SPLINE_SURFACE ( 3, 1, ( 
 ( #43339, #15127 ),
 ( #45726, #12215 ),
 ( #31299, #7154 ),
 ( #40416, #30993 ) ),
 .UNSPECIFIED., .F., .F., .F. ) 
 B_SPLINE_SURFACE_WITH_KNOTS ( ( 4, 4 ),
 ( 2, 2 ),
 ( 0.000000000000000000, 1.000000000000000000 ),
 ( 0.000000000000000000, 1.000000000000000000 ),
 .UNSPECIFIED. ) 
 GEOMETRIC_REPRESENTATION_ITEM ( )  RATIONAL_B_SPLINE_SURFACE ( (
 ( 1.000000000000000000, 1.000000000000000000),
 ( 0.9751682680413298332, 0.9999560080971552356),
 ( 0.9751682680413298332, 0.9999560080971552356),
 ( 1.000000000000000000, 1.000000000000000000) ) ) 
 REPRESENTATION_ITEM ( '' )  SURFACE ( )  );
#47756 = LINE ( 'NONE', #23946, #16887 ) ;
#47757 = ORIENTED_EDGE ( 'NONE', *, *, #21584, .T. ) ;
#47758 = CIRCLE ( 'NONE', #38788, 15.14599999999999369 ) ;
#47759 = CIRCLE ( 'NONE', #38790, 47.91270532121795611 ) ;
#47760 = EDGE_CURVE ( 'NONE', #43756, #53679, #30552, .T. ) ;
#47761 = DIRECTION ( 'NONE',  ( -1.000000000000000000, -1.836909530733580185E-16, 1.836909530733574022E-16 ) ) ;
#47762 = DIRECTION ( 'NONE',  ( -1.000000000000000000, -3.135800716341471541E-16, -1.298891185607920445E-16 ) ) ;
#47763 = CARTESIAN_POINT ( 'NONE',  ( 0.8560838555295158248, -45.77741231505087427, -10.23725333375899105 ) ) ;
#47764 = LINE ( 'NONE', #14875, #26033 ) ;
#47765 = B_SPLINE_CURVE_WITH_KNOTS ( 'NONE', 3,
 ( #29503, #10721, #29812, #48924, #1289, #52995 ),
 .UNSPECIFIED., .F., .F.,
 ( 4, 2, 4 ),
 ( 3.127317220692750759E-18, 0.0002447193893791708465, 0.0004894387787583385488 ),
 .UNSPECIFIED. ) ;
#47766 = CARTESIAN_POINT ( 'NONE',  ( 2.281448460670565836, 25.11570011049370876, 40.87338159040645280 ) ) ;
#47767 = CARTESIAN_POINT ( 'NONE',  ( 0.1097557419366048670, 42.78407272074150569, 5.407604117549856149 ) ) ;
#47768 = DIRECTION ( 'NONE',  ( 0.000000000000000000, 0.000000000000000000, 1.000000000000000000 ) ) ;
#47769 = EDGE_CURVE ( 'NONE', #1942, #15748, #60503, .T. ) ;
#47770 = CARTESIAN_POINT ( 'NONE',  ( 4.960386119450151732, -34.04466635746562986, -27.48448939458741691 ) ) ;
#47771 = CARTESIAN_POINT ( 'NONE',  ( 0.8560838555295223751, 9.983184696771347788, -45.83349056521751663 ) ) ;
#47772 = CARTESIAN_POINT ( 'NONE',  ( 0.3622758884714600280, 26.89560658783384994, -33.69533458712316332 ) ) ;
#47773 =( BOUNDED_SURFACE ( )  B_SPLINE_SURFACE ( 3, 1, ( 
 ( #37060, #56125 ),
 ( #13239, #59907 ),
 ( #32343, #17019 ),
 ( #61128, #22948 ) ),
 .UNSPECIFIED., .F., .F., .F. ) 
 B_SPLINE_SURFACE_WITH_KNOTS ( ( 4, 4 ),
 ( 2, 2 ),
 ( 0.000000000000000000, 1.000000000000000000 ),
 ( 0.000000000000000000, 1.000000000000000000 ),
 .UNSPECIFIED. ) 
 GEOMETRIC_REPRESENTATION_ITEM ( )  RATIONAL_B_SPLINE_SURFACE ( (
 ( 1.000000000000000000, 1.000000000000000000),
 ( 0.9751682680413298332, 0.9999560080971552356),
 ( 0.9751682680413298332, 0.9999560080971552356),
 ( 1.000000000000000000, 1.000000000000000000) ) ) 
 REPRESENTATION_ITEM ( '' )  SURFACE ( )  );
#47775 = ORIENTED_EDGE ( 'NONE', *, *, #51689, .F. ) ;
#47774 = CARTESIAN_POINT ( 'NONE',  ( 0.9730545539215883499, -6.101350888304943432, 42.47233286818615028 ) ) ;
#47776 = EDGE_LOOP ( 'NONE', ( #24737, #53038, #7942, #25374 ) ) ;
#47777 = CARTESIAN_POINT ( 'NONE',  ( 0.8751705887134553219, 46.67919521768871505, 11.58504748649215976 ) ) ;
#47778 = CARTESIAN_POINT ( 'NONE',  ( 0.1097557419366048670, 39.92664986079710587, 16.29667732266766222 ) ) ;
#47779 = CARTESIAN_POINT ( 'NONE',  ( 5.960721111146673579, -14.51823969584089902, -14.50930005615011709 ) ) ;
#47780 =( BOUNDED_SURFACE ( )  B_SPLINE_SURFACE ( 3, 1, ( 
 ( #5566, #38829 ),
 ( #571, #11228 ),
 ( #6178, #29394 ),
 ( #19396, #49425 ) ),
 .UNSPECIFIED., .F., .F., .F. ) 
 B_SPLINE_SURFACE_WITH_KNOTS ( ( 4, 4 ),
 ( 2, 2 ),
 ( 0.000000000000000000, 1.000000000000000000 ),
 ( 0.000000000000000000, 1.000000000000000000 ),
 .UNSPECIFIED. ) 
 GEOMETRIC_REPRESENTATION_ITEM ( )  RATIONAL_B_SPLINE_SURFACE ( (
 ( 1.000000000000000000, 1.000000000000000000),
 ( 0.9953485035131437453, 0.8621029689291515030),
 ( 0.9953485035131437453, 0.8621029689291515030),
 ( 1.000000000000000000, 1.000000000000000000) ) ) 
 REPRESENTATION_ITEM ( '' )  SURFACE ( )  );
#47781 = B_SPLINE_CURVE_WITH_KNOTS ( 'NONE', 3,
 ( #38190, #13763, #47571, #4308, #42572, #61631, #52555, #4612, #53473, #43503, #53175, #57864, #1776, #34102, #14682, #15907 ),
 .UNSPECIFIED., .F., .F.,
 ( 4, 3, 3, 3, 3, 4 ),
 ( 9.813676791237319219E-18, 0.0002724568934985605886, 0.0004086836638483811769, 0.0005449104342063590314, 0.0008173270854453652638, 0.001089761613562689442 ),
 .UNSPECIFIED. ) ;
#47782 = EDGE_CURVE ( 'NONE', #10104, #13648, #5135, .T. ) ;
#47783 = VERTEX_POINT ( 'NONE', #25938 ) ;
#47784 = FACE_OUTER_BOUND ( 'NONE', #4673, .T. ) ;
#47785 = CARTESIAN_POINT ( 'NONE',  ( 0.7056555295713342613, 37.48482836297272769, -29.82339362082558765 ) ) ;
#47786 = CARTESIAN_POINT ( 'NONE',  ( 4.956653778116992370, 27.17045123668527751, -39.67974989265010777 ) ) ;
#47788 = EDGE_CURVE ( 'NONE', #47109, #54823, #2420, .T. ) ;
#47787 = VERTEX_POINT ( 'NONE', #45376 ) ;
#47789 = ORIENTED_EDGE ( 'NONE', *, *, #30455, .T. ) ;
#47790 = CARTESIAN_POINT ( 'NONE',  ( 1.827326673878742591, 36.65065268305627910, 22.58371678864595111 ) ) ;
#47791 = CIRCLE ( 'NONE', #40839, 42.92674063221959813 ) ;
#47792 = CARTESIAN_POINT ( 'NONE',  ( 0.5987334363312691865, -7.239498697625133872, -48.57110833694409280 ) ) ;
#47793 = CARTESIAN_POINT ( 'NONE',  ( 4.335381028904216727, 42.17650767838677694, 24.91784596868934898 ) ) ;
#47794 = CARTESIAN_POINT ( 'NONE',  ( 0.5782707292762423457, -35.26595510591648974, -30.92003823049223143 ) ) ;
#47795 = B_SPLINE_CURVE_WITH_KNOTS ( 'NONE', 3,
 ( #57118, #33659, #57729, #33972 ),
 .UNSPECIFIED., .F., .F.,
 ( 4, 4 ),
 ( 1.969819611697804288E-17, 0.004444306975806115896 ),
 .UNSPECIFIED. ) ;
#47796 = CARTESIAN_POINT ( 'NONE',  ( 4.956653778116996811, 45.35992544608552635, -15.97476558431834626 ) ) ;
#47797 = B_SPLINE_CURVE_WITH_KNOTS ( 'NONE', 3,
 ( #35529, #44938, #43709, #29571 ),
 .UNSPECIFIED., .F., .F.,
 ( 4, 4 ),
 ( 0.000000000000000000, 0.004445488388166993383 ),
 .UNSPECIFIED. ) ;
#47798 = CARTESIAN_POINT ( 'NONE',  ( 0.9752132459055847802, 42.57112816680955802, 5.369621847647748858 ) ) ;
#47799 = VERTEX_POINT ( 'NONE', #40999 ) ;
#47800 = B_SPLINE_CURVE_WITH_KNOTS ( 'NONE', 3,
 ( #46857, #28339, #51206, #47767, #32435, #4814, #116, #47157, #37148, #3898, #51510, #57431, #23038, #8290, #9531, #37775, #42167, #61221, #33369 ),
 .UNSPECIFIED., .F., .F.,
 ( 4, 3, 3, 3, 3, 3, 4 ),
 ( 1.161956753697875813E-16, 0.0002618519381806256457, 0.0003927759815485963547, 0.0005237000248299426711, 0.0006546240681324986925, 0.0007855481115631319502, 0.0009699050456655111587 ),
 .UNSPECIFIED. ) ;
#47801 = CARTESIAN_POINT ( 'NONE',  ( 4.958415959904820092, 19.57736038521061417, -40.98696029434518096 ) ) ;
#47802 = CARTESIAN_POINT ( 'NONE',  ( -6.063463321072276813, -6.635954031850941348, 18.07718359055500557 ) ) ;
#47803 = AXIS2_PLACEMENT_3D ( 'NONE', #43845, #43525, #9998 ) ;
#47804 = ORIENTED_EDGE ( 'NONE', *, *, #3295, .T. ) ;
#47805 = VECTOR ( 'NONE', #17926, 999.9999999999998863 ) ;
#47806 = CARTESIAN_POINT ( 'NONE',  ( 1.088908134280556661, -37.54826033999246704, -20.77739698351972564 ) ) ;
#47807 = CARTESIAN_POINT ( 'NONE',  ( 0.6067375320500720814, -47.89177856776002074, -0.7090021732338949167 ) ) ;
#47808 = CARTESIAN_POINT ( 'NONE',  ( 0.6017667736363748743, 46.37677940471279925, 12.78803812527904249 ) ) ;
#47809 = CARTESIAN_POINT ( 'NONE',  ( 3.240649175237396484, -43.82655554202737136, 3.807616934414570053 ) ) ;
#47810 = EDGE_CURVE ( 'NONE', #58502, #51012, #60784, .T. ) ;
#47811 = ORIENTED_EDGE ( 'NONE', *, *, #32269, .F. ) ;
#47812 = ORIENTED_EDGE ( 'NONE', *, *, #35711, .T. ) ;
#47813 = CARTESIAN_POINT ( 'NONE',  ( 0.5807400328401637335, -17.82553128098439998, 44.45848844984437420 ) ) ;
#47814 = CARTESIAN_POINT ( 'NONE',  ( 0.6041374136657476912, -44.51224464244987900, -18.24862627831519646 ) ) ;
#47815 = EDGE_CURVE ( 'NONE', #23761, #539, #12731, .T. ) ;
#47816 = CARTESIAN_POINT ( 'NONE',  ( 0.1103310638050662290, -37.30561229499315345, -21.63353985999675189 ) ) ;
#47817 = CARTESIAN_POINT ( 'NONE',  ( 1.231276596079881935, -34.07446381689681658, -24.41736444846283405 ) ) ;
#47818 = EDGE_LOOP ( 'NONE', ( #42896, #46040, #18576, #25672 ) ) ;
#47819 = CARTESIAN_POINT ( 'NONE',  ( 0.6041374136657476912, -46.42299778158164258, 12.61972904329520340 ) ) ;
#47821 = ORIENTED_EDGE ( 'NONE', *, *, #50072, .F. ) ;
#47820 = ADVANCED_FACE ( 'NONE', ( #18946 ), #54141, .F. ) ;
#47822 = FACE_OUTER_BOUND ( 'NONE', #53826, .T. ) ;
#47823 = CARTESIAN_POINT ( 'NONE',  ( -2.601141883200665639, 14.55883463511893794, 3.291771792917906225 ) ) ;
#47824 = ADVANCED_FACE ( 'NONE', ( #38067 ), #17773, .F. ) ;
#47825 = ORIENTED_EDGE ( 'NONE', *, *, #46634, .T. ) ;
#47826 = CARTESIAN_POINT ( 'NONE',  ( 0.5819845901640493535, -0.4540519722834164829, 47.89381229371849713 ) ) ;
#47827 = EDGE_CURVE ( 'NONE', #22696, #3215, #35136, .T. ) ;
#47828 = LINE ( 'NONE', #61880, #5724 ) ;
#47829 = CARTESIAN_POINT ( 'NONE',  ( 0.9741495583595169983, 26.43366215195310076, -33.79932324264157018 ) ) ;
#47830 = VECTOR ( 'NONE', #14398, 1000.000000000000000 ) ;
#47831 = ORIENTED_EDGE ( 'NONE', *, *, #39386, .F. ) ;
#47832 = CARTESIAN_POINT ( 'NONE',  ( 0.7954196712028469562, 47.79303691884131666, -5.415566793624839725 ) ) ;
#47833 = CARTESIAN_POINT ( 'NONE',  ( 3.240649175237395596, -42.97983288049779560, 9.380771981139487181 ) ) ;
#47834 = CARTESIAN_POINT ( 'NONE',  ( 4.975801465491694664, 47.76942479135480824, 3.702618843597622167 ) ) ;
#47835 = ADVANCED_FACE ( 'NONE', ( #19867 ), #60550, .F. ) ;
#47836 = CARTESIAN_POINT ( 'NONE',  ( 0.6017667736363750963, 29.56223180955331387, -37.95278695280779857 ) ) ;
#47837 = CARTESIAN_POINT ( 'NONE',  ( 4.975801465491695552, 0.000000000000000000, 0.000000000000000000 ) ) ;
#47838 = VERTEX_POINT ( 'NONE', #42750 ) ;
#47839 = CARTESIAN_POINT ( 'NONE',  ( 4.322998006666165516, -36.74401119231389146, -30.86725474310346584 ) ) ;
#47840 = CARTESIAN_POINT ( 'NONE',  ( 1.834102595619085729, -16.63057890322184207, 40.78751757831550862 ) ) ;
#47841 = VERTEX_POINT ( 'NONE', #14247 ) ;
#47842 = FACE_OUTER_BOUND ( 'NONE', #14964, .T. ) ;
#47843 = CARTESIAN_POINT ( 'NONE',  ( 3.238741278300275805, 29.07934833201323599, 31.66556122967967823 ) ) ;
#47844 = LINE ( 'NONE', #61595, #2793 ) ;
#47845 = FACE_OUTER_BOUND ( 'NONE', #30155, .T. ) ;
#47846 = B_SPLINE_CURVE_WITH_KNOTS ( 'NONE', 3,
 ( #58133, #57505, #9937, #15256, #53730, #507 ),
 .UNSPECIFIED., .F., .F.,
 ( 4, 2, 4 ),
 ( 9.898949898072313973E-18, 0.0002445244328975399502, 0.0004890488657950699258 ),
 .UNSPECIFIED. ) ;
#47847 = CARTESIAN_POINT ( 'NONE',  ( 0.5998501479064699549, -41.39809967730504781, 24.50586714782532027 ) ) ;
#47848 = LINE ( 'NONE', #8366, #20091 ) ;
#47849 = CARTESIAN_POINT ( 'NONE',  ( 50.67307810846496352, 15.27178771460631346, 2.649999999999992806 ) ) ;
#47850 = CARTESIAN_POINT ( 'NONE',  ( 0.5987334363312691865, -30.14260600494100828, -38.76836609534854716 ) ) ;
#47851 = CARTESIAN_POINT ( 'NONE',  ( 5.880360259849739535, -47.04104239318773040, 9.405269135694428684 ) ) ;
#47852 = CARTESIAN_POINT ( 'NONE',  ( 0.1073791018717578927, -25.86618856530687793, -34.50606437925538472 ) ) ;
#47854 = ORIENTED_EDGE ( 'NONE', *, *, #39144, .T. ) ;
#47853 = CARTESIAN_POINT ( 'NONE',  ( 0.1103878639767399139, -5.580746265797351668, 42.76182653383947496 ) ) ;
#47855 = EDGE_LOOP ( 'NONE', ( #48284, #59036, #38132, #44140 ) ) ;
#47856 = CIRCLE ( 'NONE', #4788, 2.649999999999999467 ) ;
#47857 = CARTESIAN_POINT ( 'NONE',  ( 2.624215991343620935, 22.77108897942195043, -42.26352390376072776 ) ) ;
#47858 = CARTESIAN_POINT ( 'NONE',  ( 48.39222823129596662, 15.41626216437607155, -1.615489271240708291 ) ) ;
#47859 = EDGE_CURVE ( 'NONE', #27767, #52998, #42567, .T. ) ;
#47860 = CARTESIAN_POINT ( 'NONE',  ( 1.154321485836934391, 30.92445806269079611, 29.75729673892710636 ) ) ;
#47861 = CARTESIAN_POINT ( 'NONE',  ( 0.3622758884714730732, 17.25816669464937902, 39.50828911767005280 ) ) ;
#47862 = LINE ( 'NONE', #205, #35556 ) ;
#47863 =( BOUNDED_SURFACE ( )  B_SPLINE_SURFACE ( 3, 1, ( 
 ( #13493, #41704 ),
 ( #4049, #32597 ),
 ( #51681, #47308 ),
 ( #47017, #23191 ) ),
 .UNSPECIFIED., .F., .F., .F. ) 
 B_SPLINE_SURFACE_WITH_KNOTS ( ( 4, 4 ),
 ( 2, 2 ),
 ( 0.000000000000000000, 1.000000000000000000 ),
 ( 0.000000000000000000, 1.000000000000000000 ),
 .UNSPECIFIED. ) 
 GEOMETRIC_REPRESENTATION_ITEM ( )  RATIONAL_B_SPLINE_SURFACE ( (
 ( 1.000000000000000000, 1.000000000000000000),
 ( 0.7282232189291694135, 0.9929344683865672927),
 ( 0.7282232189291694135, 0.9929344683865672927),
 ( 1.000000000000000000, 1.000000000000000000) ) ) 
 REPRESENTATION_ITEM ( '' )  SURFACE ( )  );
#47864 = EDGE_CURVE ( 'NONE', #27102, #17686, #9701, .T. ) ;
#47865 = ORIENTED_EDGE ( 'NONE', *, *, #2673, .T. ) ;
#47866 = CARTESIAN_POINT ( 'NONE',  ( 0.2885697896453110478, -4.828949182955637909, -42.84523253470159432 ) ) ;
#47867 = CIRCLE ( 'NONE', #20848, 47.09074272231896430 ) ;
#47868 = CARTESIAN_POINT ( 'NONE',  ( 0.9762797500689124330, 40.28286501695569655, 11.55922018180428168 ) ) ;
#47869 = DIRECTION ( 'NONE',  ( -1.000000000000000000, -0.000000000000000000, -0.000000000000000000 ) ) ;
#47870 = ORIENTED_EDGE ( 'NONE', *, *, #52891, .F. ) ;
#47871 = CARTESIAN_POINT ( 'NONE',  ( 5.917102823773431552, -2.004558746498307453, -20.01178308606155554 ) ) ;
#47872 = CARTESIAN_POINT ( 'NONE',  ( 0.5834584762367743815, -25.08023035601203077, -39.62597676149527359 ) ) ;
#47873 = ORIENTED_EDGE ( 'NONE', *, *, #53523, .T. ) ;
#47874 = DIRECTION ( 'NONE',  ( -1.000000000000000000, 0.000000000000000000, 0.000000000000000000 ) ) ;
#47875 = ORIENTED_EDGE ( 'NONE', *, *, #54267, .F. ) ;
#47876 = CARTESIAN_POINT ( 'NONE',  ( 51.18719699018952696, 15.28630115564075354, -2.565184398965006718 ) ) ;
#47877 = CARTESIAN_POINT ( 'NONE',  ( -6.077587904424778920, -1.855182226445892812, -19.16648951426968850 ) ) ;
#47878 = ORIENTED_EDGE ( 'NONE', *, *, #12552, .F. ) ;
#47879 = CARTESIAN_POINT ( 'NONE',  ( 4.549368137175248350, 23.67244292351589507, 35.80950303116109268 ) ) ;
#47880 = CARTESIAN_POINT ( 'NONE',  ( 5.894904586330512508, -4.663773726906393691, 19.56472914931000417 ) ) ;
#47881 = CARTESIAN_POINT ( 'NONE',  ( 3.238931869106855377, 27.59912060131728140, 32.96367555688120632 ) ) ;
#47882 = CARTESIAN_POINT ( 'NONE',  ( 3.678834586032787346, 18.63781918815739047, -45.29066201258165592 ) ) ;
#47883 = ORIENTED_EDGE ( 'NONE', *, *, #37418, .F. ) ;
#47884 = CARTESIAN_POINT ( 'NONE',  ( 4.975801465491695552, -20.67815041659169495, 43.22084481528186473 ) ) ;
#47885 = EDGE_CURVE ( 'NONE', #50643, #8101, #43061, .T. ) ;
#47886 = ORIENTED_EDGE ( 'NONE', *, *, #13814, .F. ) ;
#47887 = CARTESIAN_POINT ( 'NONE',  ( 1.231276596079887264, 41.91134057782999633, -0.8463462572780159343 ) ) ;
#47889 = EDGE_CURVE ( 'NONE', #16525, #4313, #33654, .T. ) ;
#47888 = ORIENTED_EDGE ( 'NONE', *, *, #36593, .F. ) ;
#47890 = ORIENTED_EDGE ( 'NONE', *, *, #58906, .T. ) ;
#47891 = CARTESIAN_POINT ( 'NONE',  ( 0.5806925824938502512, -46.82446035038566379, -2.586943222941716858 ) ) ;
#47892 = CARTESIAN_POINT ( 'NONE',  ( -4.915099999999998914, 12.80000000000000071, -3.000000000000000000 ) ) ;
#47893 = EDGE_CURVE ( 'NONE', #14204, #1298, #24806, .T. ) ;
#47894 = VECTOR ( 'NONE', #7965, 1000.000000000000341 ) ;
#47895 = CARTESIAN_POINT ( 'NONE',  ( 0.9757402383260949108, 33.98983788393820760, 26.18833306844161157 ) ) ;
#47896 = DIRECTION ( 'NONE',  ( 0.000000000000000000, 0.000000000000000000, 1.000000000000000000 ) ) ;
#47897 = VERTEX_POINT ( 'NONE', #42445 ) ;
#47898 = DIRECTION ( 'NONE',  ( -1.000000000000000000, -0.000000000000000000, -0.000000000000000000 ) ) ;
#47899 = EDGE_CURVE ( 'NONE', #54294, #51708, #61507, .T. ) ;
#47900 = CARTESIAN_POINT ( 'NONE',  ( 5.917102823773431552, 8.458006992050780326, 18.24696785151336087 ) ) ;
#47901 = CARTESIAN_POINT ( 'NONE',  ( 0.1147471544378676628, -38.29299291615923551, 21.92256558882251127 ) ) ;
#47902 = ORIENTED_EDGE ( 'NONE', *, *, #32456, .F. ) ;
#47903 = ORIENTED_EDGE ( 'NONE', *, *, #21230, .T. ) ;
#47904 = CARTESIAN_POINT ( 'NONE',  ( 2.301529144917015213, -48.01619158420457723, 1.287519423137106100 ) ) ;
#47905 = FACE_OUTER_BOUND ( 'NONE', #11284, .T. ) ;
#47906 = CARTESIAN_POINT ( 'NONE',  ( 4.956445790443991584, 34.56007374686787159, 31.98654955994301829 ) ) ;
#47907 = CARTESIAN_POINT ( 'NONE',  ( 0.1103744047535531458, -34.23648668783411608, 26.22174028894811926 ) ) ;
#47908 = CARTESIAN_POINT ( 'NONE',  ( 0.2285344041767114198, -42.47718627262295144, 11.92433715794502191 ) ) ;
#47909 = ORIENTED_EDGE ( 'NONE', *, *, #53303, .F. ) ;
#47910 = EDGE_CURVE ( 'NONE', #6891, #36980, #20918, .T. ) ;
#47911 = AXIS2_PLACEMENT_3D ( 'NONE', #23637, #51820, #52747 ) ;
#47912 = ORIENTED_EDGE ( 'NONE', *, *, #15780, .F. ) ;
#47913 = EDGE_CURVE ( 'NONE', #7184, #34476, #28788, .T. ) ;
#47914 = CARTESIAN_POINT ( 'NONE',  ( 0.5987334308729321819, -34.85272393231409893, 34.59552776107961591 ) ) ;
#47915 = CARTESIAN_POINT ( 'NONE',  ( 4.553261556744875094, 42.54662847375985280, -10.92355122382294752 ) ) ;
#47916 = CARTESIAN_POINT ( 'NONE',  ( 0.5824935313925965197, -42.01861599602651864, -20.82484302059208403 ) ) ;
#47917 = CARTESIAN_POINT ( 'NONE',  ( 0.2279481005628796741, -32.21654163078297728, 30.14295825603286971 ) ) ;
#47918 = CARTESIAN_POINT ( 'NONE',  ( 0.9754292580325136797, 41.90451261907242042, 0.5824852461694604022 ) ) ;
#47919 = CARTESIAN_POINT ( 'NONE',  ( 5.974727161628367256, 18.95664195401516849, -7.868887636447420952 ) ) ;
#47920 = AXIS2_PLACEMENT_3D ( 'NONE', #33444, #24336, #33754 ) ;
#47921 = ORIENTED_EDGE ( 'NONE', *, *, #4560, .T. ) ;
#47922 = CARTESIAN_POINT ( 'NONE',  ( -6.063463321072276813, -19.21812676738393222, -1.218218384457852688 ) ) ;
#47923 = DIRECTION ( 'NONE',  ( 0.000000000000000000, 0.000000000000000000, 1.000000000000000000 ) ) ;
#47924 = B_SPLINE_CURVE_WITH_KNOTS ( 'NONE', 3,
 ( #52201, #56596, #9601, #13713 ),
 .UNSPECIFIED., .F., .F.,
 ( 4, 4 ),
 ( 1.409462824231155764E-18, 0.004446298630425058948 ),
 .UNSPECIFIED. ) ;
#47925 = CARTESIAN_POINT ( 'NONE',  ( 0.5809828226811548646, -46.40184912890831015, -11.86925843957216742 ) ) ;
#47926 = CARTESIAN_POINT ( 'NONE',  ( 0.1087620492084206414, -16.16798550313395921, -39.97903073778059024 ) ) ;
#47927 = CARTESIAN_POINT ( 'NONE',  ( 0.5806925824938499181, 40.62497527030964051, -23.42720099863178973 ) ) ;
#47928 = DIRECTION ( 'NONE',  ( -0.9848077530122080203, -0.1736481776669315524, 2.220446049250313574E-16 ) ) ;
#47929 = CARTESIAN_POINT ( 'NONE',  ( 0.6845945791218034371, 17.66463248440769718, -43.45534811625321225 ) ) ;
#47930 = EDGE_CURVE ( 'NONE', #60718, #26211, #31350, .T. ) ;
#47931 = ORIENTED_EDGE ( 'NONE', *, *, #58693, .T. ) ;
#47932 = CARTESIAN_POINT ( 'NONE',  ( 0.8557997880470606944, -11.51622788066425684, -46.50333260518571876 ) ) ;
#47933 = AXIS2_PLACEMENT_3D ( 'NONE', #18365, #17737, #23059 ) ;
#47934 = CARTESIAN_POINT ( 'NONE',  ( 0.3676999524040323597, -40.57213187173838520, -17.31625533148287843 ) ) ;
#47935 = CARTESIAN_POINT ( 'NONE',  ( 0.5827359174754808135, 18.66406616558040454, -44.10985444762169294 ) ) ;
#47936 = CARTESIAN_POINT ( 'NONE',  ( 2.533389852662419894, 40.31838374093042177, 17.66008109417097316 ) ) ;
#47937 = CARTESIAN_POINT ( 'NONE',  ( 0.5782707292762423457, 39.98024706216853019, -24.52174950030242684 ) ) ;
#47938 = ORIENTED_EDGE ( 'NONE', *, *, #4020, .F. ) ;
#47939 = CARTESIAN_POINT ( 'NONE',  ( 8.000000000000000000, 9.184850993605147156E-15, -75.00000000000001421 ) ) ;
#47940 = CARTESIAN_POINT ( 'NONE',  ( 7.000000000000007105, -2.650000000000270806, 80.00000000000000000 ) ) ;
#47941 = ORIENTED_EDGE ( 'NONE', *, *, #43869, .T. ) ;
#47942 = CARTESIAN_POINT ( 'NONE',  ( -6.016104459813374383, -18.68131780085930060, -2.464823636987640398 ) ) ;
#47943 = CIRCLE ( 'NONE', #21919, 4.000000000000000888 ) ;
#47944 = CARTESIAN_POINT ( 'NONE',  ( 2.281351352603294913, -4.956540261593444185, -47.71649595778614383 ) ) ;
#47945 = ORIENTED_EDGE ( 'NONE', *, *, #32777, .T. ) ;
#47946 = FACE_OUTER_BOUND ( 'NONE', #20090, .T. ) ;
#47947 = AXIS2_PLACEMENT_3D ( 'NONE', #32379, #27980, #4147 ) ;
#47948 = ORIENTED_EDGE ( 'NONE', *, *, #59228, .T. ) ;
#47949 = CARTESIAN_POINT ( 'NONE',  ( 0.1073791018717578927, -11.62916352156179123, 41.52698815987148606 ) ) ;
#47950 = VERTEX_POINT ( 'NONE', #54258 ) ;
#47951 = DIRECTION ( 'NONE',  ( 0.000000000000000000, 0.000000000000000000, 1.000000000000000000 ) ) ;
#47952 = CARTESIAN_POINT ( 'NONE',  ( -6.078075953587585900, 19.09862890096253096, -2.457142313838282632 ) ) ;
#47953 = ORIENTED_EDGE ( 'NONE', *, *, #55378, .F. ) ;
#47954 = CARTESIAN_POINT ( 'NONE',  ( 3.680882792899938138, -45.82784180332847512, 14.19444521819950822 ) ) ;
#47955 = VERTEX_POINT ( 'NONE', #6023 ) ;
#47956 = CARTESIAN_POINT ( 'NONE',  ( 0.5848930533535030563, 45.18167862054185235, 12.56538894812371332 ) ) ;
#47957 = FACE_OUTER_BOUND ( 'NONE', #2496, .T. ) ;
#47958 = CARTESIAN_POINT ( 'NONE',  ( 0.9762797500689124330, 35.79768877047989406, -21.79105926469756938 ) ) ;
#47959 = EDGE_CURVE ( 'NONE', #31634, #41223, #10455, .T. ) ;
#47960 = ORIENTED_EDGE ( 'NONE', *, *, #54194, .F. ) ;
#47961 = CARTESIAN_POINT ( 'NONE',  ( 5.896278296736517710, 20.06830682785023612, -1.337924017888618256 ) ) ;
#47962 = B_SPLINE_CURVE_WITH_KNOTS ( 'NONE', 3,
 ( #46021, #22190, #40391, #31583, #7758, #14572, #58062, #48075, #752, #28644, #43705, #9534, #19575, #9859, #33990, #19891 ),
 .UNSPECIFIED., .F., .F.,
 ( 4, 3, 3, 3, 3, 4 ),
 ( 2.501947744657918636E-17, 0.0002612764279487718617, 0.0003919131003184756130, 0.0005225497727000653642, 0.0007837925190632448122, 0.001045051706266714999 ),
 .UNSPECIFIED. ) ;
#47963 = CARTESIAN_POINT ( 'NONE',  ( 0.5832655196449157975, 16.64216000364581305, 43.84374178131214705 ) ) ;
#47964 = EDGE_LOOP ( 'NONE', ( #55536, #46342, #46583, #52631 ) ) ;
#47965 = ADVANCED_FACE ( 'NONE', ( #11699 ), #30553, .F. ) ;
#47966 = CARTESIAN_POINT ( 'NONE',  ( 0.5839879882012688483, -33.86758487442378396, -33.86754218494331781 ) ) ;
#47967 = CARTESIAN_POINT ( 'NONE',  ( 3.407937589446178528, -10.00592723328954570, -9.356405769959156515 ) ) ;
#47969 = EDGE_LOOP ( 'NONE', ( #7410, #41052, #39124, #27295 ) ) ;
#47968 = B_SPLINE_CURVE_WITH_KNOTS ( 'NONE', 3,
 ( #42176, #28048, #32760, #51836, #8938, #47168 ),
 .UNSPECIFIED., .F., .F.,
 ( 4, 2, 4 ),
 ( 1.549946925021254854E-16, 0.0002445252820015224966, 0.0004890505640028900607 ),
 .UNSPECIFIED. ) ;
#47970 = CARTESIAN_POINT ( 'NONE',  ( -2.708315649062916552, -14.54141329178161257, -1.648584381066990678 ) ) ;
#47971 = ORIENTED_EDGE ( 'NONE', *, *, #3147, .T. ) ;
#47972 = AXIS2_PLACEMENT_3D ( 'NONE', #53995, #50242, #2301 ) ;
#47973 = FACE_OUTER_BOUND ( 'NONE', #33571, .T. ) ;
#47974 =( BOUNDED_SURFACE ( )  B_SPLINE_SURFACE ( 3, 1, ( 
 ( #2754, #55676 ),
 ( #13414, #60083 ),
 ( #8374, #36611 ),
 ( #26572, #32521 ) ),
 .UNSPECIFIED., .F., .F., .F. ) 
 B_SPLINE_SURFACE_WITH_KNOTS ( ( 4, 4 ),
 ( 2, 2 ),
 ( 0.000000000000000000, 1.000000000000000000 ),
 ( 0.000000000000000000, 1.000000000000000000 ),
 .UNSPECIFIED. ) 
 GEOMETRIC_REPRESENTATION_ITEM ( )  RATIONAL_B_SPLINE_SURFACE ( (
 ( 1.000000000000000000, 1.000000000000000000),
 ( 0.9952954269826590483, 0.8620686068821339365),
 ( 0.9952954269826590483, 0.8620686068821339365),
 ( 1.000000000000000000, 1.000000000000000000) ) ) 
 REPRESENTATION_ITEM ( '' )  SURFACE ( )  );
#47975 = CARTESIAN_POINT ( 'NONE',  ( 0.5786265663353153954, 0.7221568112306425702, 47.89572889566446179 ) ) ;
#47976 = ORIENTED_EDGE ( 'NONE', *, *, #14753, .F. ) ;
#47977 = CARTESIAN_POINT ( 'NONE',  ( 0.1073791018717483448, -37.58707531572191840, -21.14095454447545919 ) ) ;
#47978 = CARTESIAN_POINT ( 'NONE',  ( 0.1154773475650540254, 25.09645238721858007, -36.29203366611179149 ) ) ;
#47979 = CARTESIAN_POINT ( 'NONE',  ( 0.2940135542859015350, -0.6094639541808186678, 44.11200632911605624 ) ) ;
#47980 = CARTESIAN_POINT ( 'NONE',  ( 4.335381028904216727, -37.95090345676174337, 30.97556737946691285 ) ) ;
#47981 = ADVANCED_FACE ( 'NONE', ( #35198 ), #2930, .F. ) ;
#47982 = AXIS2_PLACEMENT_3D ( 'NONE', #44127, #53165, #28754 ) ;
#47983 = VERTEX_POINT ( 'NONE', #5713 ) ;
#47984 = FACE_OUTER_BOUND ( 'NONE', #42409, .T. ) ;
#47985 = CARTESIAN_POINT ( 'NONE',  ( 0.3676999524040366896, 5.056646555325087000, 43.82215089355334925 ) ) ;
#47986 = EDGE_CURVE ( 'NONE', #14441, #44739, #57498, .T. ) ;
#47987 = CARTESIAN_POINT ( 'NONE',  ( 0.8760168074886965917, 48.09529047980636562, 0.8912768426707960989 ) ) ;
#47988 = B_SPLINE_CURVE_WITH_KNOTS ( 'NONE', 3,
 ( #14980, #52544, #9638, #28749, #58160, #47872, #15283, #4921, #34389, #44124, #29666, #14670, #34091, #48467, #214, #57533 ),
 .UNSPECIFIED., .F., .F.,
 ( 4, 3, 3, 3, 3, 4 ),
 ( 1.250973872328959318E-17, 0.0002732102107931917343, 0.0004098135523333763298, 0.0005464168938824918781, 0.0008195847345945395405, 0.001092771384553104181 ),
 .UNSPECIFIED. ) ;
#47989 = B_SPLINE_CURVE_WITH_KNOTS ( 'NONE', 3,
 ( #27363, #36476, #51772, #3843, #27981, #60549, #42709, #23285, #32079, #56774, #3534, #55541, #42411, #18588, #8239, #9172, #32380, #22668, #61770 ),
 .UNSPECIFIED., .F., .F.,
 ( 4, 3, 3, 3, 3, 3, 4 ),
 ( 8.674294979774126656E-18, 0.0002724573126191752134, 0.0004086839781548500493, 0.0005449106435901828957, 0.0006811373090491488558, 0.0008459866663933638450, 0.001010840725717211197 ),
 .UNSPECIFIED. ) ;
#47990 = CARTESIAN_POINT ( 'NONE',  ( 0.9762797500689124330, -39.42083772998312696, -14.22400568939859866 ) ) ;
#47991 = CARTESIAN_POINT ( 'NONE',  ( 0.5850706913938534814, 37.88789093229845406, -29.30134895053016564 ) ) ;
#47992 = CARTESIAN_POINT ( 'NONE',  ( 0.8744876279028263033, -35.88078294188978390, 33.50999053799454686 ) ) ;
#47993 = CARTESIAN_POINT ( 'NONE',  ( 0.3676999524040323597, -41.19158123804999860, 15.78620342045440239 ) ) ;
#47994 = AXIS2_PLACEMENT_3D ( 'NONE', #12106, #40006, #30870 ) ;
#47995 = CARTESIAN_POINT ( 'NONE',  ( 0.7057020205114998834, 38.50899875908095282, -28.48867101281786773 ) ) ;
#47996 = CARTESIAN_POINT ( 'NONE',  ( -2.569797478183790229, 12.44213550320642625, 7.701637110048724644 ) ) ;
#47997 = CARTESIAN_POINT ( 'NONE',  ( 0.6023142530420679819, 48.10676733004997629, -0.2618396477462503480 ) ) ;
#47998 = CARTESIAN_POINT ( 'NONE',  ( 0.8744876279028306332, 32.34273794994798834, -36.93639603806098393 ) ) ;
#47999 = CARTESIAN_POINT ( 'NONE',  ( -69.95594261585600293, 0.000000000000000000, 0.000000000000000000 ) ) ;
#48000 = CARTESIAN_POINT ( 'NONE',  ( 4.553261556744873317, -29.36425772793689859, 32.66925058691941075 ) ) ;
#48001 = CARTESIAN_POINT ( 'NONE',  ( 4.549368137175248350, 40.58005590356670211, 13.99871866169379508 ) ) ;
#48002 = DIRECTION ( 'NONE',  ( 1.000000000000000000, 0.000000000000000000, 0.000000000000000000 ) ) ;
#48003 = EDGE_CURVE ( 'NONE', #39646, #21594, #32136, .T. ) ;
#48004 = DIRECTION ( 'NONE',  ( 0.02222222222222222307, -0.9997530559290660479, 0.000000000000000000 ) ) ;
#48005 = ORIENTED_EDGE ( 'NONE', *, *, #40620, .F. ) ;
#48006 = CARTESIAN_POINT ( 'NONE',  ( -99.49999999999975842, -9.184850993605117179E-15, 3.081487911019577365E-29 ) ) ;
#48007 = CARTESIAN_POINT ( 'NONE',  ( 4.549368137175248350, -38.59302160394740611, -18.79584381673521065 ) ) ;
#48008 = CARTESIAN_POINT ( 'NONE',  ( 0.5980894510889448457, -24.66136644716850057, 41.31170365136845390 ) ) ;
#48009 = ORIENTED_EDGE ( 'NONE', *, *, #12752, .F. ) ;
#48010 = CARTESIAN_POINT ( 'NONE',  ( 0.9752570700956793015, 5.371905812152142801, 42.57087745267993029 ) ) ;
#48011 = CARTESIAN_POINT ( 'NONE',  ( 5.959547316686252039, -16.28624005235107930, 12.49238070347948870 ) ) ;
#48012 = UNCERTAINTY_MEASURE_WITH_UNIT (LENGTH_MEASURE( 1.000000000000000082E-05 ), #11240, 'distance_accuracy_value', 'NONE');
#48013 = EDGE_LOOP ( 'NONE', ( #57383, #48193, #3517, #24894 ) ) ;
#48014 = ORIENTED_EDGE ( 'NONE', *, *, #3639, .F. ) ;
#48015 = CARTESIAN_POINT ( 'NONE',  ( 0.6253024248130509832, -31.15133493648745855, 37.96101367314130925 ) ) ;
#48016 = VERTEX_POINT ( 'NONE', #11379 ) ;
#48017 = VECTOR ( 'NONE', #46582, 1000.000000000000000 ) ;
#48018 = CARTESIAN_POINT ( 'NONE',  ( 0.9972139404380334637, 25.59643345733279318, -34.43899251299745146 ) ) ;
#48019 = ORIENTED_EDGE ( 'NONE', *, *, #45080, .T. ) ;
#48020 = ORIENTED_EDGE ( 'NONE', *, *, #61644, .T. ) ;
#48021 = ORIENTED_EDGE ( 'NONE', *, *, #38359, .F. ) ;
#48022 = FACE_OUTER_BOUND ( 'NONE', #39756, .T. ) ;
#48023 = PLANE ( 'NONE',  #14107 ) ;
#48024 = CARTESIAN_POINT ( 'NONE',  ( 0.6039202388192952409, -45.45307514328631981, -18.58982713388583008 ) ) ;
#48025 = ORIENTED_EDGE ( 'NONE', *, *, #60446, .T. ) ;
#48026 =( BOUNDED_SURFACE ( )  B_SPLINE_SURFACE ( 3, 1, ( 
 ( #12687, #26761 ),
 ( #47123, #56489 ),
 ( #23303, #31460 ),
 ( #41815, #60881 ) ),
 .UNSPECIFIED., .F., .F., .F. ) 
 B_SPLINE_SURFACE_WITH_KNOTS ( ( 4, 4 ),
 ( 2, 2 ),
 ( 0.000000000000000000, 1.000000000000000000 ),
 ( 0.000000000000000000, 1.000000000000000000 ),
 .UNSPECIFIED. ) 
 GEOMETRIC_REPRESENTATION_ITEM ( )  RATIONAL_B_SPLINE_SURFACE ( (
 ( 1.000000000000000000, 1.000000000000000000),
 ( 0.9953040768229005630, 0.8617119497784937465),
 ( 0.9953040768229005630, 0.8617119497784937465),
 ( 1.000000000000000000, 1.000000000000000000) ) ) 
 REPRESENTATION_ITEM ( '' )  SURFACE ( )  );
#48027 = CLOSED_SHELL ( 'NONE', ( #16345, #50524, #30267, #24660, #45225, #53805, #24460, #20348, #27226, #11884, #16073, #58467, #15641, #24045, #37080, #2034, #1308, #35324, #9709, #3408, #41234, #56482, #58599, #23788, #36878, #57608, #47374, #16635, #5227, #4221, #46567, #31465, #45413, #29416 ) ) ;
#48028 = CARTESIAN_POINT ( 'NONE',  ( 0.9730545539215883499, -34.34678117142538412, -25.71816799638815354 ) ) ;
#48029 = ORIENTED_EDGE ( 'NONE', *, *, #48278, .T. ) ;
#48030 = EDGE_CURVE ( 'NONE', #51786, #7613, #50776, .T. ) ;
#48031 = ORIENTED_EDGE ( 'NONE', *, *, #90, .T. ) ;
#48032 = CARTESIAN_POINT ( 'NONE',  ( 4.967162193818130511, 0.000000000000000000, 0.000000000000000000 ) ) ;
#48033 = VECTOR ( 'NONE', #24082, 1000.000000000000114 ) ;
#48034 = ORIENTED_EDGE ( 'NONE', *, *, #41898, .T. ) ;
#48035 = CARTESIAN_POINT ( 'NONE',  ( 0.6008123274975392114, 46.46679437735655682, 15.88683642047475786 ) ) ;
#48036 = CARTESIAN_POINT ( 'NONE',  ( 0.5980271706414711508, 36.93900200886698570, 32.36602189689958209 ) ) ;
#48037 = CARTESIAN_POINT ( 'NONE',  ( 0.9730545539215883499, -0.5054011016615761465, 42.90536227157002003 ) ) ;
#48038 = CARTESIAN_POINT ( 'NONE',  ( 5.000000000000007994, -56.56854249492410958, 56.56854249492351983 ) ) ;
#48039 = EDGE_CURVE ( 'NONE', #29160, #26818, #6677, .T. ) ;
#48040 = VERTEX_POINT ( 'NONE', #59278 ) ;
#48041 = CARTESIAN_POINT ( 'NONE',  ( 0.6031356755773454870, -12.45109777649142124, 46.46822857981022281 ) ) ;
#48042 = DIRECTION ( 'NONE',  ( -0.07836865515943410021, 0.6006129930017499730, -0.7956898808744407026 ) ) ;
#48043 = EDGE_CURVE ( 'NONE', #32533, #57834, #25350, .T. ) ;
#48044 =( BOUNDED_SURFACE ( )  B_SPLINE_SURFACE ( 3, 1, ( 
 ( #3799, #12312 ),
 ( #8825, #27939 ),
 ( #31402, #17311 ),
 ( #50501, #7573 ) ),
 .UNSPECIFIED., .F., .F., .F. ) 
 B_SPLINE_SURFACE_WITH_KNOTS ( ( 4, 4 ),
 ( 2, 2 ),
 ( 0.000000000000000000, 1.000000000000000000 ),
 ( 0.000000000000000000, 1.000000000000000000 ),
 .UNSPECIFIED. ) 
 GEOMETRIC_REPRESENTATION_ITEM ( )  RATIONAL_B_SPLINE_SURFACE ( (
 ( 1.000000000000000000, 1.000000000000000000),
 ( 0.9754377213608244057, 0.9999580625633939235),
 ( 0.9754377213608244057, 0.9999580625633939235),
 ( 1.000000000000000000, 1.000000000000000000) ) ) 
 REPRESENTATION_ITEM ( '' )  SURFACE ( )  );
#48045 = CARTESIAN_POINT ( 'NONE',  ( 0.8554163680231708922, -46.15020320557310640, 8.447734441619822121 ) ) ;
#48046 = ORIENTED_EDGE ( 'NONE', *, *, #5631, .T. ) ;
#48047 = CARTESIAN_POINT ( 'NONE',  ( 0.1129192098497455998, -35.64954734424960492, 26.00118385641814456 ) ) ;
#48048 = LINE ( 'NONE', #5098, #18657 ) ;
#48049 = CARTESIAN_POINT ( 'NONE',  ( 1.091591847532197956, 33.37174725983657453, -25.35913002808713301 ) ) ;
#48050 = ORIENTED_EDGE ( 'NONE', *, *, #11187, .T. ) ;
#48051 = ORIENTED_EDGE ( 'NONE', *, *, #1373, .T. ) ;
#48052 = CARTESIAN_POINT ( 'NONE',  ( 1.227938101723756947, 39.32113113558990847, -17.20315230597801914 ) ) ;
#48053 = DIRECTION ( 'NONE',  ( 0.09835009131224552170, 0.7941905447268735596, 0.5996571005210433736 ) ) ;
#48054 = CARTESIAN_POINT ( 'NONE',  ( 0.9972139404380309102, -17.02682566833155420, -39.38665787682681696 ) ) ;
#48055 = EDGE_CURVE ( 'NONE', #25998, #15054, #44002, .T. ) ;
#48056 = CARTESIAN_POINT ( 'NONE',  ( 0.7056313189692664523, -41.47346934225711834, 21.90205434826647490 ) ) ;
#48057 = CARTESIAN_POINT ( 'NONE',  ( 2.301430502907646058, -13.67112791032074703, 46.04685681264140840 ) ) ;
#48058 = CARTESIAN_POINT ( 'NONE',  ( 0.1147471544378676767, -31.47985608552908587, 30.91877826350230762 ) ) ;
#48059 = SURFACE_SIDE_STYLE ('',( #9839 ) ) ;
#48060 = CARTESIAN_POINT ( 'NONE',  ( 4.291220156522059348, -28.73895862173575821, -37.32909394351617749 ) ) ;
#48061 = CARTESIAN_POINT ( 'NONE',  ( 0.6000166863083106206, 44.01764848084250303, 21.77774331572114264 ) ) ;
#48062 = CARTESIAN_POINT ( 'NONE',  ( -6.072942160501519027, 19.10003410082485331, -2.448031788263385522 ) ) ;
#48063 = CARTESIAN_POINT ( 'NONE',  ( 5.880360259849752858, 31.66572319753561970, -36.03610316515350576 ) ) ;
#48064 = DIRECTION ( 'NONE',  ( -1.000000000000000000, -1.836909530733573529E-16, 1.361838123766461297E-32 ) ) ;
#48065 = ORIENTED_EDGE ( 'NONE', *, *, #15513, .T. ) ;
#48066 = CARTESIAN_POINT ( 'NONE',  ( 4.975610109902397937, -37.61482235126130291, -31.26618855282533360 ) ) ;
#48067 = CARTESIAN_POINT ( 'NONE',  ( 0.1092565886968784455, -34.40108480122233914, -26.00565248013041142 ) ) ;
#48068 = DIRECTION ( 'NONE',  ( 1.836909530733573776E-16, -1.000000000000000000, 0.000000000000000000 ) ) ;
#48069 = CARTESIAN_POINT ( 'NONE',  ( 0.8760168074886965917, -0.8912768426709639646, 48.09529047980636562 ) ) ;
#48070 = CARTESIAN_POINT ( 'NONE',  ( 0.8744876279028306332, -48.57046782678520458, 7.159588358747709158 ) ) ;
#48071 = CARTESIAN_POINT ( 'NONE',  ( 0.9762797500689124330, 19.69530149098661909, 36.99215976885973589 ) ) ;
#48072 = ITEM_DEFINED_TRANSFORMATION ( 'NONE', 'NONE', #52907,  #14677 ) ;
#48073 = CARTESIAN_POINT ( 'NONE',  ( 4.956653778116991482, 20.77844580450620526, -43.37017594958032873 ) ) ;
#48074 = AXIS2_PLACEMENT_3D ( 'NONE', #53838, #34158, #291 ) ;
#48075 = CARTESIAN_POINT ( 'NONE',  ( 0.6028777368367060907, 22.79122549791117436, -43.49827432915513015 ) ) ;
#48076 = CARTESIAN_POINT ( 'NONE',  ( 0.6029443449137436017, -30.65199525294410421, 38.36658344180290214 ) ) ;
#48077 = DIRECTION ( 'NONE',  ( -0.000000000000000000, -0.000000000000000000, 1.000000000000000000 ) ) ;
#48078 = CARTESIAN_POINT ( 'NONE',  ( -6.078726893082806448, 3.069885851706565916, -19.00973019603939917 ) ) ;
#48080 = ORIENTED_EDGE ( 'NONE', *, *, #9400, .T. ) ;
#48079 = CARTESIAN_POINT ( 'NONE',  ( 1.231276596079881935, 38.91607545535268997, -15.58254928345689017 ) ) ;
#48081 = ORIENTED_EDGE ( 'NONE', *, *, #4675, .T. ) ;
#48082 = CARTESIAN_POINT ( 'NONE',  ( 0.2224561200757635415, -37.71651051365644491, 20.89867881469703548 ) ) ;
#48083 = CARTESIAN_POINT ( 'NONE',  ( 0.1368894036331282649, 14.63874681665168964, -41.62413263434208943 ) ) ;
#48084 = CARTESIAN_POINT ( 'NONE',  ( 4.322998006666179727, 36.74401119231410462, -30.86725474310321360 ) ) ;
#48085 = EDGE_CURVE ( 'NONE', #56336, #1542, #44829, .T. ) ;
#48086 = VERTEX_POINT ( 'NONE', #55507 ) ;
#48087 = CARTESIAN_POINT ( 'NONE',  ( 0.8753041380234530822, -2.462982411634171864, -49.04153388213872944 ) ) ;
#48088 = LINE ( 'NONE', #10179, #43214 ) ;
#48089 = FACE_OUTER_BOUND ( 'NONE', #3429, .T. ) ;
#48090 = B_SPLINE_CURVE_WITH_KNOTS ( 'NONE', 3,
 ( #54583, #60526, #36453, #12038 ),
 .UNSPECIFIED., .F., .F.,
 ( 4, 4 ),
 ( 3.127317220692750759E-18, 0.004050076154993002484 ),
 .UNSPECIFIED. ) ;
#48091 = EDGE_CURVE ( 'NONE', #27049, #25537, #17040, .T. ) ;
#48092 = ORIENTED_EDGE ( 'NONE', *, *, #55697, .T. ) ;
#48093 = ORIENTED_EDGE ( 'NONE', *, *, #48494, .T. ) ;
#48094 = CARTESIAN_POINT ( 'NONE',  ( 0.2224561200757595725, 17.20021002050924963, -39.54039348282962152 ) ) ;
#48095 = EDGE_CURVE ( 'NONE', #53301, #52962, #58166, .T. ) ;
#48096 = CARTESIAN_POINT ( 'NONE',  ( 0.8744876279028263033, -6.955970791787605911, -48.60004650947661275 ) ) ;
#48097 = FACE_OUTER_BOUND ( 'NONE', #15279, .T. ) ;
#48098 = CARTESIAN_POINT ( 'NONE',  ( 0.5997462898726536595, -47.63132954987522538, -11.95023328037962251 ) ) ;
#48099 = CARTESIAN_POINT ( 'NONE',  ( 2.528100132419517365, -5.786187675422820753, 41.57852583746639397 ) ) ;
#48100 = B_SPLINE_CURVE_WITH_KNOTS ( 'NONE', 3,
 ( #27471, #176, #52501, #47515 ),
 .UNSPECIFIED., .F., .F.,
 ( 4, 4 ),
 ( 1.734723475976807094E-18, 0.004050076154993000749 ),
 .UNSPECIFIED. ) ;
#48101 = CARTESIAN_POINT ( 'NONE',  ( 0.5839880159502333079, 38.02605095487717790, -29.12121614504424372 ) ) ;
#48102 = VERTEX_POINT ( 'NONE', #17628 ) ;
#48103 = ADVANCED_FACE ( 'NONE', ( #36437 ), #47773, .F. ) ;
#48104 = ORIENTED_EDGE ( 'NONE', *, *, #37151, .F. ) ;
#48105 = CARTESIAN_POINT ( 'NONE',  ( 4.975801465491694664, 21.70134120755201224, -42.71626295676241369 ) ) ;
#48106 = CARTESIAN_POINT ( 'NONE',  ( 2.185380717157383135, 44.01027289648202867, 1.384081877772499691 ) ) ;
#48107 = ORIENTED_EDGE ( 'NONE', *, *, #41870, .T. ) ;
#48108 = DIRECTION ( 'NONE',  ( -1.000000000000000000, -0.000000000000000000, -0.000000000000000000 ) ) ;
#48109 = CARTESIAN_POINT ( 'NONE',  ( 0.5806925824938502512, 28.25565086187734920, 37.42780459384778879 ) ) ;
#48110 = CARTESIAN_POINT ( 'NONE',  ( 4.549368137175248350, -40.71620287708353914, 13.59764261105679317 ) ) ;
#48111 = DIRECTION ( 'NONE',  ( 0.000000000000000000, 0.000000000000000000, 1.000000000000000000 ) ) ;
#48112 = ORIENTED_EDGE ( 'NONE', *, *, #29156, .F. ) ;
#48113 = ORIENTED_EDGE ( 'NONE', *, *, #40702, .T. ) ;
#48114 = DIRECTION ( 'NONE',  ( 0.000000000000000000, 0.000000000000000000, 1.000000000000000000 ) ) ;
#48115 = CARTESIAN_POINT ( 'NONE',  ( 0.9752570700956786354, -42.51066151201240473, -5.829291291129111485 ) ) ;
#48116 = ADVANCED_FACE ( 'NONE', ( #46452 ), #11736, .F. ) ;
#48117 = CARTESIAN_POINT ( 'NONE',  ( 0.5850706913938534814, -6.071602062250944343, 47.50996714391780529 ) ) ;
#48118 = CIRCLE ( 'NONE', #51135, 42.92674063221959813 ) ;
#48119 = CARTESIAN_POINT ( 'NONE',  ( 0.5837374860065642768, 29.30115996485994501, 37.88763545422886381 ) ) ;
#48120 = ORIENTED_EDGE ( 'NONE', *, *, #56283, .F. ) ;
#48121 = CARTESIAN_POINT ( 'NONE',  ( -6.017396004339686577, 18.20079405513556736, -4.878103249820876286 ) ) ;
#48122 = ORIENTED_EDGE ( 'NONE', *, *, #9277, .T. ) ;
#48123 = CARTESIAN_POINT ( 'NONE',  ( 0.5797568599927149791, -44.09074186209018364, -15.97597542316375119 ) ) ;
#48124 = CARTESIAN_POINT ( 'NONE',  ( 0.1149546198390367369, 9.551346850799093957, 43.07804937968931114 ) ) ;
#48125 =( BOUNDED_SURFACE ( )  B_SPLINE_SURFACE ( 3, 1, ( 
 ( #38853, #52916 ),
 ( #39162, #43867 ),
 ( #9382, #33524 ),
 ( #57908, #15035 ) ),
 .UNSPECIFIED., .F., .F., .F. ) 
 B_SPLINE_SURFACE_WITH_KNOTS ( ( 4, 4 ),
 ( 2, 2 ),
 ( 0.000000000000000000, 1.000000000000000000 ),
 ( 0.000000000000000000, 1.000000000000000000 ),
 .UNSPECIFIED. ) 
 GEOMETRIC_REPRESENTATION_ITEM ( )  RATIONAL_B_SPLINE_SURFACE ( (
 ( 1.000000000000000000, 1.000000000000000000),
 ( 0.7211978278499970862, 0.9934217856018976445),
 ( 0.7211978278499970862, 0.9934217856018976445),
 ( 1.000000000000000000, 1.000000000000000000) ) ) 
 REPRESENTATION_ITEM ( '' )  SURFACE ( )  );
#48126 = ORIENTED_EDGE ( 'NONE', *, *, #48055, .F. ) ;
#48127 = B_SPLINE_CURVE_WITH_KNOTS ( 'NONE', 3,
 ( #11268, #35398, #26279, #26587 ),
 .UNSPECIFIED., .F., .F.,
 ( 4, 4 ),
 ( 7.757919228897728493E-18, 0.005013413432710142441 ),
 .UNSPECIFIED. ) ;
#48128 = CARTESIAN_POINT ( 'NONE',  ( 0.5832367798473397924, -47.44985149964044524, -6.521664418777663563 ) ) ;
#48129 = CARTESIAN_POINT ( 'NONE',  ( 0.9722240741986378776, -39.86121768686897582, 15.88116971565374236 ) ) ;
#48130 = EDGE_CURVE ( 'NONE', #45673, #5852, #41030, .T. ) ;
#48131 = ORIENTED_EDGE ( 'NONE', *, *, #50356, .T. ) ;
#48132 = CARTESIAN_POINT ( 'NONE',  ( 0.6254311100348639574, 47.77988293940229170, -5.596225872411531910 ) ) ;
#48133 = FACE_OUTER_BOUND ( 'NONE', #14811, .T. ) ;
#48134 = CARTESIAN_POINT ( 'NONE',  ( -6.077587904424778920, -8.912150607695132010, -17.06955163264957420 ) ) ;
#48135 = CARTESIAN_POINT ( 'NONE',  ( 0.6009453534118438522, 29.63106322864184605, -37.89911869481701956 ) ) ;
#48136 = CARTESIAN_POINT ( 'NONE',  ( 4.956653778116480780, -21.75875759808806720, 42.88673967249081898 ) ) ;
#48137 = ORIENTED_EDGE ( 'NONE', *, *, #11415, .F. ) ;
#48138 = DIRECTION ( 'NONE',  ( 0.000000000000000000, 0.000000000000000000, 1.000000000000000000 ) ) ;
#48139 = CARTESIAN_POINT ( 'NONE',  ( 42.00000000000000711, 7.805869035311033600E-47, 13.00000000000000178 ) ) ;
#48140 =( BOUNDED_SURFACE ( )  B_SPLINE_SURFACE ( 3, 1, ( 
 ( #40704, #31584 ),
 ( #31275, #59774 ),
 ( #2751, #21883 ),
 ( #41616, #41021 ) ),
 .UNSPECIFIED., .F., .F., .F. ) 
 B_SPLINE_SURFACE_WITH_KNOTS ( ( 4, 4 ),
 ( 2, 2 ),
 ( 0.000000000000000000, 1.000000000000000000 ),
 ( 0.000000000000000000, 1.000000000000000000 ),
 .UNSPECIFIED. ) 
 GEOMETRIC_REPRESENTATION_ITEM ( )  RATIONAL_B_SPLINE_SURFACE ( (
 ( 1.000000000000000000, 1.000000000000000000),
 ( 0.7223157951917480446, 0.9931996967497186413),
 ( 0.7223157951917480446, 0.9931996967497186413),
 ( 1.000000000000000000, 1.000000000000000000) ) ) 
 REPRESENTATION_ITEM ( '' )  SURFACE ( )  );
#48141 = CARTESIAN_POINT ( 'NONE',  ( -90.00000000000000000, 0.000000000000000000, -6.887500000000022382 ) ) ;
#48142 = ORIENTED_EDGE ( 'NONE', *, *, #53926, .T. ) ;
#48143 = B_SPLINE_CURVE_WITH_KNOTS ( 'NONE', 3,
 ( #28724, #13717, #56907, #19040, #24025, #4579 ),
 .UNSPECIFIED., .F., .F.,
 ( 4, 2, 4 ),
 ( 7.208110037058612184E-18, 0.0002291472222819933421, 0.0004582944445639794743 ),
 .UNSPECIFIED. ) ;
#48145 = DIRECTION ( 'NONE',  ( -1.000000000000000000, -0.000000000000000000, -0.000000000000000000 ) ) ;
#48144 =( BOUNDED_SURFACE ( )  B_SPLINE_SURFACE ( 3, 1, ( 
 ( #1712, #1104 ),
 ( #485, #57803 ),
 ( #43763, #20850 ),
 ( #24939, #29618 ) ),
 .UNSPECIFIED., .F., .F., .F. ) 
 B_SPLINE_SURFACE_WITH_KNOTS ( ( 4, 4 ),
 ( 2, 2 ),
 ( 0.000000000000000000, 1.000000000000000000 ),
 ( 0.000000000000000000, 1.000000000000000000 ),
 .UNSPECIFIED. ) 
 GEOMETRIC_REPRESENTATION_ITEM ( )  RATIONAL_B_SPLINE_SURFACE ( (
 ( 1.000000000000000000, 1.000000000000000000),
 ( 0.9751682680413298332, 0.9999560080971552356),
 ( 0.9751682680413298332, 0.9999560080971552356),
 ( 1.000000000000000000, 1.000000000000000000) ) ) 
 REPRESENTATION_ITEM ( '' )  SURFACE ( )  );
#48146 = CARTESIAN_POINT ( 'NONE',  ( 0.5997462898726536595, 22.24958391914503153, 43.77793560195857481 ) ) ;
#48147 = CARTESIAN_POINT ( 'NONE',  ( 4.962356264823608143, 41.32726869310149453, -7.955655864260332777 ) ) ;
#48148 = CARTESIAN_POINT ( 'NONE',  ( 4.975801465491694664, 3.702618843597456522, -47.76942479135481534 ) ) ;
#48149 = DIRECTION ( 'NONE',  ( -1.000000000000000000, 0.000000000000000000, 0.000000000000000000 ) ) ;
#48150 = CARTESIAN_POINT ( 'NONE',  ( 0.5980894510889457338, -11.77356634613350295, 46.65000524237065349 ) ) ;
#48151 = DIRECTION ( 'NONE',  ( 0.000000000000000000, 0.000000000000000000, 1.000000000000000000 ) ) ;
#48152 = CARTESIAN_POINT ( 'NONE',  ( 0.6253024248130502061, -30.07742766060853867, -38.81742614778193001 ) ) ;
#48153 = CARTESIAN_POINT ( 'NONE',  ( 4.549368137175248350, 0.000000000000000000, 0.000000000000000000 ) ) ;
#48154 = CARTESIAN_POINT ( 'NONE',  ( 0.9754292580325134576, -11.85895070474203195, -40.19568080138092370 ) ) ;
#48155 = B_SPLINE_CURVE_WITH_KNOTS ( 'NONE', 3,
 ( #37733, #33026, #61788, #53322, #10747, #49556 ),
 .UNSPECIFIED., .F., .F.,
 ( 4, 2, 4 ),
 ( 8.547914836739548796E-17, 0.0002293366620881453642, 0.0004586733241762052391 ),
 .UNSPECIFIED. ) ;
#48157 = ORIENTED_EDGE ( 'NONE', *, *, #3280, .F. ) ;
#48156 = CARTESIAN_POINT ( 'NONE',  ( 1.231276596079881047, -0.5545928549373742023, -41.91621640586514985 ) ) ;
#48158 = ORIENTED_EDGE ( 'NONE', *, *, #2245, .T. ) ;
#48159 = CARTESIAN_POINT ( 'NONE',  ( 4.999999999999986677, 54.69470952478017978, -58.44237546506749226 ) ) ;
#48160 = DIRECTION ( 'NONE',  ( 0.09722883295013595717, 0.5631913828983637904, -0.8205863880617221273 ) ) ;
#48161 = EDGE_CURVE ( 'NONE', #12689, #14433, #32040, .T. ) ;
#48162 = CARTESIAN_POINT ( 'NONE',  ( 0.5998501479064708430, -48.10473956285919428, -0.5236536531313246146 ) ) ;
#48163 = DIRECTION ( 'NONE',  ( 0.000000000000000000, 0.000000000000000000, 1.000000000000000000 ) ) ;
#48164 = CARTESIAN_POINT ( 'NONE',  ( 5.894904586330512508, -11.93156318453012332, 16.19157842939372216 ) ) ;
#48165 = ADVANCED_FACE ( 'NONE', ( #3497 ), #60547, .F. ) ;
#48166 = CONICAL_SURFACE ( 'NONE', #38212, 42.08604991992415023, 1.569615340895231137 ) ;
#48167 = CIRCLE ( 'NONE', #61101, 2.649999999999992806 ) ;
#48168 = VERTEX_POINT ( 'NONE', #4406 ) ;
#48169 = CARTESIAN_POINT ( 'NONE',  ( 0.1119899015040011769, -22.39194001793237021, -38.02055142190635451 ) ) ;
#48170 = ADVANCED_FACE ( 'NONE', ( #33279 ), #58909, .F. ) ;
#48171 = ADVANCED_FACE ( 'NONE', ( #47073 ), #22157, .F. ) ;
#48172 = DIRECTION ( 'NONE',  ( -1.000000000000000000, -0.000000000000000000, -0.000000000000000000 ) ) ;
#48173 = ADVANCED_FACE ( 'NONE', ( #56433 ), #43777, .F. ) ;
#48174 = CARTESIAN_POINT ( 'NONE',  ( 4.549368137175248350, 8.582197505784431968, -42.06008734272388239 ) ) ;
#48175 = ORIENTED_EDGE ( 'NONE', *, *, #1824, .T. ) ;
#48176 = B_SPLINE_CURVE_WITH_KNOTS ( 'NONE', 3,
 ( #8790, #22595, #3457, #23206 ),
 .UNSPECIFIED., .F., .F.,
 ( 4, 4 ),
 ( 0.000000000000000000, 0.004447772540403838876 ),
 .UNSPECIFIED. ) ;
#48177 = CARTESIAN_POINT ( 'NONE',  ( 0.5838002273316440505, 47.50378804015153378, -6.116619957188266454 ) ) ;
#48178 = ORIENTED_EDGE ( 'NONE', *, *, #14284, .F. ) ;
#48179 = ADVANCED_FACE ( 'NONE', ( #43611 ), #50503, .F. ) ;
#48180 = CARTESIAN_POINT ( 'NONE',  ( 9.999999999999994671, 54.69470952478017978, -58.44237546506749226 ) ) ;
#48181 = ORIENTED_EDGE ( 'NONE', *, *, #9772, .T. ) ;
#48182 = EDGE_CURVE ( 'NONE', #50188, #7184, #3578, .T. ) ;
#48183 = CARTESIAN_POINT ( 'NONE',  ( 0.7954190325252786797, -13.28627193046336963, -46.22745637125036211 ) ) ;
#48184 = CARTESIAN_POINT ( 'NONE',  ( 0.6029303876144825880, 33.92442033626736020, 34.10953954078152606 ) ) ;
#48185 = ORIENTED_EDGE ( 'NONE', *, *, #60803, .T. ) ;
#48186 = CARTESIAN_POINT ( 'NONE',  ( 5.901463166500146684, 19.00451910135517508, 6.583777340316350646 ) ) ;
#48187 = CARTESIAN_POINT ( 'NONE',  ( 5.895881250540457863, 18.99851645375293785, 6.601822033710092796 ) ) ;
#48188 = CARTESIAN_POINT ( 'NONE',  ( 1.231276596079887264, -16.87422718933211030, 38.37365278131431268 ) ) ;
#48189 = FACE_OUTER_BOUND ( 'NONE', #51164, .T. ) ;
#48190 = B_SPLINE_CURVE_WITH_KNOTS ( 'NONE', 3,
 ( #31563, #17468, #60661, #27173, #40685, #60063 ),
 .UNSPECIFIED., .F., .F.,
 ( 4, 2, 4 ),
 ( 1.267602517345562747E-16, 0.0002450741128632333721, 0.0004901482257263400011 ),
 .UNSPECIFIED. ) ;
#48191 = ORIENTED_EDGE ( 'NONE', *, *, #12076, .F. ) ;
#48192 = CARTESIAN_POINT ( 'NONE',  ( 0.9762797500689124330, -7.469026406145721886, -41.23758515880873432 ) ) ;
#48193 = ORIENTED_EDGE ( 'NONE', *, *, #57466, .T. ) ;
#48194 = CARTESIAN_POINT ( 'NONE',  ( 4.975801465491694664, -43.22084481528235500, 20.67815041659062913 ) ) ;
#48195 = EDGE_LOOP ( 'NONE', ( #15813, #45206, #1182, #13998 ) ) ;
#48196 = ORIENTED_EDGE ( 'NONE', *, *, #41476, .T. ) ;
#48197 = LINE ( 'NONE', #1477, #44689 ) ;
#48198 = CARTESIAN_POINT ( 'NONE',  ( 5.959828726073459926, -20.34941966491241061, 2.683617577144038258 ) ) ;
#48199 = B_SPLINE_CURVE_WITH_KNOTS ( 'NONE', 3,
 ( #41726, #37962, #33552, #46418, #60787, #3464 ),
 .UNSPECIFIED., .F., .F.,
 ( 4, 2, 4 ),
 ( 8.554130121340520410E-17, 0.0002293366620881455268, 0.0004586733241762055101 ),
 .UNSPECIFIED. ) ;
#48200 = CARTESIAN_POINT ( 'NONE',  ( 0.3622758884714600280, 20.83792692158919735, 37.74294673546592804 ) ) ;
#48201 = ORIENTED_EDGE ( 'NONE', *, *, #50700, .T. ) ;
#48202 = CARTESIAN_POINT ( 'NONE',  ( 2.643462169533613793, -30.32726672320774242, -37.25264019563404361 ) ) ;
#48203 = CARTESIAN_POINT ( 'NONE',  ( -6.001507490154111224, 17.40350523682695183, 7.225628667346644107 ) ) ;
#48204 = CARTESIAN_POINT ( 'NONE',  ( -6.077587904424778920, 19.25606354205735116, 0.006185319731012296589 ) ) ;
#48206 = EDGE_LOOP ( 'NONE', ( #7680, #8134, #36882, #42826 ) ) ;
#48205 = EDGE_CURVE ( 'NONE', #26015, #47983, #32803, .T. ) ;
#48207 = ORIENTED_EDGE ( 'NONE', *, *, #38786, .F. ) ;
#48208 = CYLINDRICAL_SURFACE ( 'NONE', #4472, 13.00000000000000178 ) ;
#48210 = EDGE_CURVE ( 'NONE', #29821, #8960, #15597, .T. ) ;
#48209 = CARTESIAN_POINT ( 'NONE',  ( 0.8560838555295223751, 9.983184696771347788, -45.83349056521751663 ) ) ;
#48211 = CARTESIAN_POINT ( 'NONE',  ( 4.967162193818130511, 0.000000000000000000, 0.000000000000000000 ) ) ;
#48212 = CARTESIAN_POINT ( 'NONE',  ( 5.901463166500145796, -7.242130809805398250, 18.76351277544543450 ) ) ;
#48213 = CARTESIAN_POINT ( 'NONE',  ( 0.9972139404380300221, -26.64066783422312668, -33.63772329383408533 ) ) ;
#48214 = ORIENTED_EDGE ( 'NONE', *, *, #41247, .F. ) ;
#48215 = ORIENTED_EDGE ( 'NONE', *, *, #1761, .F. ) ;
#48216 = CARTESIAN_POINT ( 'NONE',  ( 0.6009453534118438522, 12.02914401651108101, 46.57942464365178381 ) ) ;
#48217 = CARTESIAN_POINT ( 'NONE',  ( 0.5997462898726536595, -19.39900779840410294, -45.11352487427429736 ) ) ;
#48219 = CARTESIAN_POINT ( 'NONE',  ( -5.995132425357893702, -17.41298668506965441, -7.203480333239262734 ) ) ;
#48218 = B_SPLINE_CURVE_WITH_KNOTS ( 'NONE', 3,
 ( #19974, #29964, #39088, #10555 ),
 .UNSPECIFIED., .F., .F.,
 ( 4, 4 ),
 ( 1.517883041479706015E-18, 0.004444878191957669575 ),
 .UNSPECIFIED. ) ;
#48220 = CARTESIAN_POINT ( 'NONE',  ( 0.9740398440564320692, -21.09418882170562881, 37.36539512268012686 ) ) ;
#48221 = CARTESIAN_POINT ( 'NONE',  ( -6.017396004339687465, 16.31924478664288358, -9.420565012089255674 ) ) ;
#48222 = CARTESIAN_POINT ( 'NONE',  ( 1.231276596079881047, 20.88402890667877898, -36.34740854095476692 ) ) ;
#48223 = B_SPLINE_CURVE_WITH_KNOTS ( 'NONE', 3,
 ( #28851, #322, #23, #9744, #33572, #9431 ),
 .UNSPECIFIED., .F., .F.,
 ( 4, 2, 4 ),
 ( 6.805474077711127748E-18, 0.0002291472222819918513, 0.0004582944445639769264 ),
 .UNSPECIFIED. ) ;
#48224 =( BOUNDED_SURFACE ( )  B_SPLINE_SURFACE ( 3, 1, ( 
 ( #24637, #5193 ),
 ( #500, #4571 ),
 ( #48744, #47522 ),
 ( #14025, #19641 ) ),
 .UNSPECIFIED., .F., .F., .F. ) 
 B_SPLINE_SURFACE_WITH_KNOTS ( ( 4, 4 ),
 ( 2, 2 ),
 ( 0.000000000000000000, 1.000000000000000000 ),
 ( 0.000000000000000000, 1.000000000000000000 ),
 .UNSPECIFIED. ) 
 GEOMETRIC_REPRESENTATION_ITEM ( )  RATIONAL_B_SPLINE_SURFACE ( (
 ( 1.000000000000000000, 1.000000000000000000),
 ( 0.9729067724841187204, 0.9999501103223794596),
 ( 0.9729067724841187204, 0.9999501103223794596),
 ( 1.000000000000000000, 1.000000000000000000) ) ) 
 REPRESENTATION_ITEM ( '' )  SURFACE ( )  );
#48225 = EDGE_LOOP ( 'NONE', ( #33633, #31333, #42904, #42116 ) ) ;
#48226 = CARTESIAN_POINT ( 'NONE',  ( 3.660176727303412036, -22.37119938028460453, -42.51126973288305066 ) ) ;
#48227 = FACE_OUTER_BOUND ( 'NONE', #40218, .T. ) ;
#48228 = CARTESIAN_POINT ( 'NONE',  ( 0.1158403557922069033, 29.63666118841771535, 32.68957969730956847 ) ) ;
#48229 =( BOUNDED_SURFACE ( )  B_SPLINE_SURFACE ( 3, 1, ( 
 ( #10435, #5396 ),
 ( #44901, #15139 ),
 ( #48954, #29525 ),
 ( #44584, #30442 ) ),
 .UNSPECIFIED., .F., .F., .F. ) 
 B_SPLINE_SURFACE_WITH_KNOTS ( ( 4, 4 ),
 ( 2, 2 ),
 ( 0.000000000000000000, 1.000000000000000000 ),
 ( 0.000000000000000000, 1.000000000000000000 ),
 .UNSPECIFIED. ) 
 GEOMETRIC_REPRESENTATION_ITEM ( )  RATIONAL_B_SPLINE_SURFACE ( (
 ( 1.000000000000000000, 1.000000000000000000),
 ( 0.7223157951917476005, 0.9931996967497186413),
 ( 0.7223157951917476005, 0.9931996967497186413),
 ( 1.000000000000000000, 1.000000000000000000) ) ) 
 REPRESENTATION_ITEM ( '' )  SURFACE ( )  );
#48230 = CARTESIAN_POINT ( 'NONE',  ( 4.975801465491695552, 32.01766832630263337, 35.64402118370968964 ) ) ;
#48231 = LINE ( 'NONE', #43545, #31202 ) ;
#48232 = CARTESIAN_POINT ( 'NONE',  ( 0.9789889208857693870, -34.49671343044144578, 23.79730364012634070 ) ) ;
#48233 = CARTESIAN_POINT ( 'NONE',  ( 1.231276596079881047, -6.136529359146127405, -41.46829847537036784 ) ) ;
#48234 = EDGE_CURVE ( 'NONE', #28122, #60037, #58763, .T. ) ;
#48235 = ORIENTED_EDGE ( 'NONE', *, *, #8973, .T. ) ;
#48236 = CARTESIAN_POINT ( 'NONE',  ( 2.526552050251864578, -6.809858322089334948, 42.43615142762123327 ) ) ;
#48237 = EDGE_CURVE ( 'NONE', #25596, #48917, #25230, .T. ) ;
#48238 = CARTESIAN_POINT ( 'NONE',  ( 0.5807400328401574052, 29.58941477093014782, 37.66660715020876893 ) ) ;
#48239 = CARTESIAN_POINT ( 'NONE',  ( 0.6029443199889047422, -47.50135088858169752, -12.45629582236396082 ) ) ;
#48240 = CARTESIAN_POINT ( 'NONE',  ( 0.7413678028165007206, 40.12541269520018261, 18.28762827187034645 ) ) ;
#48241 = CARTESIAN_POINT ( 'NONE',  ( 4.967162193818130511, -36.06913038482816347, 23.56777426397165698 ) ) ;
#48242 = EDGE_CURVE ( 'NONE', #25196, #57230, #18587, .T. ) ;
#48243 = ORIENTED_EDGE ( 'NONE', *, *, #6408, .F. ) ;
#48244 = CARTESIAN_POINT ( 'NONE',  ( 0.9754402186311937895, -37.06569162601115153, 21.61645729243100433 ) ) ;
#48245 = CARTESIAN_POINT ( 'NONE',  ( 2.282816707992320282, 26.79502893056672264, -38.58138658755097339 ) ) ;
#48246 = COLOUR_RGB ( '', 0.72549020, 0.75294118, 0.79215686) ;
#48247 = ADVANCED_BREP_SHAPE_REPRESENTATION ( '', ( #30206, #14677 ), #61711 ) ;
#48248 = CARTESIAN_POINT ( 'NONE',  ( -6.077587904424778920, -6.644566705894775716, -18.07334376049006508 ) ) ;
#48249 = CIRCLE ( 'NONE', #33233, 2.649999999999997691 ) ;
#48250 = ORIENTED_EDGE ( 'NONE', *, *, #732, .T. ) ;
#48251 = DIRECTION ( 'NONE',  ( 0.000000000000000000, 0.000000000000000000, 1.000000000000000000 ) ) ;
#48252 = CARTESIAN_POINT ( 'NONE',  ( 1.227938101723756947, -11.92353943227920610, -41.23019537246722876 ) ) ;
#48253 = ORIENTED_EDGE ( 'NONE', *, *, #17141, .T. ) ;
#48254 = CARTESIAN_POINT ( 'NONE',  ( 0.2885697896453109368, -17.24062360132741389, 39.51953439758081288 ) ) ;
#48255 = ORIENTED_EDGE ( 'NONE', *, *, #13045, .T. ) ;
#48256 = DIRECTION ( 'NONE',  ( 0.000000000000000000, 0.000000000000000000, 1.000000000000000000 ) ) ;
#48257 = ORIENTED_EDGE ( 'NONE', *, *, #1457, .F. ) ;
#48258 = CARTESIAN_POINT ( 'NONE',  ( 0.2940135542859009798, -13.32164043950363030, -42.05680021937001101 ) ) ;
#48259 = CARTESIAN_POINT ( 'NONE',  ( 0.5850706913938533704, 41.38834827854208243, 24.10530971368303099 ) ) ;
#48260 = ORIENTED_EDGE ( 'NONE', *, *, #46232, .F. ) ;
#48261 = CARTESIAN_POINT ( 'NONE',  ( 3.661921753702003457, -47.02171908594613825, -1.260578453094312934 ) ) ;
#48262 = EDGE_LOOP ( 'NONE', ( #42978, #22889, #7326, #25430 ) ) ;
#48263 = LINE ( 'NONE', #52944, #54753 ) ;
#48264 = LINE ( 'NONE', #5317, #18738 ) ;
#48265 = CARTESIAN_POINT ( 'NONE',  ( 0.3622758884714730732, 25.58609868863768355, -34.70015533914803285 ) ) ;
#48266 = B_SPLINE_CURVE_WITH_KNOTS ( 'NONE', 3,
 ( #12717, #40005, #7668, #26173, #16794, #59058 ),
 .UNSPECIFIED., .F., .F.,
 ( 4, 2, 4 ),
 ( 5.294859796737922701E-18, 0.0002445244328975365350, 0.0004890488657950677574 ),
 .UNSPECIFIED. ) ;
#48267 = ORIENTED_EDGE ( 'NONE', *, *, #36461, .F. ) ;
#48268 = CARTESIAN_POINT ( 'NONE',  ( 0.9752570700956794125, -16.20701641182888153, -39.72995844664874454 ) ) ;
#48269 = CARTESIAN_POINT ( 'NONE',  ( 0.8753041380234471980, -34.64850320773107484, -34.79395857525886271 ) ) ;
#48270 = CARTESIAN_POINT ( 'NONE',  ( 0.5980271706414711508, -38.93680501037938058, -29.93283244909104823 ) ) ;
#48271 = EDGE_LOOP ( 'NONE', ( #6219, #4603, #36571, #19394 ) ) ;
#48272 = DIRECTION ( 'NONE',  ( 0.000000000000000000, 0.000000000000000000, 1.000000000000000000 ) ) ;
#48273 = CARTESIAN_POINT ( 'NONE',  ( 2.281448460670569389, -40.87338159040653807, 25.11570011049356665 ) ) ;
#48274 = VERTEX_POINT ( 'NONE', #6253 ) ;
#48275 = CARTESIAN_POINT ( 'NONE',  ( 1.231276596079887264, 25.54232633153331733, 33.23952972879620660 ) ) ;
#48276 = ORIENTED_EDGE ( 'NONE', *, *, #41173, .T. ) ;
#48277 = CARTESIAN_POINT ( 'NONE',  ( 2.282803330402963571, -20.95673854281690751, 42.03941028493377274 ) ) ;
#48278 = EDGE_CURVE ( 'NONE', #44819, #36669, #43852, .T. ) ;
#48279 = CARTESIAN_POINT ( 'NONE',  ( 0.1158516988532803521, 25.28452981770051977, 36.16123215172029859 ) ) ;
#48280 = ORIENTED_EDGE ( 'NONE', *, *, #47662, .F. ) ;
#48281 = CARTESIAN_POINT ( 'NONE',  ( -5.440000000000003055, 15.14599999999999902, 0.000000000000000000 ) ) ;
#48282 = CARTESIAN_POINT ( 'NONE',  ( 2.891212509699203626, -1.730266096895115631E-16, -41.99381090189411481 ) ) ;
#48283 = DIRECTION ( 'NONE',  ( -1.000000000000000000, -0.000000000000000000, -0.000000000000000000 ) ) ;
#48284 = ORIENTED_EDGE ( 'NONE', *, *, #8137, .F. ) ;
#48285 = DIRECTION ( 'NONE',  ( -1.000000000000000000, -0.000000000000000000, 1.925929944387235853E-32 ) ) ;
#48286 = CARTESIAN_POINT ( 'NONE',  ( 3.660176727303398714, -27.72864483302497263, -39.22755245663876877 ) ) ;
#48287 = CARTESIAN_POINT ( 'NONE',  ( 5.959828726073459926, -10.25888482581847327, -17.77796293532169258 ) ) ;
#48288 = AXIS2_PLACEMENT_3D ( 'NONE', #58595, #25107, #11324 ) ;
#48289 = CARTESIAN_POINT ( 'NONE',  ( 4.956653778116989706, -42.88673967249116004, -21.75875759808752008 ) ) ;
#48290 = VECTOR ( 'NONE', #15003, 1000.000000000000114 ) ;
#48291 = CARTESIAN_POINT ( 'NONE',  ( 3.661921753702002125, 24.23902541992542936, 40.31253862666358145 ) ) ;
#48292 = CARTESIAN_POINT ( 'NONE',  ( 3.270143674763207553, 5.490410281242951385, -12.53844339339229030 ) ) ;
#48293 = CARTESIAN_POINT ( 'NONE',  ( -17.42809333609977784, -7.737545843317588101, 2.032524859195957490 ) ) ;
#48294 = CARTESIAN_POINT ( 'NONE',  ( 4.553261556744873317, 12.71466023209499419, 42.04612920360230532 ) ) ;
#48295 = CARTESIAN_POINT ( 'NONE',  ( 0.6031356755773454870, 48.10744332413212021, -2.564066888715896384E-05 ) ) ;
#48296 = B_SPLINE_CURVE_WITH_KNOTS ( 'NONE', 3,
 ( #27850, #51954, #42902, #14383, #9989, #48200 ),
 .UNSPECIFIED., .F., .F.,
 ( 4, 2, 4 ),
 ( 1.870559545977334001E-17, 0.0002293319059085083820, 0.0004586638118169980615 ),
 .UNSPECIFIED. ) ;
#48297 = CARTESIAN_POINT ( 'NONE',  ( 0.1073791018717578927, -21.98088480513690968, 37.10214135362851096 ) ) ;
#48298 = CARTESIAN_POINT ( 'NONE',  ( 0.1158403557922069033, 39.73803855110582361, 19.17885813323219324 ) ) ;
#48299 = CARTESIAN_POINT ( 'NONE',  ( 0.5824935313925970748, -1.202929742068020502, 46.88060512716833017 ) ) ;
#48300 = ADVANCED_FACE ( 'NONE', ( #15401 ), #48824, .T. ) ;
#48301 = VECTOR ( 'NONE', #42102, 999.9999999999998863 ) ;
#48302 = EDGE_CURVE ( 'NONE', #18536, #58789, #34505, .T. ) ;
#48303 = CARTESIAN_POINT ( 'NONE',  ( 0.5827357941260203900, 34.12346967353462190, 33.60975216782498620 ) ) ;
#48304 = CARTESIAN_POINT ( 'NONE',  ( 1.154321485836932837, 34.54400167111899123, 25.46626718279321011 ) ) ;
#48305 = ORIENTED_EDGE ( 'NONE', *, *, #15160, .T. ) ;
#48306 = CARTESIAN_POINT ( 'NONE',  ( 0.3622758884714600280, -0.8252992914331080954, 43.10531414739104150 ) ) ;
#48307 = CARTESIAN_POINT ( 'NONE',  ( 3.727782113643637096, 18.41520185780067465, -39.92064774577724506 ) ) ;
#48308 = CARTESIAN_POINT ( 'NONE',  ( 0.9730545539215883499, 21.89037132892435622, 36.90443313492338717 ) ) ;
#48309 = EDGE_CURVE ( 'NONE', #57398, #1942, #6567, .T. ) ;
#48310 = ORIENTED_EDGE ( 'NONE', *, *, #13073, .T. ) ;
#48311 = CARTESIAN_POINT ( 'NONE',  ( 2.533389852662419894, 26.46405011077438729, 35.17249754379179194 ) ) ;
#48312 = VERTEX_POINT ( 'NONE', #1265 ) ;
#48313 = ORIENTED_EDGE ( 'NONE', *, *, #49345, .T. ) ;
#48314 = FACE_OUTER_BOUND ( 'NONE', #47125, .T. ) ;
#48315 = ORIENTED_EDGE ( 'NONE', *, *, #29845, .T. ) ;
#48316 = EDGE_CURVE ( 'NONE', #27840, #31862, #1890, .T. ) ;
#48317 = CARTESIAN_POINT ( 'NONE',  ( 4.975610109902397937, 47.16372689271670993, -12.96272628450527264 ) ) ;
#48318 = ORIENTED_EDGE ( 'NONE', *, *, #55295, .T. ) ;
#48319 = ORIENTED_EDGE ( 'NONE', *, *, #42443, .F. ) ;
#48320 = CARTESIAN_POINT ( 'NONE',  ( 0.1102847568649952675, 11.25043675627740569, 41.63105453442841508 ) ) ;
#48322 = VERTEX_POINT ( 'NONE', #15711 ) ;
#48321 = EDGE_CURVE ( 'NONE', #10602, #35182, #38031, .T. ) ;
#48323 = CARTESIAN_POINT ( 'NONE',  ( -90.00000000000000000, 0.000000000000000000, 0.000000000000000000 ) ) ;
#48324 = B_SPLINE_CURVE_WITH_KNOTS ( 'NONE', 3,
 ( #39537, #21029, #15724, #49214, #44552, #1582 ),
 .UNSPECIFIED., .F., .F.,
 ( 4, 2, 4 ),
 ( 8.741117365843378158E-19, 0.0002450742804987333088, 0.0004901485609974657503 ),
 .UNSPECIFIED. ) ;
#48325 = CIRCLE ( 'NONE', #35333, 47.09074272231896430 ) ;
#48326 = CARTESIAN_POINT ( 'NONE',  ( 0.3676999524040366896, 9.009680404096547690, -43.18305503711933113 ) ) ;
#48327 = ORIENTED_EDGE ( 'NONE', *, *, #21019, .F. ) ;
#48328 = CARTESIAN_POINT ( 'NONE',  ( 5.860006189529246790, 26.78264244998098675, 40.11385274514691446 ) ) ;
#48329 =( BOUNDED_SURFACE ( )  B_SPLINE_SURFACE ( 3, 1, ( 
 ( #18840, #37963 ),
 ( #57017, #33244 ),
 ( #28212, #4374 ),
 ( #47640, #45422 ) ),
 .UNSPECIFIED., .F., .F., .F. ) 
 B_SPLINE_SURFACE_WITH_KNOTS ( ( 4, 4 ),
 ( 2, 2 ),
 ( 0.000000000000000000, 1.000000000000000000 ),
 ( 0.000000000000000000, 1.000000000000000000 ),
 .UNSPECIFIED. ) 
 GEOMETRIC_REPRESENTATION_ITEM ( )  RATIONAL_B_SPLINE_SURFACE ( (
 ( 1.000000000000000000, 1.000000000000000000),
 ( 0.7223157951917480446, 0.9931996967497186413),
 ( 0.7223157951917480446, 0.9931996967497186413),
 ( 1.000000000000000000, 1.000000000000000000) ) ) 
 REPRESENTATION_ITEM ( '' )  SURFACE ( )  );
#48330 = CARTESIAN_POINT ( 'NONE',  ( 0.8554163680231738898, 23.34472558242499929, -40.69679668712380050 ) ) ;
#48331 = VERTEX_POINT ( 'NONE', #35441 ) ;
#48332 = ORIENTED_EDGE ( 'NONE', *, *, #7129, .T. ) ;
#48333 = CARTESIAN_POINT ( 'NONE',  ( 0.6001305935487315502, -38.48510059944067763, 28.87057754790872721 ) ) ;
#48334 = EDGE_LOOP ( 'NONE', ( #39593, #35720, #31022, #1863 ) ) ;
#48335 = CARTESIAN_POINT ( 'NONE',  ( 48.11999735391012223, 12.44538514811858221, 1.178318479186655887 ) ) ;
#48336 = DIRECTION ( 'NONE',  ( 0.09722883295013591554, 0.3366266327598319563, -0.9366050737423600170 ) ) ;
#48337 = CARTESIAN_POINT ( 'NONE',  ( 4.962356264823608143, 27.50309822711080443, -31.85616401533997077 ) ) ;
#48338 = CARTESIAN_POINT ( 'NONE',  ( 4.549368137175248350, 18.79584381673477012, 38.59302160394760506 ) ) ;
#48339 = CIRCLE ( 'NONE', #20358, 2.649999999999997691 ) ;
#48340 = VERTEX_POINT ( 'NONE', #34822 ) ;
#48341 = CARTESIAN_POINT ( 'NONE',  ( 0.3622758884714600280, 20.83792692158919735, 37.74294673546592804 ) ) ;
#48342 = DIRECTION ( 'NONE',  ( -1.000000000000000000, -0.000000000000000000, -0.000000000000000000 ) ) ;
#48343 = CARTESIAN_POINT ( 'NONE',  ( 5.896782393890504181, 10.82771479451271368, 16.94953330350728748 ) ) ;
#48344 = EDGE_CURVE ( 'NONE', #56562, #60958, #55176, .T. ) ;
#48345 = CARTESIAN_POINT ( 'NONE',  ( 0.000000000000000000, 0.000000000000000000, 0.000000000000000000 ) ) ;
#48346 = ORIENTED_EDGE ( 'NONE', *, *, #7618, .T. ) ;
#48347 = CARTESIAN_POINT ( 'NONE',  ( 0.5980271706414711508, -30.07077130958509414, -38.83037413788716918 ) ) ;
#48348 = CARTESIAN_POINT ( 'NONE',  ( 4.960156602257182357, -25.36362146861359435, -38.88108289790888961 ) ) ;
#48349 = CARTESIAN_POINT ( 'NONE',  ( 0.6000166863083090663, -25.01014854877471549, 42.26483113981026207 ) ) ;
#48350 = CARTESIAN_POINT ( 'NONE',  ( 0.8560838555295158248, -35.39593983670192756, 30.78149244527153883 ) ) ;
#48351 = ORIENTED_EDGE ( 'NONE', *, *, #15565, .T. ) ;
#48352 = EDGE_LOOP ( 'NONE', ( #8750, #31918, #10911, #50768 ) ) ;
#48353 = CARTESIAN_POINT ( 'NONE',  ( -13.51351822333069030, -12.53706398592619387, 7.845252193381024343E-16 ) ) ;
#48354 = CARTESIAN_POINT ( 'NONE',  ( 0.5998501479064699549, -33.64490850298868452, 34.38546660123239462 ) ) ;
#48355 = CARTESIAN_POINT ( 'NONE',  ( -2.601141883200665639, -2.823446916239304105, 14.65686102071543395 ) ) ;
#48356 = B_SPLINE_CURVE_WITH_KNOTS ( 'NONE', 3,
 ( #44919, #55505, #50507, #7580 ),
 .UNSPECIFIED., .F., .F.,
 ( 4, 4 ),
 ( 3.252606517456513302E-19, 0.004446298630425065020 ),
 .UNSPECIFIED. ) ;
#48357 = CARTESIAN_POINT ( 'NONE',  ( 0.3676999524040323597, 43.44964275340426951, -7.620966337964178550 ) ) ;
#48358 = CARTESIAN_POINT ( 'NONE',  ( -2.601141883200662974, 5.573165628699144669, 13.84684990690933581 ) ) ;
#48359 = CARTESIAN_POINT ( 'NONE',  ( 0.1139756605157203340, -31.41879322388790996, 30.98087558558663446 ) ) ;
#48360 = CARTESIAN_POINT ( 'NONE',  ( 0.5997462898726536595, 33.39998138387895921, -35.99990102348682797 ) ) ;
#48361 = CARTESIAN_POINT ( 'NONE',  ( 0.5988103622719987973, 18.96890139669993047, -44.21009254328985350 ) ) ;
#48362 = CARTESIAN_POINT ( 'NONE',  ( 4.962356264823603702, -10.17958088187380739, -40.83640203215431086 ) ) ;
#48363 = CARTESIAN_POINT ( 'NONE',  ( 1.092182651088185130, 3.417759894675622245, -41.77415590702738513 ) ) ;
#48364 = ORIENTED_EDGE ( 'NONE', *, *, #36692, .T. ) ;
#48365 = CARTESIAN_POINT ( 'NONE',  ( 0.9730545539215883499, -42.47233286818622133, 6.101350888304490461 ) ) ;
#48366 = CARTESIAN_POINT ( 'NONE',  ( 0.1129192098497455998, -35.64954734424960492, 26.00118385641814456 ) ) ;
#48367 = CARTESIAN_POINT ( 'NONE',  ( 0.1158816050234199313, -35.35831000359211629, 26.39568061246079367 ) ) ;
#48368 = CARTESIAN_POINT ( 'NONE',  ( 0.5804410086790514622, 37.14246315962216016, 28.63489623329385125 ) ) ;
#48369 = CARTESIAN_POINT ( 'NONE',  ( 0.7954196712028480665, -34.61997730204605261, 33.39101545667277549 ) ) ;
#48370 = CARTESIAN_POINT ( 'NONE',  ( 0.6028618097248864549, -46.42282207635412306, 12.61968633793835082 ) ) ;
#48371 = DIRECTION ( 'NONE',  ( 0.000000000000000000, 0.000000000000000000, 1.000000000000000000 ) ) ;
#48372 = CARTESIAN_POINT ( 'NONE',  ( 0.9756950546413946102, -26.04419981250910610, 34.10037081504545853 ) ) ;
#48373 = CARTESIAN_POINT ( 'NONE',  ( 0.9757892942422816684, -11.05594550521674257, 41.45966865212809438 ) ) ;
#48374 = EDGE_CURVE ( 'NONE', #24079, #873, #29786, .T. ) ;
#48375 = CARTESIAN_POINT ( 'NONE',  ( 5.960721111146673579, 18.96073515164537326, 7.860635756377957861 ) ) ;
#48376 = CARTESIAN_POINT ( 'NONE',  ( -6.017396004339686577, 4.878103249821066356, 18.20079405513551407 ) ) ;
#48378 = EDGE_LOOP ( 'NONE', ( #22709, #45736, #46116, #2788 ) ) ;
#48377 = DIRECTION ( 'NONE',  ( 0.000000000000000000, 0.000000000000000000, -1.000000000000000000 ) ) ;
#48380 = ORIENTED_EDGE ( 'NONE', *, *, #45221, .T. ) ;
#48379 = B_SPLINE_CURVE_WITH_KNOTS ( 'NONE', 3,
 ( #42989, #10688, #5031, #58267, #43606, #24156 ),
 .UNSPECIFIED., .F., .F.,
 ( 4, 2, 4 ),
 ( 1.266794085606387986E-16, 0.0002450741128632352695, 0.0004901482257263437958 ),
 .UNSPECIFIED. ) ;
#48381 = CARTESIAN_POINT ( 'NONE',  ( 0.2885697896453110478, -37.73587455644762656, 20.85752796052947389 ) ) ;
#48382 = CARTESIAN_POINT ( 'NONE',  ( 4.226256110419178924, 43.63133558763896502, -5.209011885762705241 ) ) ;
#48383 = DIRECTION ( 'NONE',  ( -0.9848077530122077983, -0.1736481776669315802, 5.551115123125782702E-17 ) ) ;
#48384 = EDGE_CURVE ( 'NONE', #3834, #26385, #38838, .T. ) ;
#48385 = B_SPLINE_CURVE_WITH_KNOTS ( 'NONE', 3,
 ( #57357, #27338, #13878, #51747 ),
 .UNSPECIFIED., .F., .F.,
 ( 4, 4 ),
 ( 5.721958498152796815E-17, 0.005004948556313859077 ),
 .UNSPECIFIED. ) ;
#48386 = ORIENTED_EDGE ( 'NONE', *, *, #48003, .T. ) ;
#48387 = CARTESIAN_POINT ( 'NONE',  ( 0.1073791018717483448, -10.69234304550083081, 41.77800844988496465 ) ) ;
#48389 = CARTESIAN_POINT ( 'NONE',  ( 0.5997462898726536595, -47.36625756029543055, 12.96106765957438789 ) ) ;
#48388 = AXIS2_PLACEMENT_3D ( 'NONE', #23006, #61188, #56490 ) ;
#48390 =( BOUNDED_SURFACE ( )  B_SPLINE_SURFACE ( 3, 1, ( 
 ( #34854, #53921 ),
 ( #49543, #38635 ),
 ( #14819, #11048 ),
 ( #58002, #15432 ) ),
 .UNSPECIFIED., .F., .F., .F. ) 
 B_SPLINE_SURFACE_WITH_KNOTS ( ( 4, 4 ),
 ( 2, 2 ),
 ( 0.000000000000000000, 1.000000000000000000 ),
 ( 0.000000000000000000, 1.000000000000000000 ),
 .UNSPECIFIED. ) 
 GEOMETRIC_REPRESENTATION_ITEM ( )  RATIONAL_B_SPLINE_SURFACE ( (
 ( 1.000000000000000000, 1.000000000000000000),
 ( 0.9754377213608244057, 0.9999580625633939235),
 ( 0.9754377213608244057, 0.9999580625633939235),
 ( 1.000000000000000000, 1.000000000000000000) ) ) 
 REPRESENTATION_ITEM ( '' )  SURFACE ( )  );
#48391 = ORIENTED_EDGE ( 'NONE', *, *, #51843, .T. ) ;
#48392 = VERTEX_POINT ( 'NONE', #26632 ) ;
#48393 = CARTESIAN_POINT ( 'NONE',  ( 0.5998501479064708430, -23.59887241503325228, -41.92175333043611829 ) ) ;
#48394 = CARTESIAN_POINT ( 'NONE',  ( 4.963659409799330291, -42.53037318521005261, 13.93274247732006721 ) ) ;
#48395 = CARTESIAN_POINT ( 'NONE',  ( 4.962356264823608143, 0.000000000000000000, 0.000000000000000000 ) ) ;
#48396 = CARTESIAN_POINT ( 'NONE',  ( 0.9972139404380291339, -34.43899251299751541, -25.59643345733265463 ) ) ;
#48397 = EDGE_CURVE ( 'NONE', #21951, #13149, #23032, .T. ) ;
#48398 = CARTESIAN_POINT ( 'NONE',  ( 3.238931869106854933, -41.01619136531535759, 12.88361013339092409 ) ) ;
#48399 = CARTESIAN_POINT ( 'NONE',  ( 0.8560838555295158248, -20.57050347530512724, 42.15717282805135113 ) ) ;
#48400 =( BOUNDED_SURFACE ( )  B_SPLINE_SURFACE ( 3, 1, ( 
 ( #11069, #58964 ),
 ( #59269, #34878 ),
 ( #25147, #25451 ),
 ( #2570, #49890 ) ),
 .UNSPECIFIED., .F., .F., .F. ) 
 B_SPLINE_SURFACE_WITH_KNOTS ( ( 4, 4 ),
 ( 2, 2 ),
 ( 0.000000000000000000, 1.000000000000000000 ),
 ( 0.000000000000000000, 1.000000000000000000 ),
 .UNSPECIFIED. ) 
 GEOMETRIC_REPRESENTATION_ITEM ( )  RATIONAL_B_SPLINE_SURFACE ( (
 ( 1.000000000000000000, 1.000000000000000000),
 ( 0.9754377213608244057, 0.9999580625633939235),
 ( 0.9754377213608244057, 0.9999580625633939235),
 ( 1.000000000000000000, 1.000000000000000000) ) ) 
 REPRESENTATION_ITEM ( '' )  SURFACE ( )  );
#48401 = CARTESIAN_POINT ( 'NONE',  ( 0.1129192098497455998, 33.28205046155587610, 28.96993104685618547 ) ) ;
#48402 = ORIENTED_EDGE ( 'NONE', *, *, #32284, .T. ) ;
#48403 = ORIENTED_EDGE ( 'NONE', *, *, #60454, .F. ) ;
#48404 = CARTESIAN_POINT ( 'NONE',  ( 0.8753041380234530822, -19.05925361776951377, 45.25354328012912219 ) ) ;
#48405 = CARTESIAN_POINT ( 'NONE',  ( 3.390910168358336918, 43.97017820572943236, 0.8488610546097931087 ) ) ;
#48406 = EDGE_LOOP ( 'NONE', ( #45581, #34787, #31754, #46346 ) ) ;
#48407 = CARTESIAN_POINT ( 'NONE',  ( 4.549368137175248350, 0.000000000000000000, 0.000000000000000000 ) ) ;
#48408 = DIRECTION ( 'NONE',  ( -1.000000000000000000, -1.836909530733573529E-16, 1.361838123766461297E-32 ) ) ;
#48409 = CARTESIAN_POINT ( 'NONE',  ( 4.967162193818130511, -36.06913038482782952, -23.56777426397217567 ) ) ;
#48410 = CARTESIAN_POINT ( 'NONE',  ( -2.000000000000009770, 3.464101615137749057, -5.600000000000000533 ) ) ;
#48411 = ORIENTED_EDGE ( 'NONE', *, *, #59521, .F. ) ;
#48412 = ORIENTED_EDGE ( 'NONE', *, *, #3609, .F. ) ;
#48413 = CARTESIAN_POINT ( 'NONE',  ( 0.2885697896453107147, 4.828949182955358133, 42.84523253470162985 ) ) ;
#48414 = CARTESIAN_POINT ( 'NONE',  ( 4.956445790444027999, 19.33052208089617352, -42.94029536716791995 ) ) ;
#48415 = DIRECTION ( 'NONE',  ( 0.000000000000000000, 0.000000000000000000, 1.000000000000000000 ) ) ;
#48416 = FACE_OUTER_BOUND ( 'NONE', #24051, .T. ) ;
#48417 = ORIENTED_EDGE ( 'NONE', *, *, #39485, .F. ) ;
#48418 = CARTESIAN_POINT ( 'NONE',  ( 0.6028777368367059797, 4.802101709542340835, -48.87207432145972774 ) ) ;
#48419 = EDGE_LOOP ( 'NONE', ( #6411, #16420 ) ) ;
#48420 = CARTESIAN_POINT ( 'NONE',  ( 0.3622758884714730732, -26.89560658783362612, -33.69533458712334806 ) ) ;
#48421 = CARTESIAN_POINT ( 'NONE',  ( 0.1158816050234199174, 9.824088614716016465, 43.01661683809371794 ) ) ;
#48422 = B_SPLINE_CURVE_WITH_KNOTS ( 'NONE', 3,
 ( #40772, #27258, #36991, #7197 ),
 .UNSPECIFIED., .F., .F.,
 ( 4, 4 ),
 ( 9.159602786276758478E-17, 0.005004741218457508210 ),
 .UNSPECIFIED. ) ;
#48423 = ORIENTED_EDGE ( 'NONE', *, *, #3376, .T. ) ;
#48424 = CARTESIAN_POINT ( 'NONE',  ( 0.5988103564986354543, -5.677495323491076107, 47.77151399983768698 ) ) ;
#48425 = CARTESIAN_POINT ( 'NONE',  ( 3.238018933889920792, -12.74072440564281017, 4.132969149063494108 ) ) ;
#48426 = CARTESIAN_POINT ( 'NONE',  ( 0.9747592971366230152, 25.86343094887233107, -34.23774590565611220 ) ) ;
#48427 = VECTOR ( 'NONE', #6784, 999.9999999999998863 ) ;
#48428 = EDGE_CURVE ( 'NONE', #20429, #27219, #59615, .T. ) ;
#48429 = CARTESIAN_POINT ( 'NONE',  ( 0.8560838555295158248, -38.14845555156047396, -27.29593693413630362 ) ) ;
#48430 = CARTESIAN_POINT ( 'NONE',  ( 0.7044674535452954967, 21.96536420255956656, 43.92408790470009450 ) ) ;
#48431 = CARTESIAN_POINT ( 'NONE',  ( 0.2940133293163008088, -7.834165653650041250, 43.41504806042732412 ) ) ;
#48432 = CARTESIAN_POINT ( 'NONE',  ( -2.708315649062916552, -5.842990691604515341, -13.41752550814508105 ) ) ;
#48433 = ORIENTED_EDGE ( 'NONE', *, *, #7201, .T. ) ;
#48434 = ADVANCED_FACE ( 'NONE', ( #21325 ), #60925, .F. ) ;
#48435 = CARTESIAN_POINT ( 'NONE',  ( 0.9757892942422807803, 39.62259979733206450, -16.46777583825560853 ) ) ;
#48436 = DIRECTION ( 'NONE',  ( 0.000000000000000000, 0.000000000000000000, 1.000000000000000000 ) ) ;
#48437 = CARTESIAN_POINT ( 'NONE',  ( 3.376099380956838925, -13.03750648666899181, -3.119584626537831085 ) ) ;
#48438 = ORIENTED_EDGE ( 'NONE', *, *, #3043, .F. ) ;
#48439 = CARTESIAN_POINT ( 'NONE',  ( 0.6254311100348657337, -0.6881768005105882713, 48.10157347124184923 ) ) ;
#48440 = CARTESIAN_POINT ( 'NONE',  ( 0.8753041380234524160, 46.31375555491767670, -16.31485134079719757 ) ) ;
#48441 = CARTESIAN_POINT ( 'NONE',  ( 3.660087539127321321, -10.60624038924625800, 46.85281175970452949 ) ) ;
#48442 = CARTESIAN_POINT ( 'NONE',  ( 0.6017667736363749853, 38.37782726569690794, -29.00830848931586914 ) ) ;
#48443 =( NAMED_UNIT ( * ) SI_UNIT ( $, .STERADIAN. ) SOLID_ANGLE_UNIT ( ) );
#48444 = CARTESIAN_POINT ( 'NONE',  ( 4.291220156522060236, 29.64992983783088931, 36.60970715421529320 ) ) ;
#48445 = CARTESIAN_POINT ( 'NONE',  ( 0.5988103564986354543, 46.62176022926370678, 11.86435738293459430 ) ) ;
#48446 = EDGE_CURVE ( 'NONE', #29889, #43532, #17249, .T. ) ;
#48448 = ORIENTED_EDGE ( 'NONE', *, *, #25040, .T. ) ;
#48447 = CARTESIAN_POINT ( 'NONE',  ( 4.549368137175248350, -35.57418903283131328, 24.02461520945210793 ) ) ;
#48449 = VERTEX_POINT ( 'NONE', #12870 ) ;
#48450 = CARTESIAN_POINT ( 'NONE',  ( 0.5838002273316444946, -12.52789267095215919, 46.22850660674015444 ) ) ;
#48451 = FACE_BOUND ( 'NONE', #16341, .T. ) ;
#48452 = CARTESIAN_POINT ( 'NONE',  ( 1.827326673878743479, -29.55671596281188229, -31.30008222956372066 ) ) ;
#48453 = EDGE_CURVE ( 'NONE', #19013, #3215, #21867, .T. ) ;
#48454 = DIRECTION ( 'NONE',  ( 0.09722883295013597105, -0.5223840607312808526, 0.8471490111763407826 ) ) ;
#48455 = CARTESIAN_POINT ( 'NONE',  ( 0.9741495583595157770, 42.59115242362818066, -5.208308905147688961 ) ) ;
#48456 = FACE_OUTER_BOUND ( 'NONE', #7162, .T. ) ;
#48457 = EDGE_CURVE ( 'NONE', #32075, #14690, #48422, .T. ) ;
#48458 = ORIENTED_EDGE ( 'NONE', *, *, #33567, .F. ) ;
#48459 = AXIS2_PLACEMENT_3D ( 'NONE', #4384, #22924, #33873 ) ;
#48460 = LINE ( 'NONE', #19665, #39362 ) ;
#48461 = CARTESIAN_POINT ( 'NONE',  ( -18.52085513643809378, -7.737644335448998767, 2.032152541669497658 ) ) ;
#48462 = CARTESIAN_POINT ( 'NONE',  ( 2.526464513654347321, -6.809833384818750446, -42.43615126908563440 ) ) ;
#48463 = ORIENTED_EDGE ( 'NONE', *, *, #5631, .F. ) ;
#48464 = EDGE_CURVE ( 'NONE', #44739, #61394, #35020, .T. ) ;
#48465 = CIRCLE ( 'NONE', #43489, 2.649999999999992806 ) ;
#48466 = CARTESIAN_POINT ( 'NONE',  ( 0.8744876279028306332, 23.49358985382604459, 43.10917867646859492 ) ) ;
#48467 = CARTESIAN_POINT ( 'NONE',  ( 0.5824935313925946323, -25.54019697864863758, -39.33111383301602615 ) ) ;
#48468 = ORIENTED_EDGE ( 'NONE', *, *, #45769, .T. ) ;
#48469 = CARTESIAN_POINT ( 'NONE',  ( 0.3622758884714730732, 40.13994584881760375, 15.73321244754868964 ) ) ;
#48470 = ORIENTED_EDGE ( 'NONE', *, *, #4656, .T. ) ;
#48471 =( BOUNDED_SURFACE ( )  B_SPLINE_SURFACE ( 3, 1, ( 
 ( #28271, #47389 ),
 ( #9786, #5368 ),
 ( #28888, #61763 ),
 ( #48011, #10099 ) ),
 .UNSPECIFIED., .F., .F., .F. ) 
 B_SPLINE_SURFACE_WITH_KNOTS ( ( 4, 4 ),
 ( 2, 2 ),
 ( 0.000000000000000000, 1.000000000000000000 ),
 ( 0.000000000000000000, 1.000000000000000000 ),
 .UNSPECIFIED. ) 
 GEOMETRIC_REPRESENTATION_ITEM ( )  RATIONAL_B_SPLINE_SURFACE ( (
 ( 1.000000000000000000, 1.000000000000000000),
 ( 0.9953390228620291325, 0.8624445117760984880),
 ( 0.9953390228620291325, 0.8624445117760984880),
 ( 1.000000000000000000, 1.000000000000000000) ) ) 
 REPRESENTATION_ITEM ( '' )  SURFACE ( )  );
#48472 = CARTESIAN_POINT ( 'NONE',  ( 0.8744876279028306332, 36.80052600666260787, -32.49725120702428427 ) ) ;
#48473 = CARTESIAN_POINT ( 'NONE',  ( -6.016761891674565099, 18.20023637398599092, 4.880293656735028129 ) ) ;
#48474 = VERTEX_POINT ( 'NONE', #60433 ) ;
#48475 = CARTESIAN_POINT ( 'NONE',  ( 5.880360259849752858, 39.91356965504147780, -26.61251048557207355 ) ) ;
#48476 = DIRECTION ( 'NONE',  ( -1.000000000000000000, -1.836909530733573776E-16, 1.925929944387235853E-32 ) ) ;
#48477 = CARTESIAN_POINT ( 'NONE',  ( 0.3622758884714730732, 26.89560658783340585, 33.69533458712353280 ) ) ;
#48478 = LINE ( 'NONE', #19684, #7354 ) ;
#48479 = ORIENTED_EDGE ( 'NONE', *, *, #5935, .F. ) ;
#48480 = CARTESIAN_POINT ( 'NONE',  ( 5.901463166500145796, 16.58986915973337517, -11.37075686150944165 ) ) ;
#48481 = DIRECTION ( 'NONE',  ( 1.000000000000000000, 0.000000000000000000, 0.000000000000000000 ) ) ;
#48482 = ORIENTED_EDGE ( 'NONE', *, *, #50112, .F. ) ;
#48483 = CARTESIAN_POINT ( 'NONE',  ( 0.1073791018717578927, 11.62916352156150346, -41.52698815987157133 ) ) ;
#48484 = AXIS2_PLACEMENT_3D ( 'NONE', #55285, #31821, #50905 ) ;
#48485 = EDGE_LOOP ( 'NONE', ( #54699, #15824, #19719, #53334 ) ) ;
#48486 = CARTESIAN_POINT ( 'NONE',  ( 5.896278296736517710, -9.670675947513094783, 17.63533402951516038 ) ) ;
#48487 = EDGE_LOOP ( 'NONE', ( #8126, #56399, #14242, #44466 ) ) ;
#48488 = CARTESIAN_POINT ( 'NONE',  ( 2.299652685299202748, 12.16322236728107242, -47.50092363841177701 ) ) ;
#48489 = CARTESIAN_POINT ( 'NONE',  ( 0.9787284016396619046, 35.96249882395619579, -21.51824057086865949 ) ) ;
#48490 = ADVANCED_FACE ( 'NONE', ( #31963 ), #49770, .F. ) ;
#48491 = CARTESIAN_POINT ( 'NONE',  ( 0.5809828226811617480, 41.20389530892307306, 24.41822904836939401 ) ) ;
#48492 = ORIENTED_EDGE ( 'NONE', *, *, #20519, .F. ) ;
#48493 = CARTESIAN_POINT ( 'NONE',  ( 0.8557997880470599172, 23.15977007032323343, 41.93815086860265495 ) ) ;
#48494 = EDGE_CURVE ( 'NONE', #24124, #5027, #36462, .T. ) ;
#48495 = CARTESIAN_POINT ( 'NONE',  ( 0.5827359174754822568, -6.611633125157127644, 47.43746338751530800 ) ) ;
#48496 =( BOUNDED_SURFACE ( )  B_SPLINE_SURFACE ( 3, 1, ( 
 ( #47276, #24080 ),
 ( #52886, #34116 ),
 ( #4322, #23458 ),
 ( #42586, #43208 ) ),
 .UNSPECIFIED., .F., .F., .F. ) 
 B_SPLINE_SURFACE_WITH_KNOTS ( ( 4, 4 ),
 ( 2, 2 ),
 ( 0.000000000000000000, 1.000000000000000000 ),
 ( 0.000000000000000000, 1.000000000000000000 ),
 .UNSPECIFIED. ) 
 GEOMETRIC_REPRESENTATION_ITEM ( )  RATIONAL_B_SPLINE_SURFACE ( (
 ( 1.000000000000000000, 1.000000000000000000),
 ( 0.7223157951917476005, 0.9931996967497186413),
 ( 0.7223157951917476005, 0.9931996967497186413),
 ( 1.000000000000000000, 1.000000000000000000) ) ) 
 REPRESENTATION_ITEM ( '' )  SURFACE ( )  );
#48497 = CARTESIAN_POINT ( 'NONE',  ( 0.8751705887134553219, -37.60752970653848593, 29.98056538504896906 ) ) ;
#48498 = EDGE_LOOP ( 'NONE', ( #34017, #33707, #3536, #37199 ) ) ;
#48499 = EDGE_CURVE ( 'NONE', #45323, #30629, #11043, .T. ) ;
#48500 = EDGE_LOOP ( 'NONE', ( #24186, #53006, #10893, #26011 ) ) ;
#48501 = DIRECTION ( 'NONE',  ( 0.000000000000000000, 0.000000000000000000, 1.000000000000000000 ) ) ;
#48502 = DIRECTION ( 'NONE',  ( -3.273063162220391312E-16, 1.000000000000000000, 1.047380211910525220E-14 ) ) ;
#48503 = CARTESIAN_POINT ( 'NONE',  ( -6.078075953587585900, -12.94978436788747977, 14.25125464905995720 ) ) ;
#48504 = CARTESIAN_POINT ( 'NONE',  ( 0.5997462898726536595, -13.47075269803155351, 47.22383351542719510 ) ) ;
#48506 = STYLED_ITEM ( 'NONE', ( #19395 ), #9707 ) ;
#48505 = CARTESIAN_POINT ( 'NONE',  ( 4.322998006666165516, 4.155494336618067663, 47.80838462754066143 ) ) ;
#48507 = VERTEX_POINT ( 'NONE', #3732 ) ;
#48508 = EDGE_CURVE ( 'NONE', #60397, #49193, #10385, .T. ) ;
#48509 = EDGE_CURVE ( 'NONE', #22420, #48322, #43238, .T. ) ;
#48510 = FACE_OUTER_BOUND ( 'NONE', #57789, .T. ) ;
#48511 = ORIENTED_EDGE ( 'NONE', *, *, #7416, .T. ) ;
#48512 = AXIS2_PLACEMENT_3D ( 'NONE', #17491, #31586, #26259 ) ;
#48513 = CARTESIAN_POINT ( 'NONE',  ( -6.072942160501519027, 18.63017572808498556, -4.870391630012254502 ) ) ;
#48514 = CARTESIAN_POINT ( 'NONE',  ( 0.6027444965799114707, -19.75836062456551190, -44.95715406158468852 ) ) ;
#48515 = AXIS2_PLACEMENT_3D ( 'NONE', #37501, #55331, #46282 ) ;
#48516 = CARTESIAN_POINT ( 'NONE',  ( 0.1158516988532802966, -42.66856749330737841, 11.23990689026689616 ) ) ;
#48517 = CARTESIAN_POINT ( 'NONE',  ( 4.967162193818130511, -38.83676580803754064, -18.65818244221298983 ) ) ;
#48518 = CARTESIAN_POINT ( 'NONE',  ( 1.657374760986086271, 11.00619257538987128, 42.65857677238747669 ) ) ;
#48519 = CARTESIAN_POINT ( 'NONE',  ( 0.8760168074886965917, -7.161346975774058876, 47.56749362999700992 ) ) ;
#48520 = CARTESIAN_POINT ( 'NONE',  ( 0.5809828226811548646, 29.58751527316178809, 37.66417181417562432 ) ) ;
#48521 = EDGE_CURVE ( 'NONE', #24982, #37659, #12609, .T. ) ;
#48522 = CARTESIAN_POINT ( 'NONE',  ( 3.680882792899936362, 20.05474345988747231, 43.58303137875414279 ) ) ;
#48523 = ADVANCED_FACE ( 'NONE', ( #29711 ), #15756, .F. ) ;
#48524 = CARTESIAN_POINT ( 'NONE',  ( 0.8751705887134423323, 19.22545746485661766, -44.08562551107063143 ) ) ;
#48525 = CARTESIAN_POINT ( 'NONE',  ( 0.9772918015221172539, -34.31474319015040919, 24.05899531453268736 ) ) ;
#48526 = B_SPLINE_CURVE_WITH_KNOTS ( 'NONE', 3,
 ( #16417, #26119, #2293, #21422, #40558, #31125, #3525, #47095, #28270, #13894, #52071, #42699, #8539, #57070, #61158, #17971, #32070, #23275, #22661, #27663, #32372, #37091, #41791, #42401, #13575 ),
 .UNSPECIFIED., .F., .F.,
 ( 4, 3, 3, 3, 3, 3, 3, 3, 4 ),
 ( 2.602085213965210642E-18, 0.0005656085177311379053, 0.001131215744874499406, 0.001696821861372765916, 0.002262427090022497284, 0.002828031679238745925, 0.003393635864401605730, 0.003977030878808131623, 0.004561030005651159000 ),
 .UNSPECIFIED. ) ;
#48527 = CARTESIAN_POINT ( 'NONE',  ( 5.896278296736517710, 3.350760724586278272, 19.83177708075989898 ) ) ;
#48528 = EDGE_CURVE ( 'NONE', #22660, #37333, #21579, .T. ) ;
#48529 = ORIENTED_EDGE ( 'NONE', *, *, #52383, .T. ) ;
#48530 = CARTESIAN_POINT ( 'NONE',  ( 0.9762797500689124330, 24.45014227842982635, 34.03697001423955726 ) ) ;
#48531 = CARTESIAN_POINT ( 'NONE',  ( 1.827326673878744145, 4.394636550976061429, 42.82501343454097054 ) ) ;
#48532 = CARTESIAN_POINT ( 'NONE',  ( 4.335381028904216727, 34.47659336712059286, 34.80116890942834118 ) ) ;
#48533 = CARTESIAN_POINT ( 'NONE',  ( 3.559346040607745287, 40.46425943014002513, 17.20680069949995072 ) ) ;
#48534 = DIRECTION ( 'NONE',  ( -1.000000000000000000, -0.000000000000000000, 1.925929944387235853E-32 ) ) ;
#48535 = VERTEX_POINT ( 'NONE', #15024 ) ;
#48536 = CARTESIAN_POINT ( 'NONE',  ( 4.962356264823608143, 7.429277797797782412, -41.42513040734446861 ) ) ;
#48537 = CARTESIAN_POINT ( 'NONE',  ( 5.910764540655178756, -15.79365219732140524, -12.45238084621602326 ) ) ;
#48538 = EDGE_CURVE ( 'NONE', #55943, #42440, #23801, .T. ) ;
#48539 = CARTESIAN_POINT ( 'NONE',  ( 1.091591847532193738, 38.27654012929355076, 17.07821614473897398 ) ) ;
#48540 = VERTEX_POINT ( 'NONE', #58507 ) ;
#48541 = CARTESIAN_POINT ( 'NONE',  ( 0.1064266379913940963, -30.88821943652591173, -30.09411261783680303 ) ) ;
#48542 = EDGE_CURVE ( 'NONE', #28462, #7712, #53804, .T. ) ;
#48543 = CIRCLE ( 'NONE', #58542, 42.08604991992415023 ) ;
#48544 = CARTESIAN_POINT ( 'NONE',  ( 0.9754292589017242721, 15.60437141757889634, 38.89512899525495015 ) ) ;
#48545 = VERTEX_POINT ( 'NONE', #58205 ) ;
#48546 = CARTESIAN_POINT ( 'NONE',  ( 0.8557997880470697982, 37.44587306708137930, -29.88293891557432858 ) ) ;
#48547 = AXIS2_PLACEMENT_3D ( 'NONE', #9395, #33231, #15357 ) ;
#48548 = ORIENTED_EDGE ( 'NONE', *, *, #36184, .F. ) ;
#48549 = CARTESIAN_POINT ( 'NONE',  ( 3.660087539127326206, -48.00143792263125420, 1.881558488211557911 ) ) ;
#48550 = VERTEX_POINT ( 'NONE', #15329 ) ;
#48551 = CARTESIAN_POINT ( 'NONE',  ( 3.238018933889920792, 1.066824900592079794, -13.35175557741863450 ) ) ;
#48552 = DIRECTION ( 'NONE',  ( 0.1024043820194936449, -0.6940285268068357993, 0.7126273545981369750 ) ) ;
#48553 = ORIENTED_EDGE ( 'NONE', *, *, #37154, .F. ) ;
#48554 = PLANE ( 'NONE',  #27094 ) ;
#48555 = CIRCLE ( 'NONE', #21560, 0.2800000000000007483 ) ;
#48556 = B_SPLINE_CURVE_WITH_KNOTS ( 'NONE', 3,
 ( #28782, #252, #29396, #15014, #33815, #14703 ),
 .UNSPECIFIED., .F., .F.,
 ( 4, 2, 4 ),
 ( 3.471140604459641645E-18, 0.0002291459268755735145, 0.0004582918537511435596 ),
 .UNSPECIFIED. ) ;
#48557 = VERTEX_POINT ( 'NONE', #10623 ) ;
#48558 = CARTESIAN_POINT ( 'NONE',  ( 0.9780303403264761775, 19.85596553096524985, -36.90637135005560765 ) ) ;
#48559 = CARTESIAN_POINT ( 'NONE',  ( 0.1073791018717483448, 30.14884492832389284, -30.83464511437107447 ) ) ;
#48560 = DIRECTION ( 'NONE',  ( 1.000000000000000000, 0.000000000000000000, 0.000000000000000000 ) ) ;
#48561 = B_SPLINE_CURVE_WITH_KNOTS ( 'NONE', 3,
 ( #24726, #52914, #10950, #29417, #272, #47927 ),
 .UNSPECIFIED., .F., .F.,
 ( 4, 2, 4 ),
 ( 1.197050036191770715E-16, 0.0002448718616795901148, 0.0004897437233590605336 ),
 .UNSPECIFIED. ) ;
#48562 = ORIENTED_EDGE ( 'NONE', *, *, #52104, .F. ) ;
#48564 = DIRECTION ( 'NONE',  ( -0.07836865515943411409, -0.6131273243286173846, -0.7860872967108246678 ) ) ;
#48563 = B_SPLINE_CURVE_WITH_KNOTS ( 'NONE', 3,
 ( #51586, #20869, #6418, #25559, #53731, #828 ),
 .UNSPECIFIED., .F., .F.,
 ( 4, 2, 4 ),
 ( 8.560751122900633232E-17, 0.0002293366620881450661, 0.0004586733241762045343 ),
 .UNSPECIFIED. ) ;
#48565 = CARTESIAN_POINT ( 'NONE',  ( 0.5838002273316423851, 33.96372661229982270, -33.77111476497738352 ) ) ;
#48566 = CARTESIAN_POINT ( 'NONE',  ( 0.6009453534118439633, 23.67490308139347022, 41.87889766923463242 ) ) ;
#48567 = ORIENTED_EDGE ( 'NONE', *, *, #55023, .F. ) ;
#48568 = EDGE_CURVE ( 'NONE', #448, #28808, #34232, .T. ) ;
#48569 = CARTESIAN_POINT ( 'NONE',  ( 0.7044674535453004927, 46.86672925371311749, 14.67352758780444510 ) ) ;
#48570 = CARTESIAN_POINT ( 'NONE',  ( 0.1129192098497447394, -17.41650932123218354, 40.54154647825593827 ) ) ;
#48571 = VERTEX_POINT ( 'NONE', #44168 ) ;
#48572 = CARTESIAN_POINT ( 'NONE',  ( 0.8751705887134423323, 38.69254731947834358, -28.56654290188613032 ) ) ;
#48573 = ADVANCED_FACE ( 'NONE', ( #1499 ), #5290, .F. ) ;
#48574 =( BOUNDED_SURFACE ( )  B_SPLINE_SURFACE ( 3, 1, ( 
 ( #33568, #5327 ),
 ( #39203, #57950 ),
 ( #53262, #33878 ),
 ( #58564, #5019 ) ),
 .UNSPECIFIED., .F., .F., .F. ) 
 B_SPLINE_SURFACE_WITH_KNOTS ( ( 4, 4 ),
 ( 2, 2 ),
 ( 0.000000000000000000, 1.000000000000000000 ),
 ( 0.000000000000000000, 1.000000000000000000 ),
 .UNSPECIFIED. ) 
 GEOMETRIC_REPRESENTATION_ITEM ( )  RATIONAL_B_SPLINE_SURFACE ( (
 ( 1.000000000000000000, 1.000000000000000000),
 ( 0.9953485035131437453, 0.8621029689291523912),
 ( 0.9953485035131437453, 0.8621029689291523912),
 ( 1.000000000000000000, 1.000000000000000000) ) ) 
 REPRESENTATION_ITEM ( '' )  SURFACE ( )  );
#48575 = ORIENTED_EDGE ( 'NONE', *, *, #56212, .F. ) ;
#48576 = CARTESIAN_POINT ( 'NONE',  ( 4.967162193818130511, -36.06913038482782952, -23.56777426397217567 ) ) ;
#48577 = CARTESIAN_POINT ( 'NONE',  ( 4.956653778116996811, 40.28700667097716348, -26.26162724282331951 ) ) ;
#48578 = VERTEX_POINT ( 'NONE', #60360 ) ;
#48579 = CARTESIAN_POINT ( 'NONE',  ( 0.9784957157296357844, -12.63863412949661758, -39.95745217519625925 ) ) ;
#48580 = CARTESIAN_POINT ( 'NONE',  ( 0.6039202388192953519, 48.99530948556961363, -3.320144765254160912 ) ) ;
#48581 = CARTESIAN_POINT ( 'NONE',  ( 0.8744876279028306332, -48.79802643035336018, -5.394688766001929814 ) ) ;
#48582 = CARTESIAN_POINT ( 'NONE',  ( 0.3622758884714600280, -40.13994584881793770, 15.73321244754782811 ) ) ;
#48583 = EDGE_CURVE ( 'NONE', #46644, #30061, #11834, .T. ) ;
#48584 = ADVANCED_FACE ( 'NONE', ( #45085 ), #18132, .F. ) ;
#48585 = ORIENTED_EDGE ( 'NONE', *, *, #17586, .F. ) ;
#48586 = CARTESIAN_POINT ( 'NONE',  ( 5.838029081930957709, 1.558325986592992818, -47.20843863413011832 ) ) ;
#48587 = EDGE_CURVE ( 'NONE', #50941, #37408, #47856, .T. ) ;
#48588 = CARTESIAN_POINT ( 'NONE',  ( 0.9762797500689124330, 41.46413394121043439, -6.086902470967093137 ) ) ;
#48589 = CARTESIAN_POINT ( 'NONE',  ( 5.959828726073459926, -17.77343634131834804, -10.26672511661749709 ) ) ;
#48590 = LINE ( 'NONE', #32975, #11851 ) ;
#48591 = EDGE_CURVE ( 'NONE', #31957, #28574, #45455, .T. ) ;
#48592 = CARTESIAN_POINT ( 'NONE',  ( 0.7242486021783849370, -35.83732651437340166, 33.56631482120374699 ) ) ;
#48593 = CARTESIAN_POINT ( 'NONE',  ( -6.078075953587585900, 18.62492360731175012, 4.889518879085924752 ) ) ;
#48594 = CONICAL_SURFACE ( 'NONE', #13600, 42.92674063221959813, 1.485477209440487556 ) ;
#48595 = CARTESIAN_POINT ( 'NONE',  ( 0.6064515330803583737, 46.56800900943660082, 5.545707613471479114 ) ) ;
#48596 = CARTESIAN_POINT ( 'NONE',  ( 3.270143674763207553, -12.74832469035455951, 4.983712007628184892 ) ) ;
#48597 = CIRCLE ( 'NONE', #53585, 0.02570000000000870199 ) ;
#48598 = CARTESIAN_POINT ( 'NONE',  ( 0.1157991065609915715, -43.75142591887181709, -5.723206758729824983 ) ) ;
#48599 = B_SPLINE_CURVE_WITH_KNOTS ( 'NONE', 3,
 ( #15783, #33825, #19112, #27024, #36753, #41454 ),
 .UNSPECIFIED., .F., .F.,
 ( 4, 2, 4 ),
 ( 1.530125426324321260E-16, 0.0002445252820015212498, 0.0004890505640028894102 ),
 .UNSPECIFIED. ) ;
#48600 = CARTESIAN_POINT ( 'NONE',  ( -6.017396004339687465, -17.40836349643162251, -7.212050743684361720 ) ) ;
#48601 = CARTESIAN_POINT ( 'NONE',  ( 0.5830082357119560355, -1.840022353388820919, 46.85985864978006532 ) ) ;
#48602 = CARTESIAN_POINT ( 'NONE',  ( 2.526464513654346433, 29.52129845577976042, -31.23609615087146452 ) ) ;
#48603 = LINE ( 'NONE', #43947, #53193 ) ;
#48604 = AXIS2_PLACEMENT_3D ( 'NONE', #26882, #41018, #46938 ) ;
#48605 = ORIENTED_EDGE ( 'NONE', *, *, #18992, .T. ) ;
#48606 = CARTESIAN_POINT ( 'NONE',  ( 0.8751705887134423323, 0.8911681664088411114, -48.08707113907595243 ) ) ;
#48607 = CARTESIAN_POINT ( 'NONE',  ( 0.9785694773339244090, -1.622802894008406271, 41.87722431682728086 ) ) ;
#48608 = CARTESIAN_POINT ( 'NONE',  ( 0.7246131072078584312, 28.62741613354240755, 38.65593150731059069 ) ) ;
#48609 = ORIENTED_EDGE ( 'NONE', *, *, #13387, .T. ) ;
#48610 = DIRECTION ( 'NONE',  ( -0.07906939808003035641, -0.02523889567981928844, 0.9965495614529791268 ) ) ;
#48611 = CARTESIAN_POINT ( 'NONE',  ( 2.185380717157383135, 26.35783754162028814, 35.27157783820779002 ) ) ;
#48612 = B_SPLINE_CURVE_WITH_KNOTS ( 'NONE', 3,
 ( #57002, #4358, #23495, #18195 ),
 .UNSPECIFIED., .F., .F.,
 ( 4, 4 ),
 ( 0.000000000000000000, 0.005004948556313816577 ),
 .UNSPECIFIED. ) ;
#48613 = ORIENTED_EDGE ( 'NONE', *, *, #61732, .F. ) ;
#48614 = ORIENTED_EDGE ( 'NONE', *, *, #43307, .T. ) ;
#48615 = ADVANCED_FACE ( 'NONE', ( #12797 ), #24908, .F. ) ;
#48616 = CARTESIAN_POINT ( 'NONE',  ( 0.5839879882104919151, -5.421203860810959572E-16, -47.89596766822081975 ) ) ;
#48617 = ORIENTED_EDGE ( 'NONE', *, *, #26365, .T. ) ;
#48618 = CARTESIAN_POINT ( 'NONE',  ( -6.016761891674564211, -9.418621820384613486, 16.32039929810254009 ) ) ;
#48619 = ORIENTED_EDGE ( 'NONE', *, *, #13452, .F. ) ;
#48620 = ORIENTED_EDGE ( 'NONE', *, *, #23919, .T. ) ;
#48621 = CARTESIAN_POINT ( 'NONE',  ( 0.6000166863083090663, -20.35571918921390377, -44.69304395538888031 ) ) ;
#48622 = ORIENTED_EDGE ( 'NONE', *, *, #38809, .F. ) ;
#48623 = CARTESIAN_POINT ( 'NONE',  ( 0.6017667736363750963, -29.56223180955360164, 37.95278695280759251 ) ) ;
#48624 = DIRECTION ( 'NONE',  ( 0.9848077530122079093, 0.1736481776669316079, -5.551115123125783935E-17 ) ) ;
#48625 = CARTESIAN_POINT ( 'NONE',  ( 0.9783242366443551941, -17.39724996613036012, -38.12702694706867845 ) ) ;
#48626 = ORIENTED_EDGE ( 'NONE', *, *, #50360, .T. ) ;
#48628 = B_SPLINE_CURVE_WITH_KNOTS ( 'NONE', 3,
 ( #11270, #44501, #20978, #26282 ),
 .UNSPECIFIED., .F., .F.,
 ( 4, 4 ),
 ( 4.670885906470169154E-18, 0.004050076154992999881 ),
 .UNSPECIFIED. ) ;
#48627 = CARTESIAN_POINT ( 'NONE',  ( 5.981074661064941900, -10.25489689131118176, -17.77917279944628959 ) ) ;
#48629 = CARTESIAN_POINT ( 'NONE',  ( 0.9972139404380282457, 39.89035676513734785, 15.81078898082002837 ) ) ;
#48630 = ORIENTED_EDGE ( 'NONE', *, *, #26293, .T. ) ;
#48631 = VERTEX_POINT ( 'NONE', #25949 ) ;
#48632 = CARTESIAN_POINT ( 'NONE',  ( 0.3676999524040323597, 30.26295534861902681, -32.09523511193413725 ) ) ;
#48633 = AXIS2_PLACEMENT_3D ( 'NONE', #49026, #39974, #58705 ) ;
#48634 = CARTESIAN_POINT ( 'NONE',  ( 5.896782393890504181, -7.234636363571307349, -18.76662259344776018 ) ) ;
#48635 = LINE ( 'NONE', #4774, #4217 ) ;
#48636 = VECTOR ( 'NONE', #35036, 1000.000000000000114 ) ;
#48637 = CARTESIAN_POINT ( 'NONE',  ( 0.3676999524040366896, -43.63756228305280160, 6.458617600967457406 ) ) ;
#48638 = CARTESIAN_POINT ( 'NONE',  ( 0.1073791018717483448, 6.109314776652144729, 42.68962945260955877 ) ) ;
#48639 = EDGE_LOOP ( 'NONE', ( #13339, #36801, #29267, #61733 ) ) ;
#48640 = CARTESIAN_POINT ( 'NONE',  ( 0.1152809850208375009, -1.193148287966932397, -44.10806819225567921 ) ) ;
#48641 = FACE_OUTER_BOUND ( 'NONE', #41915, .T. ) ;
#48642 = EDGE_CURVE ( 'NONE', #18131, #54002, #31224, .T. ) ;
#48643 = CARTESIAN_POINT ( 'NONE',  ( -6.078726893082806448, 9.979253153318763836, 16.46841060244423360 ) ) ;
#48644 = ORIENTED_EDGE ( 'NONE', *, *, #51541, .F. ) ;
#48645 = CARTESIAN_POINT ( 'NONE',  ( 0.8551540677456715978, 41.03346287276427518, 24.74404575822789809 ) ) ;
#48646 = CARTESIAN_POINT ( 'NONE',  ( 0.6029443199889047422, -13.97243605900292707, -47.07768762833914877 ) ) ;
#48647 = EDGE_CURVE ( 'NONE', #53393, #39665, #2739, .T. ) ;
#48648 = CARTESIAN_POINT ( 'NONE',  ( 0.8753041380234530822, -24.68967207985825496, 42.44476905888459584 ) ) ;
#48649 = CARTESIAN_POINT ( 'NONE',  ( 1.112077966505211846, -5.996671051578201350, 43.67001558767432812 ) ) ;
#48650 = VECTOR ( 'NONE', #58522, 999.9999999999998863 ) ;
#48651 = EDGE_CURVE ( 'NONE', #38898, #36353, #10262, .T. ) ;
#48652 = ORIENTED_EDGE ( 'NONE', *, *, #51532, .T. ) ;
#48653 = VERTEX_POINT ( 'NONE', #56904 ) ;
#48654 = LINE ( 'NONE', #33965, #42938 ) ;
#48655 = EDGE_CURVE ( 'NONE', #5070, #47280, #33438, .T. ) ;
#48656 = DIRECTION ( 'NONE',  ( 0.000000000000000000, 0.000000000000000000, 1.000000000000000000 ) ) ;
#48657 = CARTESIAN_POINT ( 'NONE',  ( 0.1104177457020373287, -39.83992599038897708, 16.50753524010228546 ) ) ;
#48658 = B_SPLINE_CURVE_WITH_KNOTS ( 'NONE', 3,
 ( #43897, #20071, #39187, #15370, #20983, #44507 ),
 .UNSPECIFIED., .F., .F.,
 ( 4, 2, 4 ),
 ( 1.261467247513764704E-16, 0.0002450741128632373837, 0.0004901482257263485662 ),
 .UNSPECIFIED. ) ;
#48659 = CARTESIAN_POINT ( 'NONE',  ( 0.6000166863083090663, 49.04012132094738519, -2.624877622902973329 ) ) ;
#48660 = CARTESIAN_POINT ( 'NONE',  ( -7.632783294297951215E-14, -4.618802153517020948, -0.3572655899081733644 ) ) ;
#48661 = CARTESIAN_POINT ( 'NONE',  ( 1.600000000000000089, -11.64055411052240352, 0.000000000000000000 ) ) ;
#48662 = CYLINDRICAL_SURFACE ( 'NONE', #27995, 8.000000000000000000 ) ;
#48663 = CARTESIAN_POINT ( 'NONE',  ( 4.967162193818130511, 0.000000000000000000, 0.000000000000000000 ) ) ;
#48664 = CARTESIAN_POINT ( 'NONE',  ( 5.896782393890504181, 19.00205529748287248, 6.591508275760228130 ) ) ;
#48665 = CARTESIAN_POINT ( 'NONE',  ( 0.1092355843206037486, 30.70542469027324728, -30.28032287551047119 ) ) ;
#48666 = CARTESIAN_POINT ( 'NONE',  ( 5.965394784446460541, -2.693446924985777535, 20.34787558161481869 ) ) ;
#48668 = ORIENTED_EDGE ( 'NONE', *, *, #41633, .F. ) ;
#48667 = EDGE_CURVE ( 'NONE', #20580, #60741, #44672, .T. ) ;
#48669 = B_SPLINE_CURVE_WITH_KNOTS ( 'NONE', 3,
 ( #34287, #433, #58668, #20194 ),
 .UNSPECIFIED., .F., .F.,
 ( 4, 4 ),
 ( 5.157703690291707425E-17, 0.005004948556313851271 ),
 .UNSPECIFIED. ) ;
#48670 = CARTESIAN_POINT ( 'NONE',  ( 0.1158516988532803521, -7.090803588212395425, -43.55069073282524528 ) ) ;
#48671 = CARTESIAN_POINT ( 'NONE',  ( 0.6026777506516367566, 41.25117635047293163, 26.64370170114134950 ) ) ;
#48672 = EDGE_CURVE ( 'NONE', #25125, #40399, #27443, .T. ) ;
#48673 = CARTESIAN_POINT ( 'NONE',  ( -6.016104459813371719, -0.005335450884934395989, -18.84322058118302579 ) ) ;
#48674 = CARTESIAN_POINT ( 'NONE',  ( 0.1073791018717578927, -37.10214135362874543, -21.98088480513651888 ) ) ;
#48675 = CARTESIAN_POINT ( 'NONE',  ( 0.6009452777970412107, -46.35353542372332925, 12.87217382175413327 ) ) ;
#48676 = CARTESIAN_POINT ( 'NONE',  ( 0.5807400328401637335, 47.41494605191442702, 6.791881299635756264 ) ) ;
#48677 = CARTESIAN_POINT ( 'NONE',  ( 0.9757787079277443487, -26.15233402543291774, 34.01751575780809844 ) ) ;
#48678 = CARTESIAN_POINT ( 'NONE',  ( 0.6846871229502932144, 37.47592888575248082, 29.84551600520645209 ) ) ;
#48679 = B_SPLINE_CURVE_WITH_KNOTS ( 'NONE', 3,
 ( #1049, #16094, #742, #25471 ),
 .UNSPECIFIED., .F., .F.,
 ( 4, 4 ),
 ( 2.250920953359534068E-17, 0.004564976165746187711 ),
 .UNSPECIFIED. ) ;
#48680 = VECTOR ( 'NONE', #26780, 1000.000000000000114 ) ;
#48681 = CARTESIAN_POINT ( 'NONE',  ( 0.8557997880470697982, 28.43566216845025352, -38.55640757422408882 ) ) ;
#48682 = B_SPLINE_CURVE_WITH_KNOTS ( 'NONE', 3,
 ( #12550, #36364, #40448, #45755, #50433, #16621, #7499, #2806, #6878, #36057, #31329, #46371, #31642, #21938, #3119, #17860, #3417, #7185, #36985 ),
 .UNSPECIFIED., .F., .F.,
 ( 4, 3, 3, 3, 3, 3, 4 ),
 ( 1.153344816771540786E-16, 0.0002618519381806247784, 0.0003927759815485972763, 0.0005237000248299418037, 0.0006546240681324968494, 0.0007855481115631319502, 0.0009699050456655100745 ),
 .UNSPECIFIED. ) ;
#48684 = ORIENTED_EDGE ( 'NONE', *, *, #21638, .T. ) ;
#48683 = CARTESIAN_POINT ( 'NONE',  ( 5.860006189529246790, 40.09484204000600727, 26.81109398084720752 ) ) ;
#48685 = ORIENTED_EDGE ( 'NONE', *, *, #23735, .F. ) ;
#48686 = AXIS2_PLACEMENT_3D ( 'NONE', #61108, #31083, #60489 ) ;
#48687 = CARTESIAN_POINT ( 'NONE',  ( 0.1098349054025746230, -43.12395110775227636, -0.2133124578263222715 ) ) ;
#48688 = CARTESIAN_POINT ( 'NONE',  ( 5.896782393890504181, -13.98685533979025131, 14.45316451791071266 ) ) ;
#48689 = CONICAL_SURFACE ( 'NONE', #56677, 43.92652462719577500, 1.486293639869522343 ) ;
#48690 = DIRECTION ( 'NONE',  ( 1.000000000000000000, 1.836909530733573776E-16, -1.925929944387235579E-32 ) ) ;
#48691 = ORIENTED_EDGE ( 'NONE', *, *, #27414, .T. ) ;
#48692 = CARTESIAN_POINT ( 'NONE',  ( 0.1087620492084205442, -11.51076657762363986, 41.55994353650422113 ) ) ;
#48693 = CARTESIAN_POINT ( 'NONE',  ( 0.1064266418746777354, -30.09411284098551320, -30.88821921809838145 ) ) ;
#48694 = CARTESIAN_POINT ( 'NONE',  ( 0.5819845901640493535, -41.25023214430184737, -24.34012668949530322 ) ) ;
#48695 = ORIENTED_EDGE ( 'NONE', *, *, #14173, .T. ) ;
#48696 = EDGE_LOOP ( 'NONE', ( #17434, #14751, #34585, #6106 ) ) ;
#48697 =( BOUNDED_SURFACE ( )  B_SPLINE_SURFACE ( 3, 1, ( 
 ( #45595, #51193 ),
 ( #50274, #12704 ),
 ( #50888, #35587 ),
 ( #59663, #49970 ) ),
 .UNSPECIFIED., .F., .F., .F. ) 
 B_SPLINE_SURFACE_WITH_KNOTS ( ( 4, 4 ),
 ( 2, 2 ),
 ( 0.000000000000000000, 1.000000000000000000 ),
 ( 0.000000000000000000, 1.000000000000000000 ),
 .UNSPECIFIED. ) 
 GEOMETRIC_REPRESENTATION_ITEM ( )  RATIONAL_B_SPLINE_SURFACE ( (
 ( 1.000000000000000000, 1.000000000000000000),
 ( 0.9729067724841187204, 0.9999501103223794596),
 ( 0.9729067724841187204, 0.9999501103223794596),
 ( 1.000000000000000000, 1.000000000000000000) ) ) 
 REPRESENTATION_ITEM ( '' )  SURFACE ( )  );
#48698 = ADVANCED_FACE ( 'NONE', ( #56597 ), #20509, .F. ) ;
#48699 = CARTESIAN_POINT ( 'NONE',  ( 0.6031356219577718170, -24.12932366310838006, -41.61861914321203670 ) ) ;
#48700 = AXIS2_PLACEMENT_3D ( 'NONE', #31363, #45183, #50763 ) ;
#48701 = CARTESIAN_POINT ( 'NONE',  ( 0.5980271706414711508, 43.94069670602949884, 21.93773953328807735 ) ) ;
#48702 = CARTESIAN_POINT ( 'NONE',  ( 4.967162193818129623, 32.10009971360071290, 28.74031574030022540 ) ) ;
#48703 = CARTESIAN_POINT ( 'NONE',  ( 1.227938101723756947, 42.43379953535195170, -6.439911493064139236 ) ) ;
#48704 = CARTESIAN_POINT ( 'NONE',  ( 0.9775691876210972353, -40.99194725836810704, -8.717451976188911544 ) ) ;
#48705 = VECTOR ( 'NONE', #39387, 1000.000000000000114 ) ;
#48706 = CARTESIAN_POINT ( 'NONE',  ( 0.5797568599927148680, -29.79412097160983208, -36.21513032145659139 ) ) ;
#48707 = CARTESIAN_POINT ( 'NONE',  ( 0.9758171775293909000, 42.54217005300511545, 5.594812732687240775 ) ) ;
#48708 = ORIENTED_EDGE ( 'NONE', *, *, #28555, .F. ) ;
#48709 = EDGE_LOOP ( 'NONE', ( #43262, #32542, #16548, #61156 ) ) ;
#48710 = CARTESIAN_POINT ( 'NONE',  ( 3.782542959838394836, 37.01845254676131702, -19.92164713169448120 ) ) ;
#48711 = LINE ( 'NONE', #39337, #42577 ) ;
#48712 = ORIENTED_EDGE ( 'NONE', *, *, #23090, .T. ) ;
#48713 = DIRECTION ( 'NONE',  ( -1.000000000000000000, -0.000000000000000000, -0.000000000000000000 ) ) ;
#48714 = CARTESIAN_POINT ( 'NONE',  ( 0.8560838555295223751, -0.6537497281626496459, 46.90357604036880446 ) ) ;
#48715 = LINE ( 'NONE', #15522, #40805 ) ;
#48716 = CARTESIAN_POINT ( 'NONE',  ( 0.1129192098497455998, -40.71518461128082578, -17.00663193740825463 ) ) ;
#48717 = B_SPLINE_CURVE_WITH_KNOTS ( 'NONE', 3,
 ( #7306, #12671, #45883, #36170 ),
 .UNSPECIFIED., .F., .F.,
 ( 4, 4 ),
 ( 0.000000000000000000, 0.005013413432710150247 ),
 .UNSPECIFIED. ) ;
#48718 = ORIENTED_EDGE ( 'NONE', *, *, #44180, .T. ) ;
#48719 = CARTESIAN_POINT ( 'NONE',  ( 1.227938101723756947, -6.439911493064287562, -42.43379953535192328 ) ) ;
#48720 = CARTESIAN_POINT ( 'NONE',  ( 0.9762797500689124330, -37.62962005162893320, -18.44821075215020656 ) ) ;
#48721 = VERTEX_POINT ( 'NONE', #8995 ) ;
#48722 = CARTESIAN_POINT ( 'NONE',  ( 0.3676999524040323597, 42.11837424242189343, -13.11461530118710428 ) ) ;
#48723 = ADVANCED_FACE ( 'NONE', ( #41922 ), #41756, .F. ) ;
#48724 = CIRCLE ( 'NONE', #10728, 47.09074272231896430 ) ;
#48725 = ORIENTED_EDGE ( 'NONE', *, *, #61497, .F. ) ;
#48726 = DIRECTION ( 'NONE',  ( -1.000000000000000000, -0.000000000000000000, -0.000000000000000000 ) ) ;
#48727 = CARTESIAN_POINT ( 'NONE',  ( 0.1139756605157203201, 10.20580263603494409, 42.92780931109022902 ) ) ;
#48728 = B_SPLINE_CURVE_WITH_KNOTS ( 'NONE', 3,
 ( #36379, #51053, #45777, #7515 ),
 .UNSPECIFIED., .F., .F.,
 ( 4, 4 ),
 ( 2.168404344971008868E-18, 0.004048833967417085622 ),
 .UNSPECIFIED. ) ;
#48729 = AXIS2_PLACEMENT_3D ( 'NONE', #19852, #23922, #9201 ) ;
#48730 = ORIENTED_EDGE ( 'NONE', *, *, #27876, .T. ) ;
#48731 = CARTESIAN_POINT ( 'NONE',  ( 0.8744876279028263033, 43.84003649649913115, 22.09980204357308153 ) ) ;
#48732 = VECTOR ( 'NONE', #50706, 1000.000000000000114 ) ;
#48733 = EDGE_CURVE ( 'NONE', #38797, #60545, #5013, .T. ) ;
#48734 = DIRECTION ( 'NONE',  ( 1.000000000000000000, 0.000000000000000000, 0.000000000000000000 ) ) ;
#48735 = CARTESIAN_POINT ( 'NONE',  ( 4.549368137175248350, 18.79584381673477012, 38.59302160394760506 ) ) ;
#48736 = CARTESIAN_POINT ( 'NONE',  ( -2.708315649062916552, 2.171184472130498477, 14.47261168455370317 ) ) ;
#48737 = CARTESIAN_POINT ( 'NONE',  ( 1.321505333908969293, -3.855830693249186147, -5.565789719053443996 ) ) ;
#48738 = CARTESIAN_POINT ( 'NONE',  ( 0.5806925824938502512, 45.37089516811273882, 11.86188155343358197 ) ) ;
#48739 = CARTESIAN_POINT ( 'NONE',  ( 4.956653778117001252, 47.94889704119056972, -3.690426056929486887 ) ) ;
#48740 = CARTESIAN_POINT ( 'NONE',  ( 0.8557997880470599172, 47.89938907511594124, 0.9121262075947815795 ) ) ;
#48741 = ORIENTED_EDGE ( 'NONE', *, *, #25902, .T. ) ;
#48742 = CARTESIAN_POINT ( 'NONE',  ( 0.5819845079324663661, -23.55367910461026071, 41.70428776698889806 ) ) ;
#48743 = CARTESIAN_POINT ( 'NONE',  ( 0.9784957157296363395, 41.56508225881332663, 5.355090457728283404 ) ) ;
#48744 = CARTESIAN_POINT ( 'NONE',  ( 5.894904586330512508, -15.78384355525793836, 12.46594138782888628 ) ) ;
#48745 = EDGE_LOOP ( 'NONE', ( #49248, #44916, #15579, #49716 ) ) ;
#48746 = CARTESIAN_POINT ( 'NONE',  ( 4.958415959904820092, 45.28449214630080633, 3.538181012081810461 ) ) ;
#48747 = CARTESIAN_POINT ( 'NONE',  ( 4.956445790443989807, 42.27038699792205279, 20.75457619864928205 ) ) ;
#48749 = EDGE_CURVE ( 'NONE', #3699, #59613, #52854, .T. ) ;
#48748 = CARTESIAN_POINT ( 'NONE',  ( 0.7242003506639976829, 48.94187641115512832, -3.962878686162724318 ) ) ;
#48750 = FACE_OUTER_BOUND ( 'NONE', #12549, .T. ) ;
#48751 = CARTESIAN_POINT ( 'NONE',  ( 0.5782707292762442330, 33.12197115878082343, -33.20649605520746661 ) ) ;
#48752 = B_SPLINE_CURVE_WITH_KNOTS ( 'NONE', 3,
 ( #24539, #18938, #24228, #33347 ),
 .UNSPECIFIED., .F., .F.,
 ( 4, 4 ),
 ( 6.505213034913026604E-19, 0.004041751736740997747 ),
 .UNSPECIFIED. ) ;
#48753 = CARTESIAN_POINT ( 'NONE',  ( 1.227938101723756947, 41.23019537246726429, -11.92353943227906399 ) ) ;
#48754 = CARTESIAN_POINT ( 'NONE',  ( 0.2885700199627516116, -41.84838128711415806, -10.38006184593188053 ) ) ;
#48755 =( BOUNDED_SURFACE ( )  B_SPLINE_SURFACE ( 3, 1, ( 
 ( #19322, #47516 ),
 ( #4564, #19025 ),
 ( #38142, #48430 ),
 ( #48134, #53119 ) ),
 .UNSPECIFIED., .F., .F., .F. ) 
 B_SPLINE_SURFACE_WITH_KNOTS ( ( 4, 4 ),
 ( 2, 2 ),
 ( 0.000000000000000000, 1.000000000000000000 ),
 ( 0.000000000000000000, 1.000000000000000000 ),
 .UNSPECIFIED. ) 
 GEOMETRIC_REPRESENTATION_ITEM ( )  RATIONAL_B_SPLINE_SURFACE ( (
 ( 1.000000000000000000, 1.000000000000000000),
 ( 0.9953485035131437453, 0.8621029689291523912),
 ( 0.9953485035131437453, 0.8621029689291523912),
 ( 1.000000000000000000, 1.000000000000000000) ) ) 
 REPRESENTATION_ITEM ( '' )  SURFACE ( )  );
#48756 = CARTESIAN_POINT ( 'NONE',  ( 0.6030672459662954621, -0.08726629989097470230, 48.10738700891300823 ) ) ;
#48757 = CARTESIAN_POINT ( 'NONE',  ( 1.000110580585052311, -11.78687190425167941, -40.21799514501766737 ) ) ;
#48759 = EDGE_LOOP ( 'NONE', ( #6877, #57998, #25434, #40017 ) ) ;
#48758 = CARTESIAN_POINT ( 'NONE',  ( 0.8751705887134553219, -44.76769609654225235, -17.57879340691528469 ) ) ;
#48760 = ORIENTED_EDGE ( 'NONE', *, *, #47231, .T. ) ;
#48761 = CARTESIAN_POINT ( 'NONE',  ( 0.5827357941260213892, -12.04516435546833364, 46.35666768646130009 ) ) ;
#48762 = LINE ( 'NONE', #59072, #7484 ) ;
#48763 = CARTESIAN_POINT ( 'NONE',  ( 0.1129192098497447394, -42.80154921430116843, -10.72283417016740259 ) ) ;
#48764 = CARTESIAN_POINT ( 'NONE',  ( 1.088908134280554885, 0.7803765577541792453, 42.90644581410506220 ) ) ;
#48765 = CARTESIAN_POINT ( 'NONE',  ( 4.975801465491694664, 27.09127437476381317, -39.51822597168466444 ) ) ;
#48766 = CARTESIAN_POINT ( 'NONE',  ( 1.154321713695927842, 30.92445811446689774, -29.75729669971078195 ) ) ;
#48767 =( BOUNDED_SURFACE ( )  B_SPLINE_SURFACE ( 3, 1, ( 
 ( #3207, #36762 ),
 ( #55520, #9152 ),
 ( #38307, #32054 ),
 ( #32669, #3823 ) ),
 .UNSPECIFIED., .F., .F., .F. ) 
 B_SPLINE_SURFACE_WITH_KNOTS ( ( 4, 4 ),
 ( 2, 2 ),
 ( 0.000000000000000000, 1.000000000000000000 ),
 ( 0.000000000000000000, 1.000000000000000000 ),
 .UNSPECIFIED. ) 
 GEOMETRIC_REPRESENTATION_ITEM ( )  RATIONAL_B_SPLINE_SURFACE ( (
 ( 1.000000000000000000, 1.000000000000000000),
 ( 0.9953040768229005630, 0.8617119497784937465),
 ( 0.9953040768229005630, 0.8617119497784937465),
 ( 1.000000000000000000, 1.000000000000000000) ) ) 
 REPRESENTATION_ITEM ( '' )  SURFACE ( )  );
#48768 = ORIENTED_EDGE ( 'NONE', *, *, #22477, .F. ) ;
#48769 = ORIENTED_EDGE ( 'NONE', *, *, #44374, .F. ) ;
#48770 = EDGE_CURVE ( 'NONE', #2852, #61163, #41678, .T. ) ;
#48771 = AXIS2_PLACEMENT_3D ( 'NONE', #5399, #28919, #9196 ) ;
#48772 = CARTESIAN_POINT ( 'NONE',  ( 0.5848930533535030563, -13.72019472029248099, -44.84450177251183334 ) ) ;
#48773 = AXIS2_PLACEMENT_3D ( 'NONE', #2324, #21449, #1701 ) ;
#48774 = CARTESIAN_POINT ( 'NONE',  ( 0.7044674535452954967, 28.78324386660444389, -39.79104918604790697 ) ) ;
#48775 = B_SPLINE_CURVE_WITH_KNOTS ( 'NONE', 3,
 ( #33020, #4457, #9805, #23295, #61477, #19226, #29521, #23594, #4158, #42421, #28908, #18599, #38337, #9184, #378, #42722, #61782, #38043, #14219 ),
 .UNSPECIFIED., .F., .F.,
 ( 4, 3, 3, 3, 3, 3, 4 ),
 ( 6.939740885162003740E-18, 0.0002732106629380618898, 0.0004098138914053761368, 0.0005464171197651466897, 0.0006830203481512586933, 0.0008196235766963615730, 0.001011968216111140944 ),
 .UNSPECIFIED. ) ;
#48776 = VECTOR ( 'NONE', #24310, 1000.000000000000000 ) ;
#48777 = CYLINDRICAL_SURFACE ( 'NONE', #31794, 12.50000000000000000 ) ;
#48778 = ORIENTED_EDGE ( 'NONE', *, *, #33498, .F. ) ;
#48779 = EDGE_CURVE ( 'NONE', #14372, #44114, #58049, .T. ) ;
#48780 = CARTESIAN_POINT ( 'NONE',  ( 0.5824936645240080813, 43.03133214971953890, 18.64249533889771726 ) ) ;
#48781 = ORIENTED_EDGE ( 'NONE', *, *, #41440, .T. ) ;
#48782 = APPLICATION_CONTEXT ( 'automotive_design' ) ;
#48783 = EDGE_CURVE ( 'NONE', #1414, #35778, #47844, .T. ) ;
#48784 = CARTESIAN_POINT ( 'NONE',  ( -2.739355103387248747, -14.76959508014216738, 2.169476462111838977 ) ) ;
#48785 = ORIENTED_EDGE ( 'NONE', *, *, #27378, .F. ) ;
#48786 = DIRECTION ( 'NONE',  ( -1.000000000000000000, 0.000000000000000000, 0.000000000000000000 ) ) ;
#48787 = CARTESIAN_POINT ( 'NONE',  ( 5.901764892641288895, 1.612679500413170652, 48.94272910523713449 ) ) ;
#48788 = ORIENTED_EDGE ( 'NONE', *, *, #60357, .F. ) ;
#48789 = CARTESIAN_POINT ( 'NONE',  ( 5.896782393890504181, -17.30187591025955030, -10.25529994022567237 ) ) ;
#48790 = CARTESIAN_POINT ( 'NONE',  ( 2.301529144917014325, -28.20894756932170466, 38.87759814529768931 ) ) ;
#48791 = CARTESIAN_POINT ( 'NONE',  ( 0.7948884756798498818, 21.93744097139700600, 43.92547470690128364 ) ) ;
#48792 = FACE_OUTER_BOUND ( 'NONE', #12302, .T. ) ;
#48793 = VECTOR ( 'NONE', #11085, 1000.000000000000227 ) ;
#48794 = ORIENTED_EDGE ( 'NONE', *, *, #16258, .F. ) ;
#48795 = B_SPLINE_CURVE_WITH_KNOTS ( 'NONE', 3,
 ( #17394, #27720, #36516, #3889 ),
 .UNSPECIFIED., .F., .F.,
 ( 4, 4 ),
 ( 0.000000000000000000, 0.005014147105413707325 ),
 .UNSPECIFIED. ) ;
#48796 = CARTESIAN_POINT ( 'NONE',  ( 0.6001305935487422083, 44.64600790884054504, -17.92615948558495376 ) ) ;
#48797 = CARTESIAN_POINT ( 'NONE',  ( 5.901463166500146684, -7.242130809805130021, -18.76351277544553753 ) ) ;
#48798 = ORIENTED_EDGE ( 'NONE', *, *, #32980, .F. ) ;
#48799 = CARTESIAN_POINT ( 'NONE',  ( 4.549368137175248350, -35.57418903283098643, -24.02461520945259466 ) ) ;
#48800 = VERTEX_POINT ( 'NONE', #42233 ) ;
#48801 = CARTESIAN_POINT ( 'NONE',  ( 0.8554163680231720024, 21.74163052365390669, -41.57531689939042963 ) ) ;
#48802 = ADVANCED_FACE ( 'NONE', ( #61291 ), #39746, .F. ) ;
#48803 = VECTOR ( 'NONE', #36777, 1000.000000000000114 ) ;
#48804 = ORIENTED_EDGE ( 'NONE', *, *, #4893, .T. ) ;
#48805 = CARTESIAN_POINT ( 'NONE',  ( 5.838029081930955932, 1.558325986592309587, 47.20843863413013253 ) ) ;
#48806 = CARTESIAN_POINT ( 'NONE',  ( 0.8551540677456739292, -41.03346287276411886, -24.74404575822818231 ) ) ;
#48807 = CARTESIAN_POINT ( 'NONE',  ( -2.601141883200665639, -10.40580972892344036, -10.70114719807324732 ) ) ;
#48808 = EDGE_LOOP ( 'NONE', ( #47704, #46588, #9512, #18242 ) ) ;
#48809 = CARTESIAN_POINT ( 'NONE',  ( 0.5838002273316420521, 6.116619957188743406, 47.50378804015148404 ) ) ;
#48810 = EDGE_CURVE ( 'NONE', #6553, #55243, #6113, .T. ) ;
#48811 = CARTESIAN_POINT ( 'NONE',  ( 0.5837374860065650539, -6.071555045024926933, 47.50965286059331305 ) ) ;
#48812 = EDGE_LOOP ( 'NONE', ( #45380, #11762, #9483, #36564 ) ) ;
#48813 = EDGE_CURVE ( 'NONE', #29981, #44808, #4235, .T. ) ;
#48814 = VERTEX_POINT ( 'NONE', #34359 ) ;
#48815 = CARTESIAN_POINT ( 'NONE',  ( -6.015611763856276717, -2.465697960550925938, -18.68122482568282550 ) ) ;
#48816 = CARTESIAN_POINT ( 'NONE',  ( 0.8551540677456715978, -46.51172240253128365, 11.51835730326463292 ) ) ;
#48817 = CARTESIAN_POINT ( 'NONE',  ( -6.078457390727109555, 7.798524762019232170, 17.60617853407379130 ) ) ;
#48818 = CARTESIAN_POINT ( 'NONE',  ( 2.301430502907643838, -42.22699195640122838, 22.89309745268816343 ) ) ;
#48819 = CARTESIAN_POINT ( 'NONE',  ( 3.238741278300274029, -27.59904135366560496, 32.96375560769450175 ) ) ;
#48820 = CARTESIAN_POINT ( 'NONE',  ( -6.001507490154110336, -2.475062734132314812, -18.68062548815628432 ) ) ;
#48821 = ORIENTED_EDGE ( 'NONE', *, *, #44588, .F. ) ;
#48822 = CARTESIAN_POINT ( 'NONE',  ( 4.975610109902397937, 42.33317580307156192, -24.50207406657668230 ) ) ;
#48823 = ORIENTED_EDGE ( 'NONE', *, *, #16706, .F. ) ;
#48824 = TOROIDAL_SURFACE ( 'NONE', #4736, 15.71999999999999353, 0.2800000000000011924 ) ;
#48825 = CARTESIAN_POINT ( 'NONE',  ( -6.063463321072278589, 18.63085535290914052, -4.869464169541319443 ) ) ;
#48827 = ADVANCED_FACE ( 'NONE', ( #58740 ), #26823, .F. ) ;
#48826 = CARTESIAN_POINT ( 'NONE',  ( 5.896782393890504181, 0.6784186533438157918, 20.10138888258240186 ) ) ;
#48828 = CARTESIAN_POINT ( 'NONE',  ( 0.1139756605157203201, -42.57864162325638802, 11.57646307009704856 ) ) ;
#48829 = CARTESIAN_POINT ( 'NONE',  ( 0.8551540677456739292, 43.91216198251539993, 19.17641535420868593 ) ) ;
#48830 = CARTESIAN_POINT ( 'NONE',  ( 0.5988103564986360094, -47.61318305157298880, 6.880138274944153309 ) ) ;
#48831 = DIRECTION ( 'NONE',  ( -1.000000000000000000, -0.000000000000000000, -0.000000000000000000 ) ) ;
#48832 = CARTESIAN_POINT ( 'NONE',  ( -2.099999999999999645, 2.571758278209440971E-16, -0.2800830152838832965 ) ) ;
#48833 = FACE_OUTER_BOUND ( 'NONE', #39549, .T. ) ;
#48834 = CARTESIAN_POINT ( 'NONE',  ( 5.896278296736517710, 17.95357321928074512, -9.066211351733914015 ) ) ;
#48835 = CARTESIAN_POINT ( 'NONE',  ( 4.975610109902397937, 0.000000000000000000, 0.000000000000000000 ) ) ;
#48836 = VECTOR ( 'NONE', #61206, 1000.000000000000000 ) ;
#48837 = DIRECTION ( 'NONE',  ( 0.000000000000000000, 0.000000000000000000, 1.000000000000000000 ) ) ;
#48838 = CARTESIAN_POINT ( 'NONE',  ( 3.221118495291109163, -19.51545154787827840, -39.41964701191737674 ) ) ;
#48839 = LINE ( 'NONE', #38237, #24694 ) ;
#48840 = STYLED_ITEM ( 'NONE', ( #14408 ), #4831 ) ;
#48841 = ORIENTED_EDGE ( 'NONE', *, *, #26667, .T. ) ;
#48842 = AXIS2_PLACEMENT_3D ( 'NONE', #37363, #32349, #51422 ) ;
#48843 = CARTESIAN_POINT ( 'NONE',  ( 1.231276596079881935, -41.24008908601427237, 7.518764738683684001 ) ) ;
#48844 = DIRECTION ( 'NONE',  ( -1.000000000000000000, -0.000000000000000000, -0.000000000000000000 ) ) ;
#48845 = CARTESIAN_POINT ( 'NONE',  ( 0.6021447746440204973, -47.56697795495951908, -12.20343178457942912 ) ) ;
#48846 = CARTESIAN_POINT ( 'NONE',  ( 1.231276596079887264, -30.51591784428387655, 28.74118176309011830 ) ) ;
#48847 = CARTESIAN_POINT ( 'NONE',  ( 4.956653778117001252, 45.71126949320271393, -14.93973939759840519 ) ) ;
#48848 = ORIENTED_EDGE ( 'NONE', *, *, #40723, .F. ) ;
#48849 = EDGE_CURVE ( 'NONE', #7742, #21941, #7231, .T. ) ;
#48850 = CARTESIAN_POINT ( 'NONE',  ( 4.958415959904820092, -31.93886907500617056, 32.29725369179636374 ) ) ;
#48851 = CARTESIAN_POINT ( 'NONE',  ( 0.9752570700956805227, 16.63323182627922492, -39.55341424149091267 ) ) ;
#48852 = EDGE_CURVE ( 'NONE', #27996, #17526, #55064, .T. ) ;
#48853 = CARTESIAN_POINT ( 'NONE',  ( 5.901463166500145796, 10.83443963266029186, -16.94499301229943455 ) ) ;
#48854 = EDGE_LOOP ( 'NONE', ( #30215, #60561, #8409, #9006 ) ) ;
#48855 = CARTESIAN_POINT ( 'NONE',  ( -6.016761891674565099, -18.68153697670640057, -2.462934516564000198 ) ) ;
#48856 = EDGE_CURVE ( 'NONE', #23449, #22677, #2022, .T. ) ;
#48857 = LINE ( 'NONE', #34468, #50955 ) ;
#48858 = VERTEX_POINT ( 'NONE', #24330 ) ;
#48859 = AXIS2_PLACEMENT_3D ( 'NONE', #57780, #47488, #18677 ) ;
#48860 = CARTESIAN_POINT ( 'NONE',  ( 5.974727161628369032, -0.01551142186663802443, 20.52494643607030156 ) ) ;
#48861 = VECTOR ( 'NONE', #37930, 1000.000000000000000 ) ;
#48862 = VERTEX_POINT ( 'NONE', #19646 ) ;
#48863 = CARTESIAN_POINT ( 'NONE',  ( 4.834790513006555379, 43.96797211434383001, 17.30337449969409036 ) ) ;
#48864 = ORIENTED_EDGE ( 'NONE', *, *, #1209, .F. ) ;
#48865 = CARTESIAN_POINT ( 'NONE',  ( 4.967162193818130511, 2.375726030842579828, 43.02067033766019932 ) ) ;
#48866 = DIRECTION ( 'NONE',  ( -0.07836865515943410021, 0.7104869166657039603, 0.6993330359244890326 ) ) ;
#48867 = ORIENTED_EDGE ( 'NONE', *, *, #30649, .F. ) ;
#48868 = CARTESIAN_POINT ( 'NONE',  ( 4.956653778116966613, 0.000000000000000000, 0.000000000000000000 ) ) ;
#48869 = VERTEX_POINT ( 'NONE', #49060 ) ;
#48870 = CARTESIAN_POINT ( 'NONE',  ( 0.2885700199627501683, -41.43179222486428159, 11.93479339212595391 ) ) ;
#48871 = CARTESIAN_POINT ( 'NONE',  ( 0.1139756605157202923, -1.016815145924514940, 44.11259804924259242 ) ) ;
#48872 =( BOUNDED_SURFACE ( )  B_SPLINE_SURFACE ( 3, 1, ( 
 ( #14369, #33477 ),
 ( #47880, #33791 ),
 ( #864, #14680 ),
 ( #544, #52870 ) ),
 .UNSPECIFIED., .F., .F., .F. ) 
 B_SPLINE_SURFACE_WITH_KNOTS ( ( 4, 4 ),
 ( 2, 2 ),
 ( 0.000000000000000000, 1.000000000000000000 ),
 ( 0.000000000000000000, 1.000000000000000000 ),
 .UNSPECIFIED. ) 
 GEOMETRIC_REPRESENTATION_ITEM ( )  RATIONAL_B_SPLINE_SURFACE ( (
 ( 1.000000000000000000, 1.000000000000000000),
 ( 0.9729067724841187204, 0.9999501103223794596),
 ( 0.9729067724841187204, 0.9999501103223794596),
 ( 1.000000000000000000, 1.000000000000000000) ) ) 
 REPRESENTATION_ITEM ( '' )  SURFACE ( )  );
#48873 = EDGE_CURVE ( 'NONE', #40968, #26687, #22844, .T. ) ;
#48874 = ORIENTED_EDGE ( 'NONE', *, *, #38672, .F. ) ;
#48875 = CARTESIAN_POINT ( 'NONE',  ( 0.6000166863083090663, 44.01764848084281567, -21.77774331572052802 ) ) ;
#48876 = CARTESIAN_POINT ( 'NONE',  ( 4.967162193818129623, -19.45289607368849616, 38.44485641567065670 ) ) ;
#48877 = CIRCLE ( 'NONE', #29867, 48.09070567114147110 ) ;
#48878 = CARTESIAN_POINT ( 'NONE',  ( 0.6064782688330895288, -34.30055712449948402, -31.98134186315069272 ) ) ;
#48879 = CARTESIAN_POINT ( 'NONE',  ( 0.1119899015040012186, -6.487605976147421849, -43.64484250046918845 ) ) ;
#48880 = ORIENTED_EDGE ( 'NONE', *, *, #8319, .T. ) ;
#48881 = EDGE_CURVE ( 'NONE', #4904, #11211, #15476, .T. ) ;
#48882 = DIRECTION ( 'NONE',  ( -0.07836865515943411409, 0.4916162952473615566, -0.8672783706145107407 ) ) ;
#48883 = CARTESIAN_POINT ( 'NONE',  ( 1.227938101723757836, -10.28900963485409292, 41.66816631169188412 ) ) ;
#48884 = ORIENTED_EDGE ( 'NONE', *, *, #59321, .T. ) ;
#48885 = CARTESIAN_POINT ( 'NONE',  ( 0.7056555295713310416, 47.37451042924662659, -7.085402321211308418 ) ) ;
#48886 = EDGE_CURVE ( 'NONE', #49767, #18458, #43908, .T. ) ;
#48887 = VERTEX_POINT ( 'NONE', #53432 ) ;
#48888 = PRODUCT_DEFINITION_FORMATION_WITH_SPECIFIED_SOURCE ( 'ANY', '', #3260, .NOT_KNOWN. ) ;
#48889 = CARTESIAN_POINT ( 'NONE',  ( 0.5800708057587387056, -47.56394202401741467, 5.628966369368871625 ) ) ;
#48890 = CARTESIAN_POINT ( 'NONE',  ( 0.1129192098497455998, 24.84520063729130612, 36.46461014570008530 ) ) ;
#48891 = ORIENTED_EDGE ( 'NONE', *, *, #51261, .T. ) ;
#48892 = CARTESIAN_POINT ( 'NONE',  ( 0.5817216825391136048, 5.146892874490390568, 46.61270691502455321 ) ) ;
#48893 = CARTESIAN_POINT ( 'NONE',  ( -6.077587904424778920, 5.472951620448459842, 18.46192898789725945 ) ) ;
#48894 = CARTESIAN_POINT ( 'NONE',  ( 52.60679555148794861, 12.39585383992677059, 1.616669970113162824 ) ) ;
#48895 = CARTESIAN_POINT ( 'NONE',  ( 0.000000000000000000, 0.000000000000000000, -5.574599999999999334 ) ) ;
#48896 = VERTEX_POINT ( 'NONE', #10542 ) ;
#48897 = CARTESIAN_POINT ( 'NONE',  ( 0.6009453534118439633, 18.81239552212984734, -44.27682103112812229 ) ) ;
#48898 = B_SPLINE_CURVE_WITH_KNOTS ( 'NONE', 3,
 ( #5463, #44053, #14599, #47798, #28987, #39034, #57456, #58087, #48707, #5763, #1082, #20218, #56860, #16130, #20825, #44350, #16746, #7000, #16429 ),
 .UNSPECIFIED., .F., .F.,
 ( 4, 3, 3, 3, 3, 3, 4 ),
 ( 5.204170427930421283E-18, 0.0002724573126191742376, 0.0004086839781548464172, 0.0005449106435901809441, 0.0006811373090491470127, 0.0008459866663933670976, 0.001010840725717214450 ),
 .UNSPECIFIED. ) ;
#48899 = VECTOR ( 'NONE', #15259, 1000.000000000000114 ) ;
#48901 = ADVANCED_FACE ( 'NONE', ( #29637 ), #43397, .F. ) ;
#48900 = CARTESIAN_POINT ( 'NONE',  ( 0.8557997880470599172, -5.347802024196930404, -47.60865952217005059 ) ) ;
#48902 = DIRECTION ( 'NONE',  ( -0.07439287786467650709, -0.9597484305373210622, 0.2708295585865034272 ) ) ;
#48903 = CARTESIAN_POINT ( 'NONE',  ( 0.7762777257811889209, 46.03397617421228460, 13.25585385760123813 ) ) ;
#48904 = DIRECTION ( 'NONE',  ( -1.000000000000000000, -0.000000000000000000, -0.000000000000000000 ) ) ;
#48905 = VECTOR ( 'NONE', #25805, 1000.000000000000114 ) ;
#48906 = CARTESIAN_POINT ( 'NONE',  ( 0.1073791018717483448, 6.109314776652144729, 42.68962945260955877 ) ) ;
#48907 = VECTOR ( 'NONE', #41198, 1000.000000000000000 ) ;
#48908 = CARTESIAN_POINT ( 'NONE',  ( -16.58652169825008116, -7.842521733728388789, -1.582602419930230209 ) ) ;
#48909 = CARTESIAN_POINT ( 'NONE',  ( 4.975801465491695552, -36.39623109580445259, -31.15993731089111662 ) ) ;
#48910 = DIRECTION ( 'NONE',  ( -1.000000000000000000, -0.000000000000000000, -0.000000000000000000 ) ) ;
#48911 = CARTESIAN_POINT ( 'NONE',  ( 4.975801465491695552, 0.000000000000000000, 0.000000000000000000 ) ) ;
#48912 = CARTESIAN_POINT ( 'NONE',  ( -6.000000000000001776, 4.730042041638951881E-15, 0.000000000000000000 ) ) ;
#48913 = CARTESIAN_POINT ( 'NONE',  ( -6.016104459813371719, 4.882138007282748937, 18.19977249352312398 ) ) ;
#48914 = B_SPLINE_CURVE_WITH_KNOTS ( 'NONE', 3,
 ( #59591, #60507, #2579, #50201 ),
 .UNSPECIFIED., .F., .F.,
 ( 4, 4 ),
 ( 2.338762560254090381E-17, 0.004564976165746187711 ),
 .UNSPECIFIED. ) ;
#48915 = CARTESIAN_POINT ( 'NONE',  ( 4.967162193818130511, 28.74031574030056646, -32.10009971360042158 ) ) ;
#48916 = FACE_OUTER_BOUND ( 'NONE', #58153, .T. ) ;
#48917 = VERTEX_POINT ( 'NONE', #26793 ) ;
#48918 = CONICAL_SURFACE ( 'NONE', #15940, 42.08604991992415023, 1.569615340895231137 ) ;
#48919 = CARTESIAN_POINT ( 'NONE',  ( 0.8557997880470697982, 34.51495345639548873, 33.22501220301912639 ) ) ;
#48920 = DIRECTION ( 'NONE',  ( 0.000000000000000000, 0.000000000000000000, 1.000000000000000000 ) ) ;
#48921 = CARTESIAN_POINT ( 'NONE',  ( 2.526552050251863246, -34.82218744039922598, 25.19159344346109108 ) ) ;
#48922 = ORIENTED_EDGE ( 'NONE', *, *, #8967, .F. ) ;
#48923 = EDGE_CURVE ( 'NONE', #48322, #18237, #22250, .T. ) ;
#48924 = CARTESIAN_POINT ( 'NONE',  ( 0.6253024248130482077, -14.62917846302403291, 46.87676785908598731 ) ) ;
#48925 = CARTESIAN_POINT ( 'NONE',  ( 0.1313383488274120214, -39.59253935480808906, 17.09007684155433537 ) ) ;
#48926 = EDGE_CURVE ( 'NONE', #19080, #34420, #58833, .T. ) ;
#48927 = AXIS2_PLACEMENT_3D ( 'NONE', #57024, #48481, #17146 ) ;
#48928 = ORIENTED_EDGE ( 'NONE', *, *, #57655, .T. ) ;
#48929 = ORIENTED_EDGE ( 'NONE', *, *, #49050, .T. ) ;
#48930 = CARTESIAN_POINT ( 'NONE',  ( 5.959547316686252039, 5.308980600728456345, -19.82715097195157128 ) ) ;
#48931 = EDGE_CURVE ( 'NONE', #50728, #55180, #13872, .T. ) ;
#48932 = ORIENTED_EDGE ( 'NONE', *, *, #51962, .T. ) ;
#48933 = EDGE_CURVE ( 'NONE', #41808, #19302, #414, .T. ) ;
#48934 = CARTESIAN_POINT ( 'NONE',  ( 1.088908134280560214, 25.50067491870088787, -34.51503525510825909 ) ) ;
#48935 = EDGE_CURVE ( 'NONE', #23152, #30283, #48266, .T. ) ;
#48936 = VERTEX_POINT ( 'NONE', #22098 ) ;
#48937 = VERTEX_POINT ( 'NONE', #45932 ) ;
#48938 = CARTESIAN_POINT ( 'NONE',  ( 0.1092355843206037486, 10.87081649985031362, 41.73183925352184787 ) ) ;
#48939 = ORIENTED_EDGE ( 'NONE', *, *, #32993, .F. ) ;
#48940 = CARTESIAN_POINT ( 'NONE',  ( 0.1365634738349425226, -11.94249462058610511, -42.47633978888153905 ) ) ;
#48941 = B_SPLINE_CURVE_WITH_KNOTS ( 'NONE', 3,
 ( #31626, #60725, #13152, #21303, #26304, #3102 ),
 .UNSPECIFIED., .F., .F.,
 ( 4, 2, 4 ),
 ( 1.208080024524897422E-16, 0.0002448718616795926627, 0.0004897437233590644368 ),
 .UNSPECIFIED. ) ;
#48942 = CARTESIAN_POINT ( 'NONE',  ( 0.7242486021783812733, 46.85219368132524664, -14.69297143608327261 ) ) ;
#48943 = ORIENTED_EDGE ( 'NONE', *, *, #23632, .F. ) ;
#48944 = CARTESIAN_POINT ( 'NONE',  ( 1.091591847532197290, -34.10780222139759132, -24.36014816420187401 ) ) ;
#48945 =( BOUNDED_SURFACE ( )  B_SPLINE_SURFACE ( 3, 1, ( 
 ( #46083, #2509 ),
 ( #31339, #3127 ),
 ( #26951, #34579 ),
 ( #44307, #25163 ) ),
 .UNSPECIFIED., .F., .F., .F. ) 
 B_SPLINE_SURFACE_WITH_KNOTS ( ( 4, 4 ),
 ( 2, 2 ),
 ( 0.000000000000000000, 1.000000000000000000 ),
 ( 0.000000000000000000, 1.000000000000000000 ),
 .UNSPECIFIED. ) 
 GEOMETRIC_REPRESENTATION_ITEM ( )  RATIONAL_B_SPLINE_SURFACE ( (
 ( 1.000000000000000000, 1.000000000000000000),
 ( 0.7269869731126817891, 0.9931720237060910339),
 ( 0.7269869731126817891, 0.9931720237060910339),
 ( 1.000000000000000000, 1.000000000000000000) ) ) 
 REPRESENTATION_ITEM ( '' )  SURFACE ( )  );
#48946 = AXIS2_PLACEMENT_3D ( 'NONE', #60698, #21586, #26584 ) ;
#48947 = EDGE_CURVE ( 'NONE', #58301, #25935, #42296, .T. ) ;
#48948 = CARTESIAN_POINT ( 'NONE',  ( 5.895881250540457863, -19.93402233083546093, 2.676272654655019512 ) ) ;
#48949 = ORIENTED_EDGE ( 'NONE', *, *, #58617, .F. ) ;
#48950 = EDGE_CURVE ( 'NONE', #45191, #3699, #32880, .T. ) ;
#48951 = ORIENTED_EDGE ( 'NONE', *, *, #13387, .F. ) ;
#48952 = CARTESIAN_POINT ( 'NONE',  ( 0.1368894036331260167, 43.42692794240723941, 7.807896990118506686 ) ) ;
#48953 = VECTOR ( 'NONE', #26947, 1000.000000000000227 ) ;
#48954 = CARTESIAN_POINT ( 'NONE',  ( -6.010958268070873523, -17.40352239307052784, -7.224487401384482865 ) ) ;
#48955 = CARTESIAN_POINT ( 'NONE',  ( 0.5809828226811553087, 46.40184912890838831, 11.86925843957183879 ) ) ;
#48956 = CARTESIAN_POINT ( 'NONE',  ( 0.9783242366443563043, 35.92089602389015113, 21.58758251975879361 ) ) ;
#48957 = ORIENTED_EDGE ( 'NONE', *, *, #12842, .T. ) ;
#48958 = CARTESIAN_POINT ( 'NONE',  ( 0.6031357023905875581, -12.49325238079570610, 46.45693331047437624 ) ) ;
#48959 = CARTESIAN_POINT ( 'NONE',  ( -6.077587904424778920, 17.84644683124317055, -7.231898567702747194 ) ) ;
#48960 = CARTESIAN_POINT ( 'NONE',  ( 0.8753041380234465318, 48.01981714478390728, 10.25843502950123209 ) ) ;
#48961 = DIRECTION ( 'NONE',  ( 0.07500201931887537365, -0.9232442575324723011, 0.3768218916562637855 ) ) ;
#48962 = VERTEX_POINT ( 'NONE', #16173 ) ;
#48963 = CARTESIAN_POINT ( 'NONE',  ( 1.657374760986086271, -42.91185007314042821, -9.973142461258767355 ) ) ;
#48964 = CARTESIAN_POINT ( 'NONE',  ( 4.956445790444004018, -46.59545590650535019, -6.811867512257778756 ) ) ;
#48965 = CARTESIAN_POINT ( 'NONE',  ( 3.559346040607745287, 7.771245481046687331, -43.27860932626300894 ) ) ;
#48966 = CARTESIAN_POINT ( 'NONE',  ( 0.5549461598389365813, -6.171197268387964563, 43.67074558261452211 ) ) ;
#48967 = ORIENTED_EDGE ( 'NONE', *, *, #48587, .F. ) ;
#48968 = B_SPLINE_CURVE_WITH_KNOTS ( 'NONE', 3,
 ( #60179, #7235, #31071, #59871, #26989, #50176, #51083, #1926, #21053, #45199, #26360, #2226, #45496, #21668, #40812, #16988, #17288, #36104, #31379 ),
 .UNSPECIFIED., .F., .F.,
 ( 4, 3, 3, 3, 3, 3, 4 ),
 ( 4.336808689942017736E-18, 0.0002724573126191742376, 0.0004086839781548492903, 0.0005449106435901836546, 0.0006811373090491489642, 0.0008459866663933718681, 0.001010840725717213583 ),
 .UNSPECIFIED. ) ;
#48969 = ORIENTED_EDGE ( 'NONE', *, *, #57125, .T. ) ;
#48970 = CARTESIAN_POINT ( 'NONE',  ( -17.97369999999976642, -7.719455939378113030, 2.099999999999994760 ) ) ;
#48971 = CARTESIAN_POINT ( 'NONE',  ( 0.8760168074886965917, -34.63873394077511136, 33.37827814204064936 ) ) ;
#48972 = CARTESIAN_POINT ( 'NONE',  ( 0.1103878639767399417, -39.82320122342716928, 16.54784522866399499 ) ) ;
#48974 = EDGE_CURVE ( 'NONE', #5781, #25122, #20640, .T. ) ;
#48973 = CARTESIAN_POINT ( 'NONE',  ( 0.5980271706414711508, 49.05158475245164595, -2.447708339389331744 ) ) ;
#48975 = CARTESIAN_POINT ( 'NONE',  ( 0.1102847568649952675, 34.15672344772088564, -26.32556309315081222 ) ) ;
#48976 = CARTESIAN_POINT ( 'NONE',  ( 4.834790513006553603, 13.00147983508858474, 45.42632345922534398 ) ) ;
#48977 = CARTESIAN_POINT ( 'NONE',  ( 5.960721111146673579, -20.35079619394247885, 2.672857320902960243 ) ) ;
#48978 = EDGE_CURVE ( 'NONE', #35664, #15368, #55828, .T. ) ;
#48979 = DIRECTION ( 'NONE',  ( -1.000000000000000000, -0.000000000000000000, -0.000000000000000000 ) ) ;
#48980 = CARTESIAN_POINT ( 'NONE',  ( 5.981074661064941900, 20.35019299530685188, 2.670494474392067996 ) ) ;
#48981 = CARTESIAN_POINT ( 'NONE',  ( 0.1100053167205930493, 30.36644426605139913, -30.62023953839050705 ) ) ;
#48982 = CARTESIAN_POINT ( 'NONE',  ( 0.6009453534118439633, -6.711694149738577586, 47.63713118507416056 ) ) ;
#48983 = CARTESIAN_POINT ( 'NONE',  ( 0.1152809850208375980, -6.823767124828218122, -43.59336514557998754 ) ) ;
#48984 = CARTESIAN_POINT ( 'NONE',  ( 3.376099380956842921, 4.385778397990434563, -12.66780689289931949 ) ) ;
#48985 = PRODUCT_RELATED_PRODUCT_CATEGORY ( 'part', '', ( #6712 ) ) ;
#48986 = CARTESIAN_POINT ( 'NONE',  ( 0.7056555295713242693, 29.82339362082594647, 37.48482836297240794 ) ) ;
#48987 = CARTESIAN_POINT ( 'NONE',  ( 0.6009453534118440743, -24.43073772334946980, 41.44251633523849421 ) ) ;
#48988 = CARTESIAN_POINT ( 'NONE',  ( 0.6008123274975391004, 33.33610813491660707, -36.05909657181671690 ) ) ;
#48989 = CARTESIAN_POINT ( 'NONE',  ( 0.5797568599927143129, 45.39179688724399142, -11.78176913787528157 ) ) ;
#48990 = CARTESIAN_POINT ( 'NONE',  ( 1.227938101723756947, 6.439911493064564674, 42.43379953535188065 ) ) ;
#48991 = CARTESIAN_POINT ( 'NONE',  ( 0.9754402186311951217, -10.92425836141448414, 41.49454543482929125 ) ) ;
#48992 = CARTESIAN_POINT ( 'NONE',  ( 0.7954196712028467342, -47.56618050291069721, -7.138712347928016122 ) ) ;
#48993 = CARTESIAN_POINT ( 'NONE',  ( 0.6016118706126977189, 48.13416090936247116, 9.729008599828327775 ) ) ;
#48995 = ORIENTED_EDGE ( 'NONE', *, *, #20374, .F. ) ;
#48994 = CARTESIAN_POINT ( 'NONE',  ( 0.9722240741986382107, 10.54237114526883978, 41.59310805473373307 ) ) ;
#48996 = ORIENTED_EDGE ( 'NONE', *, *, #17980, .F. ) ;
#48997 = CIRCLE ( 'NONE', #31976, 15.43999999999999240 ) ;
#48998 = CARTESIAN_POINT ( 'NONE',  ( 0.1103310638050661874, -43.12437788119554227, -0.08238894504380574191 ) ) ;
#48999 = DIRECTION ( 'NONE',  ( 0.000000000000000000, 0.000000000000000000, 1.000000000000000000 ) ) ;
#49000 = CARTESIAN_POINT ( 'NONE',  ( -2.601141883200665639, -4.674544242619546708, 14.17547401652520023 ) ) ;
#49001 = VERTEX_POINT ( 'NONE', #40613 ) ;
#49002 = ORIENTED_EDGE ( 'NONE', *, *, #61076, .T. ) ;
#49003 = LINE ( 'NONE', #30195, #2265 ) ;
#49004 = CARTESIAN_POINT ( 'NONE',  ( 0.9762797500689124330, 9.222352665238359393, 40.88120590813919364 ) ) ;
#49005 = CARTESIAN_POINT ( 'NONE',  ( 1.830465331921977912, -43.51298832088521351, -6.855355808774353576 ) ) ;
#49006 = EDGE_CURVE ( 'NONE', #25607, #11251, #57217, .T. ) ;
#49007 = VERTEX_POINT ( 'NONE', #59680 ) ;
#49008 = ORIENTED_EDGE ( 'NONE', *, *, #41820, .T. ) ;
#49009 = LINE ( 'NONE', #39954, #12581 ) ;
#49010 = EDGE_CURVE ( 'NONE', #22549, #55841, #4189, .T. ) ;
#49011 = ADVANCED_FACE ( 'NONE', ( #50586 ), #45608, .F. ) ;
#49012 = CONICAL_SURFACE ( 'NONE', #42019, 42.92674063221959813, 1.485477209440487556 ) ;
#49013 = CARTESIAN_POINT ( 'NONE',  ( 5.960221823109900008, -12.49086489703240055, 16.28736530777569058 ) ) ;
#49014 = CARTESIAN_POINT ( 'NONE',  ( 0.5987334308729317378, -0.9689265936116925326, 49.09810676417087905 ) ) ;
#49015 = CARTESIAN_POINT ( 'NONE',  ( 3.407937589446174087, -13.51415833181186699, -2.242416846335737901 ) ) ;
#49016 = EDGE_CURVE ( 'NONE', #16043, #12966, #27725, .T. ) ;
#49017 = CARTESIAN_POINT ( 'NONE',  ( 0.9783242366443547500, -41.01462390377462697, -8.610175157245297584 ) ) ;
#49018 = CARTESIAN_POINT ( 'NONE',  ( -6.078726893082806448, 5.482141236671949969, 18.45914864585853721 ) ) ;
#49019 = CARTESIAN_POINT ( 'NONE',  ( 0.1119898979215348395, 43.99420329544292940, -3.386943260680373324 ) ) ;
#49020 = ORIENTED_EDGE ( 'NONE', *, *, #11547, .F. ) ;
#49021 = VERTEX_POINT ( 'NONE', #42462 ) ;
#49022 = FACE_OUTER_BOUND ( 'NONE', #37796, .T. ) ;
#49023 = CARTESIAN_POINT ( 'NONE',  ( 4.322998006666179727, 25.80712523194219088, 40.45864630878526924 ) ) ;
#49024 = ORIENTED_EDGE ( 'NONE', *, *, #11747, .F. ) ;
#49025 = CARTESIAN_POINT ( 'NONE',  ( 5.880360259849739535, 36.03610316515383261, -31.66572319753524312 ) ) ;
#49026 = CARTESIAN_POINT ( 'NONE',  ( -49.49999999999975842, 1.232595164407830946E-29, 1.078520768856852078E-29 ) ) ;
#49027 = CARTESIAN_POINT ( 'NONE',  ( 0.5804410086790514622, -20.23572001627618988, 42.30881098870866452 ) ) ;
#49028 = CARTESIAN_POINT ( 'NONE',  ( 0.1152339509894530906, -40.98274918812253986, -16.35105377150610195 ) ) ;
#49029 = ORIENTED_EDGE ( 'NONE', *, *, #22916, .T. ) ;
#49030 = CARTESIAN_POINT ( 'NONE',  ( 0.5830081025819953133, 46.44033818253048906, -6.521274712388932748 ) ) ;
#49031 = CARTESIAN_POINT ( 'NONE',  ( 0.8557997880470690211, -29.88293891557446003, -37.44587306708127983 ) ) ;
#49032 = CARTESIAN_POINT ( 'NONE',  ( 5.958863334805807099, 2.680345151634613288, -20.34989385289154740 ) ) ;
#49033 = CARTESIAN_POINT ( 'NONE',  ( 4.967162193818130511, 13.42934394584164082, 40.93989340068615945 ) ) ;
#49034 = B_SPLINE_CURVE_WITH_KNOTS ( 'NONE', 3,
 ( #3894, #14260, #56522, #46853, #36839, #60913 ),
 .UNSPECIFIED., .F., .F.,
 ( 4, 2, 4 ),
 ( 3.218090308046738493E-18, 0.0002447193893791694912, 0.0004894387787583358383 ),
 .UNSPECIFIED. ) ;
#49035 = ORIENTED_EDGE ( 'NONE', *, *, #29878, .F. ) ;
#49036 = CARTESIAN_POINT ( 'NONE',  ( 0.5850706913938534814, -47.89601588673689037, 0.1816364388698667454 ) ) ;
#49037 = VERTEX_POINT ( 'NONE', #9225 ) ;
#49038 = CARTESIAN_POINT ( 'NONE',  ( 4.956445790443998689, -4.175462451062247560, 46.90526157542890218 ) ) ;
#49039 = CARTESIAN_POINT ( 'NONE',  ( 4.833616638992208614, 15.29495699393663344, 43.64812679991126743 ) ) ;
#49040 = ORIENTED_EDGE ( 'NONE', *, *, #29902, .F. ) ;
#49041 = CARTESIAN_POINT ( 'NONE',  ( 5.894904586330512508, 0.6732998044285471995, 20.10164369983209198 ) ) ;
#49042 = CARTESIAN_POINT ( 'NONE',  ( -6.001507490154110336, 16.32705935667506836, 9.408444979392378116 ) ) ;
#49043 = CARTESIAN_POINT ( 'NONE',  ( 4.834790513006555379, 13.00147983508924376, -45.42632345922514503 ) ) ;
#49044 = B_SPLINE_CURVE_WITH_KNOTS ( 'NONE', 3,
 ( #3747, #52289, #32913, #51990 ),
 .UNSPECIFIED., .F., .F.,
 ( 4, 4 ),
 ( 0.000000000000000000, 0.004442905043737215703 ),
 .UNSPECIFIED. ) ;
#49045 = CARTESIAN_POINT ( 'NONE',  ( -6.057079549204054558, -19.21686681020089082, -1.242280603864441613 ) ) ;
#49046 = DIRECTION ( 'NONE',  ( -1.000000000000000000, -0.000000000000000000, -0.000000000000000000 ) ) ;
#49047 = CARTESIAN_POINT ( 'NONE',  ( 0.1368894036331287922, -31.24908945182261633, 31.15053345217901537 ) ) ;
#49048 = VECTOR ( 'NONE', #6997, 1000.000000000000114 ) ;
#49049 = CARTESIAN_POINT ( 'NONE',  ( 0.5839254288179549501, 46.28738487712343641, -12.30867641975529025 ) ) ;
#49050 = EDGE_CURVE ( 'NONE', #43021, #55001, #7186, .T. ) ;
#49051 = DIRECTION ( 'NONE',  ( -1.000000000000000000, -1.836909530733573776E-16, 1.925929944387235853E-32 ) ) ;
#49052 = ORIENTED_EDGE ( 'NONE', *, *, #39106, .F. ) ;
#49053 = FACE_OUTER_BOUND ( 'NONE', #44217, .T. ) ;
#49054 = CARTESIAN_POINT ( 'NONE',  ( 4.549368137175248350, 0.000000000000000000, 0.000000000000000000 ) ) ;
#49055 = CARTESIAN_POINT ( 'NONE',  ( 0.9762797500689124330, 15.53330887509081215, 38.92352888134283262 ) ) ;
#49056 = VECTOR ( 'NONE', #16096, 999.9999999999998863 ) ;
#49057 = EDGE_LOOP ( 'NONE', ( #43773, #11225, #11428, #61958 ) ) ;
#49058 = CARTESIAN_POINT ( 'NONE',  ( 3.782542959838397501, -32.30855296672242361, 26.89600822785905621 ) ) ;
#49059 = CARTESIAN_POINT ( 'NONE',  ( 4.975610109902397937, 8.374023221151757568, 48.19050883970187016 ) ) ;
#49060 = CARTESIAN_POINT ( 'NONE',  ( 0.5998501479064699549, -44.24259072156099393, 18.89267974119588445 ) ) ;
#49061 = CARTESIAN_POINT ( 'NONE',  ( 0.6001305935487315502, 17.92615948558476546, 44.64600790884062320 ) ) ;
#49062 = B_SPLINE_CURVE_WITH_KNOTS ( 'NONE', 3,
 ( #50885, #7333, #59347, #21772, #8271, #46214 ),
 .UNSPECIFIED., .F., .F.,
 ( 4, 2, 4 ),
 ( 6.040475531737862511E-18, 0.0002291472222819939113, 0.0004582944445639817511 ),
 .UNSPECIFIED. ) ;
#49063 = CARTESIAN_POINT ( 'NONE',  ( 0.6016117650947688800, -19.55888191429318468, 45.04443575523212218 ) ) ;
#49064 = CARTESIAN_POINT ( 'NONE',  ( 0.5998501479064699549, 48.10473956285920138, -0.5236536531309904374 ) ) ;
#49065 = B_SPLINE_CURVE_WITH_KNOTS ( 'NONE', 3,
 ( #39414, #29987, #16512, #50024 ),
 .UNSPECIFIED., .F., .F.,
 ( 4, 4 ),
 ( 9.490380264008620755E-17, 0.005004948556313905915 ),
 .UNSPECIFIED. ) ;
#49066 = DIRECTION ( 'NONE',  ( 6.853073559125476786E-15, 0.7071067811865437980, 0.7071067811865512365 ) ) ;
#49067 = CARTESIAN_POINT ( 'NONE',  ( 5.910764540655177868, -11.91768246006605381, -16.20092846876983828 ) ) ;
#49068 = B_SPLINE_CURVE_WITH_KNOTS ( 'NONE', 3,
 ( #11263, #30355, #44807, #59472 ),
 .UNSPECIFIED., .F., .F.,
 ( 4, 4 ),
 ( 0.000000000000000000, 0.005013413432710142441 ),
 .UNSPECIFIED. ) ;
#49069 = CARTESIAN_POINT ( 'NONE',  ( 0.8751705887134553219, 46.67919521768871505, 11.58504748649215976 ) ) ;
#49070 = CARTESIAN_POINT ( 'NONE',  ( 4.967162193818130511, 18.65818244221310351, -38.83676580803746958 ) ) ;
#49072 = ORIENTED_EDGE ( 'NONE', *, *, #60749, .T. ) ;
#49071 = CARTESIAN_POINT ( 'NONE',  ( 0.8744876279028306332, 48.35212675551500183, 8.510105087371359289 ) ) ;
#49073 = VERTEX_POINT ( 'NONE', #27405 ) ;
#49074 = CARTESIAN_POINT ( 'NONE',  ( 0.5837374860065648319, -12.22086613152793610, 46.31070423340725029 ) ) ;
#49075 = CARTESIAN_POINT ( 'NONE',  ( 0.8551540677456834771, -47.61725548905986471, -5.348818140991398629 ) ) ;
#49076 = CARTESIAN_POINT ( 'NONE',  ( 0.1092355843206037486, 16.22491322981570860, 39.95589129953373941 ) ) ;
#49077 = EDGE_CURVE ( 'NONE', #22282, #15568, #49034, .T. ) ;
#49078 = CARTESIAN_POINT ( 'NONE',  ( 4.956653778116975495, -8.845409907521238679, 47.27023054223749909 ) ) ;
#49079 = CARTESIAN_POINT ( 'NONE',  ( 5.838029081930957709, -37.05692651727552800, 29.28906374820066461 ) ) ;
#49080 = CARTESIAN_POINT ( 'NONE',  ( 0.1154773475650540809, 9.643119492786247804, -43.05756468373434842 ) ) ;
#49081 = EDGE_CURVE ( 'NONE', #45060, #42739, #54217, .T. ) ;
#49082 = VERTEX_POINT ( 'NONE', #57128 ) ;
#49083 = ORIENTED_EDGE ( 'NONE', *, *, #58755, .T. ) ;
#49084 = ADVANCED_FACE ( 'NONE', ( #56828 ), #26911, .F. ) ;
#49085 = CARTESIAN_POINT ( 'NONE',  ( 0.7056313189692725585, -38.18416368027698127, 27.23450546632662039 ) ) ;
#49086 = LINE ( 'NONE', #33775, #4172 ) ;
#49087 = CARTESIAN_POINT ( 'NONE',  ( 0.8551540677456834771, -17.49081417858818810, 44.61036085020945308 ) ) ;
#49088 = VERTEX_POINT ( 'NONE', #18027 ) ;
#49089 = ADVANCED_FACE ( 'NONE', ( #47154 ), #54135, .F. ) ;
#49090 = CARTESIAN_POINT ( 'NONE',  ( 0.1092355843206037486, -0.3005923759136885365, 43.12343565949664992 ) ) ;
#49091 = CARTESIAN_POINT ( 'NONE',  ( 4.553261556744873317, 17.98701270972406618, 40.07501640179154379 ) ) ;
#49092 = ORIENTED_EDGE ( 'NONE', *, *, #55367, .F. ) ;
#49093 = CIRCLE ( 'NONE', #41122, 42.08604991992415023 ) ;
#49094 = DIRECTION ( 'NONE',  ( 0.07836865515943412797, 0.1379401902675633507, -0.9873352307081167956 ) ) ;
#49095 = VERTEX_POINT ( 'NONE', #22401 ) ;
#49096 = CARTESIAN_POINT ( 'NONE',  ( 4.960386119450151732, 17.98972314615696177, 39.88491351121328421 ) ) ;
#49097 = EDGE_CURVE ( 'NONE', #61466, #35404, #15828, .T. ) ;
#49098 = CARTESIAN_POINT ( 'NONE',  ( 4.975610109902397937, 20.32389311291169065, 44.49032227207074186 ) ) ;
#49099 = ORIENTED_EDGE ( 'NONE', *, *, #32748, .T. ) ;
#49100 = CARTESIAN_POINT ( 'NONE',  ( -6.072942160501519027, -11.02874586101359000, 15.78514893886643122 ) ) ;
#49101 = CARTESIAN_POINT ( 'NONE',  ( 0.6000166863083106206, 46.44114019838972496, 15.97009639238170919 ) ) ;
#49102 = CARTESIAN_POINT ( 'NONE',  ( 0.7242486021783836048, -48.58740928524382952, -7.090495139422609228 ) ) ;
#49103 = CARTESIAN_POINT ( 'NONE',  ( 0.6000166863083106206, 5.235566842224463890, 48.83044461756470866 ) ) ;
#49104 = ADVANCED_FACE ( 'NONE', ( #15176 ), #18496, .F. ) ;
#49105 = ORIENTED_EDGE ( 'NONE', *, *, #28002, .F. ) ;
#49106 = LINE ( 'NONE', #53476, #10732 ) ;
#49107 = CARTESIAN_POINT ( 'NONE',  ( 2.618530812446111078, 15.57291328060457225, 44.35325423408038148 ) ) ;
#49108 = ORIENTED_EDGE ( 'NONE', *, *, #52542, .T. ) ;
#49109 = CARTESIAN_POINT ( 'NONE',  ( 4.962356264823593932, 7.429277797797228189, 41.42513040734459651 ) ) ;
#49110 = ORIENTED_EDGE ( 'NONE', *, *, #3597, .F. ) ;
#49111 = CARTESIAN_POINT ( 'NONE',  ( 0.9789889208857709413, 4.290552630147678848, 41.68844031827409680 ) ) ;
#49112 = ORIENTED_EDGE ( 'NONE', *, *, #20722, .T. ) ;
#49113 = CARTESIAN_POINT ( 'NONE',  ( 0.8744876279028263033, 11.79038800009220722, -47.65854384249244191 ) ) ;
#49114 = CARTESIAN_POINT ( 'NONE',  ( 5.960721111146673579, 17.77882586010652943, 10.25731071096588920 ) ) ;
#49115 = CARTESIAN_POINT ( 'NONE',  ( 0.5800708057587354860, 41.16170989303203953, 24.48933404430274763 ) ) ;
#49116 = ORIENTED_EDGE ( 'NONE', *, *, #43149, .F. ) ;
#49117 = CARTESIAN_POINT ( 'NONE',  ( 0.3676999524040366896, 41.59822836379080968, -14.68121181363270367 ) ) ;
#49118 = CARTESIAN_POINT ( 'NONE',  ( 4.691466044806103852, -14.64802401911199503, -42.11359095667484098 ) ) ;
#49119 = FACE_OUTER_BOUND ( 'NONE', #12759, .T. ) ;
#49120 = EDGE_LOOP ( 'NONE', ( #29659, #11785 ) ) ;
#49121 =( BOUNDED_SURFACE ( )  B_SPLINE_SURFACE ( 3, 1, ( 
 ( #11102, #10792 ),
 ( #6046, #54907 ),
 ( #45249, #11401 ),
 ( #25800, #44324 ) ),
 .UNSPECIFIED., .F., .F., .F. ) 
 B_SPLINE_SURFACE_WITH_KNOTS ( ( 4, 4 ),
 ( 2, 2 ),
 ( 0.000000000000000000, 1.000000000000000000 ),
 ( 0.000000000000000000, 1.000000000000000000 ),
 .UNSPECIFIED. ) 
 GEOMETRIC_REPRESENTATION_ITEM ( )  RATIONAL_B_SPLINE_SURFACE ( (
 ( 1.000000000000000000, 1.000000000000000000),
 ( 0.9953390228620291325, 0.8624445117760984880),
 ( 0.9953390228620291325, 0.8624445117760984880),
 ( 1.000000000000000000, 1.000000000000000000) ) ) 
 REPRESENTATION_ITEM ( '' )  SURFACE ( )  );
#49122 = VERTEX_POINT ( 'NONE', #59529 ) ;
#49123 = CARTESIAN_POINT ( 'NONE',  ( -6.016104459813371719, -2.464823636987321986, -18.68131780085934324 ) ) ;
#49124 = CARTESIAN_POINT ( 'NONE',  ( 3.221118495291108275, 30.94270617206736063, 31.26196338061407332 ) ) ;
#49125 = CARTESIAN_POINT ( 'NONE',  ( 1.827119703190778877, 25.21842556008185099, -34.89020442382232545 ) ) ;
#49126 = CARTESIAN_POINT ( 'NONE',  ( 0.1073791018717483448, 30.83464511437097499, 30.14884492832400298 ) ) ;
#49127 = ADVANCED_FACE ( 'NONE', ( #10157, #57427 ), #4810, .T. ) ;
#49128 = CARTESIAN_POINT ( 'NONE',  ( 0.2224561200757582402, 29.94832483817993918, 31.02237548791962496 ) ) ;
#49129 = CARTESIAN_POINT ( 'NONE',  ( 4.834790513006553603, 45.58586227964563875, 12.43054709759641341 ) ) ;
#49130 = ORIENTED_EDGE ( 'NONE', *, *, #9848, .F. ) ;
#49131 = DIRECTION ( 'NONE',  ( 0.000000000000000000, -0.7071067811865435759, -0.7071067811865514585 ) ) ;
#49132 = ORIENTED_EDGE ( 'NONE', *, *, #20661, .T. ) ;
#49133 = CARTESIAN_POINT ( 'NONE',  ( 0.5835226383429279462, 36.91662246350897902, 28.92067531079992548 ) ) ;
#49134 = CARTESIAN_POINT ( 'NONE',  ( 0.6029443449137436017, -19.83806479063774475, -44.92205163776239374 ) ) ;
#49135 = CARTESIAN_POINT ( 'NONE',  ( -69.95594261585600293, 0.000000000000000000, -12.50000000000000000 ) ) ;
#49136 = CARTESIAN_POINT ( 'NONE',  ( 0.5807400328401574052, 44.45848844984468684, -17.82553128098360418 ) ) ;
#49137 = CARTESIAN_POINT ( 'NONE',  ( 1.834102595619085507, 11.06747130359428510, 42.63459655962281403 ) ) ;
#49138 =( BOUNDED_SURFACE ( )  B_SPLINE_SURFACE ( 3, 1, ( 
 ( #16090, #11384 ),
 ( #49583, #4113 ),
 ( #4412, #56438 ),
 ( #13246, #18876 ) ),
 .UNSPECIFIED., .F., .F., .F. ) 
 B_SPLINE_SURFACE_WITH_KNOTS ( ( 4, 4 ),
 ( 2, 2 ),
 ( 0.000000000000000000, 1.000000000000000000 ),
 ( 0.000000000000000000, 1.000000000000000000 ),
 .UNSPECIFIED. ) 
 GEOMETRIC_REPRESENTATION_ITEM ( )  RATIONAL_B_SPLINE_SURFACE ( (
 ( 1.000000000000000000, 1.000000000000000000),
 ( 0.9751682680413298332, 0.9999560080971552356),
 ( 0.9751682680413298332, 0.9999560080971552356),
 ( 1.000000000000000000, 1.000000000000000000) ) ) 
 REPRESENTATION_ITEM ( '' )  SURFACE ( )  );
#49139 = CONICAL_SURFACE ( 'NONE', #35155, 43.92652462719577500, 1.486293639869522343 ) ;
#49140 = CARTESIAN_POINT ( 'NONE',  ( 0.6008122571543322854, 37.10904107904137561, -32.16323398943794842 ) ) ;
#49141 = CARTESIAN_POINT ( 'NONE',  ( 5.910764540655178756, 8.479982303152816314, 18.23708141692025464 ) ) ;
#49142 = CARTESIAN_POINT ( 'NONE',  ( 0.9762797500689124330, 10.20671408566037286, -40.64662068068250278 ) ) ;
#49143 = CARTESIAN_POINT ( 'NONE',  ( 4.975610109902397937, -28.45381238669816426, 39.78479568629648355 ) ) ;
#49144 = DIRECTION ( 'NONE',  ( 0.000000000000000000, 0.000000000000000000, 1.000000000000000000 ) ) ;
#49145 = CARTESIAN_POINT ( 'NONE',  ( 0.5809828226811617480, -23.47450554821680413, -41.74875432577673706 ) ) ;
#49146 = CARTESIAN_POINT ( 'NONE',  ( 4.390527457369402420, -20.03612350786727703, -39.09909322997283709 ) ) ;
#49147 = DIRECTION ( 'NONE',  ( 0.000000000000000000, 0.000000000000000000, 1.000000000000000000 ) ) ;
#49148 = CARTESIAN_POINT ( 'NONE',  ( 0.6846871229502932144, -47.90045233486063125, -0.8641397935264564234 ) ) ;
#49149 = ORIENTED_EDGE ( 'NONE', *, *, #8921, .F. ) ;
#49150 = ADVANCED_FACE ( 'NONE', ( #54828 ), #4929, .F. ) ;
#49151 = DIRECTION ( 'NONE',  ( 0.000000000000000000, 0.000000000000000000, 1.000000000000000000 ) ) ;
#49152 = CARTESIAN_POINT ( 'NONE',  ( 0.5837800005270563641, -19.74018744120785129, -42.53892639016367383 ) ) ;
#49153 = CARTESIAN_POINT ( 'NONE',  ( -6.016761891674565099, -4.873659902332239113, -18.20201388312100477 ) ) ;
#49154 = CARTESIAN_POINT ( 'NONE',  ( 4.956653778116991482, 9.917440902361805755, -47.05699031914939212 ) ) ;
#49155 = CARTESIAN_POINT ( 'NONE',  ( 0.8560838555295223751, -44.00447048317975174, 16.24744323198866169 ) ) ;
#49156 = VERTEX_POINT ( 'NONE', #5727 ) ;
#49157 = EDGE_CURVE ( 'NONE', #19838, #38743, #31063, .T. ) ;
#49158 = CARTESIAN_POINT ( 'NONE',  ( 4.691466044806103852, 14.01607102724543097, -42.32811009116542067 ) ) ;
#49159 = CARTESIAN_POINT ( 'NONE',  ( 10.00000000000000888, 0.000000000000000000, 0.000000000000000000 ) ) ;
#49160 = EDGE_CURVE ( 'NONE', #60741, #17733, #46845, .T. ) ;
#49161 = CARTESIAN_POINT ( 'NONE',  ( 1.199999999999992628, 0.000000000000000000, 0.000000000000000000 ) ) ;
#49162 = B_SPLINE_CURVE_WITH_KNOTS ( 'NONE', 3,
 ( #25646, #44789, #20957, #8936, #125, #18041, #52146, #37158, #23350, #56535, #13972, #3594, #37465, #13651, #32442, #47166, #4207, #22729, #47466 ),
 .UNSPECIFIED., .F., .F.,
 ( 4, 3, 3, 3, 3, 3, 4 ),
 ( 0.000000000000000000, 0.0002612768053151720343, 0.0003919133833142926602, 0.0005225499612322615124, 0.0006531865391693370427, 0.0008112755173415195321, 0.0009693688056799733320 ),
 .UNSPECIFIED. ) ;
#49163 = ORIENTED_EDGE ( 'NONE', *, *, #41082, .F. ) ;
#49164 = CARTESIAN_POINT ( 'NONE',  ( 0.8751705887134423323, -44.76769609654249393, 17.57879340691464165 ) ) ;
#49165 = CARTESIAN_POINT ( 'NONE',  ( 1.088313998177380171, -41.24258460930631998, -11.85828975620052184 ) ) ;
#49166 = ORIENTED_EDGE ( 'NONE', *, *, #52261, .T. ) ;
#49167 = DIRECTION ( 'NONE',  ( 1.000000000000000000, 0.000000000000000000, 0.000000000000000000 ) ) ;
#49168 = ORIENTED_EDGE ( 'NONE', *, *, #28361, .T. ) ;
#49169 = CARTESIAN_POINT ( 'NONE',  ( 1.830465331921977024, -28.41911767823002322, 33.65605155494778700 ) ) ;
#49170 = VERTEX_POINT ( 'NONE', #11962 ) ;
#49171 = DIRECTION ( 'NONE',  ( -0.07439287786467652097, -0.01320009283085550773, -0.9971416435352944418 ) ) ;
#49172 = CARTESIAN_POINT ( 'NONE',  ( 4.691466044806102964, 29.14742760351063566, 33.74235639413337395 ) ) ;
#49173 = ORIENTED_EDGE ( 'NONE', *, *, #48453, .F. ) ;
#49174 = CARTESIAN_POINT ( 'NONE',  ( 0.8751705887134553219, -46.21789262997766201, 13.30665218149281870 ) ) ;
#49175 = EDGE_CURVE ( 'NONE', #45995, #1414, #10211, .T. ) ;
#49176 = AXIS2_PLACEMENT_3D ( 'NONE', #34033, #48415, #44365 ) ;
#49177 = ORIENTED_EDGE ( 'NONE', *, *, #56174, .T. ) ;
#49178 = CARTESIAN_POINT ( 'NONE',  ( 0.1073791018717483448, -41.52698815987176317, 11.62916352156079824 ) ) ;
#49179 = CARTESIAN_POINT ( 'NONE',  ( 0.1064266379913938604, 33.86837498006626390, -26.69589650908249467 ) ) ;
#49180 = AXIS2_PLACEMENT_3D ( 'NONE', #12737, #12420, #27124 ) ;
#49181 = B_SPLINE_CURVE_WITH_KNOTS ( 'NONE', 3,
 ( #42623, #33224, #57000, #51995, #28190, #3445, #4053, #47311, #13189, #61684, #18817, #51067, #42940, #8161, #32290, #8454, #22892, #15348, #25351, #10959, #19738, #597, #34456, #29733, #53830 ),
 .UNSPECIFIED., .F., .F.,
 ( 4, 3, 3, 3, 3, 3, 3, 3, 4 ),
 ( 6.254634441385501517E-18, 0.0005656085177311410495, 0.001131215744874500924, 0.001696821861372766133, 0.002262427090022499018, 0.002828031679238747226, 0.003393635864401604862, 0.003977030878808132490, 0.004561030005651159867 ),
 .UNSPECIFIED. ) ;
#49182 = ORIENTED_EDGE ( 'NONE', *, *, #8269, .T. ) ;
#49183 = DIRECTION ( 'NONE',  ( 0.000000000000000000, -0.7071067811865553443, 0.7071067811865395791 ) ) ;
#49184 = CARTESIAN_POINT ( 'NONE',  ( 4.975610109902397937, -37.61482235126175766, 31.26618855282478648 ) ) ;
#49185 = CARTESIAN_POINT ( 'NONE',  ( 0.8744876279028263033, -14.81965677138014037, 46.80521149998127584 ) ) ;
#49186 = CARTESIAN_POINT ( 'NONE',  ( 0.2940133293163009753, -6.245378493101266137, -43.67191084731638995 ) ) ;
#49187 = ORIENTED_EDGE ( 'NONE', *, *, #55692, .T. ) ;
#49188 = FACE_OUTER_BOUND ( 'NONE', #47422, .T. ) ;
#49189 = CARTESIAN_POINT ( 'NONE',  ( -6.063463321072276813, 15.44190279602993243, 11.50513322467118549 ) ) ;
#49190 = B_SPLINE_CURVE_WITH_KNOTS ( 'NONE', 3,
 ( #15445, #30443, #54544, #34866, #53936, #11062 ),
 .UNSPECIFIED., .F., .F.,
 ( 4, 2, 4 ),
 ( 1.449324869460184762E-16, 0.0002445252820015209245, 0.0004890505640028968912 ),
 .UNSPECIFIED. ) ;
#49191 = EDGE_LOOP ( 'NONE', ( #54954, #29375, #46679, #21439 ) ) ;
#49192 = CARTESIAN_POINT ( 'NONE',  ( 0.5824936645240091915, -46.76557133587090931, -3.495642526042641141 ) ) ;
#49193 = VERTEX_POINT ( 'NONE', #43698 ) ;
#49194 = CARTESIAN_POINT ( 'NONE',  ( 5.880360259849739535, -31.66572319753537101, -36.03610316515372602 ) ) ;
#49195 = CARTESIAN_POINT ( 'NONE',  ( 0.1157991065609915715, 25.17735855925881694, 36.23593494745534116 ) ) ;
#49196 = EDGE_LOOP ( 'NONE', ( #56544, #45506, #48609, #45345 ) ) ;
#49197 = CARTESIAN_POINT ( 'NONE',  ( -2.601141883200662974, -0.9259886695526062805, -14.89758277215632098 ) ) ;
#49198 = CARTESIAN_POINT ( 'NONE',  ( 0.8753041380234530822, -14.82204010568715447, -46.81287702094778780 ) ) ;
#49199 = DIRECTION ( 'NONE',  ( -1.000000000000000000, -0.000000000000000000, -0.000000000000000000 ) ) ;
#49200 = CARTESIAN_POINT ( 'NONE',  ( -18.52475027399287200, -12.33207363406532941, -2.044797646294537419 ) ) ;
#49201 = ORIENTED_EDGE ( 'NONE', *, *, #28804, .T. ) ;
#49202 = CARTESIAN_POINT ( 'NONE',  ( 5.910764540655178756, 0.6875337509666024083, 20.10046108452352698 ) ) ;
#49203 = ADVANCED_FACE ( 'NONE', ( #745 ), #22520, .F. ) ;
#49204 = B_SPLINE_CURVE_WITH_KNOTS ( 'NONE', 3,
 ( #42581, #33492, #61950, #33805, #56339, #52567, #61642, #13450, #47581, #23766, #14382, #56957, #14079, #33181, #42899, #19089, #38199, #29082, #52881 ),
 .UNSPECIFIED., .F., .F.,
 ( 4, 3, 3, 3, 3, 3, 4 ),
 ( 6.938893903907228378E-18, 0.0002732106629380587999, 0.0004098138914053727757, 0.0005464171197651509181, 0.0006830203481512618375, 0.0008196235766963736076, 0.001011968216111140293 ),
 .UNSPECIFIED. ) ;
#49205 = CARTESIAN_POINT ( 'NONE',  ( 5.959547316686252039, 14.51128755440541340, -14.51632612601513728 ) ) ;
#49206 = CARTESIAN_POINT ( 'NONE',  ( 2.000000000000027089, 3.464101615137739731, -5.600000000000000533 ) ) ;
#49207 = ADVANCED_FACE ( 'NONE', ( #55752 ), #24517, .F. ) ;
#49208 = CARTESIAN_POINT ( 'NONE',  ( 0.8557997880470599172, 28.43566216844970640, 38.55640757422448672 ) ) ;
#49209 = CARTESIAN_POINT ( 'NONE',  ( 4.956445790443988919, 44.65954324082213134, 14.93530206124989945 ) ) ;
#49210 = EDGE_CURVE ( 'NONE', #45553, #11417, #52016, .T. ) ;
#49211 = CARTESIAN_POINT ( 'NONE',  ( -6.078726893082806448, 18.62537590944114640, 4.887679766589625885 ) ) ;
#49212 = CARTESIAN_POINT ( 'NONE',  ( 0.8557997880470606944, 38.55640757422477805, -28.43566216844931915 ) ) ;
#49213 = CARTESIAN_POINT ( 'NONE',  ( 4.967162193818130511, 0.000000000000000000, 0.000000000000000000 ) ) ;
#49214 = CARTESIAN_POINT ( 'NONE',  ( 0.7245667037590765025, 47.57651946688177702, -7.091191019330373102 ) ) ;
#49215 = CARTESIAN_POINT ( 'NONE',  ( -5.719999999999999751, 4.781475508499492452E-15, 0.000000000000000000 ) ) ;
#49216 = CARTESIAN_POINT ( 'NONE',  ( 4.694002226626921015, -9.808094470216756733, 44.52062504401121146 ) ) ;
#49217 = CARTESIAN_POINT ( 'NONE',  ( 4.960386119450149955, -37.88391031994039793, 21.89168343328246991 ) ) ;
#49218 = AXIS2_PLACEMENT_3D ( 'NONE', #55825, #3201, #3813 ) ;
#49219 = B_SPLINE_CURVE_WITH_KNOTS ( 'NONE', 3,
 ( #3826, #47377, #4733, #14191 ),
 .UNSPECIFIED., .F., .F.,
 ( 4, 4 ),
 ( 4.336808689942017255E-19, 0.004446298630425055479 ),
 .UNSPECIFIED. ) ;
#49220 = EDGE_CURVE ( 'NONE', #28915, #42953, #51234, .T. ) ;
#49221 = DIRECTION ( 'NONE',  ( 0.09722883295013598492, -0.2759265041300023591, -0.9562484605800682935 ) ) ;
#49222 = CARTESIAN_POINT ( 'NONE',  ( 5.896782393890504181, 20.06749419425502978, 1.349727247095894089 ) ) ;
#49223 = ORIENTED_EDGE ( 'NONE', *, *, #47192, .T. ) ;
#49224 = CARTESIAN_POINT ( 'NONE',  ( 2.879087469061463178, -3.139839183809346235, -43.88898593819631344 ) ) ;
#49225 = CARTESIAN_POINT ( 'NONE',  ( 1.834102595619085729, 19.20967481895078066, -39.63819040026742613 ) ) ;
#49226 = ORIENTED_EDGE ( 'NONE', *, *, #46191, .T. ) ;
#49227 = EDGE_CURVE ( 'NONE', #34790, #24212, #55006, .T. ) ;
#49228 = CARTESIAN_POINT ( 'NONE',  ( 0.9752132459055864455, 5.831562321021558581, 42.51031254975315221 ) ) ;
#49229 = DIRECTION ( 'NONE',  ( -1.000000000000000000, -0.000000000000000000, -0.000000000000000000 ) ) ;
#49230 = EDGE_CURVE ( 'NONE', #3214, #31693, #18183, .T. ) ;
#49231 = EDGE_LOOP ( 'NONE', ( #30371, #27655, #984, #9396 ) ) ;
#49232 = ORIENTED_EDGE ( 'NONE', *, *, #45647, .F. ) ;
#49233 =( BOUNDED_SURFACE ( )  B_SPLINE_SURFACE ( 3, 1, ( 
 ( #1397, #26458 ),
 ( #40906, #11144 ),
 ( #20844, #58717 ),
 ( #54322, #39983 ) ),
 .UNSPECIFIED., .F., .F., .F. ) 
 B_SPLINE_SURFACE_WITH_KNOTS ( ( 4, 4 ),
 ( 2, 2 ),
 ( 0.000000000000000000, 1.000000000000000000 ),
 ( 0.000000000000000000, 1.000000000000000000 ),
 .UNSPECIFIED. ) 
 GEOMETRIC_REPRESENTATION_ITEM ( )  RATIONAL_B_SPLINE_SURFACE ( (
 ( 1.000000000000000000, 1.000000000000000000),
 ( 0.7282232189291694135, 0.9929344683865672927),
 ( 0.7282232189291694135, 0.9929344683865672927),
 ( 1.000000000000000000, 1.000000000000000000) ) ) 
 REPRESENTATION_ITEM ( '' )  SURFACE ( )  );
#49234 = DIRECTION ( 'NONE',  ( -1.000000000000000000, 0.000000000000000000, 0.000000000000000000 ) ) ;
#49235 = EDGE_LOOP ( 'NONE', ( #16650, #2311, #15755, #23749 ) ) ;
#49236 = LINE ( 'NONE', #44570, #22978 ) ;
#49237 = VERTEX_POINT ( 'NONE', #7839 ) ;
#49238 = VERTEX_POINT ( 'NONE', #41696 ) ;
#49239 = CARTESIAN_POINT ( 'NONE',  ( -6.078075953587585900, 7.789670135765644154, 17.61011679186417922 ) ) ;
#49240 = ORIENTED_EDGE ( 'NONE', *, *, #50336, .T. ) ;
#49241 = FACE_OUTER_BOUND ( 'NONE', #66, .T. ) ;
#49242 = EDGE_CURVE ( 'NONE', #15459, #25014, #16883, .T. ) ;
#49243 = B_SPLINE_CURVE_WITH_KNOTS ( 'NONE', 3,
 ( #46902, #52179, #3626, #28380, #52488, #8970 ),
 .UNSPECIFIED., .F., .F.,
 ( 4, 2, 4 ),
 ( 9.660965348001700255E-18, 0.0002448709889506567772, 0.0004897419779013039050 ),
 .UNSPECIFIED. ) ;
#49244 = CARTESIAN_POINT ( 'NONE',  ( 0.6253024248130479856, 46.81662110580109726, -14.82053358194312764 ) ) ;
#49245 = ORIENTED_EDGE ( 'NONE', *, *, #37883, .T. ) ;
#49246 = LINE ( 'NONE', #49871, #50685 ) ;
#49247 = DIRECTION ( 'NONE',  ( 0.1024043820194936449, -0.7811075516170163935, 0.6159418278945469893 ) ) ;
#49248 = ORIENTED_EDGE ( 'NONE', *, *, #4711, .F. ) ;
#49249 = CARTESIAN_POINT ( 'NONE',  ( 0.6845945791218023269, 23.29905063694661749, 40.71315217630468908 ) ) ;
#49250 = CARTESIAN_POINT ( 'NONE',  ( 0.5807400328401574052, 33.48217046439159361, -34.25275203086199838 ) ) ;
#49251 = DIRECTION ( 'NONE',  ( 0.000000000000000000, 0.000000000000000000, 1.000000000000000000 ) ) ;
#49252 = ORIENTED_EDGE ( 'NONE', *, *, #52265, .F. ) ;
#49253 = VECTOR ( 'NONE', #7524, 1000.000000000000000 ) ;
#49254 = CARTESIAN_POINT ( 'NONE',  ( 0.8557997880470599172, -37.44587306708076824, -29.88293891557508530 ) ) ;
#49255 = VECTOR ( 'NONE', #41191, 999.9999999999998863 ) ;
#49256 = CARTESIAN_POINT ( 'NONE',  ( 2.643462169533613793, 42.27470921730908771, 22.81120928486510024 ) ) ;
#49257 = FACE_OUTER_BOUND ( 'NONE', #40197, .T. ) ;
#49258 = ORIENTED_EDGE ( 'NONE', *, *, #51566, .T. ) ;
#49259 = FACE_OUTER_BOUND ( 'NONE', #2715, .T. ) ;
#49260 = CARTESIAN_POINT ( 'NONE',  ( 0.8560838555295223751, 45.47430759461099115, 11.50913475776684791 ) ) ;
#49261 = CARTESIAN_POINT ( 'NONE',  ( 1.834102595619085729, 8.527011080115599384, -43.21444002757956326 ) ) ;
#49262 = CARTESIAN_POINT ( 'NONE',  ( 0.3676999524040366896, -6.224421213753956295, 43.67158302462379282 ) ) ;
#49263 = EDGE_CURVE ( 'NONE', #351, #47799, #22857, .T. ) ;
#49264 = ORIENTED_EDGE ( 'NONE', *, *, #33245, .F. ) ;
#49265 = ORIENTED_EDGE ( 'NONE', *, *, #6210, .T. ) ;
#49266 = CARTESIAN_POINT ( 'NONE',  ( 4.549368137175248350, 0.000000000000000000, 0.000000000000000000 ) ) ;
#49267 = CARTESIAN_POINT ( 'NONE',  ( 1.834102595619085507, 42.19596157538738623, 12.63719001938783926 ) ) ;
#49268 = EDGE_CURVE ( 'NONE', #45559, #31387, #4973, .T. ) ;
#49269 = CARTESIAN_POINT ( 'NONE',  ( 0.1087620492084205859, -39.97903073778078209, 16.16798550313352578 ) ) ;
#49271 = B_SPLINE_CURVE_WITH_KNOTS ( 'NONE', 3,
 ( #31037, #13800, #60755, #37608, #41692, #37294 ),
 .UNSPECIFIED., .F., .F.,
 ( 4, 2, 4 ),
 ( 1.209554233810030470E-16, 0.0002448718616795917953, 0.0004897437233590627020 ),
 .UNSPECIFIED. ) ;
#49270 = CARTESIAN_POINT ( 'NONE',  ( 2.528100132419516033, -18.76087228870760981, -37.55374082030813554 ) ) ;
#49272 = DIRECTION ( 'NONE',  ( -1.000000000000000000, -0.000000000000000000, -0.000000000000000000 ) ) ;
#49273 = EDGE_CURVE ( 'NONE', #9094, #20821, #34085, .T. ) ;
#49274 = B_SPLINE_CURVE_WITH_KNOTS ( 'NONE', 3,
 ( #34533, #30735, #44876, #54844 ),
 .UNSPECIFIED., .F., .F.,
 ( 4, 4 ),
 ( 0.000000000000000000, 0.004444103432399267896 ),
 .UNSPECIFIED. ) ;
#49275 = CARTESIAN_POINT ( 'NONE',  ( 4.956653778116995035, 36.51451553856460919, -31.29546495791814209 ) ) ;
#49276 = CARTESIAN_POINT ( 'NONE',  ( 3.559346040607745287, -14.46634168074828608, -41.52294835290280162 ) ) ;
#49277 = EDGE_CURVE ( 'NONE', #47251, #9480, #29611, .T. ) ;
#49278 = CARTESIAN_POINT ( 'NONE',  ( 0.9762797500689124330, 15.53330887509081215, 38.92352888134283262 ) ) ;
#49279 = CARTESIAN_POINT ( 'NONE',  ( 2.648799415243696664, 33.97949776740117755, -35.35408314133994168 ) ) ;
#49280 = CARTESIAN_POINT ( 'NONE',  ( 1.154321485836933725, -42.43366804742922938, 6.418927614505942181 ) ) ;
#49281 = CARTESIAN_POINT ( 'NONE',  ( 5.910764540655178756, -17.31247307865842089, -10.23618651500110666 ) ) ;
#49282 = CARTESIAN_POINT ( 'NONE',  ( 4.322998006666165516, 36.74401119231367119, 30.86725474310372519 ) ) ;
#49283 = FACE_OUTER_BOUND ( 'NONE', #54871, .T. ) ;
#49284 = CARTESIAN_POINT ( 'NONE',  ( 0.3676999524040323597, 33.04872056100222011, 29.21870381457103605 ) ) ;
#49285 = CARTESIAN_POINT ( 'NONE',  ( 0.6254311100348644015, -44.17670535157497369, -19.04346769887678192 ) ) ;
#49286 = CARTESIAN_POINT ( 'NONE',  ( 1.088908134280554663, 6.374115321933079059, 42.43751564162685241 ) ) ;
#49287 = B_SPLINE_CURVE_WITH_KNOTS ( 'NONE', 3,
 ( #25514, #58393, #1691, #25213 ),
 .UNSPECIFIED., .F., .F.,
 ( 4, 4 ),
 ( 0.000000000000000000, 0.005014147105413699519 ),
 .UNSPECIFIED. ) ;
#49288 = ADVANCED_FACE ( 'NONE', ( #4044 ), #49847, .T. ) ;
#49289 = CARTESIAN_POINT ( 'NONE',  ( 0.9756354156337454508, -11.23134828980305855, 41.41248945940461113 ) ) ;
#49290 = EDGE_CURVE ( 'NONE', #1527, #21489, #24105, .T. ) ;
#49291 = CARTESIAN_POINT ( 'NONE',  ( -1.139999999999998570, 0.000000000000000000, 0.000000000000000000 ) ) ;
#49292 = CARTESIAN_POINT ( 'NONE',  ( 0.5997462898726536595, 49.03735788587803768, -2.624721264558313560 ) ) ;
#49294 = ORIENTED_EDGE ( 'NONE', *, *, #60368, .F. ) ;
#49293 = DIRECTION ( 'NONE',  ( 0.09722883295013594329, -0.6264263058867762801, -0.7733929385093980535 ) ) ;
#49295 = ORIENTED_EDGE ( 'NONE', *, *, #26670, .T. ) ;
#49296 = CARTESIAN_POINT ( 'NONE',  ( 0.1073791018717483448, -33.91564619577824402, 26.63563652260111070 ) ) ;
#49297 = CARTESIAN_POINT ( 'NONE',  ( 0.7242003506639999033, 49.04682596084168011, 2.328204736043216538 ) ) ;
#49298 = CARTESIAN_POINT ( 'NONE',  ( 0.1156867017252034557, 41.83675885982486875, 14.02242544569421234 ) ) ;
#49299 = ORIENTED_EDGE ( 'NONE', *, *, #40512, .F. ) ;
#49300 = ORIENTED_EDGE ( 'NONE', *, *, #23690, .T. ) ;
#49301 = CARTESIAN_POINT ( 'NONE',  ( 0.5809828226811617480, 44.03860873105695362, 18.83114015454715684 ) ) ;
#49302 = DIRECTION ( 'NONE',  ( 0.000000000000000000, 0.000000000000000000, 1.000000000000000000 ) ) ;
#49303 = CARTESIAN_POINT ( 'NONE',  ( 0.1084644655670281704, -37.14658555883747937, 21.90577137312928002 ) ) ;
#49304 = B_SPLINE_CURVE_WITH_KNOTS ( 'NONE', 3,
 ( #24349, #47860, #38466, #9950, #61610, #13417 ),
 .UNSPECIFIED., .F., .F.,
 ( 4, 2, 4 ),
 ( 9.590134410337311873E-18, 0.0002291978881530175153, 0.0004583957763060254355 ),
 .UNSPECIFIED. ) ;
#49305 = AXIS2_PLACEMENT_3D ( 'NONE', #34970, #25239, #7031 ) ;
#49306 =( BOUNDED_SURFACE ( )  B_SPLINE_SURFACE ( 3, 1, ( 
 ( #28025, #47145 ),
 ( #18018, #23327 ),
 ( #51499, #7654 ),
 ( #26785, #34273 ) ),
 .UNSPECIFIED., .F., .F., .F. ) 
 B_SPLINE_SURFACE_WITH_KNOTS ( ( 4, 4 ),
 ( 2, 2 ),
 ( 0.000000000000000000, 1.000000000000000000 ),
 ( 0.000000000000000000, 1.000000000000000000 ),
 .UNSPECIFIED. ) 
 GEOMETRIC_REPRESENTATION_ITEM ( )  RATIONAL_B_SPLINE_SURFACE ( (
 ( 1.000000000000000000, 1.000000000000000000),
 ( 0.9732289882329797637, 0.9999525324661233672),
 ( 0.9732289882329797637, 0.9999525324661233672),
 ( 1.000000000000000000, 1.000000000000000000) ) ) 
 REPRESENTATION_ITEM ( '' )  SURFACE ( )  );
#49307 = ORIENTED_EDGE ( 'NONE', *, *, #29289, .F. ) ;
#49308 = ORIENTED_EDGE ( 'NONE', *, *, #2451, .F. ) ;
#49309 = CARTESIAN_POINT ( 'NONE',  ( 4.962356264823608143, 0.000000000000000000, 0.000000000000000000 ) ) ;
#49310 = CARTESIAN_POINT ( 'NONE',  ( 0.1129192098497455998, 33.91039995638899995, -28.23183597612607798 ) ) ;
#49311 = CARTESIAN_POINT ( 'NONE',  ( 0.5824936645240099686, -38.45573382456261413, -26.84016980301536393 ) ) ;
#49312 = CARTESIAN_POINT ( 'NONE',  ( 0.5806925824938502512, 16.34374012233117313, -43.95571090492413191 ) ) ;
#49313 = B_SPLINE_CURVE_WITH_KNOTS ( 'NONE', 3,
 ( #10279, #54085, #5241, #34401, #24373, #29372 ),
 .UNSPECIFIED., .F., .F.,
 ( 4, 2, 4 ),
 ( 0.000000000000000000, 0.0002447195606305749629, 0.0004894391212611499259 ),
 .UNSPECIFIED. ) ;
#49314 = CARTESIAN_POINT ( 'NONE',  ( 3.660087539127321321, 14.24113226412049293, 45.87884541725750154 ) ) ;
#49315 = ADVANCED_FACE ( 'NONE', ( #9379 ), #7301, .F. ) ;
#49316 = LINE ( 'NONE', #6370, #45620 ) ;
#49317 = ADVANCED_FACE ( 'NONE', ( #589 ), #30932, .F. ) ;
#49318 = CARTESIAN_POINT ( 'NONE',  ( 4.549368137175248350, 38.59302160394752690, -18.79584381673492288 ) ) ;
#49319 = ORIENTED_EDGE ( 'NONE', *, *, #48210, .F. ) ;
#49320 = ORIENTED_EDGE ( 'NONE', *, *, #19699, .F. ) ;
#49321 = CARTESIAN_POINT ( 'NONE',  ( 4.975801465491695552, 42.71626295676264817, -21.70134120755155394 ) ) ;
#49322 = DIRECTION ( 'NONE',  ( -1.000000000000000000, -0.000000000000000000, -0.000000000000000000 ) ) ;
#49323 = ORIENTED_EDGE ( 'NONE', *, *, #41395, .T. ) ;
#49324 = CARTESIAN_POINT ( 'NONE',  ( -2.708315649062916552, -8.698422600177206476, 11.76894112707797646 ) ) ;
#49325 = FACE_OUTER_BOUND ( 'NONE', #43054, .T. ) ;
#49326 = CARTESIAN_POINT ( 'NONE',  ( 0.6023142530420679819, 46.53533807097414154, 12.19802990522816977 ) ) ;
#49327 = CARTESIAN_POINT ( 'NONE',  ( 0.5809828226811565299, -17.82437196699712700, 44.45562576850595349 ) ) ;
#49328 = B_SPLINE_CURVE_WITH_KNOTS ( 'NONE', 3,
 ( #6555, #7818, #1879, #25699 ),
 .UNSPECIFIED., .F., .F.,
 ( 4, 4 ),
 ( 1.301042606982605321E-18, 0.004048833967417083887 ),
 .UNSPECIFIED. ) ;
#49329 = VERTEX_POINT ( 'NONE', #14720 ) ;
#49330 = CARTESIAN_POINT ( 'NONE',  ( 0.1064266418746776799, 5.071708474752668394, 42.82540703015434502 ) ) ;
#49331 = CARTESIAN_POINT ( 'NONE',  ( 0.6021447746440204973, -35.09404424325450833, 34.35038861120762732 ) ) ;
#49332 = FACE_OUTER_BOUND ( 'NONE', #13278, .T. ) ;
#49333 = CARTESIAN_POINT ( 'NONE',  ( -2.601141883200662974, -14.54530301301453932, -3.351057703021369960 ) ) ;
#49334 = B_SPLINE_CURVE_WITH_KNOTS ( 'NONE', 3,
 ( #12330, #41457, #55829, #12951, #59601, #35519 ),
 .UNSPECIFIED., .F., .F.,
 ( 4, 2, 4 ),
 ( 1.843143693225357538E-18, 0.0002447193893791695996, 0.0004894387787583373561 ),
 .UNSPECIFIED. ) ;
#49335 = VERTEX_POINT ( 'NONE', #48230 ) ;
#49336 = CARTESIAN_POINT ( 'NONE',  ( 0.6067375320500709712, -46.44340905096873939, 11.71046088714736122 ) ) ;
#49337 = CARTESIAN_POINT ( 'NONE',  ( 0.5988103564986355654, -47.77151399983773672, -5.677495323490556522 ) ) ;
#49338 = ORIENTED_EDGE ( 'NONE', *, *, #19005, .T. ) ;
#49339 = CARTESIAN_POINT ( 'NONE',  ( -5.272380000000000067, 0.000000000000000000, 0.000000000000000000 ) ) ;
#49340 = CARTESIAN_POINT ( 'NONE',  ( 0.1156495703730067298, 9.951406056163939695, 42.98735245088273160 ) ) ;
#49341 = B_SPLINE_CURVE_WITH_KNOTS ( 'NONE', 3,
 ( #57202, #47227, #33753, #4896, #42849, #32511, #28409, #19043, #4273, #3971, #42537, #23722, #56909, #18101, #28727, #61295 ),
 .UNSPECIFIED., .F., .F.,
 ( 4, 3, 3, 3, 3, 4 ),
 ( 1.095097866269904594E-17, 0.0002724568934985562517, 0.0004086836638483807432, 0.0005449104342063607661, 0.0008173270854453682996, 0.001089761613562689659 ),
 .UNSPECIFIED. ) ;
#49342 = ORIENTED_EDGE ( 'NONE', *, *, #2670, .T. ) ;
#49343 = DIRECTION ( 'NONE',  ( 1.850371707708593823E-16, -1.000000000000000000, 0.000000000000000000 ) ) ;
#49344 = CARTESIAN_POINT ( 'NONE',  ( 0.6023142530420679819, -47.66103033449103066, 6.538792732869052493 ) ) ;
#49345 = EDGE_CURVE ( 'NONE', #14400, #13993, #15424, .T. ) ;
#49346 = CARTESIAN_POINT ( 'NONE',  ( 3.238018933889920792, -13.37994740236393376, -0.6200805412425434149 ) ) ;
#49347 = VECTOR ( 'NONE', #15251, 1000.000000000000000 ) ;
#49348 = ADVANCED_FACE ( 'NONE', ( #57584 ), #33330, .F. ) ;
#49349 = CARTESIAN_POINT ( 'NONE',  ( -6.077587904424778920, -19.21610359950803115, -1.239912838430589970 ) ) ;
#49350 = CARTESIAN_POINT ( 'NONE',  ( 0.3676999524040323597, -35.84016207189440451, 25.71834687500696859 ) ) ;
#49351 = CARTESIAN_POINT ( 'NONE',  ( 3.680882792899937694, -1.849662971457888272, -47.94008871805917948 ) ) ;
#49352 = CARTESIAN_POINT ( 'NONE',  ( -6.001507490154110336, -2.444174634178271521, 18.68469198366096151 ) ) ;
#49353 = CARTESIAN_POINT ( 'NONE',  ( 1.000433927950262314, 29.60512436931191260, 29.66404033051502154 ) ) ;
#49354 = DIRECTION ( 'NONE',  ( 0.000000000000000000, 1.000000000000000000, 0.000000000000000000 ) ) ;
#49355 = ADVANCED_FACE ( 'NONE', ( #271 ), #30641, .T. ) ;
#49356 = CARTESIAN_POINT ( 'NONE',  ( 0.5998501479064708430, -17.92509395669076966, -44.64337787626241294 ) ) ;
#49357 = EDGE_CURVE ( 'NONE', #20018, #49695, #25960, .T. ) ;
#49358 = CARTESIAN_POINT ( 'NONE',  ( 4.967162193818130511, 0.000000000000000000, 0.000000000000000000 ) ) ;
#49359 = VERTEX_POINT ( 'NONE', #20340 ) ;
#49360 = EDGE_CURVE ( 'NONE', #51862, #29310, #8631, .T. ) ;
#49361 = CARTESIAN_POINT ( 'NONE',  ( -16.92102945109384393, -12.36669815058221289, 1.822278859258224193 ) ) ;
#49362 = CARTESIAN_POINT ( 'NONE',  ( 0.5997462898726536595, -13.47075269803155351, 47.22383351542719510 ) ) ;
#49363 = CARTESIAN_POINT ( 'NONE',  ( 0.6027444965799114707, 22.59817970401703846, 43.59886225525149683 ) ) ;
#49364 = CARTESIAN_POINT ( 'NONE',  ( 0.1152809850208375841, 44.04716389649329500, -2.606268436906177488 ) ) ;
#49365 = VECTOR ( 'NONE', #20602, 1000.000000000000000 ) ;
#49366 = DIRECTION ( 'NONE',  ( 0.000000000000000000, 1.000000000000000000, 0.000000000000000000 ) ) ;
#49367 = CYLINDRICAL_SURFACE ( 'NONE', #44644, 12.50000000000000000 ) ;
#49368 = DIRECTION ( 'NONE',  ( -1.000000000000000000, -5.251280333798721377E-15, 4.807811143603695798E-15 ) ) ;
#49369 = CARTESIAN_POINT ( 'NONE',  ( 2.618530812446115519, 29.00550538245366283, 36.99199165639301867 ) ) ;
#49370 = EDGE_CURVE ( 'NONE', #32229, #29392, #3418, .T. ) ;
#49371 = CARTESIAN_POINT ( 'NONE',  ( 4.967162193818130511, 0.000000000000000000, 0.000000000000000000 ) ) ;
#49372 = CARTESIAN_POINT ( 'NONE',  ( 0.6030672459662951290, 0.08726629989075269933, -48.10738700891300823 ) ) ;
#49374 = ORIENTED_EDGE ( 'NONE', *, *, #7690, .F. ) ;
#49373 = CARTESIAN_POINT ( 'NONE',  ( 0.3622758884714730732, -37.74294673546571488, -20.83792692158958815 ) ) ;
#49375 = ORIENTED_EDGE ( 'NONE', *, *, #35528, .F. ) ;
#49376 = DIRECTION ( 'NONE',  ( -1.000000000000000000, 0.000000000000000000, -0.000000000000000000 ) ) ;
#49377 = CARTESIAN_POINT ( 'NONE',  ( -16.98648177666931858, 7.159091074317976755, -1.550344604434408250E-15 ) ) ;
#49378 = CARTESIAN_POINT ( 'NONE',  ( 0.2285344041767065348, -42.86264843728616825, -10.45440286372519623 ) ) ;
#49379 = CARTESIAN_POINT ( 'NONE',  ( 1.227938101723756947, 17.20315230597844192, 39.32113113558972373 ) ) ;
#49380 = CARTESIAN_POINT ( 'NONE',  ( 1.227938101723756947, -42.43379953535190197, 6.439911493064418124 ) ) ;
#49381 = LINE ( 'NONE', #40328, #55061 ) ;
#49382 = VERTEX_POINT ( 'NONE', #49448 ) ;
#49383 = VERTEX_POINT ( 'NONE', #35068 ) ;
#49384 = DIRECTION ( 'NONE',  ( 0.000000000000000000, 0.000000000000000000, 1.000000000000000000 ) ) ;
#49385 =( BOUNDED_SURFACE ( )  B_SPLINE_SURFACE ( 3, 1, ( 
 ( #2850, #21983 ),
 ( #46114, #22288 ),
 ( #60473, #55470 ),
 ( #60783, #12595 ) ),
 .UNSPECIFIED., .F., .F., .F. ) 
 B_SPLINE_SURFACE_WITH_KNOTS ( ( 4, 4 ),
 ( 2, 2 ),
 ( 0.000000000000000000, 1.000000000000000000 ),
 ( 0.000000000000000000, 1.000000000000000000 ),
 .UNSPECIFIED. ) 
 GEOMETRIC_REPRESENTATION_ITEM ( )  RATIONAL_B_SPLINE_SURFACE ( (
 ( 1.000000000000000000, 1.000000000000000000),
 ( 0.9952954269826590483, 0.8620686068821339365),
 ( 0.9952954269826590483, 0.8620686068821339365),
 ( 1.000000000000000000, 1.000000000000000000) ) ) 
 REPRESENTATION_ITEM ( '' )  SURFACE ( )  );
#49386 = CARTESIAN_POINT ( 'NONE',  ( 0.1103744047535531458, -11.12399292196407963, -41.66501489234560296 ) ) ;
#49387 = CARTESIAN_POINT ( 'NONE',  ( 1.231276596079881047, 15.85305549123227564, -38.80666698661426040 ) ) ;
#49388 = EDGE_LOOP ( 'NONE', ( #51540, #15073 ) ) ;
#49389 = B_SPLINE_CURVE_WITH_KNOTS ( 'NONE', 3,
 ( #29810, #48921, #34841, #44256 ),
 .UNSPECIFIED., .F., .F.,
 ( 4, 4 ),
 ( 1.084202172485504434E-18, 0.004048833967417086489 ),
 .UNSPECIFIED. ) ;
#49390 = VECTOR ( 'NONE', #24483, 1000.000000000000114 ) ;
#49391 = CARTESIAN_POINT ( 'NONE',  ( 0.7044674535452954967, -26.17468433047410770, 41.55344297421019206 ) ) ;
#49392 = CARTESIAN_POINT ( 'NONE',  ( 4.963659409799326738, 43.98510776953422408, -8.262218268420037148 ) ) ;
#49393 = EDGE_LOOP ( 'NONE', ( #32559, #8854, #5338, #29997 ) ) ;
#49394 = EDGE_CURVE ( 'NONE', #38461, #14894, #16252, .T. ) ;
#49395 = CARTESIAN_POINT ( 'NONE',  ( 0.9754402186311955658, 41.39745964575708825, -11.28658745892475324 ) ) ;
#49396 = ORIENTED_EDGE ( 'NONE', *, *, #26903, .T. ) ;
#49397 = CARTESIAN_POINT ( 'NONE',  ( 5.981074661064941900, -5.303881226583540887, -19.82752479807525958 ) ) ;
#49398 = CARTESIAN_POINT ( 'NONE',  ( 0.5806925824938499181, -46.82446035038572063, 2.586943222941027631 ) ) ;
#49399 = EDGE_LOOP ( 'NONE', ( #21362, #17444, #51452, #33377 ) ) ;
#49400 = CARTESIAN_POINT ( 'NONE',  ( 3.238018933889920792, -1.956241471238032492, 13.25068344176485802 ) ) ;
#49401 = CARTESIAN_POINT ( 'NONE',  ( 5.960721111146673579, 12.50019045452738276, -16.28018152803680252 ) ) ;
#49402 = CARTESIAN_POINT ( 'NONE',  ( 0.5839879327111927587, 41.43370681949809864, -24.02664985973661871 ) ) ;
#49403 = LINE ( 'NONE', #29074, #22360 ) ;
#49404 = VECTOR ( 'NONE', #55717, 1000.000000000000000 ) ;
#49405 = ORIENTED_EDGE ( 'NONE', *, *, #1401, .T. ) ;
#49406 = B_SPLINE_CURVE_WITH_KNOTS ( 'NONE', 3,
 ( #4764, #52706, #5992, #16357, #6931, #35483, #45204, #39887, #15439, #25754 ),
 .UNSPECIFIED., .F., .F.,
 ( 4, 3, 3, 4 ),
 ( 1.157434093048479169E-16, 0.0002618519381806256457, 0.0003927759815485974389, 0.0004849530346204834448 ),
 .UNSPECIFIED. ) ;
#49407 = CARTESIAN_POINT ( 'NONE',  ( 5.901463166500145796, 14.90686821212704061, 13.50196839156843076 ) ) ;
#49408 = CARTESIAN_POINT ( 'NONE',  ( 5.272380000000000067, 0.000000000000000000, 0.000000000000000000 ) ) ;
#49409 = ORIENTED_EDGE ( 'NONE', *, *, #44360, .T. ) ;
#49410 = CARTESIAN_POINT ( 'NONE',  ( 4.975801465491694664, 47.76942479135480824, 3.702618843597622167 ) ) ;
#49411 = ORIENTED_EDGE ( 'NONE', *, *, #48182, .F. ) ;
#49412 = CARTESIAN_POINT ( 'NONE',  ( 0.6846871229502932144, 34.48177377577881941, -33.25969555998707250 ) ) ;
#49413 = ORIENTED_EDGE ( 'NONE', *, *, #30276, .T. ) ;
#49414 = LINE ( 'NONE', #16851, #19679 ) ;
#49415 = CARTESIAN_POINT ( 'NONE',  ( 0.9780106845699481077, 36.21705500758324803, -21.08687205426938505 ) ) ;
#49416 = ORIENTED_EDGE ( 'NONE', *, *, #42294, .T. ) ;
#49417 = CARTESIAN_POINT ( 'NONE',  ( 0.1147471544378677460, 43.36887420253955128, 8.129756384882995235 ) ) ;
#49418 = CARTESIAN_POINT ( 'NONE',  ( -6.010958268070873523, 17.40352239307057403, 7.224487401384361185 ) ) ;
#49419 = CARTESIAN_POINT ( 'NONE',  ( 4.553261556744873317, 40.63093864075514006, -16.69330377710856084 ) ) ;
#49420 = VERTEX_POINT ( 'NONE', #15953 ) ;
#49421 = EDGE_CURVE ( 'NONE', #12972, #4753, #23826, .T. ) ;
#49422 = ORIENTED_EDGE ( 'NONE', *, *, #12674, .T. ) ;
#49423 = CARTESIAN_POINT ( 'NONE',  ( 0.9783242366443549720, -30.90115862380460499, -28.30994323401212398 ) ) ;
#49424 = CARTESIAN_POINT ( 'NONE',  ( -6.072942160501519027, -18.90394509709863513, 3.666745430882924150 ) ) ;
#49425 = CARTESIAN_POINT ( 'NONE',  ( 0.6000166863083090663, 48.10206967781414278, -9.900220927795849946 ) ) ;
#49426 = CARTESIAN_POINT ( 'NONE',  ( 0.9972139404380304661, -0.6581143129157298599, -42.90441115546389739 ) ) ;
#49427 = CARTESIAN_POINT ( 'NONE',  ( 4.975801465491694664, -14.85979367497141546, -45.55012473237748338 ) ) ;
#49428 = CARTESIAN_POINT ( 'NONE',  ( -6.078726893082806448, -16.14009859332552921, 10.50196451462540992 ) ) ;
#49429 = ORIENTED_EDGE ( 'NONE', *, *, #3675, .T. ) ;
#49430 = EDGE_CURVE ( 'NONE', #3915, #23687, #43069, .T. ) ;
#49431 = CARTESIAN_POINT ( 'NONE',  ( 4.956653778116970166, 39.67974989265038488, 27.17045123668485829 ) ) ;
#49432 = EDGE_CURVE ( 'NONE', #1848, #44276, #12432, .T. ) ;
#49433 = CARTESIAN_POINT ( 'NONE',  ( 4.975610109902397937, 42.33317580307119954, 24.50207406657730047 ) ) ;
#49434 = VERTEX_POINT ( 'NONE', #10632 ) ;
#49435 = ADVANCED_FACE ( 'NONE', ( #29721 ), #28912, .F. ) ;
#49436 = CARTESIAN_POINT ( 'NONE',  ( -6.016489644550736315, 11.47450955518487525, 14.94663725562919865 ) ) ;
#49437 = CARTESIAN_POINT ( 'NONE',  ( -4.000000000000000000, 0.000000000000000000, -5.599999999999999645 ) ) ;
#49438 = CARTESIAN_POINT ( 'NONE',  ( 4.962356264823603702, -20.60668162140254722, -36.69605251817282010 ) ) ;
#49439 = VECTOR ( 'NONE', #2599, 1000.000000000000000 ) ;
#49440 = CARTESIAN_POINT ( 'NONE',  ( -6.063463321072278589, -4.269814012169691253, -18.77735712982391902 ) ) ;
#49441 = CARTESIAN_POINT ( 'NONE',  ( 0.5549461598389365813, 10.66800373468012175, 42.79499260174787878 ) ) ;
#49442 = FILL_AREA_STYLE ('',( #35372 ) ) ;
#49443 =( NAMED_UNIT ( * ) SI_UNIT ( $, .STERADIAN. ) SOLID_ANGLE_UNIT ( ) );
#49444 = FACE_OUTER_BOUND ( 'NONE', #53203, .T. ) ;
#49445 = CARTESIAN_POINT ( 'NONE',  ( 5.901463166500146684, 8.479222689261950663, 18.23789058324843637 ) ) ;
#49446 = CIRCLE ( 'NONE', #30427, 12.50000000000000000 ) ;
#49447 = CARTESIAN_POINT ( 'NONE',  ( 0.5997462898726536595, -47.63132954987539591, 11.95023328037892441 ) ) ;
#49449 = EDGE_CURVE ( 'NONE', #7001, #61, #21261, .T. ) ;
#49448 = CARTESIAN_POINT ( 'NONE',  ( 0.5809828226811617480, 12.92184523170268839, -46.11980934799325382 ) ) ;
#49450 = CARTESIAN_POINT ( 'NONE',  ( 2.643462169533600914, 38.93558293168539564, -28.13401304854679807 ) ) ;
#49451 = CARTESIAN_POINT ( 'NONE',  ( 0.9772918015221168098, 10.11840252319961664, 40.66884294062455751 ) ) ;
#49452 = EDGE_CURVE ( 'NONE', #30700, #36409, #46880, .T. ) ;
#49453 = CARTESIAN_POINT ( 'NONE',  ( 1.296416391601052265, -18.84992721815818228, -39.83701316547587368 ) ) ;
#49454 = CIRCLE ( 'NONE', #22449, 48.09070567114147110 ) ;
#49455 = CARTESIAN_POINT ( 'NONE',  ( 4.962356264823608143, 12.88441948660223169, -40.06528837230067097 ) ) ;
#49456 = CARTESIAN_POINT ( 'NONE',  ( 2.299746137290199055, -9.094862155372984702, -48.18261948110441750 ) ) ;
#49457 = ORIENTED_EDGE ( 'NONE', *, *, #38991, .T. ) ;
#49458 = CARTESIAN_POINT ( 'NONE',  ( 0.1073791018717578927, -33.91564619577789585, -26.63563652260155123 ) ) ;
#49459 = B_SPLINE_CURVE_WITH_KNOTS ( 'NONE', 3,
 ( #53639, #40230, #11701, #30162, #15465, #6024, #48975, #49900, #25158, #24864, #59280, #1644, #10772, #44304, #1959, #25463, #58977, #1333, #5714 ),
 .UNSPECIFIED., .F., .F.,
 ( 4, 3, 3, 3, 3, 3, 4 ),
 ( 1.165802754517233128E-16, 0.0002618519381806232063, 0.0003927759815485978184, 0.0005237000248299410448, 0.0006546240681324946810, 0.0007855481115631255534, 0.0009699050456655074724 ),
 .UNSPECIFIED. ) ;
#49460 = CARTESIAN_POINT ( 'NONE',  ( 0.1100247026804066219, 43.12411436000287779, 0.1696715072118848977 ) ) ;
#49461 = CARTESIAN_POINT ( 'NONE',  ( 0.9758171775293913441, -26.12572690811892784, -34.03798695362338123 ) ) ;
#49462 = CARTESIAN_POINT ( 'NONE',  ( 2.299746137290199943, -21.01915573909004920, -44.29984683610109641 ) ) ;
#49463 = CARTESIAN_POINT ( 'NONE',  ( 0.1097557419366048670, -41.59672960874321035, 11.37678103520264195 ) ) ;
#49464 = EDGE_LOOP ( 'NONE', ( #60241, #43878, #22314, #21607 ) ) ;
#49465 = CARTESIAN_POINT ( 'NONE',  ( 0.8551540677456834771, -47.90804413217341562, 0.9122407826474088210 ) ) ;
#49466 = CARTESIAN_POINT ( 'NONE',  ( 0.9752132459055856684, 16.20487516112007498, -39.73079175141334218 ) ) ;
#49467 = CARTESIAN_POINT ( 'NONE',  ( 0.1129192098497455998, 43.21532672376827833, 8.909956450124401073 ) ) ;
#49468 = ORIENTED_EDGE ( 'NONE', *, *, #19382, .F. ) ;
#49469 = CARTESIAN_POINT ( 'NONE',  ( 4.226256110419178924, -43.87543286663103004, 2.402840143026613973 ) ) ;
#49470 = VECTOR ( 'NONE', #40859, 1000.000000000000114 ) ;
#49471 = EDGE_CURVE ( 'NONE', #46958, #2310, #15649, .T. ) ;
#49472 = ORIENTED_EDGE ( 'NONE', *, *, #47014, .F. ) ;
#49473 = FACE_OUTER_BOUND ( 'NONE', #14217, .T. ) ;
#49474 = ORIENTED_EDGE ( 'NONE', *, *, #46403, .F. ) ;
#49475 = CARTESIAN_POINT ( 'NONE',  ( 3.238018933889920792, 11.66219248059504743, -6.587925235854247497 ) ) ;
#49476 = EDGE_LOOP ( 'NONE', ( #40961, #13430, #34407, #32305 ) ) ;
#49477 = CARTESIAN_POINT ( 'NONE',  ( 0.9747592971366232373, 21.73404615330619905, 36.99691261380215934 ) ) ;
#49478 = CARTESIAN_POINT ( 'NONE',  ( 3.270143674763207553, 9.870732238228521638, 9.482922169188000794 ) ) ;
#49479 = VERTEX_POINT ( 'NONE', #30033 ) ;
#49480 = ORIENTED_EDGE ( 'NONE', *, *, #58497, .T. ) ;
#49481 = CARTESIAN_POINT ( 'NONE',  ( 4.967162193818131399, -14.26841313271251543, -40.65506779172179108 ) ) ;
#49482 =( BOUNDED_SURFACE ( )  B_SPLINE_SURFACE ( 3, 1, ( 
 ( #27796, #22479 ),
 ( #60988, #26872 ),
 ( #56288, #17175 ),
 ( #17475, #46012 ) ),
 .UNSPECIFIED., .F., .F., .F. ) 
 B_SPLINE_SURFACE_WITH_KNOTS ( ( 4, 4 ),
 ( 2, 2 ),
 ( 0.000000000000000000, 1.000000000000000000 ),
 ( 0.000000000000000000, 1.000000000000000000 ),
 .UNSPECIFIED. ) 
 GEOMETRIC_REPRESENTATION_ITEM ( )  RATIONAL_B_SPLINE_SURFACE ( (
 ( 1.000000000000000000, 1.000000000000000000),
 ( 0.7211978278499968642, 0.9934217856018975334),
 ( 0.7211978278499968642, 0.9934217856018975334),
 ( 1.000000000000000000, 1.000000000000000000) ) ) 
 REPRESENTATION_ITEM ( '' )  SURFACE ( )  );
#49483 = CARTESIAN_POINT ( 'NONE',  ( 0.9730545539215883499, 21.89037132892487847, -36.90443313492307453 ) ) ;
#49484 = VECTOR ( 'NONE', #61886, 1000.000000000000000 ) ;
#49485 = ORIENTED_EDGE ( 'NONE', *, *, #33721, .F. ) ;
#49486 = ORIENTED_EDGE ( 'NONE', *, *, #7018, .F. ) ;
#49487 = FACE_OUTER_BOUND ( 'NONE', #10052, .T. ) ;
#49488 = CARTESIAN_POINT ( 'NONE',  ( 0.5836750258453349272, 33.99574025613956252, -33.73891062492366899 ) ) ;
#49489 = CIRCLE ( 'NONE', #22494, 48.09070567114147110 ) ;
#49490 = CARTESIAN_POINT ( 'NONE',  ( 0.6031356755773454870, 24.05374386753658555, 41.66225520948412253 ) ) ;
#49491 = CARTESIAN_POINT ( 'NONE',  ( 0.5807400328401637335, 17.82553128098407669, 44.45848844984449499 ) ) ;
#49492 = EDGE_LOOP ( 'NONE', ( #28652, #5549, #19000, #20690 ) ) ;
#49493 = DIRECTION ( 'NONE',  ( -1.000000000000000000, -0.000000000000000000, -0.000000000000000000 ) ) ;
#49494 = CARTESIAN_POINT ( 'NONE',  ( 5.901764892641307547, -41.06410928599490262, 26.67827573115522810 ) ) ;
#49495 = VECTOR ( 'NONE', #9919, 999.9999999999998863 ) ;
#49496 = ORIENTED_EDGE ( 'NONE', *, *, #21868, .F. ) ;
#49497 = CARTESIAN_POINT ( 'NONE',  ( 0.5809828226811553087, 47.41188724015889022, -6.791453954329836229 ) ) ;
#49498 = B_SPLINE_CURVE_WITH_KNOTS ( 'NONE', 3,
 ( #58387, #39030, #20215, #58085, #6681, #54301, #10814, #34619, #15205, #30207, #53389, #15511, #44961, #24596, #49017, #39640, #48704, #6067, #781 ),
 .UNSPECIFIED., .F., .F.,
 ( 4, 3, 3, 3, 3, 3, 4 ),
 ( 5.204170427930421283E-18, 0.0002732106629380602093, 0.0004098138914053775462, 0.0005464171197651487497, 0.0006830203481512609701, 0.0008196235766963675361, 0.001011968216111146148 ),
 .UNSPECIFIED. ) ;
#49499 = ORIENTED_EDGE ( 'NONE', *, *, #38356, .F. ) ;
#49500 =( BOUNDED_SURFACE ( )  B_SPLINE_SURFACE ( 3, 1, ( 
 ( #33381, #37788 ),
 ( #56843, #13343 ),
 ( #32444, #52452 ),
 ( #14581, #28658 ) ),
 .UNSPECIFIED., .F., .F., .F. ) 
 B_SPLINE_SURFACE_WITH_KNOTS ( ( 4, 4 ),
 ( 2, 2 ),
 ( 0.000000000000000000, 1.000000000000000000 ),
 ( 0.000000000000000000, 1.000000000000000000 ),
 .UNSPECIFIED. ) 
 GEOMETRIC_REPRESENTATION_ITEM ( )  RATIONAL_B_SPLINE_SURFACE ( (
 ( 1.000000000000000000, 1.000000000000000000),
 ( 0.7269869731126817891, 0.9931720237060910339),
 ( 0.7269869731126817891, 0.9931720237060910339),
 ( 1.000000000000000000, 1.000000000000000000) ) ) 
 REPRESENTATION_ITEM ( '' )  SURFACE ( )  );
#49501 = LINE ( 'NONE', #16302, #55511 ) ;
#49502 = CARTESIAN_POINT ( 'NONE',  ( -2.601141883200665639, -7.351091256667533713, -12.99064605035233733 ) ) ;
#49503 = ORIENTED_EDGE ( 'NONE', *, *, #13901, .T. ) ;
#49504 = DIRECTION ( 'NONE',  ( 0.000000000000000000, 0.000000000000000000, 1.000000000000000000 ) ) ;
#49505 = FACE_OUTER_BOUND ( 'NONE', #29069, .T. ) ;
#49506 = CARTESIAN_POINT ( 'NONE',  ( 50.67322615039200429, 12.21587082446438011, 2.649999999999992362 ) ) ;
#49507 = CARTESIAN_POINT ( 'NONE',  ( -19.64448124547968888, -12.43486301536525751, 1.279587518867056239 ) ) ;
#49508 = EDGE_CURVE ( 'NONE', #31400, #32172, #28838, .T. ) ;
#49509 = EDGE_LOOP ( 'NONE', ( #5741, #672, #3630, #23389, #5611, #16984 ) ) ;
#49510 = CARTESIAN_POINT ( 'NONE',  ( 4.956445790444036881, 42.27038699792232279, -20.75457619864872783 ) ) ;
#49511 = VERTEX_POINT ( 'NONE', #34141 ) ;
#49512 = EDGE_CURVE ( 'NONE', #15656, #5500, #44514, .T. ) ;
#49513 = FACE_OUTER_BOUND ( 'NONE', #40029, .T. ) ;
#49514 = DIRECTION ( 'NONE',  ( 0.09835009131224552170, 0.3879606369183508097, 0.9164135549743797071 ) ) ;
#49515 = FACE_OUTER_BOUND ( 'NONE', #20300, .T. ) ;
#49516 = VECTOR ( 'NONE', #31198, 1000.000000000000227 ) ;
#49517 = DIRECTION ( 'NONE',  ( 0.000000000000000000, 0.000000000000000000, 1.000000000000000000 ) ) ;
#49518 = FACE_OUTER_BOUND ( 'NONE', #14748, .T. ) ;
#49519 = CARTESIAN_POINT ( 'NONE',  ( 0.9756354156337452288, 37.22481466014927776, -21.34128958497340989 ) ) ;
#49520 = LINE ( 'NONE', #34208, #61400 ) ;
#49521 = DIRECTION ( 'NONE',  ( 0.000000000000000000, 0.000000000000000000, 1.000000000000000000 ) ) ;
#49522 = ADVANCED_FACE ( 'NONE', ( #12807 ), #11355, .F. ) ;
#49523 = CARTESIAN_POINT ( 'NONE',  ( 5.901764892641307547, 7.772884649736512053, 48.34846152321259893 ) ) ;
#49524 = CARTESIAN_POINT ( 'NONE',  ( 0.8760168074886965917, 28.57146030081927890, 38.69913431881832366 ) ) ;
#49525 = CARTESIAN_POINT ( 'NONE',  ( 0.000000000000000000, 0.000000000000000000, 0.000000000000000000 ) ) ;
#49526 = CARTESIAN_POINT ( 'NONE',  ( 2.282816707992318506, 21.41355441518730984, -41.80857153402610749 ) ) ;
#49527 = VERTEX_POINT ( 'NONE', #51289 ) ;
#49528 = CARTESIAN_POINT ( 'NONE',  ( 3.727782113643637096, -3.544252717309863243, -43.82026983693523903 ) ) ;
#49529 = AXIS2_PLACEMENT_3D ( 'NONE', #60780, #61692, #22903 ) ;
#49530 = CARTESIAN_POINT ( 'NONE',  ( 2.299652685299200972, -44.95079749811529979, -19.58845397527800003 ) ) ;
#49531 = VERTEX_POINT ( 'NONE', #36305 ) ;
#49532 = CARTESIAN_POINT ( 'NONE',  ( 0.8751705887134553219, -23.27176129838455054, 42.09020928323333521 ) ) ;
#49533 = CARTESIAN_POINT ( 'NONE',  ( 4.549368137175248350, 13.59764261105693350, 40.71620287708348940 ) ) ;
#49534 = CARTESIAN_POINT ( 'NONE',  ( 0.6030672727741701600, -12.36682345648149095, -46.49075153683468642 ) ) ;
#49535 = ORIENTED_EDGE ( 'NONE', *, *, #50574, .T. ) ;
#49536 = EDGE_CURVE ( 'NONE', #26981, #24288, #39866, .T. ) ;
#49537 = CARTESIAN_POINT ( 'NONE',  ( 0.6846871229502932144, -38.52803883689320941, 28.47437962186113225 ) ) ;
#49538 = ORIENTED_EDGE ( 'NONE', *, *, #27506, .F. ) ;
#49539 = CARTESIAN_POINT ( 'NONE',  ( 0.6028777368367060907, 10.84253002538188859, 47.89550471557602407 ) ) ;
#49540 = B_SPLINE_CURVE_WITH_KNOTS ( 'NONE', 3,
 ( #8882, #46814, #27991, #17667 ),
 .UNSPECIFIED., .F., .F.,
 ( 4, 4 ),
 ( 0.000000000000000000, 0.004447772540403802446 ),
 .UNSPECIFIED. ) ;
#49541 = ORIENTED_EDGE ( 'NONE', *, *, #58986, .T. ) ;
#49542 = ORIENTED_EDGE ( 'NONE', *, *, #55714, .F. ) ;
#49543 = CARTESIAN_POINT ( 'NONE',  ( -6.079354080745853928, 19.09774425860443259, 2.463558296672413217 ) ) ;
#49544 = ORIENTED_EDGE ( 'NONE', *, *, #31486, .F. ) ;
#49545 = LINE ( 'NONE', #25750, #59090 ) ;
#49546 = ADVANCED_FACE ( 'NONE', ( #7440 ), #35344, .F. ) ;
#49547 = CARTESIAN_POINT ( 'NONE',  ( 0.9785694773339244090, -17.43866978178105853, -38.10811202298887679 ) ) ;
#49548 = EDGE_LOOP ( 'NONE', ( #41270, #28054, #19150, #27452 ) ) ;
#49549 = CARTESIAN_POINT ( 'NONE',  ( 0.5997462898726536595, 46.43852004798865352, -15.96920429754923632 ) ) ;
#49550 = B_SPLINE_CURVE_WITH_KNOTS ( 'NONE', 3,
 ( #59390, #16820, #54068, #25581, #44719, #35009, #16195, #21817, #2063, #49386, #15893, #20890, #58764, #35627, #40332, #50310, #45336, #1758, #7697 ),
 .UNSPECIFIED., .F., .F.,
 ( 4, 3, 3, 3, 3, 3, 4 ),
 ( 1.144439277862597989E-16, 0.0002618519381806255373, 0.0003927759815486000952, 0.0005237000248299464658, 0.0006546240681325001020, 0.0007855481115631326007, 0.0009699050456655100745 ),
 .UNSPECIFIED. ) ;
#49551 = CARTESIAN_POINT ( 'NONE',  ( -6.015611763856276717, 2.465697960551318069, -18.68122482568277221 ) ) ;
#49552 = EDGE_CURVE ( 'NONE', #52623, #47838, #2640, .T. ) ;
#49553 = VERTEX_POINT ( 'NONE', #55369 ) ;
#49554 = CARTESIAN_POINT ( 'NONE',  ( 0.8751705887134423323, -47.79200036674284036, 5.393078191591890835 ) ) ;
#49555 = B_SPLINE_CURVE_WITH_KNOTS ( 'NONE', 3,
 ( #2669, #59372, #40619, #26802, #21481, #59687, #36220, #54352, #8001, #45939, #16801, #40317, #17406, #45013, #49676, #46237, #35912, #3278, #22411, #2982, #36530, #6730, #26488, #31499, #60601 ),
 .UNSPECIFIED., .F., .F.,
 ( 4, 3, 3, 3, 3, 3, 3, 3, 4 ),
 ( 5.553824967135426632E-18, 0.0005656085177311387727, 0.001131215744874499406, 0.001696821861372765482, 0.002262427090022497284, 0.002828031679238746793, 0.003393635864401605730, 0.003977030878808133357, 0.004561030005651160735 ),
 .UNSPECIFIED. ) ;
#49556 = CARTESIAN_POINT ( 'NONE',  ( 0.1073791018717483448, 41.52698815987167791, -11.62916352156108779 ) ) ;
#49557 = CARTESIAN_POINT ( 'NONE',  ( 5.959547316686252039, -14.51632612601538952, 14.51128755440516116 ) ) ;
#49558 = CARTESIAN_POINT ( 'NONE',  ( 0.9775691876210987896, 35.86428463458979365, 21.68148511147509794 ) ) ;
#49559 = ORIENTED_EDGE ( 'NONE', *, *, #42887, .T. ) ;
#49560 = ORIENTED_EDGE ( 'NONE', *, *, #1121, .F. ) ;
#49561 = CARTESIAN_POINT ( 'NONE',  ( 0.6000166863083090663, -45.71468846346261472, 17.94410043432136703 ) ) ;
#49562 = CARTESIAN_POINT ( 'NONE',  ( 4.956653778116966613, 0.000000000000000000, 0.000000000000000000 ) ) ;
#49563 = CIRCLE ( 'NONE', #512, 42.92674063221959813 ) ;
#49564 = EDGE_LOOP ( 'NONE', ( #34675, #18582, #33432, #35167 ) ) ;
#49565 = CARTESIAN_POINT ( 'NONE',  ( 5.959547316686252039, -17.77749189599210311, -10.25972575517523744 ) ) ;
#49566 = CARTESIAN_POINT ( 'NONE',  ( 5.896782393890504181, -2.006887468070398750, 20.01245835894516389 ) ) ;
#49567 = CARTESIAN_POINT ( 'NONE',  ( 1.157643937452369043, 41.42449707914801849, -6.404163984035045942 ) ) ;
#49568 = CARTESIAN_POINT ( 'NONE',  ( 0.6031356755773454870, -41.66228085015309546, -24.05369945659519004 ) ) ;
#49569 = EDGE_CURVE ( 'NONE', #3017, #1874, #28825, .T. ) ;
#49570 = B_SPLINE_CURVE_WITH_KNOTS ( 'NONE', 3,
 ( #1311, #53935, #11061, #11357 ),
 .UNSPECIFIED., .F., .F.,
 ( 4, 4 ),
 ( 7.656893354757642997E-17, 0.005004948556313879027 ),
 .UNSPECIFIED. ) ;
#49571 = ORIENTED_EDGE ( 'NONE', *, *, #56895, .F. ) ;
#49572 = ORIENTED_EDGE ( 'NONE', *, *, #1373, .F. ) ;
#49573 = CARTESIAN_POINT ( 'NONE',  ( -2.569797478183790229, -11.33042594333542041, -9.259773107243024270 ) ) ;
#49574 = CARTESIAN_POINT ( 'NONE',  ( 3.390910168358336918, 42.31681000770872458, 11.97433619475916800 ) ) ;
#49575 = EDGE_CURVE ( 'NONE', #24938, #46940, #43891, .T. ) ;
#49576 = CARTESIAN_POINT ( 'NONE',  ( 4.956445790444026223, 2.113652668516905031, -47.04328350079857302 ) ) ;
#49577 = AXIS2_PLACEMENT_3D ( 'NONE', #20029, #39141, #34428 ) ;
#49578 = CARTESIAN_POINT ( 'NONE',  ( 0.6000166863083106206, 33.40185771989251862, 36.00193581696004230 ) ) ;
#49579 = CARTESIAN_POINT ( 'NONE',  ( 0.8557997880470606944, -17.48760788519184217, -44.60232077416704755 ) ) ;
#49580 = EDGE_CURVE ( 'NONE', #26668, #36895, #17489, .T. ) ;
#49581 = CARTESIAN_POINT ( 'NONE',  ( 1.296416391601052931, -41.25474789393634012, -15.50332707143577338 ) ) ;
#49582 = CARTESIAN_POINT ( 'NONE',  ( 2.009741617377216460, -13.83851655386614077, -41.80908438618833145 ) ) ;
#49583 = CARTESIAN_POINT ( 'NONE',  ( -6.017396004339687465, 11.47005965438138375, 14.95000090562885475 ) ) ;
#49584 = CARTESIAN_POINT ( 'NONE',  ( -2.601141883200665639, -8.117336596316299335, 12.52614362249981284 ) ) ;
#49585 = LINE ( 'NONE', #20182, #59868 ) ;
#49586 = CARTESIAN_POINT ( 'NONE',  ( 0.8557997880470606944, -28.43566216844945771, -38.55640757422467857 ) ) ;
#49587 = CARTESIAN_POINT ( 'NONE',  ( 0.5800708119828337228, -41.16171018093176315, 24.48933355903750453 ) ) ;
#49588 = CARTESIAN_POINT ( 'NONE',  ( 5.895596859100789899, 14.91916793517901496, 13.48875870250535058 ) ) ;
#49589 = ADVANCED_FACE ( 'NONE', ( #59454 ), #9828, .F. ) ;
#49590 = CARTESIAN_POINT ( 'NONE',  ( 0.5807400328401637335, -47.55718917606839824, -5.711437504336458915 ) ) ;
#49591 = FACE_OUTER_BOUND ( 'NONE', #50239, .T. ) ;
#49592 = CARTESIAN_POINT ( 'NONE',  ( 3.783278058412224087, 3.901118461247438773, -42.86118820526426276 ) ) ;
#49593 = CARTESIAN_POINT ( 'NONE',  ( 0.9787284016396593511, -22.39226333978123407, 35.42488590596618536 ) ) ;
#49594 =( BOUNDED_SURFACE ( )  B_SPLINE_SURFACE ( 3, 1, ( 
 ( #36761, #9150 ),
 ( #12956, #61139 ),
 ( #55834, #60837 ),
 ( #17956, #4419 ) ),
 .UNSPECIFIED., .F., .F., .F. ) 
 B_SPLINE_SURFACE_WITH_KNOTS ( ( 4, 4 ),
 ( 2, 2 ),
 ( 0.000000000000000000, 1.000000000000000000 ),
 ( 0.000000000000000000, 1.000000000000000000 ),
 .UNSPECIFIED. ) 
 GEOMETRIC_REPRESENTATION_ITEM ( )  RATIONAL_B_SPLINE_SURFACE ( (
 ( 1.000000000000000000, 1.000000000000000000),
 ( 0.9729067724841187204, 0.9999501103223794596),
 ( 0.9729067724841187204, 0.9999501103223794596),
 ( 1.000000000000000000, 1.000000000000000000) ) ) 
 REPRESENTATION_ITEM ( '' )  SURFACE ( )  );
#49595 = CARTESIAN_POINT ( 'NONE',  ( 5.283180000000047727, 0.000000000000000000, 0.000000000000000000 ) ) ;
#49596 = CARTESIAN_POINT ( 'NONE',  ( 4.956653778116827169, 32.11725092155053574, 35.79382859084104496 ) ) ;
#49597 = CARTESIAN_POINT ( 'NONE',  ( 0.6027444965799114707, 48.17669769696837534, 9.515477649722281939 ) ) ;
#49599 = ORIENTED_EDGE ( 'NONE', *, *, #44873, .F. ) ;
#49598 = CARTESIAN_POINT ( 'NONE',  ( 1.227938101723747621, 20.72293514920750468, 37.58536632582787007 ) ) ;
#49600 = VERTEX_POINT ( 'NONE', #21568 ) ;
#49601 = CARTESIAN_POINT ( 'NONE',  ( 4.962356264823601038, -35.98698831890646943, 21.82137185415336589 ) ) ;
#49602 = CARTESIAN_POINT ( 'NONE',  ( 0.3676999524040366896, 43.96170928169366476, -3.649479463524768263 ) ) ;
#49603 = DIRECTION ( 'NONE',  ( 0.1024043820194936449, 0.7126273545981393065, 0.6940285268068333568 ) ) ;
#49604 = ORIENTED_EDGE ( 'NONE', *, *, #40952, .F. ) ;
#49605 = B_SPLINE_CURVE_WITH_KNOTS ( 'NONE', 3,
 ( #16461, #7656, #26163, #2652, #59984, #45300 ),
 .UNSPECIFIED., .F., .F.,
 ( 4, 2, 4 ),
 ( 6.149443329761889321E-18, 0.0002445244328975378903, 0.0004890488657950697090 ),
 .UNSPECIFIED. ) ;
#49606 = ORIENTED_EDGE ( 'NONE', *, *, #46606, .F. ) ;
#49607 = CARTESIAN_POINT ( 'NONE',  ( 1.157643937452368599, -23.24616979670748407, -34.88004966133790674 ) ) ;
#49608 = CARTESIAN_POINT ( 'NONE',  ( 1.827326673878743701, 1.232746109312175431, -43.03225468313001301 ) ) ;
#49609 = CARTESIAN_POINT ( 'NONE',  ( -6.072942160501519027, -18.89839206595246424, -3.695259072185007376 ) ) ;
#49610 = ORIENTED_EDGE ( 'NONE', *, *, #2961, .T. ) ;
#49611 = ORIENTED_EDGE ( 'NONE', *, *, #3995, .F. ) ;
#49612 = B_SPLINE_CURVE_WITH_KNOTS ( 'NONE', 3,
 ( #41908, #29316, #48426, #5488, #28391, #47209, #28703, #38750, #33423, #38136, #809, #14626, #4255, #52498, #171, #23700, #47829, #33116, #61580 ),
 .UNSPECIFIED., .F., .F.,
 ( 4, 3, 3, 3, 3, 3, 4 ),
 ( 9.813676791237319219E-18, 0.0002724573126191793876, 0.0004086839781548473388, 0.0005449106435901772579, 0.0006811373090491502653, 0.0008459866663933714344, 0.001010840725717214016 ),
 .UNSPECIFIED. ) ;
#49613 = CARTESIAN_POINT ( 'NONE',  ( 0.8753041380234471980, 48.01981714478390728, 10.25843502950123742 ) ) ;
#49614 = EDGE_CURVE ( 'NONE', #26701, #9789, #27492, .T. ) ;
#49615 = CARTESIAN_POINT ( 'NONE',  ( 4.956445790444035104, 41.78282513192535674, -21.71942849465849079 ) ) ;
#49616 = AXIS2_PLACEMENT_3D ( 'NONE', #52717, #52097, #38051 ) ;
#49617 = CARTESIAN_POINT ( 'NONE',  ( 2.301430502907644726, -47.77346269870103868, 4.990893951996192790 ) ) ;
#49618 = ADVANCED_FACE ( 'NONE', ( #2442 ), #48140, .F. ) ;
#49619 = ORIENTED_EDGE ( 'NONE', *, *, #24811, .T. ) ;
#49621 = CARTESIAN_POINT ( 'NONE',  ( 0.8751705887134553219, 19.22545746485597817, 44.08562551107088723 ) ) ;
#49620 = AXIS2_PLACEMENT_3D ( 'NONE', #37455, #19266, #56526 ) ;
#49622 = B_SPLINE_CURVE_WITH_KNOTS ( 'NONE', 3,
 ( #40315, #2359, #21479, #40617 ),
 .UNSPECIFIED., .F., .F.,
 ( 4, 4 ),
 ( 0.000000000000000000, 0.004442905043737217438 ),
 .UNSPECIFIED. ) ;
#49623 = EDGE_CURVE ( 'NONE', #23536, #10336, #39964, .T. ) ;
#49624 = CARTESIAN_POINT ( 'NONE',  ( 0.7764139734771247081, -29.59659215482911421, -36.38794036116326680 ) ) ;
#49625 = CARTESIAN_POINT ( 'NONE',  ( 0.1158516988532803382, 15.19273855081792846, -41.42611319155211191 ) ) ;
#49626 = ORIENTED_EDGE ( 'NONE', *, *, #59662, .T. ) ;
#49627 = EDGE_CURVE ( 'NONE', #51246, #37964, #60082, .T. ) ;
#49628 = VECTOR ( 'NONE', #340, 1000.000000000000114 ) ;
#49629 = ORIENTED_EDGE ( 'NONE', *, *, #21657, .F. ) ;
#49630 = CARTESIAN_POINT ( 'NONE',  ( 0.9762797500689124330, -30.73989051779348003, 28.48480149377514437 ) ) ;
#49631 = CARTESIAN_POINT ( 'NONE',  ( -6.015611763856276717, 9.427003116184401676, -16.31561949997065852 ) ) ;
#49632 = ORIENTED_EDGE ( 'NONE', *, *, #26251, .F. ) ;
#49633 = CARTESIAN_POINT ( 'NONE',  ( 4.549368137175248350, 19.17571786012269541, 38.40568845698284406 ) ) ;
#49634 = CARTESIAN_POINT ( 'NONE',  ( 0.8560838555295158248, -13.02223058219810881, -45.06433561859972059 ) ) ;
#49635 = CARTESIAN_POINT ( 'NONE',  ( 5.895596859100789899, -11.93344155749883662, -16.19015613903236428 ) ) ;
#49636 = CARTESIAN_POINT ( 'NONE',  ( 0.7762783648524369529, -17.50713302551360684, 44.59086139387537884 ) ) ;
#49637 = ORIENTED_EDGE ( 'NONE', *, *, #982, .T. ) ;
#49638 = CARTESIAN_POINT ( 'NONE',  ( 0.9758171775293911221, -30.34506652060224141, -30.33669560438100987 ) ) ;
#49639 = CARTESIAN_POINT ( 'NONE',  ( 4.967162193818130511, 42.96271701169388990, -3.259922920617310371 ) ) ;
#49640 = B_SPLINE_CURVE_WITH_KNOTS ( 'NONE', 3,
 ( #53726, #2351, #45308, #20557, #35284, #59364 ),
 .UNSPECIFIED., .F., .F.,
 ( 4, 2, 4 ),
 ( 3.476216610979977084E-18, 0.0002291966416970829816, 0.0004583932833941624938 ),
 .UNSPECIFIED. ) ;
#49641 = VERTEX_POINT ( 'NONE', #48156 ) ;
#49642 = CARTESIAN_POINT ( 'NONE',  ( -2.569797478183783568, 14.62602397812941390, -0.4487456364277307430 ) ) ;
#49643 = CARTESIAN_POINT ( 'NONE',  ( 0.6254087463353915632, -47.77987801197956941, -5.596276562478156080 ) ) ;
#49644 = EDGE_LOOP ( 'NONE', ( #33234, #33484, #28859, #23691 ) ) ;
#49645 = CARTESIAN_POINT ( 'NONE',  ( 4.962356264823593044, 12.88441948660167391, 40.06528837230087703 ) ) ;
#49646 = ADVANCED_FACE ( 'NONE', ( #198 ), #17766, .F. ) ;
#49647 = ORIENTED_EDGE ( 'NONE', *, *, #5994, .T. ) ;
#49648 = CARTESIAN_POINT ( 'NONE',  ( 0.6254087463353924514, -5.596276562478680106, 47.77987801197951256 ) ) ;
#49649 = EDGE_CURVE ( 'NONE', #29428, #25119, #59855, .T. ) ;
#49650 = CARTESIAN_POINT ( 'NONE',  ( 0.5804410086790514622, 37.14246315962257938, -28.63489623329331479 ) ) ;
#49651 = CARTESIAN_POINT ( 'NONE',  ( 1.231276596079887264, 24.17959027891153667, -34.24360064248551083 ) ) ;
#49652 = EDGE_CURVE ( 'NONE', #18605, #3794, #5820, .T. ) ;
#49653 = CARTESIAN_POINT ( 'NONE',  ( 0.6030672727741701600, -41.70584815505905141, 23.97812608463460293 ) ) ;
#49654 = CARTESIAN_POINT ( 'NONE',  ( 3.050102900204245682, 21.93629751651464943, 38.13429034930390316 ) ) ;
#49655 = CARTESIAN_POINT ( 'NONE',  ( -6.010958268070873523, 18.19761767765829674, 4.891065400978450661 ) ) ;
#49656 = DIRECTION ( 'NONE',  ( 0.000000000000000000, 0.000000000000000000, 1.000000000000000000 ) ) ;
#49657 = CARTESIAN_POINT ( 'NONE',  ( 7.000000000000006217, 8.392413579938656024E-13, -80.00000000000001421 ) ) ;
#49658 = FACE_OUTER_BOUND ( 'NONE', #22757, .T. ) ;
#49659 = AXIS2_PLACEMENT_3D ( 'NONE', #34739, #54420, #1495 ) ;
#49660 = CARTESIAN_POINT ( 'NONE',  ( 0.5839254288179569485, 37.94310411505145453, 29.22920395911524949 ) ) ;
#49661 = CARTESIAN_POINT ( 'NONE',  ( 0.9789233960466692253, 14.93951272412277653, 39.15542984565634299 ) ) ;
#49662 = ORIENTED_EDGE ( 'NONE', *, *, #4351, .T. ) ;
#49663 = STYLED_ITEM ( 'NONE', ( #46718 ), #51224 ) ;
#49664 = VECTOR ( 'NONE', #39279, 999.9999999999998863 ) ;
#49665 = CARTESIAN_POINT ( 'NONE',  ( -16.29513786217388116, -12.43465849276918078, 1.291204549316803174 ) ) ;
#49666 = CARTESIAN_POINT ( 'NONE',  ( 4.549368137175248350, 0.000000000000000000, 0.000000000000000000 ) ) ;
#49667 = CARTESIAN_POINT ( 'NONE',  ( -4.000000000000000000, 0.3904826640788061631, -5.600000000000000533 ) ) ;
#49668 = CARTESIAN_POINT ( 'NONE',  ( 0.1129192098497455998, 44.06201484046248140, -2.343210614524073421 ) ) ;
#49669 = ADVANCED_FACE ( 'NONE', ( #32518 ), #6805, .T. ) ;
#49670 = CARTESIAN_POINT ( 'NONE',  ( 1.827326673878743923, -31.30008222956402619, 29.55671596281155189 ) ) ;
#49671 = CARTESIAN_POINT ( 'NONE',  ( 0.1129192098497447394, 19.97823103613683315, -39.34236993944178806 ) ) ;
#49672 = CARTESIAN_POINT ( 'NONE',  ( 5.838029081930955932, -47.23414715677123610, -0.02001313068654116470 ) ) ;
#49673 =( BOUNDED_SURFACE ( )  B_SPLINE_SURFACE ( 3, 1, ( 
 ( #29953, #49061 ),
 ( #38153, #19962 ),
 ( #19333, #25253 ),
 ( #58132, #34360 ) ),
 .UNSPECIFIED., .F., .F., .F. ) 
 B_SPLINE_SURFACE_WITH_KNOTS ( ( 4, 4 ),
 ( 2, 2 ),
 ( 0.000000000000000000, 1.000000000000000000 ),
 ( 0.000000000000000000, 1.000000000000000000 ),
 .UNSPECIFIED. ) 
 GEOMETRIC_REPRESENTATION_ITEM ( )  RATIONAL_B_SPLINE_SURFACE ( (
 ( 1.000000000000000000, 1.000000000000000000),
 ( 0.9953040768229013402, 0.8617119497784988535),
 ( 0.9953040768229013402, 0.8617119497784988535),
 ( 1.000000000000000000, 1.000000000000000000) ) ) 
 REPRESENTATION_ITEM ( '' )  SURFACE ( )  );
#49674 = EDGE_CURVE ( 'NONE', #53979, #14851, #38460, .T. ) ;
#49675 = B_SPLINE_CURVE_WITH_KNOTS ( 'NONE', 3,
 ( #38242, #41710, #4664, #56687 ),
 .UNSPECIFIED., .F., .F.,
 ( 4, 4 ),
 ( 2.030441771438897272E-17, 0.004444306975806115896 ),
 .UNSPECIFIED. ) ;
#49676 = CARTESIAN_POINT ( 'NONE',  ( 2.185380717157384023, 36.09826614752458340, -25.21378559855064339 ) ) ;
#49677 = TOROIDAL_SURFACE ( 'NONE', #39698, 12.55882000000000076, 0.05882000000000066342 ) ;
#49678 = CARTESIAN_POINT ( 'NONE',  ( 2.301430502907645170, -30.25184447737462179, 37.31003439265355581 ) ) ;
#49680 = ORIENTED_EDGE ( 'NONE', *, *, #43321, .T. ) ;
#49679 = CARTESIAN_POINT ( 'NONE',  ( 0.5987334308729319599, -45.28813393713827651, 18.98809708900693849 ) ) ;
#49681 = ORIENTED_EDGE ( 'NONE', *, *, #57315, .T. ) ;
#49682 = CARTESIAN_POINT ( 'NONE',  ( 8.000000000000000000, -2.549224068967256091E-30, 75.00000000000001421 ) ) ;
#49683 = B_SPLINE_CURVE_WITH_KNOTS ( 'NONE', 3,
 ( #3351, #7752, #60991, #18099 ),
 .UNSPECIFIED., .F., .F.,
 ( 4, 4 ),
 ( 0.000000000000000000, 0.005014147105413699519 ),
 .UNSPECIFIED. ) ;
#49684 = CARTESIAN_POINT ( 'NONE',  ( 4.214292481396495482, -11.25702090725073035, -1.199999999999999956 ) ) ;
#49685 = CARTESIAN_POINT ( 'NONE',  ( 0.1092565886968785427, 16.78938711553573881, 39.72209809039404149 ) ) ;
#49686 = CYLINDRICAL_SURFACE ( 'NONE', #47517, 15.43999999999999240 ) ;
#49687 = CARTESIAN_POINT ( 'NONE',  ( 0.7954190325252783467, 0.8690070772082590933, 48.09103420665682904 ) ) ;
#49688 = CARTESIAN_POINT ( 'NONE',  ( 0.1100247026804066219, 41.69861001364773045, -10.99745200874652085 ) ) ;
#49689 = ORIENTED_EDGE ( 'NONE', *, *, #20303, .F. ) ;
#49690 = ORIENTED_EDGE ( 'NONE', *, *, #58965, .T. ) ;
#49691 = CARTESIAN_POINT ( 'NONE',  ( 4.553261556744875094, 0.000000000000000000, 0.000000000000000000 ) ) ;
#49692 = B_SPLINE_CURVE_WITH_KNOTS ( 'NONE', 3,
 ( #28681, #57464, #47806, #23985, #43115, #19298 ),
 .UNSPECIFIED., .F., .F.,
 ( 4, 2, 4 ),
 ( 1.015220885719448790E-17, 0.0002291978881530158890, 0.0004583957763060215866 ),
 .UNSPECIFIED. ) ;
#49693 = CARTESIAN_POINT ( 'NONE',  ( 4.553261556744875094, -43.85016385001095784, 2.588956575693979190 ) ) ;
#49694 = CARTESIAN_POINT ( 'NONE',  ( 3.661921753702009230, -42.79842403921696814, -19.51732624089203227 ) ) ;
#49695 = VERTEX_POINT ( 'NONE', #23115 ) ;
#49696 = EDGE_CURVE ( 'NONE', #32441, #58934, #27849, .T. ) ;
#49697 = ORIENTED_EDGE ( 'NONE', *, *, #424, .T. ) ;
#49698 = EDGE_CURVE ( 'NONE', #36963, #19158, #9309, .T. ) ;
#49699 = CARTESIAN_POINT ( 'NONE',  ( 1.157643937452369265, -27.68781119398633805, -31.47042080876771308 ) ) ;
#49700 = LINE ( 'NONE', #6758, #9694 ) ;
#49701 = ORIENTED_EDGE ( 'NONE', *, *, #44103, .F. ) ;
#49702 = CARTESIAN_POINT ( 'NONE',  ( 4.962356264823594820, 34.94214251265108118, 23.45809613945535332 ) ) ;
#49703 = CARTESIAN_POINT ( 'NONE',  ( 8.000000000000012434, -85.00000000000001421, -1.540743955509788245E-31 ) ) ;
#49704 = CONICAL_SURFACE ( 'NONE', #32736, 43.08621763946400307, 1.568696531533066763 ) ;
#49705 = ORIENTED_EDGE ( 'NONE', *, *, #43575, .T. ) ;
#49706 = EDGE_CURVE ( 'NONE', #37795, #40320, #36301, .T. ) ;
#49707 = EDGE_CURVE ( 'NONE', #11417, #60124, #19102, .T. ) ;
#49708 = CARTESIAN_POINT ( 'NONE',  ( 0.8551540677456834771, 13.28067116677201831, 46.03951182599431746 ) ) ;
#49709 = CARTESIAN_POINT ( 'NONE',  ( -6.078726893082806448, 15.43407385306378998, -11.51448676958260187 ) ) ;
#49710 = EDGE_LOOP ( 'NONE', ( #60732, #6061, #45002, #9732 ) ) ;
#49711 = FACE_OUTER_BOUND ( 'NONE', #61771, .T. ) ;
#49712 = EDGE_CURVE ( 'NONE', #14392, #46447, #41349, .T. ) ;
#49713 = CARTESIAN_POINT ( 'NONE',  ( 0.8560838555295158248, -30.97734773434503808, 35.22466126774251194 ) ) ;
#49714 = DIRECTION ( 'NONE',  ( 1.000000000000000000, 1.836909530733573776E-16, 0.000000000000000000 ) ) ;
#49715 = CARTESIAN_POINT ( 'NONE',  ( -5.995132425357893702, 7.203480333239078881, 17.41298668506973257 ) ) ;
#49716 = ORIENTED_EDGE ( 'NONE', *, *, #8546, .F. ) ;
#49717 = CARTESIAN_POINT ( 'NONE',  ( 0.6041374136657475802, 44.51224464244998558, -18.24862627831490158 ) ) ;
#49718 = DIRECTION ( 'NONE',  ( -1.000000000000000000, -0.000000000000000000, -0.000000000000000000 ) ) ;
#49719 = VERTEX_POINT ( 'NONE', #53738 ) ;
#49720 = CARTESIAN_POINT ( 'NONE',  ( 0.6000166863083106206, -31.02657807334512086, -38.06803035050636197 ) ) ;
#49721 = B_SPLINE_CURVE_WITH_KNOTS ( 'NONE', 3,
 ( #21821, #32153, #18057, #37173, #40959, #32457, #31523, #8315, #27753, #27436, #50615, #55619, #60019, #7702, #26828, #45961, #22128, #41257, #60316 ),
 .UNSPECIFIED., .F., .F.,
 ( 4, 3, 3, 3, 3, 3, 4 ),
 ( 0.000000000000000000, 0.0002612768053151694864, 0.0003919133833142915218, 0.0005225499612322621629, 0.0006531865391693355248, 0.0008112755173415210500, 0.0009693688056799720310 ),
 .UNSPECIFIED. ) ;
#49722 = EDGE_CURVE ( 'NONE', #4545, #58288, #52676, .T. ) ;
#49723 = ORIENTED_EDGE ( 'NONE', *, *, #6356, .F. ) ;
#49724 = CARTESIAN_POINT ( 'NONE',  ( 1.154321713695925622, -36.74718012229642738, -22.16897764010645133 ) ) ;
#49725 = EDGE_LOOP ( 'NONE', ( #12742, #7718, #13573, #45512 ) ) ;
#49726 = CARTESIAN_POINT ( 'NONE',  ( 4.962356264823603702, -20.60668162140254722, -36.69605251817282010 ) ) ;
#49727 = CARTESIAN_POINT ( 'NONE',  ( 1.227938101723756947, 29.74462687941269223, -30.94118573761281965 ) ) ;
#49728 = LINE ( 'NONE', #5557, #48290 ) ;
#49729 = VERTEX_POINT ( 'NONE', #14963 ) ;
#49730 = CARTESIAN_POINT ( 'NONE',  ( 0.5839254288179543950, 6.161657890844935537, 47.49799454719520497 ) ) ;
#49731 = DIRECTION ( 'NONE',  ( -1.000000000000000000, -0.000000000000000000, -0.000000000000000000 ) ) ;
#49732 = CARTESIAN_POINT ( 'NONE',  ( 16.60577576646022280, -4.999999999999991118, -10.00000000000000711 ) ) ;
#49733 = B_SPLINE_CURVE_WITH_KNOTS ( 'NONE', 3,
 ( #3419, #17547, #56047, #36665, #8430, #37284, #55734, #16944, #56352, #59829, #13469, #40764, #32578, #51657, #8748, #27864, #36058, #55123, #12245, #50434, #7501, #45756, #60135, #17244, #7822 ),
 .UNSPECIFIED., .F., .F.,
 ( 4, 3, 3, 3, 3, 3, 3, 3, 4 ),
 ( 4.336808689942017736E-18, 0.0005656085177311415916, 0.001131215744874502008, 0.001696821861372767868, 0.002262427090022499886, 0.002828031679238747660, 0.003393635864401606597, 0.003977030878808131623, 0.004561030005651158133 ),
 .UNSPECIFIED. ) ;
#49734 = ORIENTED_EDGE ( 'NONE', *, *, #4754, .F. ) ;
#49735 = VECTOR ( 'NONE', #18169, 999.9999999999998863 ) ;
#49736 = ORIENTED_EDGE ( 'NONE', *, *, #19888, .F. ) ;
#49737 = CARTESIAN_POINT ( 'NONE',  ( 0.5832366564991493529, 18.58038995918353820, 44.14509737861656191 ) ) ;
#49738 = CARTESIAN_POINT ( 'NONE',  ( 2.185380717157383135, 30.65186932183861046, 31.61143321876008017 ) ) ;
#49739 = CARTESIAN_POINT ( 'NONE',  ( 0.9784957157296394481, 38.49170563740425877, -16.57472938288250575 ) ) ;
#49740 = CARTESIAN_POINT ( 'NONE',  ( 0.1102144999581333162, -5.503895401229690343, -42.77179372778541477 ) ) ;
#49741 = CARTESIAN_POINT ( 'NONE',  ( 0.5804410086790514622, -30.69452151258743200, 35.45935984995646351 ) ) ;
#49742 = CARTESIAN_POINT ( 'NONE',  ( -2.708315649062910779, -12.80362818457450125, 7.087851317223748282 ) ) ;
#49743 = ORIENTED_EDGE ( 'NONE', *, *, #31277, .T. ) ;
#49744 = CARTESIAN_POINT ( 'NONE',  ( 0.5800708119828332787, 6.873289505980640257, 47.40012378203034160 ) ) ;
#49745 = ORIENTED_EDGE ( 'NONE', *, *, #52603, .F. ) ;
#49746 = CARTESIAN_POINT ( 'NONE',  ( -2.569797478183783568, -1.464172661884271198, 14.55946937464481117 ) ) ;
#49747 = CARTESIAN_POINT ( 'NONE',  ( 5.960721111146673579, -18.96557324978281756, -7.848955554238449928 ) ) ;
#49748 = CARTESIAN_POINT ( 'NONE',  ( 5.960221823109900008, -10.25807604135634143, 17.77840967225703039 ) ) ;
#49749 = EDGE_CURVE ( 'NONE', #57605, #31520, #54302, .T. ) ;
#49750 = CARTESIAN_POINT ( 'NONE',  ( 0.6039202388192952409, -47.54548494440610540, 12.28782219314079960 ) ) ;
#49751 = CARTESIAN_POINT ( 'NONE',  ( 4.960386119450153508, 42.96877549456534240, -8.253532405581291087 ) ) ;
#49752 = SURFACE_SIDE_STYLE ('',( #11241 ) ) ;
#49753 = EDGE_CURVE ( 'NONE', #58934, #43120, #24652, .T. ) ;
#49754 = CARTESIAN_POINT ( 'NONE',  ( 0.1158403557922069033, 20.44267117180008242, -39.10290913148882908 ) ) ;
#49755 = CARTESIAN_POINT ( 'NONE',  ( 0.7056555295713301534, -5.417452459790056629, 47.59410019435325268 ) ) ;
#49756 = AXIS2_PLACEMENT_3D ( 'NONE', #30997, #40125, #16282 ) ;
#49757 =( BOUNDED_SURFACE ( )  B_SPLINE_SURFACE ( 3, 1, ( 
 ( #26756, #55871 ),
 ( #40890, #22680 ),
 ( #59957, #56179 ),
 ( #50553, #12994 ) ),
 .UNSPECIFIED., .F., .F., .F. ) 
 B_SPLINE_SURFACE_WITH_KNOTS ( ( 4, 4 ),
 ( 2, 2 ),
 ( 0.000000000000000000, 1.000000000000000000 ),
 ( 0.000000000000000000, 1.000000000000000000 ),
 .UNSPECIFIED. ) 
 GEOMETRIC_REPRESENTATION_ITEM ( )  RATIONAL_B_SPLINE_SURFACE ( (
 ( 1.000000000000000000, 1.000000000000000000),
 ( 0.7269869731126821222, 0.9931720237060910339),
 ( 0.7269869731126821222, 0.9931720237060910339),
 ( 1.000000000000000000, 1.000000000000000000) ) ) 
 REPRESENTATION_ITEM ( '' )  SURFACE ( )  );
#49758 = CARTESIAN_POINT ( 'NONE',  ( 3.783278058412224976, -9.462251542474113819, 41.98530666033912695 ) ) ;
#49759 = DIRECTION ( 'NONE',  ( 0.000000000000000000, 0.000000000000000000, 1.000000000000000000 ) ) ;
#49760 = CONICAL_SURFACE ( 'NONE', #25743, 43.92652462719577500, 1.486293639869522343 ) ;
#49761 = CONICAL_SURFACE ( 'NONE', #42901, 43.08621763946400307, 1.568696531533066763 ) ;
#49762 = FACE_OUTER_BOUND ( 'NONE', #53220, .T. ) ;
#49763 = CARTESIAN_POINT ( 'NONE',  ( 3.407937589446174087, 13.51415833181188120, 2.242416846335643754 ) ) ;
#49764 = PRODUCT_DEFINITION_SHAPE ( 'NONE', 'NONE',  #61974 ) ;
#49765 = CYLINDRICAL_SURFACE ( 'NONE', #16477, 6.728125000000023448 ) ;
#49766 = CARTESIAN_POINT ( 'NONE',  ( 5.959828726073459926, 10.25888482581859407, -17.77796293532162863 ) ) ;
#49767 = VERTEX_POINT ( 'NONE', #38775 ) ;
#49768 = B_SPLINE_CURVE_WITH_KNOTS ( 'NONE', 3,
 ( #35130, #11952, #30713, #30395, #26631, #16951 ),
 .UNSPECIFIED., .F., .F.,
 ( 4, 2, 4 ),
 ( 1.283058336952897787E-16, 0.0002450741128632365705, 0.0004901482257263447715 ),
 .UNSPECIFIED. ) ;
#49769 = DIRECTION ( 'NONE',  ( 0.000000000000000000, 0.000000000000000000, 1.000000000000000000 ) ) ;
#49770 =( BOUNDED_SURFACE ( )  B_SPLINE_SURFACE ( 3, 1, ( 
 ( #17866, #56052 ),
 ( #24095, #9369 ),
 ( #28475, #23472 ),
 ( #33203, #19109 ) ),
 .UNSPECIFIED., .F., .F., .F. ) 
 B_SPLINE_SURFACE_WITH_KNOTS ( ( 4, 4 ),
 ( 2, 2 ),
 ( 0.000000000000000000, 1.000000000000000000 ),
 ( 0.000000000000000000, 1.000000000000000000 ),
 .UNSPECIFIED. ) 
 GEOMETRIC_REPRESENTATION_ITEM ( )  RATIONAL_B_SPLINE_SURFACE ( (
 ( 1.000000000000000000, 1.000000000000000000),
 ( 0.9953040768229013402, 0.8617119497784988535),
 ( 0.9953040768229013402, 0.8617119497784988535),
 ( 1.000000000000000000, 1.000000000000000000) ) ) 
 REPRESENTATION_ITEM ( '' )  SURFACE ( )  );
#49771 = DIRECTION ( 'NONE',  ( -0.000000000000000000, 0.000000000000000000, 1.000000000000000000 ) ) ;
#49772 = CARTESIAN_POINT ( 'NONE',  ( 0.9754402186311939005, -39.71365199966005122, -16.24692483025461343 ) ) ;
#49773 = CARTESIAN_POINT ( 'NONE',  ( 0.6016118706126977189, -45.38674246209918550, -18.75085767273094817 ) ) ;
#49774 = CARTESIAN_POINT ( 'NONE',  ( 0.1095718737110178975, -41.72082389913624212, 10.91304379104990119 ) ) ;
#49775 = ORIENTED_EDGE ( 'NONE', *, *, #2613, .F. ) ;
#49776 = CARTESIAN_POINT ( 'NONE',  ( 5.974727161628369032, 16.29297756969648603, -12.48248968439911799 ) ) ;
#49777 = CARTESIAN_POINT ( 'NONE',  ( 0.9757892942422827787, 16.37293303864358762, -39.66188497122476520 ) ) ;
#49778 = AXIS2_PLACEMENT_3D ( 'NONE', #47837, #28097, #43452 ) ;
#49779 = EDGE_CURVE ( 'NONE', #14890, #22780, #31356, .T. ) ;
#49780 = CARTESIAN_POINT ( 'NONE',  ( 0.6016118706126976079, -14.30603973001664286, 46.97752954367775402 ) ) ;
#49781 = VERTEX_POINT ( 'NONE', #34072 ) ;
#49782 = EDGE_CURVE ( 'NONE', #3829, #60616, #1862, .T. ) ;
#49783 = CARTESIAN_POINT ( 'NONE',  ( 0.1129192098497455998, -0.9297496242496093855, -44.11448008785053787 ) ) ;
#49784 = VECTOR ( 'NONE', #12734, 1000.000000000000000 ) ;
#49785 = ORIENTED_EDGE ( 'NONE', *, *, #44960, .T. ) ;
#49786 = EDGE_CURVE ( 'NONE', #27427, #56473, #15264, .T. ) ;
#49787 = FACE_OUTER_BOUND ( 'NONE', #52367, .T. ) ;
#49788 = CARTESIAN_POINT ( 'NONE',  ( 5.896782393890504181, 3.339090646272624419, 19.83372281075811827 ) ) ;
#49789 = ORIENTED_EDGE ( 'NONE', *, *, #19491, .T. ) ;
#49790 = CARTESIAN_POINT ( 'NONE',  ( 4.303969348037246512, 27.54579249306209832, 39.44373910178619980 ) ) ;
#49791 = EDGE_CURVE ( 'NONE', #38743, #37278, #12323, .T. ) ;
#49792 = EDGE_LOOP ( 'NONE', ( #43331, #4205, #42205, #61191 ) ) ;
#49793 = CARTESIAN_POINT ( 'NONE',  ( 5.901463166500146684, -18.52233187494211819, -7.838436850236139897 ) ) ;
#49794 = CARTESIAN_POINT ( 'NONE',  ( 0.1129192098497455998, 19.97823103613628248, 39.34236993944205807 ) ) ;
#49795 = ORIENTED_EDGE ( 'NONE', *, *, #22307, .T. ) ;
#49796 = ORIENTED_EDGE ( 'NONE', *, *, #22258, .F. ) ;
#49797 = CARTESIAN_POINT ( 'NONE',  ( 0.9789233960466690032, 20.25576450497998948, -36.68842775523553001 ) ) ;
#49798 = CARTESIAN_POINT ( 'NONE',  ( 1.000110580585058306, 28.65872797539951122, 30.57931970472783334 ) ) ;
#49799 = ORIENTED_EDGE ( 'NONE', *, *, #58145, .T. ) ;
#49800 = EDGE_LOOP ( 'NONE', ( #3754, #53678, #5627, #33084 ) ) ;
#49801 = CARTESIAN_POINT ( 'NONE',  ( 0.6001305935487422083, 23.60027211631772204, 41.92422178329177029 ) ) ;
#49802 = CARTESIAN_POINT ( 'NONE',  ( 5.894904586330512508, 3.346579165707272097, 19.83254446482590794 ) ) ;
#49803 = CARTESIAN_POINT ( 'NONE',  ( 0.6016117650947689910, -25.75423423388752653, -41.81232441841228109 ) ) ;
#49804 = EDGE_CURVE ( 'NONE', #1146, #19605, #54893, .T. ) ;
#49805 = VECTOR ( 'NONE', #12167, 1000.000000000000114 ) ;
#49806 = CARTESIAN_POINT ( 'NONE',  ( 0.5837799406558222826, 32.53627130208564466, -33.77328232988735834 ) ) ;
#49807 = CARTESIAN_POINT ( 'NONE',  ( 4.962356264823608143, 34.44911810793244200, 24.17630781256866612 ) ) ;
#49808 = ORIENTED_EDGE ( 'NONE', *, *, #18541, .T. ) ;
#49809 = DIRECTION ( 'NONE',  ( 0.07439287786467663199, 0.5965490341031214339, 0.7991213610169884962 ) ) ;
#49810 = CARTESIAN_POINT ( 'NONE',  ( -6.077587904424778920, 16.78120357693994791, -9.443898977817823948 ) ) ;
#49811 = ORIENTED_EDGE ( 'NONE', *, *, #10423, .F. ) ;
#49812 = CARTESIAN_POINT ( 'NONE',  ( 0.5817217712918335559, -46.75866061562757636, -3.586448304511290264 ) ) ;
#49813 = ORIENTED_EDGE ( 'NONE', *, *, #42189, .F. ) ;
#49814 = CARTESIAN_POINT ( 'NONE',  ( 4.960156602257181468, -41.40608197274652014, 20.99019478193036292 ) ) ;
#49815 = CARTESIAN_POINT ( 'NONE',  ( 4.956653778116975495, -26.26162724282400518, 40.28700667097671584 ) ) ;
#49816 = EDGE_LOOP ( 'NONE', ( #12304, #34852, #38192, #57609 ) ) ;
#49817 = FACE_OUTER_BOUND ( 'NONE', #3958, .T. ) ;
#49818 = CARTESIAN_POINT ( 'NONE',  ( 0.5980271706414734822, 36.93900200886744756, -32.36602189689906339 ) ) ;
#49819 = CARTESIAN_POINT ( 'NONE',  ( 52.25241694927984071, 12.34033889370408232, -1.995302726669112570 ) ) ;
#49820 = CARTESIAN_POINT ( 'NONE',  ( -19.64312921891423969, -12.43468193047187853, -1.281307455091694303 ) ) ;
#49821 = B_SPLINE_CURVE_WITH_KNOTS ( 'NONE', 3,
 ( #3086, #22217, #18442, #61327 ),
 .UNSPECIFIED., .F., .F.,
 ( 4, 4 ),
 ( 8.673617379884035472E-19, 0.004041751736740996012 ),
 .UNSPECIFIED. ) ;
#49822 = VECTOR ( 'NONE', #31412, 1000.000000000000000 ) ;
#49823 = VERTEX_POINT ( 'NONE', #16181 ) ;
#49824 = ORIENTED_EDGE ( 'NONE', *, *, #39071, .T. ) ;
#49825 = CARTESIAN_POINT ( 'NONE',  ( 5.958863334805807099, 14.51469124124479926, -14.51296551801787871 ) ) ;
#49827 = B_SPLINE_CURVE_WITH_KNOTS ( 'NONE', 3,
 ( #31981, #14117, #37614, #56068, #46703, #28486 ),
 .UNSPECIFIED., .F., .F.,
 ( 4, 2, 4 ),
 ( 9.929776742050823831E-18, 0.0002448709889506580240, 0.0004897419779013061818 ),
 .UNSPECIFIED. ) ;
#49826 = CARTESIAN_POINT ( 'NONE',  ( 4.000000000000003553, 2.309401076758524685, -5.242734410091827613 ) ) ;
#49828 = AXIS2_PLACEMENT_3D ( 'NONE', #38528, #52277, #24717 ) ;
#49829 =( NAMED_UNIT ( * ) SI_UNIT ( $, .STERADIAN. ) SOLID_ANGLE_UNIT ( ) );
#49830 = CARTESIAN_POINT ( 'NONE',  ( 5.960721111146673579, -7.860635756377761574, -18.96073515164545498 ) ) ;
#49831 = EDGE_CURVE ( 'NONE', #3927, #52762, #60888, .T. ) ;
#49832 = VERTEX_POINT ( 'NONE', #34368 ) ;
#49833 = CARTESIAN_POINT ( 'NONE',  ( 0.3622758884714730732, -25.58609868863794290, 34.70015533914785522 ) ) ;
#49834 = AXIS2_PLACEMENT_3D ( 'NONE', #4878, #42833, #14320 ) ;
#49835 = CARTESIAN_POINT ( 'NONE',  ( 0.2885700199627510565, 6.424755504217665170, 42.63514063525628472 ) ) ;
#49836 = CARTESIAN_POINT ( 'NONE',  ( 0.1155031312995260795, -35.46222914138566296, 26.25589337378687205 ) ) ;
#49837 = CARTESIAN_POINT ( 'NONE',  ( 5.958863334805807099, -5.313608583996656698, 19.82594244347343704 ) ) ;
#49838 = FACE_OUTER_BOUND ( 'NONE', #17755, .T. ) ;
#49839 = CARTESIAN_POINT ( 'NONE',  ( 0.6000166863083090663, 32.62822748873705336, 36.70452632376117919 ) ) ;
#49840 = CARTESIAN_POINT ( 'NONE',  ( 0.9730545539215883499, 42.60426903087360984, -5.099196237954451760 ) ) ;
#49841 = DIRECTION ( 'NONE',  ( -1.000000000000000000, -0.000000000000000000, -0.000000000000000000 ) ) ;
#49842 = B_SPLINE_CURVE_WITH_KNOTS ( 'NONE', 3,
 ( #19745, #4989, #43256, #5300 ),
 .UNSPECIFIED., .F., .F.,
 ( 4, 4 ),
 ( 2.165040709395311621E-17, 0.004444306975806115896 ),
 .UNSPECIFIED. ) ;
#49843 = CARTESIAN_POINT ( 'NONE',  ( 5.960721111146673579, -7.860635756378015593, 18.96073515164535195 ) ) ;
#49844 = CARTESIAN_POINT ( 'NONE',  ( 0.6008122571543325074, -45.35344805040789851, 18.83133825314251197 ) ) ;
#49845 = CIRCLE ( 'NONE', #18877, 7.400000000000021672 ) ;
#49846 = VERTEX_POINT ( 'NONE', #20874 ) ;
#49847 = TOROIDAL_SURFACE ( 'NONE', #7806, 15.71999999999999353, 0.2800000000000011924 ) ;
#49848 = CARTESIAN_POINT ( 'NONE',  ( 0.7242486021783874905, -19.12396628233026163, -45.22483140937365675 ) ) ;
#49849 = CARTESIAN_POINT ( 'NONE',  ( 4.956445790443988031, 0.000000000000000000, 0.000000000000000000 ) ) ;
#49850 = ORIENTED_EDGE ( 'NONE', *, *, #54275, .T. ) ;
#49851 = CARTESIAN_POINT ( 'NONE',  ( 4.967162193818130511, -42.96271701169384016, -3.259922920618186115 ) ) ;
#49852 = CARTESIAN_POINT ( 'NONE',  ( 1.227938101723756947, -4.762198645644731165, 42.65467462194916948 ) ) ;
#49853 = B_SPLINE_CURVE_WITH_KNOTS ( 'NONE', 3,
 ( #15455, #53630, #8654, #1633, #39588, #29849 ),
 .UNSPECIFIED., .F., .F.,
 ( 4, 2, 4 ),
 ( 1.823858501009600881E-17, 0.0002293319059085093849, 0.0004586638118170005009 ),
 .UNSPECIFIED. ) ;
#49854 =( BOUNDED_SURFACE ( )  B_SPLINE_SURFACE ( 3, 1, ( 
 ( #51428, #31419 ),
 ( #41458, #60520 ),
 ( #8215, #27642 ),
 ( #27334, #50517 ) ),
 .UNSPECIFIED., .F., .F., .F. ) 
 B_SPLINE_SURFACE_WITH_KNOTS ( ( 4, 4 ),
 ( 2, 2 ),
 ( 0.000000000000000000, 1.000000000000000000 ),
 ( 0.000000000000000000, 1.000000000000000000 ),
 .UNSPECIFIED. ) 
 GEOMETRIC_REPRESENTATION_ITEM ( )  RATIONAL_B_SPLINE_SURFACE ( (
 ( 1.000000000000000000, 1.000000000000000000),
 ( 0.7211978278499968642, 0.9934217856018975334),
 ( 0.7211978278499968642, 0.9934217856018975334),
 ( 1.000000000000000000, 1.000000000000000000) ) ) 
 REPRESENTATION_ITEM ( '' )  SURFACE ( )  );
#49855 = DIRECTION ( 'NONE',  ( -0.07836865515943411409, 0.3742079063795031302, -0.9240274869783747791 ) ) ;
#49856 = ORIENTED_EDGE ( 'NONE', *, *, #26437, .T. ) ;
#49857 = CARTESIAN_POINT ( 'NONE',  ( 0.8744876279028263033, -45.16590161814997373, -19.24555484778471026 ) ) ;
#49858 = FACE_OUTER_BOUND ( 'NONE', #49926, .T. ) ;
#49859 = ADVANCED_FACE ( 'NONE', ( #25264 ), #52509, .F. ) ;
#49860 = ORIENTED_EDGE ( 'NONE', *, *, #50212, .F. ) ;
#49861 = VECTOR ( 'NONE', #16318, 1000.000000000000000 ) ;
#49862 = EDGE_LOOP ( 'NONE', ( #33388, #1012, #37424, #59652 ) ) ;
#49863 = ADVANCED_FACE ( 'NONE', ( #34674 ), #27327, .T. ) ;
#49864 = VERTEX_POINT ( 'NONE', #48758 ) ;
#49865 = CARTESIAN_POINT ( 'NONE',  ( 0.1135584504625007929, 44.00383457693749989, 3.258004705455698868 ) ) ;
#49866 = B_SPLINE_CURVE_WITH_KNOTS ( 'NONE', 3,
 ( #18077, #9583, #42214, #9276 ),
 .UNSPECIFIED., .F., .F.,
 ( 4, 4 ),
 ( 4.207375016313971546E-17, 0.005004948556313856475 ),
 .UNSPECIFIED. ) ;
#49867 = VERTEX_POINT ( 'NONE', #44104 ) ;
#49868 = CARTESIAN_POINT ( 'NONE',  ( 4.975610109902397937, 45.11887670192763267, -18.88746601040027784 ) ) ;
#49869 = CARTESIAN_POINT ( 'NONE',  ( 0.9787464366903554369, -17.48005752276034741, -38.08912681975596826 ) ) ;
#49870 = ORIENTED_EDGE ( 'NONE', *, *, #15470, .T. ) ;
#49871 = CARTESIAN_POINT ( 'NONE',  ( -2.569797478183790229, 1.464172661883968551, 14.55946937464484492 ) ) ;
#49872 = STYLED_ITEM ( 'NONE', ( #36921 ), #34065 ) ;
#49873 =( BOUNDED_SURFACE ( )  B_SPLINE_SURFACE ( 3, 1, ( 
 ( #5810, #49672 ),
 ( #34068, #1130 ),
 ( #29337, #53438 ),
 ( #10242, #11171 ) ),
 .UNSPECIFIED., .F., .F., .F. ) 
 B_SPLINE_SURFACE_WITH_KNOTS ( ( 4, 4 ),
 ( 2, 2 ),
 ( 0.000000000000000000, 1.000000000000000000 ),
 ( 0.000000000000000000, 1.000000000000000000 ),
 .UNSPECIFIED. ) 
 GEOMETRIC_REPRESENTATION_ITEM ( )  RATIONAL_B_SPLINE_SURFACE ( (
 ( 1.000000000000000000, 1.000000000000000000),
 ( 0.7282232189291693025, 0.9929344683865674037),
 ( 0.7282232189291693025, 0.9929344683865674037),
 ( 1.000000000000000000, 1.000000000000000000) ) ) 
 REPRESENTATION_ITEM ( '' )  SURFACE ( )  );
#49874 = CARTESIAN_POINT ( 'NONE',  ( 4.962356264823609031, -24.61258717641066696, -34.13877780978592824 ) ) ;
#49875 = ORIENTED_EDGE ( 'NONE', *, *, #50830, .F. ) ;
#49876 = CARTESIAN_POINT ( 'NONE',  ( 0.1158403557922069033, 43.31768241345346837, -8.397541158637027436 ) ) ;
#49877 = EDGE_CURVE ( 'NONE', #6486, #33035, #1134, .T. ) ;
#49878 = CARTESIAN_POINT ( 'NONE',  ( 4.553261556744873317, -29.69864478935373242, -32.36556910513746743 ) ) ;
#49879 = CARTESIAN_POINT ( 'NONE',  ( 0.1102847568649952675, -30.42833243501171481, 30.55869130182056281 ) ) ;
#49880 = AXIS2_PLACEMENT_3D ( 'NONE', #43704, #33986, #53061 ) ;
#49881 = CARTESIAN_POINT ( 'NONE',  ( 0.9772918015221174759, 36.26796431592507020, 20.99932427792537126 ) ) ;
#49882 = ORIENTED_EDGE ( 'NONE', *, *, #27029, .F. ) ;
#49883 = ADVANCED_FACE ( 'NONE', ( #58440 ), #7677, .F. ) ;
#49884 = VERTEX_POINT ( 'NONE', #36224 ) ;
#49885 = CARTESIAN_POINT ( 'NONE',  ( 0.1129192098497455998, -6.563350895508677674, -43.63340707310831590 ) ) ;
#49886 = CARTESIAN_POINT ( 'NONE',  ( 5.896782393890504181, 5.952874097602427916, 19.21169895808557371 ) ) ;
#49887 = CARTESIAN_POINT ( 'NONE',  ( 2.009741617377216460, 13.91607796886164294, -41.78333222216257070 ) ) ;
#49888 = VERTEX_POINT ( 'NONE', #36532 ) ;
#49889 = CARTESIAN_POINT ( 'NONE',  ( 0.5549461598389366923, -42.87637096466922770, -10.33607799732926580 ) ) ;
#49890 = CARTESIAN_POINT ( 'NONE',  ( 0.6000166863083106206, -25.90381862410915659, 41.72308308835420831 ) ) ;
#49891 = DIRECTION ( 'NONE',  ( -1.000000000000000000, -1.836909530733554547E-16, -1.836909530733573529E-16 ) ) ;
#49892 = CARTESIAN_POINT ( 'NONE',  ( 4.956653778116971054, 42.88673967249130925, 21.75875759808722876 ) ) ;
#49893 = AXIS2_PLACEMENT_3D ( 'NONE', #3877, #56811, #57410 ) ;
#49894 = ORIENTED_EDGE ( 'NONE', *, *, #47893, .F. ) ;
#49895 = VERTEX_POINT ( 'NONE', #35612 ) ;
#49896 = CARTESIAN_POINT ( 'NONE',  ( 5.896782393890504181, 0.6784186533441023403, -20.10138888258239120 ) ) ;
#49897 = CARTESIAN_POINT ( 'NONE',  ( 0.8751705887134553219, 28.56654290188653178, -38.69254731947804515 ) ) ;
#49898 = CARTESIAN_POINT ( 'NONE',  ( 0.8760168074887076939, -19.22870327415273550, -44.09317760313745538 ) ) ;
#49899 = CARTESIAN_POINT ( 'NONE',  ( 4.962356264823608143, 39.61238188121388504, 14.21600504921214814 ) ) ;
#49900 = CARTESIAN_POINT ( 'NONE',  ( 0.1103878639767399417, 34.18336104662739672, -26.29099398937411536 ) ) ;
#49901 = CARTESIAN_POINT ( 'NONE',  ( 1.479689385636123067, -41.26970557461135058, -15.44005333710297379 ) ) ;
#49902 = EDGE_CURVE ( 'NONE', #8195, #759, #33384, .T. ) ;
#49903 = CARTESIAN_POINT ( 'NONE',  ( 5.958863334805807099, 16.28483817244739384, -12.49425770716470474 ) ) ;
#49904 = DIRECTION ( 'NONE',  ( -1.000000000000000000, -0.000000000000000000, -0.000000000000000000 ) ) ;
#49905 = CARTESIAN_POINT ( 'NONE',  ( 0.6023143664670691511, 12.70384782338089558, -46.39980466492348654 ) ) ;
#49906 = CARTESIAN_POINT ( 'NONE',  ( 0.6030672727741701600, -6.365785297725128800, 47.68443224372860101 ) ) ;
#49907 = CIRCLE ( 'NONE', #47911, 75.00000000000001421 ) ;
#49908 = CARTESIAN_POINT ( 'NONE',  ( 3.407937589446178528, -10.58239600294644944, 8.699069120706731439 ) ) ;
#49909 = CARTESIAN_POINT ( 'NONE',  ( 0.6029443199889047422, 41.15634887181838764, 26.78978516889554129 ) ) ;
#49910 = CARTESIAN_POINT ( 'NONE',  ( 0.2885700199627512785, -11.93479339212638379, -41.43179222486415370 ) ) ;
#49911 = B_SPLINE_CURVE_WITH_KNOTS ( 'NONE', 3,
 ( #54643, #20851, #35270, #16777 ),
 .UNSPECIFIED., .F., .F.,
 ( 4, 4 ),
 ( 0.000000000000000000, 0.005004741218457416270 ),
 .UNSPECIFIED. ) ;
#49912 = CARTESIAN_POINT ( 'NONE',  ( 0.3676999524040366896, 41.59822836379080968, -14.68121181363270367 ) ) ;
#49913 = CARTESIAN_POINT ( 'NONE',  ( 3.240649175237396484, -24.34849563854561083, 36.63899121888286459 ) ) ;
#49914 = CARTESIAN_POINT ( 'NONE',  ( -2.708315649062916552, 14.54141329178160191, 1.648584381067091931 ) ) ;
#49915 = CARTESIAN_POINT ( 'NONE',  ( 0.6023143664670691511, -6.019611522082996657, -47.72938193173970234 ) ) ;
#49916 = AXIS2_PLACEMENT_3D ( 'NONE', #34067, #53134, #28110 ) ;
#49917 = DIRECTION ( 'NONE',  ( -1.000000000000000000, -0.000000000000000000, -0.000000000000000000 ) ) ;
#49918 = CARTESIAN_POINT ( 'NONE',  ( 0.6067375320500720814, -43.97491060910871852, -18.98242280073610999 ) ) ;
#49919 = CARTESIAN_POINT ( 'NONE',  ( 0.6026777506516366456, 48.23490875577608250, 9.216288187723721492 ) ) ;
#49921 = VERTEX_POINT ( 'NONE', #6734 ) ;
#49920 = CARTESIAN_POINT ( 'NONE',  ( 0.8760168074887090262, 47.56749362999713782, -7.161346975773206225 ) ) ;
#49922 = ORIENTED_EDGE ( 'NONE', *, *, #48242, .F. ) ;
#49923 = CARTESIAN_POINT ( 'NONE',  ( 0.5980894510889457338, 46.65000524237070323, 11.77356634613333952 ) ) ;
#49924 = CARTESIAN_POINT ( 'NONE',  ( 5.896278296736517710, 3.339955767731749070, -19.83359965018905058 ) ) ;
#49925 = CARTESIAN_POINT ( 'NONE',  ( 4.549368137175248350, 38.59302160394725689, 18.79584381673547711 ) ) ;
#49926 = EDGE_LOOP ( 'NONE', ( #35676, #61627, #41896, #53452 ) ) ;
#49927 = ORIENTED_EDGE ( 'NONE', *, *, #40170, .F. ) ;
#49928 = CARTESIAN_POINT ( 'NONE',  ( 4.962356264823608143, 0.000000000000000000, 0.000000000000000000 ) ) ;
#49929 = CARTESIAN_POINT ( 'NONE',  ( 0.5980894510889457338, 33.52121017007826964, -34.51330645350367377 ) ) ;
#49930 = CARTESIAN_POINT ( 'NONE',  ( -6.077587904424778920, -18.89978312007031391, -3.687033958107209131 ) ) ;
#49931 = AXIS2_PLACEMENT_3D ( 'NONE', #7062, #21492, #31511 ) ;
#49932 = ORIENTED_EDGE ( 'NONE', *, *, #20584, .F. ) ;
#49933 = ORIENTED_EDGE ( 'NONE', *, *, #21648, .T. ) ;
#49934 = CARTESIAN_POINT ( 'NONE',  ( 4.956445790444005794, -40.23882117934059011, -24.46171131046819625 ) ) ;
#49935 = EDGE_CURVE ( 'NONE', #52878, #38564, #55596, .T. ) ;
#49936 = B_SPLINE_CURVE_WITH_KNOTS ( 'NONE', 3,
 ( #32482, #38430, #8652, #22767 ),
 .UNSPECIFIED., .F., .F.,
 ( 4, 4 ),
 ( 0.000000000000000000, 0.005004741218457418005 ),
 .UNSPECIFIED. ) ;
#49937 = VECTOR ( 'NONE', #40956, 1000.000000000000000 ) ;
#49938 = CARTESIAN_POINT ( 'NONE',  ( -2.569797478183790229, 14.24379821351257469, -3.352038560005768719 ) ) ;
#49939 = CARTESIAN_POINT ( 'NONE',  ( -6.016104459813374383, 2.454244026261090283, 18.68271063303495794 ) ) ;
#49940 = EDGE_CURVE ( 'NONE', #36534, #2574, #41507, .T. ) ;
#49941 = ORIENTED_EDGE ( 'NONE', *, *, #43840, .T. ) ;
#49942 = CARTESIAN_POINT ( 'NONE',  ( 0.8551540677456834771, 47.61725548905990735, 5.348818140991066450 ) ) ;
#49943 = B_SPLINE_CURVE_WITH_KNOTS ( 'NONE', 3,
 ( #59534, #26341, #16645, #2522 ),
 .UNSPECIFIED., .F., .F.,
 ( 4, 4 ),
 ( 1.734723475976807094E-17, 0.005004948556313820046 ),
 .UNSPECIFIED. ) ;
#49944 = FACE_OUTER_BOUND ( 'NONE', #37828, .T. ) ;
#49945 = EDGE_CURVE ( 'NONE', #57761, #44156, #51914, .T. ) ;
#49946 = CARTESIAN_POINT ( 'NONE',  ( 0.2940135542859015905, 43.96669230334707379, -3.629120636493694985 ) ) ;
#49947 = ORIENTED_EDGE ( 'NONE', *, *, #17507, .F. ) ;
#49948 = ORIENTED_EDGE ( 'NONE', *, *, #29281, .F. ) ;
#49949 = CARTESIAN_POINT ( 'NONE',  ( 43.00000000000000000, 0.000000000000000000, 0.000000000000000000 ) ) ;
#49950 = CARTESIAN_POINT ( 'NONE',  ( 3.680882792899936362, 44.99870212802617431, 16.63701193714004845 ) ) ;
#49951 = AXIS2_PLACEMENT_3D ( 'NONE', #48211, #5872, #30015 ) ;
#49952 = ORIENTED_EDGE ( 'NONE', *, *, #46218, .F. ) ;
#49953 = FACE_OUTER_BOUND ( 'NONE', #31431, .T. ) ;
#49954 = CARTESIAN_POINT ( 'NONE',  ( 2.624215991343620935, -32.93378783738872784, 34.92983774302955169 ) ) ;
#49955 = CARTESIAN_POINT ( 'NONE',  ( 3.894904216938897878, -43.82365964150300641, -3.407519347252721875 ) ) ;
#49956 = EDGE_CURVE ( 'NONE', #36178, #29343, #45322, .T. ) ;
#49957 = EDGE_LOOP ( 'NONE', ( #22968, #16285, #29400, #19106 ) ) ;
#49958 = CARTESIAN_POINT ( 'NONE',  ( 0.9757892942422827787, -30.37715353261971529, -30.30456399643821896 ) ) ;
#49959 = CARTESIAN_POINT ( 'NONE',  ( 0.6021448801613057400, -35.45754748828524328, 33.97504179162910276 ) ) ;
#49960 = CARTESIAN_POINT ( 'NONE',  ( -6.078726893082806448, -8.903615017412541022, 17.07394743140630666 ) ) ;
#49961 = CARTESIAN_POINT ( 'NONE',  ( 5.895596859100789899, 14.91916793517919970, -13.48875870250514630 ) ) ;
#49962 = CARTESIAN_POINT ( 'NONE',  ( 0.9757787079277449038, -21.42002160630794450, -37.17954582422758847 ) ) ;
#49963 = VERTEX_POINT ( 'NONE', #17109 ) ;
#49964 = CARTESIAN_POINT ( 'NONE',  ( 2.648799415243696664, -47.06172439114146044, -13.77358198225285157 ) ) ;
#49965 = DIRECTION ( 'NONE',  ( 1.000000000000000000, 0.000000000000000000, 0.000000000000000000 ) ) ;
#49966 = VERTEX_POINT ( 'NONE', #8003 ) ;
#49967 = CARTESIAN_POINT ( 'NONE',  ( 3.376099380956842921, 9.644725941468886177, 9.310620019419980409 ) ) ;
#49968 = CARTESIAN_POINT ( 'NONE',  ( 5.895596859100789899, -15.78235929336536536, 12.46777118604649814 ) ) ;
#49969 = LINE ( 'NONE', #1715, #5787 ) ;
#49970 = CARTESIAN_POINT ( 'NONE',  ( 0.5804410086790514622, 32.20888702807361881, 34.08969709851039909 ) ) ;
#49971 = CARTESIAN_POINT ( 'NONE',  ( 3.221118495291108719, 22.00098041526288029, 38.08829584569215143 ) ) ;
#49972 = VECTOR ( 'NONE', #35708, 1000.000000000000000 ) ;
#49973 =( REPRESENTATION_RELATIONSHIP ('NONE','NONE', #44881, #2385 ) REPRESENTATION_RELATIONSHIP_WITH_TRANSFORMATION ( #33370 )SHAPE_REPRESENTATION_RELATIONSHIP( ) );
#49974 = FACE_OUTER_BOUND ( 'NONE', #31945, .T. ) ;
#49975 =( BOUNDED_SURFACE ( )  B_SPLINE_SURFACE ( 3, 1, ( 
 ( #53223, #10332 ),
 ( #58221, #48532 ),
 ( #9702, #28812 ),
 ( #280, #19427 ) ),
 .UNSPECIFIED., .F., .F., .F. ) 
 B_SPLINE_SURFACE_WITH_KNOTS ( ( 4, 4 ),
 ( 2, 2 ),
 ( 0.000000000000000000, 1.000000000000000000 ),
 ( 0.000000000000000000, 1.000000000000000000 ),
 .UNSPECIFIED. ) 
 GEOMETRIC_REPRESENTATION_ITEM ( )  RATIONAL_B_SPLINE_SURFACE ( (
 ( 1.000000000000000000, 1.000000000000000000),
 ( 0.7211978278499968642, 0.9934217856018975334),
 ( 0.7211978278499968642, 0.9934217856018975334),
 ( 1.000000000000000000, 1.000000000000000000) ) ) 
 REPRESENTATION_ITEM ( '' )  SURFACE ( )  );
#49976 = CARTESIAN_POINT ( 'NONE',  ( 0.8744876279028263033, -47.70753782033983725, 11.59055156152357213 ) ) ;
#49977 = CARTESIAN_POINT ( 'NONE',  ( -6.078726893082806448, -19.21666810860935470, 1.230328440814298041 ) ) ;
#49978 = CARTESIAN_POINT ( 'NONE',  ( 5.896782393890504181, -18.51935720350340731, 7.845985957612901629 ) ) ;
#49979 = CARTESIAN_POINT ( 'NONE',  ( 0.9775691876210974574, 14.70917054435504312, 39.24250260733978735 ) ) ;
#49980 = EDGE_LOOP ( 'NONE', ( #33460, #21814, #49226, #31512 ) ) ;
#49981 = VECTOR ( 'NONE', #57091, 1000.000000000000000 ) ;
#49982 = ADVANCED_FACE ( 'NONE', ( #2364 ), #31298, .F. ) ;
#49983 = CARTESIAN_POINT ( 'NONE',  ( 0.8753041380234524160, -39.87785955339003863, -28.65125905284232388 ) ) ;
#49984 = CARTESIAN_POINT ( 'NONE',  ( -6.078726893082806448, -14.66019907464911043, 12.48489504803213812 ) ) ;
#49985 = B_SPLINE_CURVE_WITH_KNOTS ( 'NONE', 3,
 ( #49327, #50561, #2632, #17372, #49636, #1697 ),
 .UNSPECIFIED., .F., .F.,
 ( 4, 2, 4 ),
 ( 3.529906531158615134E-18, 0.0002445244328975344750, 0.0004890488657950654806 ),
 .UNSPECIFIED. ) ;
#49986 = DIRECTION ( 'NONE',  ( 0.000000000000000000, 0.7071067811865382469, 0.7071067811865566766 ) ) ;
#49987 = CARTESIAN_POINT ( 'NONE',  ( 0.5817217712918323347, -34.47346716911549436, -31.79331714917915619 ) ) ;
#49988 = CARTESIAN_POINT ( 'NONE',  ( 3.678748215320120973, 45.86478482322198857, -17.17656331805143921 ) ) ;
#49989 = EDGE_CURVE ( 'NONE', #53012, #39870, #58658, .T. ) ;
#49990 =( NAMED_UNIT ( * ) SI_UNIT ( $, .STERADIAN. ) SOLID_ANGLE_UNIT ( ) );
#49991 = CARTESIAN_POINT ( 'NONE',  ( 0.3676999524040323597, 14.45783756353398175, 41.67639039443440652 ) ) ;
#49992 = CARTESIAN_POINT ( 'NONE',  ( 0.6009452777970412107, 41.44251326863928853, -24.43074291040862533 ) ) ;
#49993 = EDGE_CURVE ( 'NONE', #38699, #53425, #33296, .T. ) ;
#49994 = CARTESIAN_POINT ( 'NONE',  ( 0.2224561200757622370, -6.380320192202297847, 42.64482917976808096 ) ) ;
#49996 = ORIENTED_EDGE ( 'NONE', *, *, #12762, .T. ) ;
#49995 = CARTESIAN_POINT ( 'NONE',  ( 4.956445790444041322, 46.03642002599030292, -9.908889005849065512 ) ) ;
#49997 = ORIENTED_EDGE ( 'NONE', *, *, #34000, .T. ) ;
#49999 = CIRCLE ( 'NONE', #54985, 42.92674063221959813 ) ;
#49998 = CARTESIAN_POINT ( 'NONE',  ( 5.965394784446460541, 17.78272165951801398, -10.25014670152096485 ) ) ;
#50000 = DIRECTION ( 'NONE',  ( 0.09722883295013594329, -0.9952333609815530169, 0.007557197398263628546 ) ) ;
#50001 = CARTESIAN_POINT ( 'NONE',  ( 3.376099380956838925, -9.627698927086731473, -9.328225822815406687 ) ) ;
#50002 = EDGE_LOOP ( 'NONE', ( #15751, #25393, #59483, #33529 ) ) ;
#50003 = CARTESIAN_POINT ( 'NONE',  ( 5.959547316686252039, 5.315863417546055736, 19.82530672674364070 ) ) ;
#50004 = CARTESIAN_POINT ( 'NONE',  ( 0.5786265663353153954, 44.52624106864143982, 17.66171603226096920 ) ) ;
#50005 = CARTESIAN_POINT ( 'NONE',  ( 45.00000000000001421, 1.592040838891559293E-15, -13.00000000000000178 ) ) ;
#50006 = B_SPLINE_CURVE_WITH_KNOTS ( 'NONE', 3,
 ( #56513, #27714, #7982, #3572 ),
 .UNSPECIFIED., .F., .F.,
 ( 4, 4 ),
 ( 0.000000000000000000, 0.004446090762761341700 ),
 .UNSPECIFIED. ) ;
#50007 = VERTEX_POINT ( 'NONE', #7361 ) ;
#50008 = ORIENTED_EDGE ( 'NONE', *, *, #58680, .F. ) ;
#50009 = CARTESIAN_POINT ( 'NONE',  ( 0.3622758884714600280, 37.74294673546586409, -20.83792692158932525 ) ) ;
#50010 = EDGE_CURVE ( 'NONE', #36259, #10386, #37746, .T. ) ;
#50011 = B_SPLINE_CURVE_WITH_KNOTS ( 'NONE', 3,
 ( #5047, #49216, #15726, #53898 ),
 .UNSPECIFIED., .F., .F.,
 ( 4, 4 ),
 ( 0.000000000000000000, 0.005013413432710148512 ),
 .UNSPECIFIED. ) ;
#50012 = CARTESIAN_POINT ( 'NONE',  ( -6.079354080745853928, -18.90111140843031379, 3.679802002046783205 ) ) ;
#50013 = CARTESIAN_POINT ( 'NONE',  ( 3.238741278300274917, -3.793425828152354295, -42.82436441900172497 ) ) ;
#50014 = ORIENTED_EDGE ( 'NONE', *, *, #8765, .T. ) ;
#50015 = ORIENTED_EDGE ( 'NONE', *, *, #55853, .T. ) ;
#50016 = CARTESIAN_POINT ( 'NONE',  ( 0.1081432562775997697, -0.4234896101214557507, 43.12249629849792854 ) ) ;
#50017 = EDGE_CURVE ( 'NONE', #57409, #56877, #2674, .T. ) ;
#50018 = CARTESIAN_POINT ( 'NONE',  ( 0.8751705887134553219, -11.58504748649232496, 46.67919521768867241 ) ) ;
#50019 = ORIENTED_EDGE ( 'NONE', *, *, #36566, .F. ) ;
#50020 = CARTESIAN_POINT ( 'NONE',  ( 0.8560838555295158248, -29.58154842764465542, -36.40473632241614155 ) ) ;
#50021 = LINE ( 'NONE', #45644, #19016 ) ;
#50022 = ORIENTED_EDGE ( 'NONE', *, *, #27900, .F. ) ;
#50023 = CARTESIAN_POINT ( 'NONE',  ( 0.5824936645240080813, -35.02382170666601979, 31.18605605234460398 ) ) ;
#50024 = CARTESIAN_POINT ( 'NONE',  ( 4.962356264823608143, 12.88441948660223169, -40.06528837230067097 ) ) ;
#50025 = ORIENTED_EDGE ( 'NONE', *, *, #31544, .F. ) ;
#50026 = CARTESIAN_POINT ( 'NONE',  ( 0.5998501479064708430, 23.59887241503295741, 41.92175333043627461 ) ) ;
#50027 = CARTESIAN_POINT ( 'NONE',  ( 5.981074661064941900, 12.50143471347281299, -16.27808421740013856 ) ) ;
#50028 = CARTESIAN_POINT ( 'NONE',  ( 4.975610109902397937, 48.43414999183889336, 6.825138951393308950 ) ) ;
#50029 = CARTESIAN_POINT ( 'NONE',  ( 5.981074661064941900, -18.96560215432023000, 7.846517100474483364 ) ) ;
#50030 = EDGE_CURVE ( 'NONE', #41301, #50843, #28063, .T. ) ;
#50031 = B_SPLINE_CURVE_WITH_KNOTS ( 'NONE', 3,
 ( #22930, #60192, #3478, #6385 ),
 .UNSPECIFIED., .F., .F.,
 ( 4, 4 ),
 ( 0.000000000000000000, 0.005014147105413695182 ),
 .UNSPECIFIED. ) ;
#50032 = ORIENTED_EDGE ( 'NONE', *, *, #8314, .F. ) ;
#50033 = CARTESIAN_POINT ( 'NONE',  ( -31.74999999999995737, 0.000000000000000000, 0.000000000000000000 ) ) ;
#50034 = CARTESIAN_POINT ( 'NONE',  ( 0.1158403557922069033, 39.77089686883259390, -19.11062713341717156 ) ) ;
#50035 = VERTEX_POINT ( 'NONE', #7678 ) ;
#50036 = CARTESIAN_POINT ( 'NONE',  ( -6.079354080745853928, 12.00682274379669146, 15.05420747987779606 ) ) ;
#50037 = VECTOR ( 'NONE', #36401, 1000.000000000000000 ) ;
#50038 = VERTEX_POINT ( 'NONE', #61229 ) ;
#50039 = CARTESIAN_POINT ( 'NONE',  ( 0.6846871229502932144, 13.23224427737893549, -46.04462816497473199 ) ) ;
#50040 = EDGE_LOOP ( 'NONE', ( #52401, #14973, #5194, #10833 ) ) ;
#50041 = CARTESIAN_POINT ( 'NONE',  ( 0.9972139404380282457, 26.64066783422334694, 33.63772329383390769 ) ) ;
#50042 = CARTESIAN_POINT ( 'NONE',  ( 0.9780106845699465534, 24.60614105318022737, 33.92446121792414004 ) ) ;
#50043 = AXIS2_PLACEMENT_3D ( 'NONE', #59579, #11684, #17308 ) ;
#50044 = CARTESIAN_POINT ( 'NONE',  ( 0.1097557419366048670, -26.07515889977844026, 34.34829179474790095 ) ) ;
#50045 = ORIENTED_EDGE ( 'NONE', *, *, #49263, .T. ) ;
#50046 = CARTESIAN_POINT ( 'NONE',  ( -6.015611763856276717, 17.41126425312547710, -7.205255340944423992 ) ) ;
#50047 = DIRECTION ( 'NONE',  ( 0.000000000000000000, -0.4999999999999993339, 0.8660254037844390407 ) ) ;
#50048 = CARTESIAN_POINT ( 'NONE',  ( 4.322998006666179727, 39.32552843303813006, 27.50295597456465302 ) ) ;
#50049 = EDGE_LOOP ( 'NONE', ( #38976, #4905, #50708, #2180 ) ) ;
#50050 = ORIENTED_EDGE ( 'NONE', *, *, #45334, .F. ) ;
#50051 =( BOUNDED_SURFACE ( )  B_SPLINE_SURFACE ( 3, 1, ( 
 ( #41929, #22798 ),
 ( #13410, #32515 ),
 ( #51589, #27803 ),
 ( #37535, #18726 ) ),
 .UNSPECIFIED., .F., .F., .F. ) 
 B_SPLINE_SURFACE_WITH_KNOTS ( ( 4, 4 ),
 ( 2, 2 ),
 ( 0.000000000000000000, 1.000000000000000000 ),
 ( 0.000000000000000000, 1.000000000000000000 ),
 .UNSPECIFIED. ) 
 GEOMETRIC_REPRESENTATION_ITEM ( )  RATIONAL_B_SPLINE_SURFACE ( (
 ( 1.000000000000000000, 1.000000000000000000),
 ( 0.9953390228620291325, 0.8624445117760984880),
 ( 0.9953390228620291325, 0.8624445117760984880),
 ( 1.000000000000000000, 1.000000000000000000) ) ) 
 REPRESENTATION_ITEM ( '' )  SURFACE ( )  );
#50052 = CARTESIAN_POINT ( 'NONE',  ( 0.7242486021783802741, -38.85568807781807266, -30.02077557914319428 ) ) ;
#50053 = CARTESIAN_POINT ( 'NONE',  ( 4.956653778116973719, 31.29546495791849736, 36.51451553856430365 ) ) ;
#50054 = CARTESIAN_POINT ( 'NONE',  ( 4.975801465491694664, 26.14269827151623105, 40.15204426031542795 ) ) ;
#50055 = CARTESIAN_POINT ( 'NONE',  ( 4.999999999999998224, -2.650000000000277911, 80.00000000000000000 ) ) ;
#50056 = CARTESIAN_POINT ( 'NONE',  ( 0.6067099128993206358, -44.51753430581926096, -17.67241243535530870 ) ) ;
#50057 = CARTESIAN_POINT ( 'NONE',  ( 4.549368137175248350, -8.582197505784124658, -42.06008734272393212 ) ) ;
#50058 = VERTEX_POINT ( 'NONE', #56532 ) ;
#50059 = CARTESIAN_POINT ( 'NONE',  ( 0.1092565886968784455, 37.19081526480825062, -21.83052579204423793 ) ) ;
#50060 = CARTESIAN_POINT ( 'NONE',  ( 2.526464513654346433, 39.22765990515345891, -17.56107808841265694 ) ) ;
#50061 = ORIENTED_EDGE ( 'NONE', *, *, #41986, .F. ) ;
#50062 = EDGE_CURVE ( 'NONE', #52610, #30576, #24287, .T. ) ;
#50063 = CARTESIAN_POINT ( 'NONE',  ( 0.5839879327111907603, -44.21534283185616943, 18.41291455875288108 ) ) ;
#50064 = CARTESIAN_POINT ( 'NONE',  ( 0.9722240741986377666, 42.90442369863401950, 0.5819399500321930097 ) ) ;
#50065 = CARTESIAN_POINT ( 'NONE',  ( 0.1157991065609915576, -42.70166050063943430, 11.11353031335356789 ) ) ;
#50066 = CARTESIAN_POINT ( 'NONE',  ( 0.8753041380234524160, -24.68967207985825141, 42.44476905888459584 ) ) ;
#50067 = CARTESIAN_POINT ( 'NONE',  ( 4.975801465491695552, -9.906103548667894998, -46.87746200127453022 ) ) ;
#50068 = EDGE_CURVE ( 'NONE', #40146, #2015, #42171, .T. ) ;
#50069 = CARTESIAN_POINT ( 'NONE',  ( 0.8551540677456834771, -11.51835730326512675, 46.51172240253117707 ) ) ;
#50070 = CARTESIAN_POINT ( 'NONE',  ( 0.5807400328401574052, -34.25275203086211917, -33.48217046439147282 ) ) ;
#50071 = CARTESIAN_POINT ( 'NONE',  ( 0.5807400328401574052, 6.791881299635576852, 47.41494605191445544 ) ) ;
#50072 = EDGE_CURVE ( 'NONE', #24678, #23496, #60116, .T. ) ;
#50073 = AXIS2_PLACEMENT_3D ( 'NONE', #23358, #8305, #18662 ) ;
#50074 = CARTESIAN_POINT ( 'NONE',  ( 1.227938101723757836, -10.28900963485409292, 41.66816631169188412 ) ) ;
#50075 = EDGE_CURVE ( 'NONE', #35725, #4600, #37155, .T. ) ;
#50076 = DIRECTION ( 'NONE',  ( 0.000000000000000000, -0.7071067811865487940, 0.7071067811865461294 ) ) ;
#50077 = EDGE_CURVE ( 'NONE', #9258, #23834, #6272, .T. ) ;
#50078 = PRESENTATION_STYLE_ASSIGNMENT (( #44786 ) ) ;
#50079 = CARTESIAN_POINT ( 'NONE',  ( 0.3676999524040366896, -22.15802448780013378, 38.14410221935873579 ) ) ;
#50080 = CARTESIAN_POINT ( 'NONE',  ( 0.9730545539215883499, 11.59290486963506517, 41.31259007387235727 ) ) ;
#50081 = CARTESIAN_POINT ( 'NONE',  ( 1.827326673878744590, -17.60663982372562941, 39.28486782721036263 ) ) ;
#50082 = B_SPLINE_CURVE_WITH_KNOTS ( 'NONE', 3,
 ( #3093, #40741, #16599, #59489 ),
 .UNSPECIFIED., .F., .F.,
 ( 4, 4 ),
 ( 0.000000000000000000, 0.005013413432710144176 ),
 .UNSPECIFIED. ) ;
#50083 = VECTOR ( 'NONE', #6601, 1000.000000000000000 ) ;
#50084 = EDGE_CURVE ( 'NONE', #19512, #32528, #1314, .T. ) ;
#50085 = ORIENTED_EDGE ( 'NONE', *, *, #24690, .T. ) ;
#50086 = CARTESIAN_POINT ( 'NONE',  ( 0.1100053167205930910, 10.98799238780951271, -41.70112744323659371 ) ) ;
#50087 = EDGE_CURVE ( 'NONE', #25604, #43021, #28731, .T. ) ;
#50088 = CARTESIAN_POINT ( 'NONE',  ( 0.1073791018717578927, 43.12183934961191056, 0.4849339620934667305 ) ) ;
#50089 = CARTESIAN_POINT ( 'NONE',  ( 0.9756354156337453398, -39.59221474545851294, -16.54067710771401778 ) ) ;
#50090 = FACE_OUTER_BOUND ( 'NONE', #25231, .T. ) ;
#50091 = CARTESIAN_POINT ( 'NONE',  ( 0.1092355843206037486, -41.73183925352188339, 10.87081649985017151 ) ) ;
#50092 = ORIENTED_EDGE ( 'NONE', *, *, #3724, .F. ) ;
#50093 = CARTESIAN_POINT ( 'NONE',  ( 0.6026777506516367566, 27.95217787757266237, -40.37600949249141991 ) ) ;
#50094 = CARTESIAN_POINT ( 'NONE',  ( 0.6008123274975391004, -14.38933995680775091, 46.95211866109849552 ) ) ;
#50095 = ORIENTED_EDGE ( 'NONE', *, *, #3340, .F. ) ;
#50096 = CARTESIAN_POINT ( 'NONE',  ( 0.9968887458511667132, 41.27232779986120192, 11.73947777183236063 ) ) ;
#50097 = ORIENTED_EDGE ( 'NONE', *, *, #13106, .F. ) ;
#50098 = LINE ( 'NONE', #21591, #45890 ) ;
#50099 = CARTESIAN_POINT ( 'NONE',  ( 0.6031356755773454870, -29.28593560184460287, 38.16621646312157878 ) ) ;
#50100 = VERTEX_POINT ( 'NONE', #28650 ) ;
#50101 = DIRECTION ( 'NONE',  ( -1.718001593797181987E-16, 1.000000000000000000, 0.000000000000000000 ) ) ;
#50102 = EDGE_LOOP ( 'NONE', ( #56089, #53628, #1442, #61860 ) ) ;
#50103 = CARTESIAN_POINT ( 'NONE',  ( 5.838029081930957709, 42.16639215765243165, 21.28521624414438662 ) ) ;
#50104 = CARTESIAN_POINT ( 'NONE',  ( 0.1098349054025746507, -26.08296594991515960, -34.34238705454293950 ) ) ;
#50105 = ORIENTED_EDGE ( 'NONE', *, *, #25917, .T. ) ;
#50106 = B_SPLINE_CURVE_WITH_KNOTS ( 'NONE', 3,
 ( #20197, #48994, #53368, #25485, #5738, #58066 ),
 .UNSPECIFIED., .F., .F.,
 ( 4, 2, 4 ),
 ( 1.738108305489988542E-18, 0.0002291966416970806777, 0.0004583932833941596206 ),
 .UNSPECIFIED. ) ;
#50107 = EDGE_CURVE ( 'NONE', #28142, #59626, #9051, .T. ) ;
#50108 = ORIENTED_EDGE ( 'NONE', *, *, #18626, .F. ) ;
#50109 = CARTESIAN_POINT ( 'NONE',  ( 0.8554163680231738898, 21.74163052365332760, 41.57531689939074226 ) ) ;
#50110 = ORIENTED_EDGE ( 'NONE', *, *, #21779, .F. ) ;
#50111 = CARTESIAN_POINT ( 'NONE',  ( 0.5819845079324652559, -38.27312975753793722, -28.79567599618802021 ) ) ;
#50112 = EDGE_CURVE ( 'NONE', #18589, #45486, #36702, .T. ) ;
#50113 = VERTEX_POINT ( 'NONE', #4204 ) ;
#50114 = ORIENTED_EDGE ( 'NONE', *, *, #11696, .F. ) ;
#50115 = CARTESIAN_POINT ( 'NONE',  ( 0.9757954354143122400, -4.033171854401937560E-17, -42.90846090505964128 ) ) ;
#50116 = CARTESIAN_POINT ( 'NONE',  ( 0.7044674535452954967, 41.61193891978883386, -26.08158856639429146 ) ) ;
#50117 = CARTESIAN_POINT ( 'NONE',  ( 2.301430502907645614, -25.12309903330049110, 40.93949994354142063 ) ) ;
#50118 = CARTESIAN_POINT ( 'NONE',  ( 0.1103744047535531458, -16.53879706351798973, 39.82693656558404882 ) ) ;
#50119 = CARTESIAN_POINT ( 'NONE',  ( 5.959547316686252039, -14.51632612601518879, -14.51128755440536366 ) ) ;
#50120 = EDGE_LOOP ( 'NONE', ( #25695, #34007, #12125, #34481 ) ) ;
#50121 = LINE ( 'NONE', #43051, #28869 ) ;
#50122 = CARTESIAN_POINT ( 'NONE',  ( 5.965394784446458765, 19.82223131420054685, -5.326334832595444269 ) ) ;
#50123 = CARTESIAN_POINT ( 'NONE',  ( 0.8753041380234524160, -48.80600061351578489, -5.395612290229641950 ) ) ;
#50124 = ORIENTED_EDGE ( 'NONE', *, *, #2597, .F. ) ;
#50125 = VERTEX_POINT ( 'NONE', #8295 ) ;
#50126 = VECTOR ( 'NONE', #15793, 1000.000000000000000 ) ;
#50127 = CARTESIAN_POINT ( 'NONE',  ( 0.9762797500689124330, 28.76866969767982951, 30.47438972336447804 ) ) ;
#50128 = CARTESIAN_POINT ( 'NONE',  ( 5.981074661064941900, 17.77058762078877763, -10.26976685693804647 ) ) ;
#50129 = ORIENTED_EDGE ( 'NONE', *, *, #9282, .T. ) ;
#50130 = CARTESIAN_POINT ( 'NONE',  ( 0.8744876279028306332, -43.20725972823464645, -23.31271664041680580 ) ) ;
#50131 = DIRECTION ( 'NONE',  ( 0.000000000000000000, 0.000000000000000000, 1.000000000000000000 ) ) ;
#50132 = CARTESIAN_POINT ( 'NONE',  ( 0.8751705887134553219, -17.57879340691572878, 44.76769609654206050 ) ) ;
#50133 =( BOUNDED_SURFACE ( )  B_SPLINE_SURFACE ( 3, 1, ( 
 ( #33247, #28515 ),
 ( #42963, #41728 ),
 ( #13209, #27604 ),
 ( #46729, #621 ) ),
 .UNSPECIFIED., .F., .F., .F. ) 
 B_SPLINE_SURFACE_WITH_KNOTS ( ( 4, 4 ),
 ( 2, 2 ),
 ( 0.000000000000000000, 1.000000000000000000 ),
 ( 0.000000000000000000, 1.000000000000000000 ),
 .UNSPECIFIED. ) 
 GEOMETRIC_REPRESENTATION_ITEM ( )  RATIONAL_B_SPLINE_SURFACE ( (
 ( 1.000000000000000000, 1.000000000000000000),
 ( 0.9953040768229005630, 0.8617119497784937465),
 ( 0.9953040768229005630, 0.8617119497784937465),
 ( 1.000000000000000000, 1.000000000000000000) ) ) 
 REPRESENTATION_ITEM ( '' )  SURFACE ( )  );
#50134 = VERTEX_POINT ( 'NONE', #27415 ) ;
#50135 = CARTESIAN_POINT ( 'NONE',  ( 3.376099380956842921, -5.222100608647028075, 12.34658045230481527 ) ) ;
#50136 = VERTEX_POINT ( 'NONE', #46545 ) ;
#50137 = EDGE_CURVE ( 'NONE', #26923, #44899, #54626, .T. ) ;
#50138 = CARTESIAN_POINT ( 'NONE',  ( 0.5980271706414734822, -47.32398142236193195, 13.13354579607525352 ) ) ;
#50139 = CARTESIAN_POINT ( 'NONE',  ( 4.553261556744875094, 0.000000000000000000, 0.000000000000000000 ) ) ;
#50140 = FACE_OUTER_BOUND ( 'NONE', #7065, .T. ) ;
#50141 = EDGE_CURVE ( 'NONE', #28691, #20504, #287, .T. ) ;
#50142 = CARTESIAN_POINT ( 'NONE',  ( 4.956445790444035104, 39.12691469764034480, -26.20348443209818967 ) ) ;
#50143 = ORIENTED_EDGE ( 'NONE', *, *, #30712, .F. ) ;
#50144 = CARTESIAN_POINT ( 'NONE',  ( 0.9757787079277456810, 21.48842038179486380, -37.14005577278797432 ) ) ;
#50145 = CARTESIAN_POINT ( 'NONE',  ( 1.231276596079881047, 15.85305549123227564, -38.80666698661426040 ) ) ;
#50146 = EDGE_CURVE ( 'NONE', #59804, #13656, #24261, .T. ) ;
#50147 = CARTESIAN_POINT ( 'NONE',  ( 0.1310142868023675411, -39.59283406808317807, -17.08943085418572139 ) ) ;
#50148 = ADVANCED_FACE ( 'NONE', ( #10793 ), #9343, .T. ) ;
#50149 =( BOUNDED_SURFACE ( )  B_SPLINE_SURFACE ( 3, 1, ( 
 ( #54279, #17336 ),
 ( #40549, #22339 ),
 ( #12340, #30484 ),
 ( #45547, #2910 ) ),
 .UNSPECIFIED., .F., .F., .F. ) 
 B_SPLINE_SURFACE_WITH_KNOTS ( ( 4, 4 ),
 ( 2, 2 ),
 ( 0.000000000000000000, 1.000000000000000000 ),
 ( 0.000000000000000000, 1.000000000000000000 ),
 .UNSPECIFIED. ) 
 GEOMETRIC_REPRESENTATION_ITEM ( )  RATIONAL_B_SPLINE_SURFACE ( (
 ( 1.000000000000000000, 1.000000000000000000),
 ( 0.9729067724841187204, 0.9999501103223794596),
 ( 0.9729067724841187204, 0.9999501103223794596),
 ( 1.000000000000000000, 1.000000000000000000) ) ) 
 REPRESENTATION_ITEM ( '' )  SURFACE ( )  );
#50150 = CARTESIAN_POINT ( 'NONE',  ( 0.1101816497532063371, 21.44450189183869071, -37.41460501058194410 ) ) ;
#50151 = EDGE_CURVE ( 'NONE', #55958, #9272, #59074, .T. ) ;
#50152 = DIRECTION ( 'NONE',  ( 1.000000000000000000, 0.000000000000000000, 0.000000000000000000 ) ) ;
#50153 = CARTESIAN_POINT ( 'NONE',  ( 0.5806925824938502512, 32.20670061096268455, -34.08739940358283604 ) ) ;
#50154 =( BOUNDED_SURFACE ( )  B_SPLINE_SURFACE ( 3, 1, ( 
 ( #24281, #28668 ),
 ( #57451, #47793 ),
 ( #4528, #140 ),
 ( #52466, #23364 ) ),
 .UNSPECIFIED., .F., .F., .F. ) 
 B_SPLINE_SURFACE_WITH_KNOTS ( ( 4, 4 ),
 ( 2, 2 ),
 ( 0.000000000000000000, 1.000000000000000000 ),
 ( 0.000000000000000000, 1.000000000000000000 ),
 .UNSPECIFIED. ) 
 GEOMETRIC_REPRESENTATION_ITEM ( )  RATIONAL_B_SPLINE_SURFACE ( (
 ( 1.000000000000000000, 1.000000000000000000),
 ( 0.7211978278499968642, 0.9934217856018975334),
 ( 0.7211978278499968642, 0.9934217856018975334),
 ( 1.000000000000000000, 1.000000000000000000) ) ) 
 REPRESENTATION_ITEM ( '' )  SURFACE ( )  );
#50155 = FACE_OUTER_BOUND ( 'NONE', #1785, .T. ) ;
#50156 = LINE ( 'NONE', #21646, #13162 ) ;
#50157 = CARTESIAN_POINT ( 'NONE',  ( 4.975610109902397937, -32.45573888811652807, 36.59336579715199633 ) ) ;
#50158 = CARTESIAN_POINT ( 'NONE',  ( 5.910764540655177868, -19.39351348817910647, -5.328496321944700576 ) ) ;
#50159 = FACE_OUTER_BOUND ( 'NONE', #41354, .T. ) ;
#50160 = ORIENTED_EDGE ( 'NONE', *, *, #21077, .F. ) ;
#50161 = CARTESIAN_POINT ( 'NONE',  ( 3.407937589446174087, 13.69123696618924413, 0.4592810312472457857 ) ) ;
#50162 = CARTESIAN_POINT ( 'NONE',  ( 0.5839254288179548391, 46.24038938821434641, 12.48406597209056024 ) ) ;
#50163 = CARTESIAN_POINT ( 'NONE',  ( 1.657374760986086271, -42.28389365164147051, 12.36781245446895738 ) ) ;
#50164 = ORIENTED_EDGE ( 'NONE', *, *, #32774, .T. ) ;
#50165 = CARTESIAN_POINT ( 'NONE',  ( 2.624215991343608501, -11.05657803851013021, -46.71702075422663114 ) ) ;
#50166 = CARTESIAN_POINT ( 'NONE',  ( 0.5997462898726536595, 10.41743419021343087, -47.98988117339822423 ) ) ;
#50167 = CARTESIAN_POINT ( 'NONE',  ( 0.6031356755773454870, -12.45114731045998369, -46.46821530722335325 ) ) ;
#50168 = VECTOR ( 'NONE', #5524, 1000.000000000000227 ) ;
#50170 = EDGE_LOOP ( 'NONE', ( #4095, #59516, #24217, #48104 ) ) ;
#50169 = VECTOR ( 'NONE', #38236, 1000.000000000000114 ) ;
#50171 = CARTESIAN_POINT ( 'NONE',  ( 0.8551540677456739292, -28.44084013485093365, -38.56334384152459904 ) ) ;
#50172 = CARTESIAN_POINT ( 'NONE',  ( 0.9757787079277443487, -41.43615150473004860, -11.14366644276454466 ) ) ;
#50173 = ORIENTED_EDGE ( 'NONE', *, *, #1822, .T. ) ;
#50174 = VERTEX_POINT ( 'NONE', #10170 ) ;
#50175 = ORIENTED_EDGE ( 'NONE', *, *, #18249, .T. ) ;
#50176 = CARTESIAN_POINT ( 'NONE',  ( 0.9756008150404611445, -5.459718823765815188, 42.55970871350804430 ) ) ;
#50177 = EDGE_LOOP ( 'NONE', ( #28074, #37514 ) ) ;
#50178 = CARTESIAN_POINT ( 'NONE',  ( -6.063463321072278589, -8.920783457832412111, 17.06575738072979576 ) ) ;
#50179 = ORIENTED_EDGE ( 'NONE', *, *, #3035, .T. ) ;
#50180 = CARTESIAN_POINT ( 'NONE',  ( 0.5839879327111912044, 0.09083573661711773217, 47.89596760851024015 ) ) ;
#50181 = B_SPLINE_CURVE_WITH_KNOTS ( 'NONE', 3,
 ( #13050, #23053, #9243, #32144, #13979, #55608, #42180, #56542, #18360, #51222, #13659, #32764, #4214, #61539, #51841, #47172 ),
 .UNSPECIFIED., .F., .F.,
 ( 4, 3, 3, 3, 3, 4 ),
 ( 2.194378057379452319E-17, 0.0002618515315864391037, 0.0003927756766341941965, 0.0005236998216950568058, 0.0007855159896329857788, 0.001047349442285925268 ),
 .UNSPECIFIED. ) ;
#50182 = EDGE_CURVE ( 'NONE', #31310, #39191, #6022, .T. ) ;
#50183 = CARTESIAN_POINT ( 'NONE',  ( 0.6000166863083090663, 37.73145429715492583, 31.43502566135683551 ) ) ;
#50184 = EDGE_LOOP ( 'NONE', ( #4755, #31005, #61926, #21540 ) ) ;
#50185 = CARTESIAN_POINT ( 'NONE',  ( 0.1155031312995260795, 43.34236963370094031, -8.269257951439607623 ) ) ;
#50186 = CARTESIAN_POINT ( 'NONE',  ( 48.86838059950356694, 12.32200637394865161, -2.116332808070153337 ) ) ;
#50187 = CARTESIAN_POINT ( 'NONE',  ( 0.5806925824938499181, -30.69245420804209701, 35.45695442407318154 ) ) ;
#50188 = VERTEX_POINT ( 'NONE', #28964 ) ;
#50189 = VERTEX_POINT ( 'NONE', #58673 ) ;
#50190 = CARTESIAN_POINT ( 'NONE',  ( 0.9740398440564310700, -42.90647580953695694, 0.4145941695171530550 ) ) ;
#50191 = CARTESIAN_POINT ( 'NONE',  ( 5.895596859100789899, 5.955534046174260965, 19.21092911436994299 ) ) ;
#50192 = CARTESIAN_POINT ( 'NONE',  ( 0.7246131072078578761, -47.79072675905350565, 5.464103862700703473 ) ) ;
#50193 = ORIENTED_EDGE ( 'NONE', *, *, #9907, .T. ) ;
#50194 = FACE_OUTER_BOUND ( 'NONE', #31641, .T. ) ;
#50195 = CARTESIAN_POINT ( 'NONE',  ( 1.227938101723748288, -37.58536632582793402, 20.72293514920737323 ) ) ;
#50196 = CARTESIAN_POINT ( 'NONE',  ( 4.960156602257182357, -43.79161740034487593, 15.40604254112629157 ) ) ;
#50197 = ORIENTED_EDGE ( 'NONE', *, *, #3485, .T. ) ;
#50198 = VERTEX_POINT ( 'NONE', #53067 ) ;
#50199 = CARTESIAN_POINT ( 'NONE',  ( 4.960156602257181468, 25.36362146861438660, -38.88108289790832117 ) ) ;
#50200 = CARTESIAN_POINT ( 'NONE',  ( 3.050102900204245682, 42.28728544019637781, 12.13304328177459546 ) ) ;
#50201 = CARTESIAN_POINT ( 'NONE',  ( 4.549368137175248350, 13.59764261105751793, -40.71620287708331176 ) ) ;
#50202 = EDGE_CURVE ( 'NONE', #11373, #868, #5299, .T. ) ;
#50203 = CARTESIAN_POINT ( 'NONE',  ( 0.6017666602106490625, 5.933006478840690434, -47.74032907933392522 ) ) ;
#50204 = AXIS2_PLACEMENT_3D ( 'NONE', #21857, #37517, #8353 ) ;
#50205 = EDGE_CURVE ( 'NONE', #49237, #51439, #35922, .T. ) ;
#50206 = CARTESIAN_POINT ( 'NONE',  ( 5.959547316686252039, 18.96183906913532269, 7.858107265727816149 ) ) ;
#50207 = CARTESIAN_POINT ( 'NONE',  ( 0.8560838555295223751, -45.77741231505103059, 10.23725333375835689 ) ) ;
#50208 = EDGE_CURVE ( 'NONE', #55475, #37747, #14576, .T. ) ;
#50209 = CARTESIAN_POINT ( 'NONE',  ( 1.227938101723748288, -42.43379953535180960, -6.439911493065006987 ) ) ;
#50210 = CARTESIAN_POINT ( 'NONE',  ( -6.078726893082806448, -19.21666810860932983, -1.230328440814576041 ) ) ;
#50211 = B_SPLINE_CURVE_WITH_KNOTS ( 'NONE', 3,
 ( #6008, #44286, #7250, #15450 ),
 .UNSPECIFIED., .F., .F.,
 ( 4, 4 ),
 ( 4.336808689942017736E-19, 0.005014147105413698652 ),
 .UNSPECIFIED. ) ;
#50212 = EDGE_CURVE ( 'NONE', #26742, #48322, #44397, .T. ) ;
#50213 = CARTESIAN_POINT ( 'NONE',  ( 0.5980271706414734822, -48.79397779905842469, -5.585425085582683913 ) ) ;
#50214 = CARTESIAN_POINT ( 'NONE',  ( 0.9769922540276041456, 32.61418167833736703, 26.31818209030647893 ) ) ;
#50215 = CARTESIAN_POINT ( 'NONE',  ( 4.956653778116970166, 47.94889704119054130, 3.690426056930153464 ) ) ;
#50216 = CARTESIAN_POINT ( 'NONE',  ( -1.114299999999999846, 0.000000000000000000, -5.633200000000004870 ) ) ;
#50217 = DIRECTION ( 'NONE',  ( 0.000000000000000000, -0.7071067811865487940, 0.7071067811865461294 ) ) ;
#50218 = CYLINDRICAL_SURFACE ( 'NONE', #54669, 4.250000000000000000 ) ;
#50219 = CARTESIAN_POINT ( 'NONE',  ( 4.335381028904216727, 45.01666255113116222, 19.31985870605503308 ) ) ;
#50220 =( BOUNDED_SURFACE ( )  B_SPLINE_SURFACE ( 3, 1, ( 
 ( #21402, #16095 ),
 ( #29561, #15478 ),
 ( #49281, #53966 ),
 ( #34587, #10782 ) ),
 .UNSPECIFIED., .F., .F., .F. ) 
 B_SPLINE_SURFACE_WITH_KNOTS ( ( 4, 4 ),
 ( 2, 2 ),
 ( 0.000000000000000000, 1.000000000000000000 ),
 ( 0.000000000000000000, 1.000000000000000000 ),
 .UNSPECIFIED. ) 
 GEOMETRIC_REPRESENTATION_ITEM ( )  RATIONAL_B_SPLINE_SURFACE ( (
 ( 1.000000000000000000, 1.000000000000000000),
 ( 0.7282232189291694135, 0.9929344683865672927),
 ( 0.7282232189291694135, 0.9929344683865672927),
 ( 1.000000000000000000, 1.000000000000000000) ) ) 
 REPRESENTATION_ITEM ( '' )  SURFACE ( )  );
#50221 = DIRECTION ( 'NONE',  ( -1.000000000000000000, -5.380183451256491399E-17, -1.298891185607892835E-16 ) ) ;
#50222 = CARTESIAN_POINT ( 'NONE',  ( -6.017396004339687465, 18.68180398134250453, 2.460690056887851807 ) ) ;
#50223 = CARTESIAN_POINT ( 'NONE',  ( 4.967162193818130511, 0.000000000000000000, 0.000000000000000000 ) ) ;
#50224 =( BOUNDED_SURFACE ( )  B_SPLINE_SURFACE ( 3, 1, ( 
 ( #17243, #11946 ),
 ( #59510, #31023 ),
 ( #35744, #55426 ),
 ( #21317, #26624 ) ),
 .UNSPECIFIED., .F., .F., .F. ) 
 B_SPLINE_SURFACE_WITH_KNOTS ( ( 4, 4 ),
 ( 2, 2 ),
 ( 0.000000000000000000, 1.000000000000000000 ),
 ( 0.000000000000000000, 1.000000000000000000 ),
 .UNSPECIFIED. ) 
 GEOMETRIC_REPRESENTATION_ITEM ( )  RATIONAL_B_SPLINE_SURFACE ( (
 ( 1.000000000000000000, 1.000000000000000000),
 ( 0.9953485035131437453, 0.8621029689291523912),
 ( 0.9953485035131437453, 0.8621029689291523912),
 ( 1.000000000000000000, 1.000000000000000000) ) ) 
 REPRESENTATION_ITEM ( '' )  SURFACE ( )  );
#50226 = ORIENTED_EDGE ( 'NONE', *, *, #29909, .T. ) ;
#50225 = CARTESIAN_POINT ( 'NONE',  ( 0.5797568599927135358, 23.08701878027053667, -40.81929534558918959 ) ) ;
#50227 = ORIENTED_EDGE ( 'NONE', *, *, #36572, .T. ) ;
#50228 = EDGE_CURVE ( 'NONE', #60, #44595, #50106, .T. ) ;
#50229 = B_SPLINE_CURVE_WITH_KNOTS ( 'NONE', 3,
 ( #36847, #13036, #47161, #23343 ),
 .UNSPECIFIED., .F., .F.,
 ( 4, 4 ),
 ( 0.000000000000000000, 0.004447772540403802446 ),
 .UNSPECIFIED. ) ;
#50230 = CARTESIAN_POINT ( 'NONE',  ( 0.6001305935487315502, 46.60388846085706405, 11.94532529598394532 ) ) ;
#50231 = CARTESIAN_POINT ( 'NONE',  ( 1.834102595619085507, 2.930864502506626224, -43.95006004689448531 ) ) ;
#50232 = FACE_OUTER_BOUND ( 'NONE', #6240, .T. ) ;
#50233 = ORIENTED_EDGE ( 'NONE', *, *, #51323, .F. ) ;
#50234 = EDGE_CURVE ( 'NONE', #32441, #37522, #30186, .T. ) ;
#50235 = ORIENTED_EDGE ( 'NONE', *, *, #38557, .T. ) ;
#50236 = CARTESIAN_POINT ( 'NONE',  ( 0.3622758884714730732, 42.62881903538210793, -6.444611261694146442 ) ) ;
#50237 = DIRECTION ( 'NONE',  ( 1.000000000000000000, 0.000000000000000000, 0.000000000000000000 ) ) ;
#50238 = EDGE_LOOP ( 'NONE', ( #18598, #57715, #14773, #2259 ) ) ;
#50239 = EDGE_LOOP ( 'NONE', ( #86, #13303, #23065, #25991 ) ) ;
#50240 = CARTESIAN_POINT ( 'NONE',  ( 0.5838002273316426072, 47.89576566046788031, 0.1361971433779728680 ) ) ;
#50241 = DIRECTION ( 'NONE',  ( -0.1736481776669312471, 0.9848077530122077983, -5.551115123125779621E-17 ) ) ;
#50242 = DIRECTION ( 'NONE',  ( -1.000000000000000000, 0.000000000000000000, 0.000000000000000000 ) ) ;
#50243 = VERTEX_POINT ( 'NONE', #758 ) ;
#50244 = CARTESIAN_POINT ( 'NONE',  ( 0.1365634738349416899, -17.27620067578395435, -40.60043731086266661 ) ) ;
#50245 = AXIS2_PLACEMENT_3D ( 'NONE', #17633, #45239, #27028 ) ;
#50246 = CARTESIAN_POINT ( 'NONE',  ( 0.6000166863083090663, -42.53190469623939407, 24.55321902762372588 ) ) ;
#50247 = VECTOR ( 'NONE', #56719, 1000.000000000000114 ) ;
#50248 = EDGE_CURVE ( 'NONE', #47719, #42350, #44325, .T. ) ;
#50249 = CARTESIAN_POINT ( 'NONE',  ( 0.3676999524040366896, 37.41430475689384139, 23.36921870497834774 ) ) ;
#50250 = VERTEX_POINT ( 'NONE', #44623 ) ;
#50251 = ORIENTED_EDGE ( 'NONE', *, *, #47047, .T. ) ;
#50252 = CARTESIAN_POINT ( 'NONE',  ( 0.6254311100348637353, 48.10157347124180660, 0.6881768005104212937 ) ) ;
#50253 = CARTESIAN_POINT ( 'NONE',  ( 2.282816707992304739, 46.95498737082395024, -1.313821682622675180 ) ) ;
#50254 = ORIENTED_EDGE ( 'NONE', *, *, #8627, .F. ) ;
#50255 = CARTESIAN_POINT ( 'NONE',  ( 0.5839879882012674051, 44.25009266679231246, -18.32902119196519664 ) ) ;
#50256 = CARTESIAN_POINT ( 'NONE',  ( 4.549368137175248350, -42.82045902618770583, -3.018832571116409014 ) ) ;
#50257 = CARTESIAN_POINT ( 'NONE',  ( 5.894904586330512508, -11.92958617826537271, -16.19303509775059169 ) ) ;
#50258 = CARTESIAN_POINT ( 'NONE',  ( 0.5809828226811553087, 11.86925843957232729, -46.40184912890826752 ) ) ;
#50259 = EDGE_LOOP ( 'NONE', ( #48243, #38710, #14223, #55463 ) ) ;
#50260 = CARTESIAN_POINT ( 'NONE',  ( 0.8560838555295158248, 11.76118766017326323, -45.40977096290972526 ) ) ;
#50261 = CARTESIAN_POINT ( 'NONE',  ( 0.6023142530420679819, 18.65157113320488236, 44.34465601638707000 ) ) ;
#50262 = B_SPLINE_CURVE_WITH_KNOTS ( 'NONE', 3,
 ( #53937, #34867, #59259, #25762 ),
 .UNSPECIFIED., .F., .F.,
 ( 4, 4 ),
 ( 0.000000000000000000, 0.005004948556313802699 ),
 .UNSPECIFIED. ) ;
#50263 = CARTESIAN_POINT ( 'NONE',  ( 0.5807400328401574052, -28.72484455891616406, -38.33001520688979014 ) ) ;
#50264 = CARTESIAN_POINT ( 'NONE',  ( 5.896278296736517710, 17.94863123379886005, 9.075991210192073666 ) ) ;
#50265 = VERTEX_POINT ( 'NONE', #39011 ) ;
#50266 = CARTESIAN_POINT ( 'NONE',  ( 0.1098349054025746785, 42.78286259078963383, -5.417317591399368304 ) ) ;
#50267 = CARTESIAN_POINT ( 'NONE',  ( 0.8753041380234471980, -47.26389509135280775, -13.31399822241900566 ) ) ;
#50268 = CARTESIAN_POINT ( 'NONE',  ( 0.6252788684277225117, -48.61071527006939874, 6.960078455442126000 ) ) ;
#50269 = EDGE_LOOP ( 'NONE', ( #2258, #31927, #55779, #52339 ) ) ;
#50270 = DIRECTION ( 'NONE',  ( 0.000000000000000000, 0.000000000000000000, 1.000000000000000000 ) ) ;
#50271 = CARTESIAN_POINT ( 'NONE',  ( 0.5782707292762442330, 37.25243273660956334, -28.49548400908462042 ) ) ;
#50272 = CARTESIAN_POINT ( 'NONE',  ( 2.299652685299201860, 46.92539516736430727, -14.22283421983313367 ) ) ;
#50273 = PRODUCT_DEFINITION_SHAPE ( 'NONE', 'NONE',  #3771 ) ;
#50274 = CARTESIAN_POINT ( 'NONE',  ( 5.894904586330512508, -13.98146465072115241, -14.45849432971074044 ) ) ;
#50275 = CARTESIAN_POINT ( 'NONE',  ( 0.5837799406558235038, -46.78519619469427937, 3.223191989498096710 ) ) ;
#50276 = CARTESIAN_POINT ( 'NONE',  ( 4.975610109902397937, -48.84566763821283786, 2.559328059280373768 ) ) ;
#50277 = CARTESIAN_POINT ( 'NONE',  ( 0.9730545539215883499, -6.101350888304360787, -42.47233286818623554 ) ) ;
#50278 = CARTESIAN_POINT ( 'NONE',  ( 5.960721111146673579, -5.318514366754798495, -19.82454228767744198 ) ) ;
#50279 = EDGE_CURVE ( 'NONE', #30761, #29776, #3292, .T. ) ;
#50280 = CARTESIAN_POINT ( 'NONE',  ( 0.6027444965799114707, 41.22745124204113409, -26.68025074793268203 ) ) ;
#50281 = CARTESIAN_POINT ( 'NONE',  ( 4.956653778116968390, 48.02038484091101367, -2.599733001514498376 ) ) ;
#50282 = ORIENTED_EDGE ( 'NONE', *, *, #9231, .T. ) ;
#50283 = EDGE_CURVE ( 'NONE', #52990, #43207, #39939, .T. ) ;
#50284 = CARTESIAN_POINT ( 'NONE',  ( 0.7762783648524382851, 11.53708172997884596, -46.49451980369966009 ) ) ;
#50285 = DIRECTION ( 'NONE',  ( -1.000000000000000000, -0.000000000000000000, -0.000000000000000000 ) ) ;
#50286 = CARTESIAN_POINT ( 'NONE',  ( 2.301529144917015213, 1.287519423136602947, 48.01619158420459144 ) ) ;
#50287 = CARTESIAN_POINT ( 'NONE',  ( 0.7044674535453004927, 5.553212498070795533, 48.79512838144990639 ) ) ;
#50288 = CARTESIAN_POINT ( 'NONE',  ( -6.001507490154111224, 0.01557731607579719395, -18.84387066167321478 ) ) ;
#50289 = CONICAL_SURFACE ( 'NONE', #25255, 42.08604991992415023, 1.569615340895231137 ) ;
#50290 = CARTESIAN_POINT ( 'NONE',  ( 0.9784957157296351182, -30.92500134937655787, 28.28387081948704918 ) ) ;
#50291 = APPLICATION_PROTOCOL_DEFINITION ( 'draft international standard', 'automotive_design', 1998, #13962 ) ;
#50292 = CARTESIAN_POINT ( 'NONE',  ( -2.569797478183790229, 2.353985772484751049, -14.44232325624824398 ) ) ;
#50293 = VECTOR ( 'NONE', #38908, 1000.000000000000000 ) ;
#50294 = CARTESIAN_POINT ( 'NONE',  ( 5.917102823773431552, -4.670717611792517765, 19.56205804721562203 ) ) ;
#50295 = CARTESIAN_POINT ( 'NONE',  ( 0.8751705887134553219, -29.98056538504934210, -37.60752970653818039 ) ) ;
#50297 = ORIENTED_EDGE ( 'NONE', *, *, #52677, .T. ) ;
#50296 = CARTESIAN_POINT ( 'NONE',  ( 3.782542959838390839, 42.00313795915501203, 1.724602847255015670 ) ) ;
#50298 = VERTEX_POINT ( 'NONE', #48079 ) ;
#50299 = DIRECTION ( 'NONE',  ( -1.000000000000000000, -0.000000000000000000, -0.000000000000000000 ) ) ;
#50300 = CARTESIAN_POINT ( 'NONE',  ( 0.8551540677456834771, -41.94570365541186874, -23.16399837394590477 ) ) ;
#50301 = CARTESIAN_POINT ( 'NONE',  ( 4.975801465491694664, -2.564218696447152279, -47.84403947906842092 ) ) ;
#50302 = ADVANCED_FACE ( 'NONE', ( #5132 ), #24157, .F. ) ;
#50303 = EDGE_LOOP ( 'NONE', ( #51374, #59504, #5405, #11292 ) ) ;
#50304 = CARTESIAN_POINT ( 'NONE',  ( 5.959547316686252039, 5.308980600728181010, 19.82715097195164233 ) ) ;
#50305 = CARTESIAN_POINT ( 'NONE',  ( 0.5839879882012688483, -47.48620708510743782, 6.251708210201897487 ) ) ;
#50306 = CARTESIAN_POINT ( 'NONE',  ( 0.7246131072078586532, 41.24126838495065783, 24.75818606403465338 ) ) ;
#50307 = ORIENTED_EDGE ( 'NONE', *, *, #22831, .F. ) ;
#50308 = ORIENTED_EDGE ( 'NONE', *, *, #24178, .F. ) ;
#50309 = CARTESIAN_POINT ( 'NONE',  ( 0.8751705887134553219, -47.55935879196475469, 7.160166390003496417 ) ) ;
#50310 = CARTESIAN_POINT ( 'NONE',  ( 0.1092355843206037486, -10.87081649985060849, -41.73183925352176971 ) ) ;
#50311 = CARTESIAN_POINT ( 'NONE',  ( 2.282816707992310512, -42.50075753973140280, -20.00456385320434549 ) ) ;
#50312 = ORIENTED_EDGE ( 'NONE', *, *, #26338, .T. ) ;
#50313 = ORIENTED_EDGE ( 'NONE', *, *, #34394, .T. ) ;
#50314 = DIRECTION ( 'NONE',  ( 0.000000000000000000, 0.000000000000000000, 1.000000000000000000 ) ) ;
#50315 = CARTESIAN_POINT ( 'NONE',  ( 3.783278058412226308, -33.06594414781516633, 27.54892951149532365 ) ) ;
#50316 = ORIENTED_EDGE ( 'NONE', *, *, #48161, .T. ) ;
#50317 = CARTESIAN_POINT ( 'NONE',  ( 0.6067375320500736358, 34.36594163291755422, -33.36326114377782659 ) ) ;
#50318 = CARTESIAN_POINT ( 'NONE',  ( 0.8560838555295158248, 16.00311602465144745, 44.09391240957503300 ) ) ;
#50319 = ORIENTED_EDGE ( 'NONE', *, *, #61454, .T. ) ;
#50320 = CARTESIAN_POINT ( 'NONE',  ( 0.7044674535453004927, 10.10543771684659298, -48.05915991111207575 ) ) ;
#50321 = CARTESIAN_POINT ( 'NONE',  ( 5.974727161628369032, 19.82959049719575262, -5.297264154380731505 ) ) ;
#50322 = ORIENTED_EDGE ( 'NONE', *, *, #52862, .T. ) ;
#50323 = CARTESIAN_POINT ( 'NONE',  ( -6.072942160501519027, 17.85441038494896304, -7.212779775845567620 ) ) ;
#50324 = CARTESIAN_POINT ( 'NONE',  ( 0.5835226383429290564, -19.57482050365606696, 42.61535963470931421 ) ) ;
#50325 = CARTESIAN_POINT ( 'NONE',  ( 1.227938101723748288, 42.65467462194924764, -4.762198645644009076 ) ) ;
#50326 = CARTESIAN_POINT ( 'NONE',  ( -6.010958268070873523, 16.32616437357125250, -9.409153349053413606 ) ) ;
#50327 = VERTEX_POINT ( 'NONE', #36458 ) ;
#50328 = ADVANCED_FACE ( 'NONE', ( #50836 ), #50149, .F. ) ;
#50329 = CARTESIAN_POINT ( 'NONE',  ( 0.5806925824938502512, 37.13995815321093374, 28.63295078613632683 ) ) ;
#50330 = CARTESIAN_POINT ( 'NONE',  ( 0.1310142868023692897, -42.83311553787496706, 4.996535778098624370 ) ) ;
#50331 = ORIENTED_EDGE ( 'NONE', *, *, #44249, .F. ) ;
#50332 = CARTESIAN_POINT ( 'NONE',  ( 1.227938101723757836, -15.63977281655870222, 39.96870412324331312 ) ) ;
#50333 =( BOUNDED_SURFACE ( )  B_SPLINE_SURFACE ( 3, 1, ( 
 ( #8093, #47243 ),
 ( #4291, #10184 ),
 ( #53079, #46033 ),
 ( #17503, #12819 ) ),
 .UNSPECIFIED., .F., .F., .F. ) 
 B_SPLINE_SURFACE_WITH_KNOTS ( ( 4, 4 ),
 ( 2, 2 ),
 ( 0.000000000000000000, 1.000000000000000000 ),
 ( 0.000000000000000000, 1.000000000000000000 ),
 .UNSPECIFIED. ) 
 GEOMETRIC_REPRESENTATION_ITEM ( )  RATIONAL_B_SPLINE_SURFACE ( (
 ( 1.000000000000000000, 1.000000000000000000),
 ( 0.7282232189291694135, 0.9929344683865672927),
 ( 0.7282232189291694135, 0.9929344683865672927),
 ( 1.000000000000000000, 1.000000000000000000) ) ) 
 REPRESENTATION_ITEM ( '' )  SURFACE ( )  );
#50334 = ORIENTED_EDGE ( 'NONE', *, *, #45068, .T. ) ;
#50335 = CARTESIAN_POINT ( 'NONE',  ( 0.5827357941260234986, -17.99287562175617694, 44.38787053017142625 ) ) ;
#50336 = EDGE_CURVE ( 'NONE', #33079, #5070, #57620, .T. ) ;
#50337 = EDGE_LOOP ( 'NONE', ( #10421, #31079, #35928, #14300 ) ) ;
#50338 = CARTESIAN_POINT ( 'NONE',  ( 0.7948884756798507700, 10.07807595004759271, 48.05341850217551070 ) ) ;
#50339 = CARTESIAN_POINT ( 'NONE',  ( 0.5988103564986355654, 44.21009236284883315, -18.96890181990844582 ) ) ;
#50340 = CARTESIAN_POINT ( 'NONE',  ( 0.1156495703730067853, -43.74427687214311078, 5.777646074687804223 ) ) ;
#50341 = ORIENTED_EDGE ( 'NONE', *, *, #7694, .F. ) ;
#50342 = CARTESIAN_POINT ( 'NONE',  ( 0.1152809850208375703, 43.26768730443608035, 8.651734959838789152 ) ) ;
#50343 = CARTESIAN_POINT ( 'NONE',  ( 3.270143674763207553, 13.28976595685393391, 3.277085381513166418 ) ) ;
#50344 = CARTESIAN_POINT ( 'NONE',  ( 0.5848930533535030563, 17.02477461160209771, 43.69702657860951689 ) ) ;
#50345 = ORIENTED_EDGE ( 'NONE', *, *, #44321, .F. ) ;
#50346 = AXIS2_PLACEMENT_3D ( 'NONE', #29265, #5439, #14888 ) ;
#50347 = B_SPLINE_CURVE_WITH_KNOTS ( 'NONE', 3,
 ( #18627, #47435, #9833, #4483 ),
 .UNSPECIFIED., .F., .F.,
 ( 4, 4 ),
 ( 1.084202172485504434E-18, 0.004446298630425059815 ),
 .UNSPECIFIED. ) ;
#50348 = ORIENTED_EDGE ( 'NONE', *, *, #22030, .T. ) ;
#50349 = CARTESIAN_POINT ( 'NONE',  ( 1.227938101723756947, -34.55893248994489397, -25.45152231597092651 ) ) ;
#50350 = CARTESIAN_POINT ( 'NONE',  ( 4.960386119450153508, 6.813122688534127391, 43.22057176742715967 ) ) ;
#50351 = CARTESIAN_POINT ( 'NONE',  ( 0.6008122571543325074, 33.33611234963518655, 36.05909266575930161 ) ) ;
#50352 = CARTESIAN_POINT ( 'NONE',  ( 3.238931869106854489, -41.96286875554261542, -9.350562014685982248 ) ) ;
#50353 = FACE_OUTER_BOUND ( 'NONE', #29223, .T. ) ;
#50354 = CARTESIAN_POINT ( 'NONE',  ( 5.272379999999998290, 1.883773750090843600E-15, -15.38217999999999996 ) ) ;
#50355 = ORIENTED_EDGE ( 'NONE', *, *, #31343, .T. ) ;
#50356 = EDGE_CURVE ( 'NONE', #21914, #44582, #6266, .T. ) ;
#50357 = CARTESIAN_POINT ( 'NONE',  ( 5.917102823773431552, 20.06759006498879572, -1.334746056486034504 ) ) ;
#50358 = CARTESIAN_POINT ( 'NONE',  ( 4.834790513006553603, 40.94190515849751222, 23.58706728096937866 ) ) ;
#50359 = ORIENTED_EDGE ( 'NONE', *, *, #37459, .T. ) ;
#50360 = EDGE_CURVE ( 'NONE', #6072, #33892, #26340, .T. ) ;
#50361 = CARTESIAN_POINT ( 'NONE',  ( 0.5807400328401637335, 17.82553128098468420, -44.45848844984423920 ) ) ;
#50362 = CARTESIAN_POINT ( 'NONE',  ( 0.5817217712918323347, 36.52004312053393420, 29.41974514646100047 ) ) ;
#50363 = CARTESIAN_POINT ( 'NONE',  ( 0.6021448801613057400, 44.13030167720265240, 21.54199648375312037 ) ) ;
#50364 = CARTESIAN_POINT ( 'NONE',  ( 0.6001305935487422083, 38.48510059944008077, 28.87057754790950881 ) ) ;
#50365 = CARTESIAN_POINT ( 'NONE',  ( 0.5850706913938534814, -6.431767090162503031, -47.46255051844960349 ) ) ;
#50366 = CARTESIAN_POINT ( 'NONE',  ( -4.467300000000000715, 0.000000000000000000, -46.67105333295396719 ) ) ;
#50367 = CARTESIAN_POINT ( 'NONE',  ( 0.8554163680231816613, 3.785871848717079935, -46.76401017296218043 ) ) ;
#50368 = EDGE_CURVE ( 'NONE', #45974, #53665, #8303, .T. ) ;
#50369 = CARTESIAN_POINT ( 'NONE',  ( 0.6031356219577718170, 38.21934428970573094, 29.21669799774976184 ) ) ;
#50370 = FACE_OUTER_BOUND ( 'NONE', #40222, .T. ) ;
#50371 = DIRECTION ( 'NONE',  ( 0.02222222222222222307, 0.9997530559290660479, -0.000000000000000000 ) ) ;
#50372 = CARTESIAN_POINT ( 'NONE',  ( 0.5850706913938534814, -18.16120156791912521, 44.31965802246099884 ) ) ;
#50373 = CARTESIAN_POINT ( 'NONE',  ( 1.231276596079881047, 8.892602616353681100, 40.96581977363184990 ) ) ;
#50374 = CARTESIAN_POINT ( 'NONE',  ( 4.956653778116975495, -36.51451553856441024, 31.29546495791839078 ) ) ;
#50375 = CARTESIAN_POINT ( 'NONE',  ( 0.1129192098497455998, -18.30288010335110016, 40.14917642626692640 ) ) ;
#50376 = CARTESIAN_POINT ( 'NONE',  ( 0.5848930533535030563, -38.55997537638119610, 26.69084826978029668 ) ) ;
#50377 = ADVANCED_FACE ( 'NONE', ( #7601 ), #16121, .F. ) ;
#50378 = B_SPLINE_CURVE_WITH_KNOTS ( 'NONE', 3,
 ( #5758, #11122, #36709, #55468 ),
 .UNSPECIFIED., .F., .F.,
 ( 4, 4 ),
 ( 2.168404344971008868E-19, 0.004041751736740987339 ),
 .UNSPECIFIED. ) ;
#50379 = CONICAL_SURFACE ( 'NONE', #33368, 42.92674063221959813, 1.485477209440487556 ) ;
#50380 = CARTESIAN_POINT ( 'NONE',  ( 0.9754292589017210524, -7.544321835733828863, -41.22390902054472406 ) ) ;
#50381 = CARTESIAN_POINT ( 'NONE',  ( 1.231276596079887264, 38.91607545535247681, 15.58254928345742840 ) ) ;
#50382 = EDGE_LOOP ( 'NONE', ( #9236, #23000, #31997, #57 ) ) ;
#50383 = CARTESIAN_POINT ( 'NONE',  ( 3.661921753701997684, 34.02818019380067938, 32.47636181182038229 ) ) ;
#50384 = CARTESIAN_POINT ( 'NONE',  ( 0.1087620492084206414, 43.12302841504342155, 0.3620418170788286538 ) ) ;
#50385 = CARTESIAN_POINT ( 'NONE',  ( 0.1152339509894530906, -38.55535503695174526, -21.45756949027179772 ) ) ;
#50386 = CARTESIAN_POINT ( 'NONE',  ( 4.956445790443998689, -27.49627641100115838, 38.22947597952995835 ) ) ;
#50387 = ORIENTED_EDGE ( 'NONE', *, *, #20645, .F. ) ;
#50388 = CARTESIAN_POINT ( 'NONE',  ( 5.981074661064941900, 20.52466374824937034, 0.008585178657687824941 ) ) ;
#50389 = CARTESIAN_POINT ( 'NONE',  ( 5.860006189529234355, -21.34829429597437311, -43.25137511473273122 ) ) ;
#50390 = B_SPLINE_CURVE_WITH_KNOTS ( 'NONE', 3,
 ( #56279, #52196, #47214, #13397, #32499, #8665 ),
 .UNSPECIFIED., .F., .F.,
 ( 4, 2, 4 ),
 ( 1.250652936113012808E-16, 0.0002448718616795918495, 0.0004897437233590586905 ),
 .UNSPECIFIED. ) ;
#50391 = VECTOR ( 'NONE', #28762, 1000.000000000000114 ) ;
#50392 =( BOUNDED_SURFACE ( )  B_SPLINE_SURFACE ( 3, 1, ( 
 ( #27296, #2553 ),
 ( #16992, #7553 ),
 ( #56098, #26677 ),
 ( #21990, #37035 ) ),
 .UNSPECIFIED., .F., .F., .F. ) 
 B_SPLINE_SURFACE_WITH_KNOTS ( ( 4, 4 ),
 ( 2, 2 ),
 ( 0.000000000000000000, 1.000000000000000000 ),
 ( 0.000000000000000000, 1.000000000000000000 ),
 .UNSPECIFIED. ) 
 GEOMETRIC_REPRESENTATION_ITEM ( )  RATIONAL_B_SPLINE_SURFACE ( (
 ( 1.000000000000000000, 1.000000000000000000),
 ( 0.9754377213608244057, 0.9999580625633939235),
 ( 0.9754377213608244057, 0.9999580625633939235),
 ( 1.000000000000000000, 1.000000000000000000) ) ) 
 REPRESENTATION_ITEM ( '' )  SURFACE ( )  );
#50393 = CARTESIAN_POINT ( 'NONE',  ( 0.1119899015040013712, 43.99420331743984747, 3.386942966197092897 ) ) ;
#50394 = VERTEX_POINT ( 'NONE', #49598 ) ;
#50395 = CARTESIAN_POINT ( 'NONE',  ( 3.407937589446174087, 7.243367523631186522, -11.62731850632876629 ) ) ;
#50396 = EDGE_LOOP ( 'NONE', ( #32188, #44132, #54309, #13067, #53599, #5673 ) ) ;
#50397 = ADVANCED_FACE ( 'NONE', ( #45864 ), #37354, .F. ) ;
#50398 = CARTESIAN_POINT ( 'NONE',  ( 0.8744876279028306332, 48.01195819035234535, -10.25679877482985169 ) ) ;
#50399 = CARTESIAN_POINT ( 'NONE',  ( 5.894904586330512508, 20.06791991542433351, 1.344619771444058642 ) ) ;
#50400 = ORIENTED_EDGE ( 'NONE', *, *, #4999, .F. ) ;
#50401 = DIRECTION ( 'NONE',  ( 0.000000000000000000, 0.000000000000000000, 1.000000000000000000 ) ) ;
#50402 = ORIENTED_EDGE ( 'NONE', *, *, #36566, .T. ) ;
#50403 = CARTESIAN_POINT ( 'NONE',  ( 5.896782393890504181, -18.51935720350329362, -7.845985957613155648 ) ) ;
#50404 = CARTESIAN_POINT ( 'NONE',  ( 0.3622758884714600280, -42.84426538328734324, 4.808133778521152202 ) ) ;
#50405 = EDGE_CURVE ( 'NONE', #15890, #5168, #27694, .T. ) ;
#50406 = EDGE_LOOP ( 'NONE', ( #57193, #34551, #36459, #60402 ) ) ;
#50407 = EDGE_CURVE ( 'NONE', #52413, #43658, #21412, .T. ) ;
#50408 = LINE ( 'NONE', #3700, #33776 ) ;
#50409 = ORIENTED_EDGE ( 'NONE', *, *, #35408, .F. ) ;
#50410 = DIRECTION ( 'NONE',  ( 0.000000000000000000, 0.000000000000000000, -1.000000000000000000 ) ) ;
#50411 =( BOUNDED_SURFACE ( )  B_SPLINE_SURFACE ( 3, 1, ( 
 ( #32056, #23564 ),
 ( #60527, #17640 ),
 ( #55837, #41466 ),
 ( #51136, #37691 ) ),
 .UNSPECIFIED., .F., .F., .F. ) 
 B_SPLINE_SURFACE_WITH_KNOTS ( ( 4, 4 ),
 ( 2, 2 ),
 ( 0.000000000000000000, 1.000000000000000000 ),
 ( 0.000000000000000000, 1.000000000000000000 ),
 .UNSPECIFIED. ) 
 GEOMETRIC_REPRESENTATION_ITEM ( )  RATIONAL_B_SPLINE_SURFACE ( (
 ( 1.000000000000000000, 1.000000000000000000),
 ( 0.9953390228620291325, 0.8624445117760984880),
 ( 0.9953390228620291325, 0.8624445117760984880),
 ( 1.000000000000000000, 1.000000000000000000) ) ) 
 REPRESENTATION_ITEM ( '' )  SURFACE ( )  );
#50412 = ORIENTED_EDGE ( 'NONE', *, *, #36442, .F. ) ;
#50413 = EDGE_CURVE ( 'NONE', #41264, #35972, #53851, .T. ) ;
#50414 = ORIENTED_EDGE ( 'NONE', *, *, #61568, .T. ) ;
#50415 = CARTESIAN_POINT ( 'NONE',  ( 0.6041374136657476912, -34.14050483116115942, -33.89363087703035404 ) ) ;
#50417 = EDGE_CURVE ( 'NONE', #29889, #437, #51647, .T. ) ;
#50416 = CARTESIAN_POINT ( 'NONE',  ( 0.5997462898726536595, 11.43624519451716992, -47.75734421002901797 ) ) ;
#50418 = CARTESIAN_POINT ( 'NONE',  ( 1.231276596079887931, -37.78837162824473950, -18.14705873423390869 ) ) ;
#50419 = FACE_OUTER_BOUND ( 'NONE', #28311, .T. ) ;
#50420 = FACE_OUTER_BOUND ( 'NONE', #47382, .T. ) ;
#50421 = VERTEX_POINT ( 'NONE', #32061 ) ;
#50422 = CARTESIAN_POINT ( 'NONE',  ( 0.9747592971366229042, 11.41797089479133476, 41.36145845824412959 ) ) ;
#50423 = CARTESIAN_POINT ( 'NONE',  ( 5.974727161628369032, 2.694421823322918463, -20.34732802718244571 ) ) ;
#50424 = CARTESIAN_POINT ( 'NONE',  ( -6.072942160501519027, 19.09631935424740234, 2.476842629158438225 ) ) ;
#50425 = ORIENTED_EDGE ( 'NONE', *, *, #61838, .F. ) ;
#50426 = VECTOR ( 'NONE', #16321, 999.9999999999998863 ) ;
#50427 = VERTEX_POINT ( 'NONE', #9158 ) ;
#50428 = DIRECTION ( 'NONE',  ( 1.000000000000000000, 0.000000000000000000, 0.000000000000000000 ) ) ;
#50429 = CARTESIAN_POINT ( 'NONE',  ( 0.3676999524040323597, 33.04872056100222011, 29.21870381457103605 ) ) ;
#50430 = B_SPLINE_CURVE_WITH_KNOTS ( 'NONE', 3,
 ( #50890, #18017, #37135, #32422, #36202, #54962 ),
 .UNSPECIFIED., .F., .F.,
 ( 4, 2, 4 ),
 ( 8.440430351524944310E-17, 0.0002293366620881469363, 0.0004586733241762094675 ),
 .UNSPECIFIED. ) ;
#50431 = CARTESIAN_POINT ( 'NONE',  ( 0.5834584762367737154, -44.36061497477145821, 15.21091148068631149 ) ) ;
#50432 = VERTEX_POINT ( 'NONE', #28264 ) ;
#50433 = CARTESIAN_POINT ( 'NONE',  ( 0.1100053167205930632, -42.77858932361500877, -5.450899213259354781 ) ) ;
#50434 = CARTESIAN_POINT ( 'NONE',  ( 1.296416391601053153, -34.64371266338438460, 27.24188956318961274 ) ) ;
#50435 = ADVANCED_FACE ( 'NONE', ( #41471 ), #13261, .T. ) ;
#50436 = EDGE_LOOP ( 'NONE', ( #18419, #48712, #56036, #48364, #61180 ) ) ;
#50437 = CARTESIAN_POINT ( 'NONE',  ( -6.010958268070873523, 13.33459572764776091, -13.31406649671948550 ) ) ;
#50438 = VERTEX_POINT ( 'NONE', #27344 ) ;
#50439 = EDGE_CURVE ( 'NONE', #57918, #48340, #14288, .T. ) ;
#50440 = CARTESIAN_POINT ( 'NONE',  ( 4.963659409799328515, 9.199077662859513893, -43.79875484948436082 ) ) ;
#50441 = CARTESIAN_POINT ( 'NONE',  ( 5.895596859100789899, 5.962379729971948983, 19.20880556328547684 ) ) ;
#50442 = CIRCLE ( 'NONE', #23434, 9.500000000000000000 ) ;
#50443 = DIRECTION ( 'NONE',  ( 0.000000000000000000, 0.000000000000000000, -1.000000000000000000 ) ) ;
#50444 = EDGE_CURVE ( 'NONE', #6088, #42198, #55840, .T. ) ;
#50445 =( LENGTH_UNIT ( ) NAMED_UNIT ( * ) SI_UNIT ( .MILLI., .METRE. ) );
#50446 = ORIENTED_EDGE ( 'NONE', *, *, #4768, .F. ) ;
#50447 = CARTESIAN_POINT ( 'NONE',  ( 0.6254311100348655117, 37.74260849418455877, 29.82834996731709154 ) ) ;
#50448 = CARTESIAN_POINT ( 'NONE',  ( -6.072942160501519915, 0.6317110510321461980, 19.24591134337431342 ) ) ;
#50449 = DIRECTION ( 'NONE',  ( 1.000000000000000000, 0.000000000000000000, 0.000000000000000000 ) ) ;
#50450 = CARTESIAN_POINT ( 'NONE',  ( 0.9745511491811756910, 37.32887948083628515, -21.15859207114708340 ) ) ;
#50451 = CARTESIAN_POINT ( 'NONE',  ( 4.967162193818130511, 14.26841313271282097, 40.65506779172170582 ) ) ;
#50452 = CARTESIAN_POINT ( 'NONE',  ( 0.5832366564991500191, 5.981458972434432475, -47.52097076201149406 ) ) ;
#50453 = EDGE_CURVE ( 'NONE', #26555, #34535, #9834, .T. ) ;
#50454 = APPLICATION_CONTEXT ( 'automotive_design' ) ;
#50455 = CARTESIAN_POINT ( 'NONE',  ( 0.1310142868023692342, -0.6370537502139506092, 43.11885108606331585 ) ) ;
#50456 = EDGE_CURVE ( 'NONE', #59315, #32617, #42693, .T. ) ;
#50457 = CARTESIAN_POINT ( 'NONE',  ( 0.8551540677456834771, 17.49081417858847942, -44.61036085020932518 ) ) ;
#50458 = CARTESIAN_POINT ( 'NONE',  ( 0.8560838555295158248, -46.73345513967312570, -4.044379407262746362 ) ) ;
#50459 = ORIENTED_EDGE ( 'NONE', *, *, #38247, .F. ) ;
#50460 = CARTESIAN_POINT ( 'NONE',  ( 0.7056759521545007408, -46.12215779644467517, 8.514422430021223676 ) ) ;
#50461 = CARTESIAN_POINT ( 'NONE',  ( 4.549368137175248350, 13.99871866169365653, -40.58005590356676606 ) ) ;
#50462 = CARTESIAN_POINT ( 'NONE',  ( 3.221118495291109163, -42.02902145736321415, 12.97392673781741657 ) ) ;
#50463 = EDGE_LOOP ( 'NONE', ( #61091, #37790, #60404, #3327 ) ) ;
#50464 = CARTESIAN_POINT ( 'NONE',  ( 2.528100132419517809, -40.03693467153145491, -12.62131691780209408 ) ) ;
#50465 = CARTESIAN_POINT ( 'NONE',  ( 5.960721111146673579, 10.25731071096582880, -17.77882586010657207 ) ) ;
#50466 = CARTESIAN_POINT ( 'NONE',  ( 0.5806925824938499181, 16.34374012233052653, 43.95571090492437349 ) ) ;
#50467 = ORIENTED_EDGE ( 'NONE', *, *, #52740, .F. ) ;
#50468 = CARTESIAN_POINT ( 'NONE',  ( 4.975801465491694664, 35.64402118370912120, 32.01766832630325155 ) ) ;
#50469 = CARTESIAN_POINT ( 'NONE',  ( 0.9745511491811728044, -41.35688774886282459, -11.43411988112647037 ) ) ;
#50470 = AXIS2_PLACEMENT_3D ( 'NONE', #12850, #50714, #41061 ) ;
#50471 = CARTESIAN_POINT ( 'NONE',  ( 4.390527457369401532, -10.08871719600491978, 42.75983070555417953 ) ) ;
#50472 = ORIENTED_EDGE ( 'NONE', *, *, #43299, .T. ) ;
#50473 = ORIENTED_EDGE ( 'NONE', *, *, #34815, .F. ) ;
#50474 = VERTEX_POINT ( 'NONE', #60845 ) ;
#50475 = CARTESIAN_POINT ( 'NONE',  ( 4.962356264823603702, -40.70360067759225586, -10.69824704058845022 ) ) ;
#50476 = EDGE_CURVE ( 'NONE', #48814, #36274, #16324, .T. ) ;
#50477 = ORIENTED_EDGE ( 'NONE', *, *, #19260, .F. ) ;
#50478 = CARTESIAN_POINT ( 'NONE',  ( 5.960721111146673579, -2.685391721745896909, -20.34914600876574298 ) ) ;
#50479 = ORIENTED_EDGE ( 'NONE', *, *, #60873, .T. ) ;
#50480 = ADVANCED_FACE ( 'NONE', ( #51438 ), #46144, .F. ) ;
#50481 = CARTESIAN_POINT ( 'NONE',  ( -6.078457390727109555, -14.65958194562084316, -12.48563847855348286 ) ) ;
#50482 = EDGE_CURVE ( 'NONE', #54850, #12765, #6808, .T. ) ;
#50483 =( BOUNDED_SURFACE ( )  B_SPLINE_SURFACE ( 3, 1, ( 
 ( #16389, #17023 ),
 ( #31414, #50511 ),
 ( #7587, #1338 ),
 ( #20473, #39604 ) ),
 .UNSPECIFIED., .F., .F., .F. ) 
 B_SPLINE_SURFACE_WITH_KNOTS ( ( 4, 4 ),
 ( 2, 2 ),
 ( 0.000000000000000000, 1.000000000000000000 ),
 ( 0.000000000000000000, 1.000000000000000000 ),
 .UNSPECIFIED. ) 
 GEOMETRIC_REPRESENTATION_ITEM ( )  RATIONAL_B_SPLINE_SURFACE ( (
 ( 1.000000000000000000, 1.000000000000000000),
 ( 0.9953040768229005630, 0.8617119497784937465),
 ( 0.9953040768229005630, 0.8617119497784937465),
 ( 1.000000000000000000, 1.000000000000000000) ) ) 
 REPRESENTATION_ITEM ( '' )  SURFACE ( )  );
#50484 = ORIENTED_EDGE ( 'NONE', *, *, #33698, .T. ) ;
#50485 = ADVANCED_FACE ( 'NONE', ( #34784 ), #914, .F. ) ;
#50486 = CARTESIAN_POINT ( 'NONE',  ( 0.1158403557922069033, 15.20339722355584477, 41.42218029083685593 ) ) ;
#50487 = CARTESIAN_POINT ( 'NONE',  ( 48.19965373053142343, 12.43020942110654659, -1.327029891807659512 ) ) ;
#50488 = DIRECTION ( 'NONE',  ( 1.000000000000000000, 0.000000000000000000, -0.000000000000000000 ) ) ;
#50489 = CARTESIAN_POINT ( 'NONE',  ( -6.078457390727109555, 3.077585051286873430, 19.00849760737558825 ) ) ;
#50491 = EDGE_CURVE ( 'NONE', #42003, #51041, #48339, .T. ) ;
#50490 = VERTEX_POINT ( 'NONE', #15985 ) ;
#50492 = DIRECTION ( 'NONE',  ( 0.000000000000000000, 0.000000000000000000, -1.000000000000000000 ) ) ;
#50493 = ORIENTED_EDGE ( 'NONE', *, *, #8600, .T. ) ;
#50494 = CARTESIAN_POINT ( 'NONE',  ( 0.6064782688330855320, -30.81732999423350350, 35.35005825236059707 ) ) ;
#50495 = CARTESIAN_POINT ( 'NONE',  ( 0.9756354156337454508, 26.01752520779911748, 34.12075394380514837 ) ) ;
#50496 = AXIS2_PLACEMENT_3D ( 'NONE', #49371, #24338, #9941 ) ;
#50497 = EDGE_CURVE ( 'NONE', #55102, #22212, #24439, .T. ) ;
#50498 = FACE_OUTER_BOUND ( 'NONE', #46961, .T. ) ;
#50499 = ORIENTED_EDGE ( 'NONE', *, *, #57069, .F. ) ;
#50500 = CARTESIAN_POINT ( 'NONE',  ( 4.967162193818130511, 0.000000000000000000, 0.000000000000000000 ) ) ;
#50501 = CARTESIAN_POINT ( 'NONE',  ( -6.078726893082806448, 0.6137717894420866571, -19.24622886331774652 ) ) ;
#50502 = CARTESIAN_POINT ( 'NONE',  ( 4.303969348037246512, -32.45857549159277511, -35.51084504003230080 ) ) ;
#50503 =( BOUNDED_SURFACE ( )  B_SPLINE_SURFACE ( 3, 1, ( 
 ( #19179, #9441 ),
 ( #35, #9755 ),
 ( #48287, #38294 ),
 ( #27950, #28244 ) ),
 .UNSPECIFIED., .F., .F., .F. ) 
 B_SPLINE_SURFACE_WITH_KNOTS ( ( 4, 4 ),
 ( 2, 2 ),
 ( 0.000000000000000000, 1.000000000000000000 ),
 ( 0.000000000000000000, 1.000000000000000000 ),
 .UNSPECIFIED. ) 
 GEOMETRIC_REPRESENTATION_ITEM ( )  RATIONAL_B_SPLINE_SURFACE ( (
 ( 1.000000000000000000, 1.000000000000000000),
 ( 0.9953390228620291325, 0.8624445117760984880),
 ( 0.9953390228620291325, 0.8624445117760984880),
 ( 1.000000000000000000, 1.000000000000000000) ) ) 
 REPRESENTATION_ITEM ( '' )  SURFACE ( )  );
#50504 = EDGE_LOOP ( 'NONE', ( #22905, #38938, #25411, #15678 ) ) ;
#50505 = ORIENTED_EDGE ( 'NONE', *, *, #54677, .T. ) ;
#50506 = CARTESIAN_POINT ( 'NONE',  ( 0.9791128995231614951, -39.59150764406756196, -13.74226897989937513 ) ) ;
#50507 = CARTESIAN_POINT ( 'NONE',  ( 3.661921753702009674, -21.49231610627914080, -41.84150418211332578 ) ) ;
#50508 =( BOUNDED_SURFACE ( )  B_SPLINE_SURFACE ( 3, 1, ( 
 ( #38054, #51175 ),
 ( #13298, #51477 ),
 ( #37741, #57101 ),
 ( #9199, #60570 ) ),
 .UNSPECIFIED., .F., .F., .F. ) 
 B_SPLINE_SURFACE_WITH_KNOTS ( ( 4, 4 ),
 ( 2, 2 ),
 ( 0.000000000000000000, 1.000000000000000000 ),
 ( 0.000000000000000000, 1.000000000000000000 ),
 .UNSPECIFIED. ) 
 GEOMETRIC_REPRESENTATION_ITEM ( )  RATIONAL_B_SPLINE_SURFACE ( (
 ( 1.000000000000000000, 1.000000000000000000),
 ( 0.7223157951917480446, 0.9931996967497186413),
 ( 0.7223157951917480446, 0.9931996967497186413),
 ( 1.000000000000000000, 1.000000000000000000) ) ) 
 REPRESENTATION_ITEM ( '' )  SURFACE ( )  );
#50509 = CARTESIAN_POINT ( 'NONE',  ( 1.231276596079881047, 20.88402890667877898, -36.34740854095476692 ) ) ;
#50510 = CARTESIAN_POINT ( 'NONE',  ( 0.6029303876144825880, 6.409038528276127522, -47.67862422489726981 ) ) ;
#50511 = CARTESIAN_POINT ( 'NONE',  ( 0.7048096507298635682, 37.64898672361954368, -29.95256433478687086 ) ) ;
#50512 = CARTESIAN_POINT ( 'NONE',  ( 0.1119898979215350893, 25.70258805518049172, 35.86555834665789178 ) ) ;
#50513 = CARTESIAN_POINT ( 'NONE',  ( 0.6028618097248862329, 12.28244208173060592, -46.51318640245703051 ) ) ;
#50514 = CARTESIAN_POINT ( 'NONE',  ( 4.975610109902397937, -23.13264022976521161, -43.09675583078175265 ) ) ;
#50515 = B_SPLINE_CURVE_WITH_KNOTS ( 'NONE', 3,
 ( #24243, #29556, #53646, #10777, #48981, #10462, #30167, #53352, #6030, #58346, #416, #5720, #58045, #29865, #15170, #48665, #25167, #44009, #11087 ),
 .UNSPECIFIED., .F., .F.,
 ( 4, 3, 3, 3, 3, 3, 4 ),
 ( 1.128550957684774488E-16, 0.0002618519381806285731, 0.0003927759815486009626, 0.0005237000248299445142, 0.0006546240681324982588, 0.0007855481115631359618, 0.0009699050456655092071 ),
 .UNSPECIFIED. ) ;
#50516 = CARTESIAN_POINT ( 'NONE',  ( 0.6252788684277179598, -42.44619877470422153, 24.69341087723536887 ) ) ;
#50517 = CARTESIAN_POINT ( 'NONE',  ( 0.8753041380234524160, -35.88662119133316963, -33.51550010581278372 ) ) ;
#50518 = CARTESIAN_POINT ( 'NONE',  ( -6.077587904424778920, 7.788877841491995468, -17.61049128685073129 ) ) ;
#50519 = AXIS2_PLACEMENT_3D ( 'NONE', #7327, #2642, #60264 ) ;
#50520 = CARTESIAN_POINT ( 'NONE',  ( 0.9730545539215883499, 29.98130006528905156, -30.69604515769618658 ) ) ;
#50521 = CARTESIAN_POINT ( 'NONE',  ( 0.7242486021783832717, 17.72443731528298372, -45.79143789214940341 ) ) ;
#50522 = CARTESIAN_POINT ( 'NONE',  ( 1.114300000000000068, 8.409404640385035208E-16, 6.866799999999992465 ) ) ;
#50523 = CARTESIAN_POINT ( 'NONE',  ( 0.5850706913938534814, 6.071602062251297838, -47.50996714391775555 ) ) ;
#50524 = ADVANCED_FACE ( 'NONE', ( #53848 ), #10352, .F. ) ;
#50525 = CARTESIAN_POINT ( 'NONE',  ( 0.8744876279028306332, -38.80702141274064587, 30.07266432244707843 ) ) ;
#50526 = CARTESIAN_POINT ( 'NONE',  ( 0.5809828226811617480, -44.03860873105681151, -18.83114015454746237 ) ) ;
#50527 = CARTESIAN_POINT ( 'NONE',  ( 0.6017666602106489515, 46.37677619531712025, -12.78804974226051705 ) ) ;
#50529 = EDGE_LOOP ( 'NONE', ( #33697, #49808, #4325, #14456, #35047 ) ) ;
#50528 = CARTESIAN_POINT ( 'NONE',  ( 2.624215991343620935, 38.92973006074512909, 28.09277600149231802 ) ) ;
#50530 = ORIENTED_EDGE ( 'NONE', *, *, #31885, .F. ) ;
#50531 = CARTESIAN_POINT ( 'NONE',  ( 0.6021447746440204973, 16.71456626119010025, -46.17536587606831944 ) ) ;
#50532 = CARTESIAN_POINT ( 'NONE',  ( 4.553261556744875094, 1.633632119647590697, -43.89613664004262716 ) ) ;
#50533 = CARTESIAN_POINT ( 'NONE',  ( 0.5988103622719987973, 34.44344971428028401, -33.58571533649124774 ) ) ;
#50534 = VERTEX_POINT ( 'NONE', #39496 ) ;
#50535 = ORIENTED_EDGE ( 'NONE', *, *, #25234, .T. ) ;
#50536 = DIRECTION ( 'NONE',  ( -1.000000000000000000, -0.000000000000000000, -0.000000000000000000 ) ) ;
#50537 = CARTESIAN_POINT ( 'NONE',  ( 0.5998501479064708430, 12.95623334615502387, -46.33007877220726556 ) ) ;
#50538 = VERTEX_POINT ( 'NONE', #24753 ) ;
#50539 = ORIENTED_EDGE ( 'NONE', *, *, #34041, .F. ) ;
#50540 = CARTESIAN_POINT ( 'NONE',  ( 5.896782393890504181, -19.39652907507971236, -5.319844614046497000 ) ) ;
#50541 = CARTESIAN_POINT ( 'NONE',  ( 0.7048096507298635682, -33.41730025321778186, 34.61049487267002434 ) ) ;
#50542 = CARTESIAN_POINT ( 'NONE',  ( 5.910764540655177868, -11.94262894392618435, 16.18254777149937951 ) ) ;
#50543 = ORIENTED_EDGE ( 'NONE', *, *, #7545, .F. ) ;
#50544 = CARTESIAN_POINT ( 'NONE',  ( -6.016104459813371719, -2.454244026261222622, 18.68271063303494017 ) ) ;
#50545 = DIRECTION ( 'NONE',  ( 0.1024043820194936449, -0.9946559125373960475, 0.01315135725336192239 ) ) ;
#50546 = EDGE_CURVE ( 'NONE', #42276, #14894, #11278, .T. ) ;
#50547 = AXIS2_PLACEMENT_3D ( 'NONE', #31143, #60559, #12681 ) ;
#50548 = CARTESIAN_POINT ( 'NONE',  ( -1.500000000000001332, 0.000000000000000000, 0.000000000000000000 ) ) ;
#50549 = ADVANCED_FACE ( 'NONE', ( #29441 ), #46349, .F. ) ;
#50550 = ORIENTED_EDGE ( 'NONE', *, *, #4798, .F. ) ;
#50551 = ORIENTED_EDGE ( 'NONE', *, *, #44868, .F. ) ;
#50552 = EDGE_CURVE ( 'NONE', #26818, #10962, #12075, .T. ) ;
#50553 = CARTESIAN_POINT ( 'NONE',  ( 5.981074661064941900, 7.846517100474821760, -18.96560215432008789 ) ) ;
#50554 = VECTOR ( 'NONE', #39481, 1000.000000000000000 ) ;
#50555 = VERTEX_POINT ( 'NONE', #10979 ) ;
#50556 = CARTESIAN_POINT ( 'NONE',  ( 5.960221823109900008, 14.51763960716778357, -14.50993159119795628 ) ) ;
#50557 = CARTESIAN_POINT ( 'NONE',  ( 0.8744876279028263033, 41.62483489565955352, -26.03311679934954626 ) ) ;
#50558 = CARTESIAN_POINT ( 'NONE',  ( 0.6009452777970410997, 33.70725232128892657, -34.32439724343003462 ) ) ;
#50559 = EDGE_CURVE ( 'NONE', #6090, #24495, #57934, .T. ) ;
#50560 = CARTESIAN_POINT ( 'NONE',  ( 0.5806925824938499181, -38.96949031362449745, 26.08833430941674436 ) ) ;
#50561 = CARTESIAN_POINT ( 'NONE',  ( 0.5800708119828343889, -17.74761857127099063, 44.48635609075551400 ) ) ;
#50562 = VECTOR ( 'NONE', #1256, 1000.000000000000114 ) ;
#50563 = ORIENTED_EDGE ( 'NONE', *, *, #4012, .F. ) ;
#50564 = CARTESIAN_POINT ( 'NONE',  ( -6.063463321072276813, 19.09660126457258045, -2.477957348582642272 ) ) ;
#50565 = FACE_OUTER_BOUND ( 'NONE', #8743, .T. ) ;
#50566 = CARTESIAN_POINT ( 'NONE',  ( 0.5804410086790514622, 42.96136033320044589, 18.81067170986479553 ) ) ;
#50567 = VERTEX_POINT ( 'NONE', #58551 ) ;
#50568 = CARTESIAN_POINT ( 'NONE',  ( 1.000110580585053865, -21.99348401176059653, -35.67497924030694634 ) ) ;
#50569 = DIRECTION ( 'NONE',  ( -1.000000000000000000, -0.000000000000000000, -0.000000000000000000 ) ) ;
#50570 =( NAMED_UNIT ( * ) SI_UNIT ( $, .STERADIAN. ) SOLID_ANGLE_UNIT ( ) );
#50571 = EDGE_CURVE ( 'NONE', #18458, #53617, #48658, .T. ) ;
#50572 = EDGE_LOOP ( 'NONE', ( #37027, #27117, #24820, #39619 ) ) ;
#50573 = DIRECTION ( 'NONE',  ( -1.000000000000000000, -1.836909530733573776E-16, 1.925929944387235579E-32 ) ) ;
#50574 = EDGE_CURVE ( 'NONE', #25700, #44327, #1541, .T. ) ;
#50575 = CARTESIAN_POINT ( 'NONE',  ( 0.6031357023905875581, -41.68407605450330067, 24.01594909943193912 ) ) ;
#50576 =( BOUNDED_SURFACE ( )  B_SPLINE_SURFACE ( 3, 1, ( 
 ( #8150, #2195 ),
 ( #27265, #26640 ),
 ( #16961, #12258 ),
 ( #21333, #3432 ) ),
 .UNSPECIFIED., .F., .F., .F. ) 
 B_SPLINE_SURFACE_WITH_KNOTS ( ( 4, 4 ),
 ( 2, 2 ),
 ( 0.000000000000000000, 1.000000000000000000 ),
 ( 0.000000000000000000, 1.000000000000000000 ),
 .UNSPECIFIED. ) 
 GEOMETRIC_REPRESENTATION_ITEM ( )  RATIONAL_B_SPLINE_SURFACE ( (
 ( 1.000000000000000000, 1.000000000000000000),
 ( 0.7269869731126817891, 0.9931720237060910339),
 ( 0.7269869731126817891, 0.9931720237060910339),
 ( 1.000000000000000000, 1.000000000000000000) ) ) 
 REPRESENTATION_ITEM ( '' )  SURFACE ( )  );
#50577 = CARTESIAN_POINT ( 'NONE',  ( 0.6008123274975392114, -43.00034267269872146, 23.71761120325872341 ) ) ;
#50578 = CARTESIAN_POINT ( 'NONE',  ( 0.2885700199627512785, 42.63514063525626341, -6.424755504217793955 ) ) ;
#50579 = CARTESIAN_POINT ( 'NONE',  ( -69.95594261585600293, 0.000000000000000000, 0.000000000000000000 ) ) ;
#50580 = CARTESIAN_POINT ( 'NONE',  ( 3.680974057930773924, -40.59247216052836649, -25.57193971028145540 ) ) ;
#50581 = CARTESIAN_POINT ( 'NONE',  ( 1.231276596079881047, 24.17959027891106416, 34.24360064248583768 ) ) ;
#50582 = CARTESIAN_POINT ( 'NONE',  ( 0.2279481005628795909, 36.55606629206238267, 24.70136644647927682 ) ) ;
#50583 = ORIENTED_EDGE ( 'NONE', *, *, #34078, .T. ) ;
#50584 = CARTESIAN_POINT ( 'NONE',  ( 0.6001305935487422083, -5.760103278698371021, 47.76436356026957952 ) ) ;
#50585 = CARTESIAN_POINT ( 'NONE',  ( 4.962356264823609031, 37.75702904547822669, -18.59145920903629090 ) ) ;
#50586 = FACE_OUTER_BOUND ( 'NONE', #11819, .T. ) ;
#50587 = FACE_OUTER_BOUND ( 'NONE', #46264, .T. ) ;
#50588 = B_SPLINE_CURVE_WITH_KNOTS ( 'NONE', 3,
 ( #34144, #24414, #53219, #43548 ),
 .UNSPECIFIED., .F., .F.,
 ( 4, 4 ),
 ( 3.252606517456513302E-19, 0.004446298630425088438 ),
 .UNSPECIFIED. ) ;
#50589 = CARTESIAN_POINT ( 'NONE',  ( 0.3676999524040366896, -11.75791688508890331, 42.51707861373098041 ) ) ;
#50590 = CARTESIAN_POINT ( 'NONE',  ( 0.9775691876210974574, -31.33375233628529699, 27.83037321917057128 ) ) ;
#50591 = SHAPE_DEFINITION_REPRESENTATION ( #45814, #6760 ) ;
#50592 = CARTESIAN_POINT ( 'NONE',  ( 0.7242003506639999033, -2.392178275000814036, -49.04374738156375457 ) ) ;
#50593 = EDGE_CURVE ( 'NONE', #14207, #473, #22480, .T. ) ;
#50594 = CARTESIAN_POINT ( 'NONE',  ( 0.6030672727741701600, 41.70584815505888798, -23.97812608463489426 ) ) ;
#50595 = DIRECTION ( 'NONE',  ( 0.000000000000000000, 0.000000000000000000, 1.000000000000000000 ) ) ;
#50597 = ORIENTED_EDGE ( 'NONE', *, *, #28467, .F. ) ;
#50596 = CARTESIAN_POINT ( 'NONE',  ( 0.8557997880470690211, -38.55640757422419540, -28.43566216845010075 ) ) ;
#50598 = VERTEX_POINT ( 'NONE', #7471 ) ;
#50599 = VECTOR ( 'NONE', #20894, 1000.000000000000114 ) ;
#50600 = CARTESIAN_POINT ( 'NONE',  ( 1.231276596079881935, 3.353048872156085825, 41.78556968953515849 ) ) ;
#50601 = CARTESIAN_POINT ( 'NONE',  ( 0.5817217712918323347, -8.248776971688084103, 46.16484195228790810 ) ) ;
#50602 = CARTESIAN_POINT ( 'NONE',  ( 2.526552050251863246, -1.212569781798230162, 42.96196914573631886 ) ) ;
#50603 = ORIENTED_EDGE ( 'NONE', *, *, #10609, .T. ) ;
#50604 = CARTESIAN_POINT ( 'NONE',  ( 4.956653778116966613, 0.000000000000000000, 0.000000000000000000 ) ) ;
#50605 = CARTESIAN_POINT ( 'NONE',  ( 0.1098349054025746924, 41.70974743324814682, -10.95525583467232700 ) ) ;
#50606 = B_SPLINE_CURVE_WITH_KNOTS ( 'NONE', 3,
 ( #11913, #39256, #48623, #21592, #45120, #5680, #55092, #59801, #24829, #50099, #11587, #2776, #19835, #2468, #7465, #58305 ),
 .UNSPECIFIED., .F., .F.,
 ( 4, 3, 3, 3, 3, 4 ),
 ( 2.221635811791082109E-17, 0.0002618515315864383447, 0.0003927756766341984249, 0.0005236998216950556131, 0.0007855159896329916335, 0.001047349442285925268 ),
 .UNSPECIFIED. ) ;
#50607 = ORIENTED_EDGE ( 'NONE', *, *, #28567, .F. ) ;
#50608 = ORIENTED_EDGE ( 'NONE', *, *, #23382, .F. ) ;
#50609 = CARTESIAN_POINT ( 'NONE',  ( 4.956445790443988031, 0.000000000000000000, 0.000000000000000000 ) ) ;
#50610 = CIRCLE ( 'NONE', #613, 43.08621763946400307 ) ;
#50611 = CARTESIAN_POINT ( 'NONE',  ( 0.1100247026804066219, -39.77655614012843444, -16.65964013375371877 ) ) ;
#50612 = DIRECTION ( 'NONE',  ( -1.000000000000000000, -0.000000000000000000, -0.000000000000000000 ) ) ;
#50613 = VERTEX_POINT ( 'NONE', #22528 ) ;
#50614 = CARTESIAN_POINT ( 'NONE',  ( 3.050102900204245682, -43.95621292022238435, 1.810136704819465203 ) ) ;
#50615 = CARTESIAN_POINT ( 'NONE',  ( 0.1157991065609915438, -42.66035988082465025, -11.27102747650922154 ) ) ;
#50616 = CARTESIAN_POINT ( 'NONE',  ( 0.3622758884714600280, -34.70015533914845918, 25.58609868863709380 ) ) ;
#50617 = CARTESIAN_POINT ( 'NONE',  ( 2.281351352603289140, -38.84542754822344079, 28.15073776031352537 ) ) ;
#50618 = CARTESIAN_POINT ( 'NONE',  ( 4.291220156522059348, -11.88564107118027025, -45.58640733412503465 ) ) ;
#50619 = EDGE_CURVE ( 'NONE', #15688, #26015, #56081, .T. ) ;
#50620 = ORIENTED_EDGE ( 'NONE', *, *, #17148, .T. ) ;
#50621 = CARTESIAN_POINT ( 'NONE',  ( -6.001507490154111224, 18.68062548815625945, 2.475062734132503550 ) ) ;
#50622 = VERTEX_POINT ( 'NONE', #26598 ) ;
#50623 = CARTESIAN_POINT ( 'NONE',  ( 0.5998501479064699549, -47.76154736470754614, -5.759754759340617092 ) ) ;
#50624 = CARTESIAN_POINT ( 'NONE',  ( 0.3622758884714730732, 34.70015533914794759, 25.58609868863780434 ) ) ;
#50625 = EDGE_CURVE ( 'NONE', #50198, #31680, #2262, .T. ) ;
#50626 = CARTESIAN_POINT ( 'NONE',  ( 4.967162193818129623, 32.10009971360071290, 28.74031574030022540 ) ) ;
#50627 = CARTESIAN_POINT ( 'NONE',  ( 4.303969348037258058, 43.57722561725987021, -20.38638383586072678 ) ) ;
#50628 = ORIENTED_EDGE ( 'NONE', *, *, #18407, .F. ) ;
#50629 = VERTEX_POINT ( 'NONE', #27221 ) ;
#50630 = CARTESIAN_POINT ( 'NONE',  ( 5.860006189529234355, 21.31760477694640343, -43.26650951066848449 ) ) ;
#50631 = CARTESIAN_POINT ( 'NONE',  ( 0.6031357023905874470, 44.46217339385169964, -18.36962560204173656 ) ) ;
#50632 = EDGE_LOOP ( 'NONE', ( #8478, #1135, #53340, #56059 ) ) ;
#50633 = CARTESIAN_POINT ( 'NONE',  ( -6.078726893082806448, 12.00325722817128771, 15.05708661006749338 ) ) ;
#50634 = ORIENTED_EDGE ( 'NONE', *, *, #32751, .F. ) ;
#50635 = CARTESIAN_POINT ( 'NONE',  ( -6.016761891674565099, 7.207804629151311815, 17.41015286184805078 ) ) ;
#50636 = VECTOR ( 'NONE', #39750, 999.9999999999998863 ) ;
#50637 = ORIENTED_EDGE ( 'NONE', *, *, #17018, .F. ) ;
#50638 = CARTESIAN_POINT ( 'NONE',  ( 4.962356264823608143, 30.91935898304044272, 28.55221248765537467 ) ) ;
#50639 = CARTESIAN_POINT ( 'NONE',  ( 0.7246131072078525470, -17.64706930304264176, -44.74808308960844272 ) ) ;
#50640 = EDGE_CURVE ( 'NONE', #38326, #13848, #53085, .T. ) ;
#50641 = AXIS2_PLACEMENT_3D ( 'NONE', #51094, #18228, #55179 ) ;
#50642 = CARTESIAN_POINT ( 'NONE',  ( 0.1158816050234198758, -43.76118062594752445, 5.648106897745077681 ) ) ;
#50643 = VERTEX_POINT ( 'NONE', #55097 ) ;
#50644 = CARTESIAN_POINT ( 'NONE',  ( 0.1147471544378676489, -27.75311504492739090, -34.30330587241221707 ) ) ;
#50645 = VECTOR ( 'NONE', #46512, 1000.000000000000000 ) ;
#50646 = DIRECTION ( 'NONE',  ( -0.07836865515943411409, 0.6131273243286226027, 0.7860872967108205600 ) ) ;
#50647 = EDGE_CURVE ( 'NONE', #48917, #5400, #24700, .T. ) ;
#50648 = CARTESIAN_POINT ( 'NONE',  ( 2.299652685299202304, 44.72136265055998905, -20.10675129242044434 ) ) ;
#50649 = EDGE_LOOP ( 'NONE', ( #40059, #306, #1754, #18190 ) ) ;
#50650 = ORIENTED_EDGE ( 'NONE', *, *, #32057, .F. ) ;
#50651 = LINE ( 'NONE', #35976, #6485 ) ;
#50652 = CARTESIAN_POINT ( 'NONE',  ( 0.9754292589017238280, -26.60990437553315147, 32.37654175510806454 ) ) ;
#50653 = CARTESIAN_POINT ( 'NONE',  ( 0.6064515330803567084, 27.24304339879380521, -38.17264625891847629 ) ) ;
#50654 = CARTESIAN_POINT ( 'NONE',  ( 0.2999999999999897193, -13.49666625504239192, -1.199999999999999956 ) ) ;
#50655 = B_SPLINE_CURVE_WITH_KNOTS ( 'NONE', 3,
 ( #13122, #36938, #37551, #32529 ),
 .UNSPECIFIED., .F., .F.,
 ( 4, 4 ),
 ( 4.336808689942017736E-19, 0.004444878191957702535 ),
 .UNSPECIFIED. ) ;
#50656 = CARTESIAN_POINT ( 'NONE',  ( 0.3622758884714730732, 41.85013935980087751, 10.35929834645937397 ) ) ;
#50657 = ORIENTED_EDGE ( 'NONE', *, *, #58313, .F. ) ;
#50658 = CONICAL_SURFACE ( 'NONE', #14693, 48.91267123290010943, 0.04450589592585339760 ) ;
#50659 = CARTESIAN_POINT ( 'NONE',  ( 0.1103310638050662013, 37.38800124003712000, -21.49083802119861630 ) ) ;
#50660 = CARTESIAN_POINT ( 'NONE',  ( 4.322998006666179727, -47.25487450103542386, 8.359821156455678803 ) ) ;
#50661 = VERTEX_POINT ( 'NONE', #50404 ) ;
#50662 = CARTESIAN_POINT ( 'NONE',  ( 0.9756950546413942771, -30.27237962848458963, 30.40918718457328040 ) ) ;
#50663 = CARTESIAN_POINT ( 'NONE',  ( -2.569797478183783568, 11.33042594333548436, -9.259773107242946111 ) ) ;
#50664 = CARTESIAN_POINT ( 'NONE',  ( 2.618530812446111078, -39.53489722556214758, 25.43066437516798217 ) ) ;
#50665 = CARTESIAN_POINT ( 'NONE',  ( 0.2940133293163011974, -38.03800459916556775, -22.34615751515019255 ) ) ;
#50666 = CARTESIAN_POINT ( 'NONE',  ( 2.282816707992308736, -45.75239461778012640, 10.64027035121241127 ) ) ;
#50667 = CARTESIAN_POINT ( 'NONE',  ( 5.960221823109900008, 18.96526051813980374, -7.849768660536363463 ) ) ;
#50668 = CARTESIAN_POINT ( 'NONE',  ( 0.9730545539215883499, -42.60426903087349615, -5.099196237955331057 ) ) ;
#50669 = EDGE_CURVE ( 'NONE', #33332, #6666, #26919, .T. ) ;
#50670 = LINE ( 'NONE', #42242, #31625 ) ;
#50671 = CARTESIAN_POINT ( 'NONE',  ( 0.2940135542859017570, -28.13058121184755578, -33.98398077587541621 ) ) ;
#50672 = DIRECTION ( 'NONE',  ( -1.000000000000000000, -0.000000000000000000, -0.000000000000000000 ) ) ;
#50673 = CARTESIAN_POINT ( 'NONE',  ( 3.783278058412225420, 12.79810311738853201, 41.09146792477071131 ) ) ;
#50674 = CARTESIAN_POINT ( 'NONE',  ( 0.8760168074886960365, 38.69913431881823129, -28.57146030081939969 ) ) ;
#50675 = CARTESIAN_POINT ( 'NONE',  ( 2.879087469061463178, 16.80966257193206914, 40.66370520502483998 ) ) ;
#50676 = CARTESIAN_POINT ( 'NONE',  ( 0.8560838555295223751, 44.99141268455589682, -13.27198623905683128 ) ) ;
#50677 = CARTESIAN_POINT ( 'NONE',  ( 0.7762783648524366198, -47.89627393592494542, 0.8897020150996511889 ) ) ;
#50678 = ORIENTED_EDGE ( 'NONE', *, *, #13745, .T. ) ;
#50679 = AXIS2_PLACEMENT_3D ( 'NONE', #21460, #50573, #6709 ) ;
#50680 = CARTESIAN_POINT ( 'NONE',  ( 0.1092355843206037486, 11.45151637801127542, -41.57624119012377406 ) ) ;
#50681 = CARTESIAN_POINT ( 'NONE',  ( 2.533389852662419894, -32.69955711577486568, -29.46505550929431649 ) ) ;
#50682 = COLOUR_RGB ( '', 0.40784314, 0.44705882, 0.49803922) ;
#50683 = CARTESIAN_POINT ( 'NONE',  ( 0.1129192098497455998, -38.20615368646939203, -22.07354996984027196 ) ) ;
#50684 = CARTESIAN_POINT ( 'NONE',  ( -4.000000000000000000, 2.309401076758496263, -0.3572655899081631503 ) ) ;
#50685 = VECTOR ( 'NONE', #15752, 1000.000000000000114 ) ;
#50686 = EDGE_LOOP ( 'NONE', ( #27897, #55481, #17140, #56366 ) ) ;
#50687 = CARTESIAN_POINT ( 'NONE',  ( 2.185380717157383579, -40.25241636799283640, 17.84832708140854152 ) ) ;
#50688 = CARTESIAN_POINT ( 'NONE',  ( 5.910764540655177868, 0.6565643306762071196, 20.10149650520694209 ) ) ;
#50689 = LINE ( 'NONE', #27209, #54517 ) ;
#50690 = VERTEX_POINT ( 'NONE', #17519 ) ;
#50691 =( BOUNDED_SURFACE ( )  B_SPLINE_SURFACE ( 3, 1, ( 
 ( #30059, #30995 ),
 ( #59482, #40418 ),
 ( #40734, #21595 ),
 ( #44815, #2470 ) ),
 .UNSPECIFIED., .F., .F., .F. ) 
 B_SPLINE_SURFACE_WITH_KNOTS ( ( 4, 4 ),
 ( 2, 2 ),
 ( 0.000000000000000000, 1.000000000000000000 ),
 ( 0.000000000000000000, 1.000000000000000000 ),
 .UNSPECIFIED. ) 
 GEOMETRIC_REPRESENTATION_ITEM ( )  RATIONAL_B_SPLINE_SURFACE ( (
 ( 1.000000000000000000, 1.000000000000000000),
 ( 0.7211978278499968642, 0.9934217856018975334),
 ( 0.7211978278499968642, 0.9934217856018975334),
 ( 1.000000000000000000, 1.000000000000000000) ) ) 
 REPRESENTATION_ITEM ( '' )  SURFACE ( )  );
#50692 = CARTESIAN_POINT ( 'NONE',  ( 3.238931869106854489, 7.419701784410564827, 42.34694073502593170 ) ) ;
#50693 = EDGE_CURVE ( 'NONE', #43662, #19259, #12839, .T. ) ;
#50694 = ORIENTED_EDGE ( 'NONE', *, *, #25283, .F. ) ;
#50695 = CONICAL_SURFACE ( 'NONE', #40729, 47.09074272231896430, 0.04450589592586084303 ) ;
#50696 = CARTESIAN_POINT ( 'NONE',  ( 3.660176727303394717, 48.00143922595156454, 1.881607889987920501 ) ) ;
#50697 = CARTESIAN_POINT ( 'NONE',  ( 1.084202172485504434E-14, 4.618802153517020059, -5.242734410091827613 ) ) ;
#50698 = ORIENTED_EDGE ( 'NONE', *, *, #45527, .T. ) ;
#50699 = CARTESIAN_POINT ( 'NONE',  ( -6.077587904424778920, -16.13490349385135758, 10.51003856501172606 ) ) ;
#50701 = ORIENTED_EDGE ( 'NONE', *, *, #656, .F. ) ;
#50700 = EDGE_CURVE ( 'NONE', #47799, #19827, #52299, .T. ) ;
#50702 = CARTESIAN_POINT ( 'NONE',  ( 0.8560838555295158248, 42.82099363437792050, 19.15033519931955297 ) ) ;
#50703 = CARTESIAN_POINT ( 'NONE',  ( 0.1102144999581332885, -26.15241010113000542, -34.28951223307520735 ) ) ;
#50704 = AXIS2_PLACEMENT_3D ( 'NONE', #21253, #44774, #26248 ) ;
#50705 = ORIENTED_EDGE ( 'NONE', *, *, #54052, .F. ) ;
#50706 = DIRECTION ( 'NONE',  ( -0.07439287786467650709, 0.7830499462674596067, -0.6174937095821624311 ) ) ;
#50707 = EDGE_CURVE ( 'NONE', #61564, #15612, #2304, .T. ) ;
#50708 = ORIENTED_EDGE ( 'NONE', *, *, #9257, .T. ) ;
#50709 = CARTESIAN_POINT ( 'NONE',  ( 0.5832367798473401255, -37.83194459509889640, -29.37285281143879700 ) ) ;
#50710 = ORIENTED_EDGE ( 'NONE', *, *, #41440, .F. ) ;
#50711 = ORIENTED_EDGE ( 'NONE', *, *, #12906, .T. ) ;
#50712 = CARTESIAN_POINT ( 'NONE',  ( 5.838029081930955932, 38.93046761018045032, 26.74852799324872876 ) ) ;
#50713 = FACE_OUTER_BOUND ( 'NONE', #1433, .T. ) ;
#50714 = DIRECTION ( 'NONE',  ( -0.000000000000000000, -0.000000000000000000, -1.000000000000000000 ) ) ;
#50715 = CARTESIAN_POINT ( 'NONE',  ( 0.8554163680231816613, -44.01281378489805007, 16.25046755781837149 ) ) ;
#50716 = CARTESIAN_POINT ( 'NONE',  ( 4.975610109902397937, -46.23629923292363486, -15.95788333023269878 ) ) ;
#50717 = ORIENTED_EDGE ( 'NONE', *, *, #11664, .F. ) ;
#50718 = CARTESIAN_POINT ( 'NONE',  ( 4.975801465491694664, -3.702618843597810905, 47.76942479135478692 ) ) ;
#50719 = CARTESIAN_POINT ( 'NONE',  ( 0.9784957157296378938, -17.42937915973441676, 38.11233132594468032 ) ) ;
#50720 = EDGE_CURVE ( 'NONE', #35039, #40264, #41145, .T. ) ;
#50721 = CARTESIAN_POINT ( 'NONE',  ( 0.7764146366350260786, -34.18255388834246844, 32.11842902975998726 ) ) ;
#50722 = ORIENTED_EDGE ( 'NONE', *, *, #48457, .T. ) ;
#50723 = B_SPLINE_CURVE_WITH_KNOTS ( 'NONE', 3,
 ( #22919, #32626, #13520, #50252, #32943, #17064 ),
 .UNSPECIFIED., .F., .F.,
 ( 4, 2, 4 ),
 ( 1.267283937151336631E-16, 0.0002450741128632353237, 0.0004901482257263439042 ),
 .UNSPECIFIED. ) ;
#50724 = EDGE_LOOP ( 'NONE', ( #34336, #56594, #55380, #25382 ) ) ;
#50725 = CARTESIAN_POINT ( 'NONE',  ( 0.9754642270333674370, 34.14824330022369026, -25.98138239028824259 ) ) ;
#50726 = CARTESIAN_POINT ( 'NONE',  ( 2.648799415243708655, 23.90046839033397319, 42.81687837771741556 ) ) ;
#50727 = CARTESIAN_POINT ( 'NONE',  ( 0.5806925824938502512, -30.69245420804159252, -35.45695442407362208 ) ) ;
#50728 = VERTEX_POINT ( 'NONE', #18763 ) ;
#50729 = DIRECTION ( 'NONE',  ( -0.07500201931887529039, 0.7741482765856609882, -0.6285452592753698609 ) ) ;
#50730 = CARTESIAN_POINT ( 'NONE',  ( 5.894904586330512508, -2.014437969560215702, -20.01178282233836470 ) ) ;
#50731 = CONICAL_SURFACE ( 'NONE', #26722, 42.92674063221959813, 1.485477209440487556 ) ;
#50732 = MECHANICAL_DESIGN_GEOMETRIC_PRESENTATION_REPRESENTATION (  '', ( #34752 ), #45759 ) ;
#50733 = ORIENTED_EDGE ( 'NONE', *, *, #17549, .T. ) ;
#50735 = CARTESIAN_POINT ( 'NONE',  ( 0.7048096507298635682, 38.67623024744010252, 28.61383451045712079 ) ) ;
#50734 = AXIS2_PLACEMENT_3D ( 'NONE', #54317, #36188, #25840 ) ;
#50736 = ORIENTED_EDGE ( 'NONE', *, *, #2954, .F. ) ;
#50737 = TOROIDAL_SURFACE ( 'NONE', #23741, 2.700000000000000622, 0.2000000000000000111 ) ;
#50738 = CARTESIAN_POINT ( 'NONE',  ( 2.643462169533613793, 30.32726672320750438, 37.25264019563424256 ) ) ;
#50739 = CARTESIAN_POINT ( 'NONE',  ( 0.7056313189692714483, -44.02267996129995709, 16.17876055149217507 ) ) ;
#50740 = CARTESIAN_POINT ( 'NONE',  ( 0.9784957157296367836, 9.488681859340672986, -40.82031324677200956 ) ) ;
#50741 = B_SPLINE_CURVE_WITH_KNOTS ( 'NONE', 3,
 ( #57367, #43955, #44259, #49228, #52686, #5058, #14502, #356, #989, #34843, #5667, #28887, #9785, #48010, #53910, #24187, #33609, #19507, #38622 ),
 .UNSPECIFIED., .F., .F.,
 ( 4, 3, 3, 3, 3, 3, 4 ),
 ( 3.469446951953614189E-18, 0.0002724573126191767855, 0.0004086839781548511335, 0.0005449106435901861483, 0.0006811373090491516747, 0.0008459866663933716512, 0.001010840725717212932 ),
 .UNSPECIFIED. ) ;
#50742 = PRESENTATION_STYLE_ASSIGNMENT (( #60750 ) ) ;
#50743 = CARTESIAN_POINT ( 'NONE',  ( 0.1064266379913938465, 39.62374453032494870, -17.02047542254809187 ) ) ;
#50744 = ORIENTED_EDGE ( 'NONE', *, *, #43405, .T. ) ;
#50745 = CARTESIAN_POINT ( 'NONE',  ( 1.227938101723756947, -41.23019537246717903, 11.92353943227934998 ) ) ;
#50746 = CARTESIAN_POINT ( 'NONE',  ( 5.959828726073459926, -16.28130559351273376, 12.49879082830540789 ) ) ;
#50747 = CARTESIAN_POINT ( 'NONE',  ( 0.1129192098497455998, 9.345467776858411568, 43.12324222292260600 ) ) ;
#50748 = CARTESIAN_POINT ( 'NONE',  ( 2.156377650103387111, -0.2527589248780885978, 46.96604083475408942 ) ) ;
#50749 = CARTESIAN_POINT ( 'NONE',  ( 4.553261556744873317, -3.993093339917161977, 43.74465420371208069 ) ) ;
#50750 = EDGE_CURVE ( 'NONE', #40414, #46714, #54346, .T. ) ;
#50751 = CARTESIAN_POINT ( 'NONE',  ( 0.5819845079324650339, 5.801222053075765217, -47.54334065046000291 ) ) ;
#50752 = CARTESIAN_POINT ( 'NONE',  ( 2.528190830796653188, 19.10480206427283179, 37.37995016366345880 ) ) ;
#50753 = CARTESIAN_POINT ( 'NONE',  ( 3.783198216974394512, 27.54889409286126778, -33.06596988314768026 ) ) ;
#50754 = EDGE_CURVE ( 'NONE', #217, #57622, #3697, .T. ) ;
#50755 =( BOUNDED_SURFACE ( )  B_SPLINE_SURFACE ( 3, 1, ( 
 ( #41563, #28906 ),
 ( #60625, #22438 ),
 ( #29519, #377 ),
 ( #28595, #10430 ) ),
 .UNSPECIFIED., .F., .F., .F. ) 
 B_SPLINE_SURFACE_WITH_KNOTS ( ( 4, 4 ),
 ( 2, 2 ),
 ( 0.000000000000000000, 1.000000000000000000 ),
 ( 0.000000000000000000, 1.000000000000000000 ),
 .UNSPECIFIED. ) 
 GEOMETRIC_REPRESENTATION_ITEM ( )  RATIONAL_B_SPLINE_SURFACE ( (
 ( 1.000000000000000000, 1.000000000000000000),
 ( 0.9953485035131437453, 0.8621029689291523912),
 ( 0.9953485035131437453, 0.8621029689291523912),
 ( 1.000000000000000000, 1.000000000000000000) ) ) 
 REPRESENTATION_ITEM ( '' )  SURFACE ( )  );
#50756 = ADVANCED_FACE ( 'NONE', ( #13440 ), #30549, .F. ) ;
#50757 = AXIS2_PLACEMENT_3D ( 'NONE', #41317, #36932, #55995 ) ;
#50758 = CARTESIAN_POINT ( 'NONE',  ( 0.5980271706414711508, 10.24496086146881169, 48.03217692119142868 ) ) ;
#50759 = CARTESIAN_POINT ( 'NONE',  ( -6.063463321072278589, -16.14731216720877782, 10.49212858547689109 ) ) ;
#50760 = EDGE_LOOP ( 'NONE', ( #11692, #60099, #5551, #14770 ) ) ;
#50761 = CARTESIAN_POINT ( 'NONE',  ( 0.8557997880470599172, 13.27832040216703469, -46.03118133706011861 ) ) ;
#50762 = LINE ( 'NONE', #36086, #42545 ) ;
#50763 = DIRECTION ( 'NONE',  ( 0.000000000000000000, 0.000000000000000000, 1.000000000000000000 ) ) ;
#50764 = VERTEX_POINT ( 'NONE', #19373 ) ;
#50765 = CARTESIAN_POINT ( 'NONE',  ( 4.962356264823608143, -40.47344704301786322, -11.53844366967987334 ) ) ;
#50766 = CARTESIAN_POINT ( 'NONE',  ( 5.965394784446458765, 10.25014670152115137, -17.78272165951790740 ) ) ;
#50767 =( BOUNDED_SURFACE ( )  B_SPLINE_SURFACE ( 3, 1, ( 
 ( #42941, #51996 ),
 ( #28191, #47312 ),
 ( #23494, #14425 ),
 ( #42624, #61685 ) ),
 .UNSPECIFIED., .F., .F., .F. ) 
 B_SPLINE_SURFACE_WITH_KNOTS ( ( 4, 4 ),
 ( 2, 2 ),
 ( 0.000000000000000000, 1.000000000000000000 ),
 ( 0.000000000000000000, 1.000000000000000000 ),
 .UNSPECIFIED. ) 
 GEOMETRIC_REPRESENTATION_ITEM ( )  RATIONAL_B_SPLINE_SURFACE ( (
 ( 1.000000000000000000, 1.000000000000000000),
 ( 0.9953040768229005630, 0.8617119497784937465),
 ( 0.9953040768229005630, 0.8617119497784937465),
 ( 1.000000000000000000, 1.000000000000000000) ) ) 
 REPRESENTATION_ITEM ( '' )  SURFACE ( )  );
#50768 = ORIENTED_EDGE ( 'NONE', *, *, #17839, .F. ) ;
#50769 = DIRECTION ( 'NONE',  ( 0.000000000000000000, 0.000000000000000000, 1.000000000000000000 ) ) ;
#50770 = B_SPLINE_CURVE_WITH_KNOTS ( 'NONE', 3,
 ( #10168, #8083, #19578, #434 ),
 .UNSPECIFIED., .F., .F.,
 ( 4, 4 ),
 ( 0.000000000000000000, 0.005013413432710152849 ),
 .UNSPECIFIED. ) ;
#50771 = CARTESIAN_POINT ( 'NONE',  ( 4.960156602257182357, 45.42786611289328391, -9.558288641081281511 ) ) ;
#50772 = CARTESIAN_POINT ( 'NONE',  ( 2.533389852662419894, -10.99890053681963664, 42.62012105467048428 ) ) ;
#50773 = EDGE_CURVE ( 'NONE', #36851, #1494, #1483, .T. ) ;
#50774 = ORIENTED_EDGE ( 'NONE', *, *, #29755, .T. ) ;
#50775 = CARTESIAN_POINT ( 'NONE',  ( 0.6031357023905875581, 29.25135304925229818, 38.19275261685284306 ) ) ;
#50776 = CIRCLE ( 'NONE', #42805, 2.500000000000002220 ) ;
#50778 = EDGE_LOOP ( 'NONE', ( #46078, #39357, #28232, #30996 ) ) ;
#50777 = EDGE_CURVE ( 'NONE', #32408, #33003, #33480, .T. ) ;
#50779 = ORIENTED_EDGE ( 'NONE', *, *, #9635, .F. ) ;
#50780 = CARTESIAN_POINT ( 'NONE',  ( 0.7056759521544978542, 21.79701521802849129, 41.52877263659524232 ) ) ;
#50781 = ORIENTED_EDGE ( 'NONE', *, *, #4069, .T. ) ;
#50782 = CARTESIAN_POINT ( 'NONE',  ( 5.960221823109900008, -2.684531185214278803, -20.34928172836729843 ) ) ;
#50783 = PRODUCT_DEFINITION_SHAPE ( 'NONE', 'NONE',  #26005 ) ;
#50784 = ORIENTED_EDGE ( 'NONE', *, *, #42946, .T. ) ;
#50785 = CARTESIAN_POINT ( 'NONE',  ( 4.291220156522060236, 18.92432707711487438, 43.14230918696951278 ) ) ;
#50786 = EDGE_CURVE ( 'NONE', #53183, #61378, #60508, .T. ) ;
#50787 = APPLICATION_CONTEXT ( 'automotive_design' ) ;
#50788 = CARTESIAN_POINT ( 'NONE',  ( 0.9740398440564311811, 16.80263250099888239, 39.48175649279239252 ) ) ;
#50789 = ORIENTED_EDGE ( 'NONE', *, *, #51528, .T. ) ;
#50790 = LINE ( 'NONE', #56104, #36496 ) ;
#50791 = CIRCLE ( 'NONE', #17813, 48.09070567114147110 ) ;
#50792 = CARTESIAN_POINT ( 'NONE',  ( 4.956653778117001252, 45.71126949320271393, -14.93973939759840519 ) ) ;
#50793 = CARTESIAN_POINT ( 'NONE',  ( 3.559346040607745287, -37.26281748359819801, 23.34336553982817364 ) ) ;
#50794 = CARTESIAN_POINT ( 'NONE',  ( 0.5824935313925942992, -29.99830834406015256, 36.04635451121971812 ) ) ;
#50795 = ORIENTED_EDGE ( 'NONE', *, *, #38228, .T. ) ;
#50796 = DIRECTION ( 'NONE',  ( 0.000000000000000000, 0.000000000000000000, 1.000000000000000000 ) ) ;
#50797 = ADVANCED_FACE ( 'NONE', ( #27839 ), #37001, .F. ) ;
#50798 = VERTEX_POINT ( 'NONE', #61331 ) ;
#50799 = VECTOR ( 'NONE', #45681, 1000.000000000000114 ) ;
#50800 = CARTESIAN_POINT ( 'NONE',  ( 0.9730545539215883499, -42.47233286818612896, -6.101350888305089093 ) ) ;
#50801 = VERTEX_POINT ( 'NONE', #19078 ) ;
#50802 = DIRECTION ( 'NONE',  ( -0.000000000000000000, -0.000000000000000000, 1.000000000000000000 ) ) ;
#50803 = CARTESIAN_POINT ( 'NONE',  ( 3.390910168358336918, 13.32450449336170095, -41.91127195087285173 ) ) ;
#50804 = EDGE_LOOP ( 'NONE', ( #10579, #57334, #1927, #9875 ) ) ;
#50805 = CARTESIAN_POINT ( 'NONE',  ( 0.5786265663353196143, -6.967625775956046041, 47.39171391660389077 ) ) ;
#50806 = CARTESIAN_POINT ( 'NONE',  ( 0.6001305935487315502, 46.60388846085722747, -11.94532529598329518 ) ) ;
#50807 = CARTESIAN_POINT ( 'NONE',  ( 0.6021448801613057400, 27.88052149016963810, 40.42545806868656655 ) ) ;
#50808 = CARTESIAN_POINT ( 'NONE',  ( 0.6031356219577719280, -41.70591683999489163, -23.97811961689673055 ) ) ;
#50809 = CIRCLE ( 'NONE', #54826, 47.91270532121795611 ) ;
#50810 = VERTEX_POINT ( 'NONE', #28443 ) ;
#50811 = ORIENTED_EDGE ( 'NONE', *, *, #17535, .T. ) ;
#50812 = CARTESIAN_POINT ( 'NONE',  ( 0.6845945791218023269, -0.7015599581314457822, 46.90324439033074810 ) ) ;
#50813 = CARTESIAN_POINT ( 'NONE',  ( 0.9775691876210974574, -41.83858028429363429, 2.422170263360079456 ) ) ;
#50814 = CARTESIAN_POINT ( 'NONE',  ( 0.9749527285493315709, -16.68386601451066653, 39.53206838353040808 ) ) ;
#50815 = CARTESIAN_POINT ( 'NONE',  ( 0.2285344041767092271, -18.55084289203973924, -40.02958154028485893 ) ) ;
#50816 = B_SPLINE_CURVE_WITH_KNOTS ( 'NONE', 3,
 ( #4198, #61523, #37774, #52136 ),
 .UNSPECIFIED., .F., .F.,
 ( 4, 4 ),
 ( 0.000000000000000000, 0.004445488388166994251 ),
 .UNSPECIFIED. ) ;
#50817 = CARTESIAN_POINT ( 'NONE',  ( 4.060580049360325461, 12.02155469950848676, 42.27233039431271067 ) ) ;
#50818 = CARTESIAN_POINT ( 'NONE',  ( 1.231276596079887264, 20.88402890667827450, 36.34740854095507245 ) ) ;
#50819 = AXIS2_PLACEMENT_3D ( 'NONE', #49949, #26136, #45273 ) ;
#50820 = CARTESIAN_POINT ( 'NONE',  ( -6.001507490154110336, 2.475062734132436493, 18.68062548815627011 ) ) ;
#50821 = AXIS2_PLACEMENT_3D ( 'NONE', #48835, #58213, #49759 ) ;
#50822 = CARTESIAN_POINT ( 'NONE',  ( 0.9968887458511649369, 4.948372828380764865, 42.62316256128683989 ) ) ;
#50823 = DIRECTION ( 'NONE',  ( -1.000000000000000000, -3.673819061467147552E-16, 1.925929944387235306E-32 ) ) ;
#50824 = EDGE_CURVE ( 'NONE', #60124, #16733, #38151, .T. ) ;
#50825 = CARTESIAN_POINT ( 'NONE',  ( -2.708315649062916552, 1.648584381067041527, -14.54141329178160547 ) ) ;
#50826 = CARTESIAN_POINT ( 'NONE',  ( 0.1092565886968783623, -21.29292791075612712, 37.50119754628571656 ) ) ;
#50827 = CARTESIAN_POINT ( 'NONE',  ( 0.5837799406558229487, -13.98113914491203502, -44.76350408298939243 ) ) ;
#50828 = CARTESIAN_POINT ( 'NONE',  ( 5.860006189529234355, -48.12869875779311002, 3.171667470662350663 ) ) ;
#50830 = EDGE_CURVE ( 'NONE', #42440, #50327, #47781, .T. ) ;
#50829 = CARTESIAN_POINT ( 'NONE',  ( 0.9785694773339237429, -22.73759263024291855, 35.20422257479631156 ) ) ;
#50831 = CARTESIAN_POINT ( 'NONE',  ( 0.1073791018717483448, -0.4849339620930353534, -43.12183934961191056 ) ) ;
#50832 = ADVANCED_FACE ( 'NONE', ( #14993 ), #44737, .F. ) ;
#50833 = CARTESIAN_POINT ( 'NONE',  ( 0.6028777368367060907, 16.87825420422721834, 46.11577131880761726 ) ) ;
#50834 = CARTESIAN_POINT ( 'NONE',  ( 0.6031357023905875581, 46.47951061918811178, -12.40899271757790423 ) ) ;
#50835 = EDGE_CURVE ( 'NONE', #14950, #10066, #49313, .T. ) ;
#50837 = ORIENTED_EDGE ( 'NONE', *, *, #41923, .T. ) ;
#50836 = FACE_OUTER_BOUND ( 'NONE', #28365, .T. ) ;
#50838 = VERTEX_POINT ( 'NONE', #546 ) ;
#50839 = LINE ( 'NONE', #59931, #54881 ) ;
#50840 = CARTESIAN_POINT ( 'NONE',  ( 0.2885697896453094380, 31.05173034173371960, -29.91358794843029401 ) ) ;
#50841 = EDGE_CURVE ( 'NONE', #23496, #56700, #48478, .T. ) ;
#50842 = CARTESIAN_POINT ( 'NONE',  ( 1.227938101723747621, 6.439911493065174852, -42.43379953535178828 ) ) ;
#50843 = VERTEX_POINT ( 'NONE', #58171 ) ;
#50844 = EDGE_LOOP ( 'NONE', ( #21989, #19318, #994, #58312 ) ) ;
#50845 = CARTESIAN_POINT ( 'NONE',  ( 0.6252788684277241771, 36.94309652552172452, -32.35200071525177634 ) ) ;
#50846 = CARTESIAN_POINT ( 'NONE',  ( 3.376099380956838925, -12.50537924370748044, -4.829479641029388759 ) ) ;
#50847 =( GEOMETRIC_REPRESENTATION_CONTEXT ( 3 ) GLOBAL_UNCERTAINTY_ASSIGNED_CONTEXT ( ( #51151 ) ) GLOBAL_UNIT_ASSIGNED_CONTEXT ( ( #53813, #11882, #11558 ) ) REPRESENTATION_CONTEXT ( 'NONE', 'WORKASPACE' ) );
#50848 = EDGE_LOOP ( 'NONE', ( #32193, #43265, #49092, #61058 ) ) ;
#50849 = ORIENTED_EDGE ( 'NONE', *, *, #53036, .F. ) ;
#50850 = EDGE_CURVE ( 'NONE', #376, #50629, #6154, .T. ) ;
#50851 = CARTESIAN_POINT ( 'NONE',  ( 0.5809828226811553087, 47.89273459658653564, -0.5448590168534052092 ) ) ;
#50852 = MECHANICAL_DESIGN_GEOMETRIC_PRESENTATION_REPRESENTATION (  '', ( #15859 ), #17879 ) ;
#50853 = EDGE_CURVE ( 'NONE', #32810, #38419, #27366, .T. ) ;
#50854 = LINE ( 'NONE', #2615, #58969 ) ;
#50855 = CARTESIAN_POINT ( 'NONE',  ( 3.678748215320120529, 48.95863509520004442, 1.290296056930659629 ) ) ;
#50856 = ORIENTED_EDGE ( 'NONE', *, *, #9749, .F. ) ;
#50857 = CARTESIAN_POINT ( 'NONE',  ( 0.5980894510889448457, 6.974827154144098706, -47.60453381548686025 ) ) ;
#50858 = B_SPLINE_CURVE_WITH_KNOTS ( 'NONE', 3,
 ( #25493, #43720, #16115, #34607 ),
 .UNSPECIFIED., .F., .F.,
 ( 4, 4 ),
 ( 2.165040709395311621E-17, 0.004444306975806114161 ),
 .UNSPECIFIED. ) ;
#50859 = CARTESIAN_POINT ( 'NONE',  ( 0.1092565886968784317, 21.83052579204411003, 37.19081526480832878 ) ) ;
#50860 = ORIENTED_EDGE ( 'NONE', *, *, #6540, .F. ) ;
#50861 = VECTOR ( 'NONE', #10406, 1000.000000000000000 ) ;
#50862 = ORIENTED_EDGE ( 'NONE', *, *, #46023, .F. ) ;
#50863 = CARTESIAN_POINT ( 'NONE',  ( -2.601141883200665639, 3.756714151560036630, -14.44584806277766376 ) ) ;
#50864 = AXIS2_PLACEMENT_3D ( 'NONE', #59040, #44076, #49343 ) ;
#50865 = ORIENTED_EDGE ( 'NONE', *, *, #4570, .F. ) ;
#50866 = CARTESIAN_POINT ( 'NONE',  ( 0.5786265663353153954, -33.35675271369563433, 34.37803667029800181 ) ) ;
#50867 = CARTESIAN_POINT ( 'NONE',  ( -6.001507490154110336, -0.01557731607540145842, -18.84387066167321478 ) ) ;
#50868 = CARTESIAN_POINT ( 'NONE',  ( 4.691466044806103852, 29.14742760351109396, -33.74235639413297605 ) ) ;
#50869 = CARTESIAN_POINT ( 'NONE',  ( 0.5848930533535030563, 4.875316827623189297, -46.64230234688091059 ) ) ;
#50870 = CARTESIAN_POINT ( 'NONE',  ( 0.7413678028165010536, -43.84383547618206478, -4.712131418766086099 ) ) ;
#50871 =( BOUNDED_SURFACE ( )  B_SPLINE_SURFACE ( 3, 1, ( 
 ( #41826, #56194 ),
 ( #8267, #13307 ),
 ( #13011, #28011 ),
 ( #61498, #42437 ) ),
 .UNSPECIFIED., .F., .F., .F. ) 
 B_SPLINE_SURFACE_WITH_KNOTS ( ( 4, 4 ),
 ( 2, 2 ),
 ( 0.000000000000000000, 1.000000000000000000 ),
 ( 0.000000000000000000, 1.000000000000000000 ),
 .UNSPECIFIED. ) 
 GEOMETRIC_REPRESENTATION_ITEM ( )  RATIONAL_B_SPLINE_SURFACE ( (
 ( 1.000000000000000000, 1.000000000000000000),
 ( 0.7211978278499968642, 0.9934217856018975334),
 ( 0.7211978278499968642, 0.9934217856018975334),
 ( 1.000000000000000000, 1.000000000000000000) ) ) 
 REPRESENTATION_ITEM ( '' )  SURFACE ( )  );
#50872 = EDGE_CURVE ( 'NONE', #25685, #18352, #9708, .T. ) ;
#50873 = ORIENTED_EDGE ( 'NONE', *, *, #3730, .T. ) ;
#50874 = FACE_OUTER_BOUND ( 'NONE', #50049, .T. ) ;
#50875 = CARTESIAN_POINT ( 'NONE',  ( 5.901764892641288895, 7.772884649737204832, -48.34846152321248525 ) ) ;
#50876 = EDGE_CURVE ( 'NONE', #43165, #16494, #49403, .T. ) ;
#50877 = CARTESIAN_POINT ( 'NONE',  ( 2.648799415243696664, -9.190926635157635971, 48.16683849783737514 ) ) ;
#50878 = ORIENTED_EDGE ( 'NONE', *, *, #43902, .F. ) ;
#50879 = CARTESIAN_POINT ( 'NONE',  ( 0.1103878639767399972, 42.74915604780180445, -5.676988162228224333 ) ) ;
#50880 = CARTESIAN_POINT ( 'NONE',  ( 3.782542959838399721, -38.26640512950806539, 17.40459973285597428 ) ) ;
#50881 = CARTESIAN_POINT ( 'NONE',  ( 4.975610109902397937, 39.54077024310177535, -28.79195887257430897 ) ) ;
#50882 = CARTESIAN_POINT ( 'NONE',  ( 0.1313383488274124378, 30.03864748494545722, -30.94058105930532321 ) ) ;
#50883 = CIRCLE ( 'NONE', #11932, 0.2500000000000002220 ) ;
#50884 = ORIENTED_EDGE ( 'NONE', *, *, #58852, .F. ) ;
#50885 = CARTESIAN_POINT ( 'NONE',  ( 1.231276596079887264, -41.76121777166943616, 3.643825084340432952 ) ) ;
#50886 = CARTESIAN_POINT ( 'NONE',  ( 0.9762797500689124330, 20.58271139965541963, -36.50584578699964311 ) ) ;
#50887 = FACE_OUTER_BOUND ( 'NONE', #42024, .T. ) ;
#50888 = CARTESIAN_POINT ( 'NONE',  ( 5.894904586330512508, -13.98322986223360864, -14.45678714934895126 ) ) ;
#50890 = CARTESIAN_POINT ( 'NONE',  ( 0.3622758884714730732, -34.70015533914812522, -25.58609868863756276 ) ) ;
#50889 = PRODUCT_DEFINITION_FORMATION_WITH_SPECIFIED_SOURCE ( 'ANY', '', #6712, .NOT_KNOWN. ) ;
#50891 = CARTESIAN_POINT ( 'NONE',  ( 0.8744876279028263033, 10.05549467470504865, 48.05452192277508061 ) ) ;
#50892 = CARTESIAN_POINT ( 'NONE',  ( 0.5800708119828335008, -6.873289505980332059, -47.40012378203037002 ) ) ;
#50893 = CARTESIAN_POINT ( 'NONE',  ( 4.958415959904816539, 2.023024899602716253, 45.37743188059704380 ) ) ;
#50894 = CARTESIAN_POINT ( 'NONE',  ( 0.6029443199889047422, 41.15632221336601759, -26.78982612343718728 ) ) ;
#50895 = CARTESIAN_POINT ( 'NONE',  ( 0.3676999524040323597, 36.51379593394458567, 24.75264207750540635 ) ) ;
#50896 = ORIENTED_EDGE ( 'NONE', *, *, #20645, .T. ) ;
#50897 = CARTESIAN_POINT ( 'NONE',  ( 5.901764892641307547, -41.01701952799340489, -26.75061824481604944 ) ) ;
#50898 = DIRECTION ( 'NONE',  ( -1.000000000000000000, -0.000000000000000000, -0.000000000000000000 ) ) ;
#50899 = CARTESIAN_POINT ( 'NONE',  ( 4.549368137175248350, 0.000000000000000000, 0.000000000000000000 ) ) ;
#50900 = CARTESIAN_POINT ( 'NONE',  ( 4.975801465491695552, -3.702618843597113685, -47.76942479135485087 ) ) ;
#50901 = CARTESIAN_POINT ( 'NONE',  ( 0.7954190325252773475, -28.58653703871186025, 38.68220061605119753 ) ) ;
#50902 = CARTESIAN_POINT ( 'NONE',  ( 0.7954190325252807892, 17.60078418394994415, -44.76287681188613021 ) ) ;
#50904 = EDGE_CURVE ( 'NONE', #28712, #38682, #866, .T. ) ;
#50903 = CARTESIAN_POINT ( 'NONE',  ( 3.240649175237394708, -14.25852668140352364, 41.61681552297525144 ) ) ;
#50905 = DIRECTION ( 'NONE',  ( 0.000000000000000000, 0.000000000000000000, 1.000000000000000000 ) ) ;
#50906 = LINE ( 'NONE', #41233, #25418 ) ;
#50907 = EDGE_CURVE ( 'NONE', #6995, #14400, #5903, .T. ) ;
#50909 = ORIENTED_EDGE ( 'NONE', *, *, #13351, .F. ) ;
#50908 = DIRECTION ( 'NONE',  ( 0.000000000000000000, 0.000000000000000000, 1.000000000000000000 ) ) ;
#50910 = ORIENTED_EDGE ( 'NONE', *, *, #2605, .T. ) ;
#50911 = CARTESIAN_POINT ( 'NONE',  ( 0.5549461598389363592, -18.65190885362596518, -39.96653589670781059 ) ) ;
#50912 = CARTESIAN_POINT ( 'NONE',  ( 0.5834584762367746036, -7.979694474790339775, 46.21212465470713227 ) ) ;
#50913 = ADVANCED_FACE ( 'NONE', ( #48792 ), #26538, .F. ) ;
#50914 = CARTESIAN_POINT ( 'NONE',  ( 4.833616638992205949, -2.572717262757654666, -46.17873762321151077 ) ) ;
#50915 = ORIENTED_EDGE ( 'NONE', *, *, #20179, .F. ) ;
#50916 = CARTESIAN_POINT ( 'NONE',  ( 4.956445790443989807, 42.27038699792205279, 20.75457619864928205 ) ) ;
#50917 = CARTESIAN_POINT ( 'NONE',  ( -6.078457390727109555, 3.068934028528322866, 19.00989623764550629 ) ) ;
#50918 = CARTESIAN_POINT ( 'NONE',  ( 0.1100247026804066219, 5.797046384219859405, -42.73303500775681130 ) ) ;
#50919 = ORIENTED_EDGE ( 'NONE', *, *, #27732, .F. ) ;
#50920 = VERTEX_POINT ( 'NONE', #25291 ) ;
#50921 = DIRECTION ( 'NONE',  ( 0.000000000000000000, 0.000000000000000000, -1.000000000000000000 ) ) ;
#50922 = AXIS2_PLACEMENT_3D ( 'NONE', #1268, #29173, #35678 ) ;
#50923 = DIRECTION ( 'NONE',  ( 3.273063162220399693E-16, -1.000000000000000000, -5.236901059552639509E-15 ) ) ;
#50924 = CARTESIAN_POINT ( 'NONE',  ( 0.9788927965476016402, 32.80188811192217457, -26.08395577600753512 ) ) ;
#50925 = ORIENTED_EDGE ( 'NONE', *, *, #30885, .F. ) ;
#50926 = CARTESIAN_POINT ( 'NONE',  ( 2.225808406068902734, -0.2642358560988280480, -49.03513448940339714 ) ) ;
#50927 = B_SPLINE_CURVE_WITH_KNOTS ( 'NONE', 3,
 ( #21365, #26363, #59561, #45498, #35791, #17595 ),
 .UNSPECIFIED., .F., .F.,
 ( 4, 2, 4 ),
 ( 1.258037581941437391E-16, 0.0002450741128632354863, 0.0004901482257263450968 ),
 .UNSPECIFIED. ) ;
#50928 = CARTESIAN_POINT ( 'NONE',  ( 0.8560838555295158248, 36.24009790160309308, 29.78301761346479282 ) ) ;
#50929 = CARTESIAN_POINT ( 'NONE',  ( 0.3676999524040366896, 29.04098611012985742, -33.20499524279568249 ) ) ;
#50930 = CARTESIAN_POINT ( 'NONE',  ( 0.1154773475650540671, 33.71449497992789901, 28.46535540432504874 ) ) ;
#50931 = VERTEX_POINT ( 'NONE', #44437 ) ;
#50932 = CARTESIAN_POINT ( 'NONE',  ( 0.7044674535452954967, -31.27352687970100931, 37.86514544162644569 ) ) ;
#50933 = FACE_OUTER_BOUND ( 'NONE', #850, .T. ) ;
#50934 = B_SPLINE_CURVE_WITH_KNOTS ( 'NONE', 3,
 ( #17488, #30964, #11886, #2750, #17799, #36609 ),
 .UNSPECIFIED., .F., .F.,
 ( 4, 2, 4 ),
 ( 8.609910155989501895E-17, 0.0002293366620881465297, 0.0004586733241762069738 ),
 .UNSPECIFIED. ) ;
#50935 = EDGE_LOOP ( 'NONE', ( #836, #12854, #17655, #42049, #23751, #51782 ) ) ;
#50936 = CARTESIAN_POINT ( 'NONE',  ( 3.783198216974387851, -27.54889409286103330, 33.06596988314791474 ) ) ;
#50937 = CARTESIAN_POINT ( 'NONE',  ( 0.8744876279028263033, -6.955970791787605911, -48.60004650947661275 ) ) ;
#50938 = CARTESIAN_POINT ( 'NONE',  ( 0.5997462898726536595, 10.41743419021273631, 47.98988117339838055 ) ) ;
#50939 =( NAMED_UNIT ( * ) PLANE_ANGLE_UNIT ( ) SI_UNIT ( $, .RADIAN. ) );
#50940 = ORIENTED_EDGE ( 'NONE', *, *, #1727, .F. ) ;
#50941 = VERTEX_POINT ( 'NONE', #25600 ) ;
#50942 = CARTESIAN_POINT ( 'NONE',  ( 4.960156602257181468, -25.36362146861414146, 38.88108289790854855 ) ) ;
#50943 = DIRECTION ( 'NONE',  ( 1.000000000000000000, 1.836909530733573776E-16, -1.925929944387235579E-32 ) ) ;
#50944 = ORIENTED_EDGE ( 'NONE', *, *, #23218, .F. ) ;
#50945 = CARTESIAN_POINT ( 'NONE',  ( 1.088908134280554219, -15.69861202536780276, 39.93902428011485739 ) ) ;
#50946 =( BOUNDED_SURFACE ( )  B_SPLINE_SURFACE ( 3, 1, ( 
 ( #18408, #34060 ),
 ( #502, #19644 ),
 ( #57195, #19331 ),
 ( #61288, #42532 ) ),
 .UNSPECIFIED., .F., .F., .F. ) 
 B_SPLINE_SURFACE_WITH_KNOTS ( ( 4, 4 ),
 ( 2, 2 ),
 ( 0.000000000000000000, 1.000000000000000000 ),
 ( 0.000000000000000000, 1.000000000000000000 ),
 .UNSPECIFIED. ) 
 GEOMETRIC_REPRESENTATION_ITEM ( )  RATIONAL_B_SPLINE_SURFACE ( (
 ( 1.000000000000000000, 1.000000000000000000),
 ( 0.9952954269826590483, 0.8620686068821339365),
 ( 0.9952954269826590483, 0.8620686068821339365),
 ( 1.000000000000000000, 1.000000000000000000) ) ) 
 REPRESENTATION_ITEM ( '' )  SURFACE ( )  );
#50947 = B_SPLINE_CURVE_WITH_KNOTS ( 'NONE', 3,
 ( #21812, #54063, #50306, #30271, #59384, #7370 ),
 .UNSPECIFIED., .F., .F.,
 ( 4, 2, 4 ),
 ( 1.275615807185303638E-16, 0.0002450741128632367874, 0.0004901482257263460726 ),
 .UNSPECIFIED. ) ;
#50948 = VECTOR ( 'NONE', #54212, 999.9999999999998863 ) ;
#50949 = EDGE_CURVE ( 'NONE', #16942, #7371, #31353, .T. ) ;
#50950 = ORIENTED_EDGE ( 'NONE', *, *, #23382, .T. ) ;
#50951 = CARTESIAN_POINT ( 'NONE',  ( 4.000000000000004441, 0.7862748000878159171, -0.03447227762756879116 ) ) ;
#50952 = ORIENTED_EDGE ( 'NONE', *, *, #23429, .T. ) ;
#50953 = CARTESIAN_POINT ( 'NONE',  ( 6.999999999999995559, 56.56854249492450037, -56.56854249492312192 ) ) ;
#50954 = CARTESIAN_POINT ( 'NONE',  ( 0.1073791018717483448, 16.05399293000815675, -40.02496097243042072 ) ) ;
#50955 = VECTOR ( 'NONE', #28822, 999.9999999999998863 ) ;
#50956 = CARTESIAN_POINT ( 'NONE',  ( 0.1157506346131639274, -43.74993170343814342, 5.734469090276133940 ) ) ;
#50957 = ORIENTED_EDGE ( 'NONE', *, *, #60515, .T. ) ;
#50958 = CARTESIAN_POINT ( 'NONE',  ( 0.1158403557922069033, 43.30320583737607620, 8.471875317169066832 ) ) ;
#50959 = CARTESIAN_POINT ( 'NONE',  ( 1.157643937452369265, -0.5751542567737857325, 41.91266481835375401 ) ) ;
#50960 = CARTESIAN_POINT ( 'NONE',  ( 5.901764892641307547, 1.526405342807678478, 48.94549574954908167 ) ) ;
#50961 = B_SPLINE_CURVE_WITH_KNOTS ( 'NONE', 3,
 ( #5376, #10731, #48934, #48018, #39251, #688 ),
 .UNSPECIFIED., .F., .F.,
 ( 4, 2, 4 ),
 ( 8.148123767742043513E-18, 0.0002291978881530126635, 0.0004583957763060171413 ),
 .UNSPECIFIED. ) ;
#50962 = EDGE_LOOP ( 'NONE', ( #4243, #61183 ) ) ;
#50963 = CARTESIAN_POINT ( 'NONE',  ( 4.694002226626920127, 45.25670317367036688, 5.487767241458856304 ) ) ;
#50964 = CARTESIAN_POINT ( 'NONE',  ( 4.956445790443996913, 7.299064093730984304, 46.52162629890795387 ) ) ;
#50965 = CARTESIAN_POINT ( 'NONE',  ( 0.1095718737110178143, 26.45591486700756434, -34.05592812063355268 ) ) ;
#50966 = CARTESIAN_POINT ( 'NONE',  ( 0.2940133293162998096, 33.06489090063801939, 29.20536833027361112 ) ) ;
#50967 = ORIENTED_EDGE ( 'NONE', *, *, #31885, .T. ) ;
#50968 = CARTESIAN_POINT ( 'NONE',  ( 0.1087620492084206553, 37.52665900408519661, -21.24797679669920925 ) ) ;
#50969 = FACE_OUTER_BOUND ( 'NONE', #7388, .T. ) ;
#50970 = AXIS2_PLACEMENT_3D ( 'NONE', #47398, #56166, #46803 ) ;
#50971 = ORIENTED_EDGE ( 'NONE', *, *, #22030, .F. ) ;
#50972 = CARTESIAN_POINT ( 'NONE',  ( 0.9772918015221170318, -26.73923612106478132, 32.26995673087623118 ) ) ;
#50973 = CARTESIAN_POINT ( 'NONE',  ( 0.5807400328401637335, 44.04145271122565219, 18.83234461715199970 ) ) ;
#50974 = CARTESIAN_POINT ( 'NONE',  ( 0.9756354156337442296, 5.729847988735970787, -42.52418499698892873 ) ) ;
#50975 = CARTESIAN_POINT ( 'NONE',  ( 0.8551540677456834771, 28.44084013485174012, -38.56334384152401640 ) ) ;
#50976 = CARTESIAN_POINT ( 'NONE',  ( -2.739355103387248747, -14.37091041638174005, 4.040358988425137632 ) ) ;
#50977 =( NAMED_UNIT ( * ) SI_UNIT ( $, .STERADIAN. ) SOLID_ANGLE_UNIT ( ) );
#50979 = ADVANCED_FACE ( 'NONE', ( #48189 ), #37730, .F. ) ;
#50978 = CARTESIAN_POINT ( 'NONE',  ( 5.965394784446460541, 5.326334832595648550, -19.82223131420049000 ) ) ;
#50980 = CARTESIAN_POINT ( 'NONE',  ( 0.9754402186311939005, -39.57010335554342362, 16.59348191374125392 ) ) ;
#50981 = CARTESIAN_POINT ( 'NONE',  ( 0.1129192098497447394, -38.68182264534125636, -21.22895156665819627 ) ) ;
#50982 = ADVANCED_FACE ( 'NONE', ( #21521 ), #54504, .F. ) ;
#50983 = CARTESIAN_POINT ( 'NONE',  ( 3.678834586032788678, -36.44297663525289721, 32.71882980167178800 ) ) ;
#50984 = CARTESIAN_POINT ( 'NONE',  ( 2.648799415243696664, 46.08255460350029153, 16.76053771527072911 ) ) ;
#50985 = B_SPLINE_CURVE_WITH_KNOTS ( 'NONE', 3,
 ( #24530, #53028, #10441, #57710, #4780, #14840 ),
 .UNSPECIFIED., .F., .F.,
 ( 4, 2, 4 ),
 ( 8.673617379884034509E-19, 0.0002291459268755701264, 0.0004582918537511393854 ),
 .UNSPECIFIED. ) ;
#50986 = CARTESIAN_POINT ( 'NONE',  ( 0.7245667037590732829, -46.66865388241075863, -11.65533952568336318 ) ) ;
#50987 = CARTESIAN_POINT ( 'NONE',  ( 4.553261556744875094, 31.39705178283641018, 30.72075365562384519 ) ) ;
#50988 = ADVANCED_FACE ( 'NONE', ( #11513 ), #13755, .F. ) ;
#50989 = CARTESIAN_POINT ( 'NONE',  ( 0.5832366564991497970, -24.18352361336798140, -41.34220239954010623 ) ) ;
#50990 = CARTESIAN_POINT ( 'NONE',  ( 3.783198216974388739, 29.18723368117363393, 31.62918462580848455 ) ) ;
#50991 = DIRECTION ( 'NONE',  ( 1.000000000000000000, -0.000000000000000000, -0.000000000000000000 ) ) ;
#50992 = CARTESIAN_POINT ( 'NONE',  ( 2.879087469061463622, 32.35613322949701143, -29.81916027017557269 ) ) ;
#50993 = ORIENTED_EDGE ( 'NONE', *, *, #21299, .T. ) ;
#50994 = CARTESIAN_POINT ( 'NONE',  ( 5.960721111146673579, 18.96073515164537326, 7.860635756377957861 ) ) ;
#50995 = ADVANCED_FACE ( 'NONE', ( #54703 ), #32966, .F. ) ;
#50996 = AXIS2_PLACEMENT_3D ( 'NONE', #8334, #56258, #22453 ) ;
#50997 = FACE_OUTER_BOUND ( 'NONE', #22980, .T. ) ;
#50998 = CARTESIAN_POINT ( 'NONE',  ( -2.708315649062916552, -9.116606751444257029, -11.44805714186568579 ) ) ;
#50999 = B_SPLINE_CURVE_WITH_KNOTS ( 'NONE', 3,
 ( #3665, #27488, #42540, #61603 ),
 .UNSPECIFIED., .F., .F.,
 ( 4, 4 ),
 ( 1.734723475976807094E-18, 0.005013413432710139839 ),
 .UNSPECIFIED. ) ;
#51000 = CARTESIAN_POINT ( 'NONE',  ( 0.6029442701453591180, -45.55116825581043116, -18.34765095834136162 ) ) ;
#51001 = ORIENTED_EDGE ( 'NONE', *, *, #31047, .F. ) ;
#51002 = EDGE_CURVE ( 'NONE', #26826, #57221, #53727, .T. ) ;
#51003 = CARTESIAN_POINT ( 'NONE',  ( 0.7044674535453004927, -35.85885898216606904, -33.55510326773016772 ) ) ;
#51004 = DIRECTION ( 'NONE',  ( 0.000000000000000000, 1.000000000000000000, -1.224646799147353207E-16 ) ) ;
#51005 = ORIENTED_EDGE ( 'NONE', *, *, #57592, .F. ) ;
#51006 = CARTESIAN_POINT ( 'NONE',  ( 0.8753041380234530822, 17.79089796329305884, 45.76704357430872960 ) ) ;
#51007 = ORIENTED_EDGE ( 'NONE', *, *, #1817, .T. ) ;
#51008 = B_SPLINE_CURVE_WITH_KNOTS ( 'NONE', 3,
 ( #46208, #22380, #17687, #24226, #57105, #19241 ),
 .UNSPECIFIED., .F., .F.,
 ( 4, 2, 4 ),
 ( 9.341771812940338307E-18, 0.0002291472222819920140, 0.0004582944445639746496 ),
 .UNSPECIFIED. ) ;
#51009 = CARTESIAN_POINT ( 'NONE',  ( -6.016104459813374383, -11.46679299034570398, -14.95258000663143960 ) ) ;
#51010 = AXIS2_PLACEMENT_3D ( 'NONE', #33513, #61062, #27259 ) ;
#51011 = DIRECTION ( 'NONE',  ( 0.000000000000000000, 0.000000000000000000, 1.000000000000000000 ) ) ;
#51012 = VERTEX_POINT ( 'NONE', #25916 ) ;
#51013 = CARTESIAN_POINT ( 'NONE',  ( 4.834790513006553603, -10.06429236341580236, -46.16599787882930883 ) ) ;
#51014 = CARTESIAN_POINT ( 'NONE',  ( 0.5834872094924173913, -29.33699246747726264, 37.85980081020210264 ) ) ;
#51015 = ORIENTED_EDGE ( 'NONE', *, *, #40419, .T. ) ;
#51016 = CARTESIAN_POINT ( 'NONE',  ( 4.691466044806104740, -42.11359095667501151, 14.64802401911153851 ) ) ;
#51017 = CARTESIAN_POINT ( 'NONE',  ( 0.1073791018717578927, -16.05399293000789385, -40.02496097243051310 ) ) ;
#51018 = MANIFOLD_SOLID_BREP ( 'Cut-Extrude-Thin4', #43082 ) ;
#51019 = ORIENTED_EDGE ( 'NONE', *, *, #60442, .T. ) ;
#51020 = CARTESIAN_POINT ( 'NONE',  ( 4.322998006666165516, -25.80712523194303287, 40.45864630878473633 ) ) ;
#51021 = EDGE_LOOP ( 'NONE', ( #27760, #28514, #7064, #13061 ) ) ;
#51022 = EDGE_CURVE ( 'NONE', #32724, #15442, #26525, .T. ) ;
#51023 = EDGE_LOOP ( 'NONE', ( #54241, #13421, #45997, #59674 ) ) ;
#51024 = EDGE_LOOP ( 'NONE', ( #24145, #21753, #19383, #30121 ) ) ;
#51025 = CARTESIAN_POINT ( 'NONE',  ( 0.9752132459055860014, -0.2329632697540915398, -42.90780255730425097 ) ) ;
#51026 = DIRECTION ( 'NONE',  ( -1.000000000000000000, -0.000000000000000000, -0.000000000000000000 ) ) ;
#51027 = DIRECTION ( 'NONE',  ( 0.000000000000000000, -1.000000000000000000, 0.000000000000000000 ) ) ;
#51028 = DIRECTION ( 'NONE',  ( 0.1011922191286467876, -0.8730847945189473824, -0.4769518595913295189 ) ) ;
#51029 = LINE ( 'NONE', #22543, #53667 ) ;
#51030 = VERTEX_POINT ( 'NONE', #60634 ) ;
#51031 = CARTESIAN_POINT ( 'NONE',  ( 4.060580049360325461, 6.517192272988030943, 43.46255744012442079 ) ) ;
#51032 = CARTESIAN_POINT ( 'NONE',  ( 5.895596859100789899, 20.06773179721815126, -1.346968346846738385 ) ) ;
#51033 = ORIENTED_EDGE ( 'NONE', *, *, #6390, .T. ) ;
#51034 = VERTEX_POINT ( 'NONE', #3931 ) ;
#51035 = CARTESIAN_POINT ( 'NONE',  ( 0.9756950546413938330, 33.98259063592758622, -26.19769393035335625 ) ) ;
#51036 = CARTESIAN_POINT ( 'NONE',  ( 3.782542959838396168, 27.96057807588762145, 31.39178120239056469 ) ) ;
#51037 = LINE ( 'NONE', #3415, #60941 ) ;
#51038 = ORIENTED_EDGE ( 'NONE', *, *, #12148, .F. ) ;
#51039 = CARTESIAN_POINT ( 'NONE',  ( 4.975610109902397937, 19.27143522741721426, -44.95621415792522413 ) ) ;
#51040 = DIRECTION ( 'NONE',  ( -0.1024043820194934507, 0.7971196296869377251, -0.5950744814819106665 ) ) ;
#51041 = VERTEX_POINT ( 'NONE', #3620 ) ;
#51042 = CARTESIAN_POINT ( 'NONE',  ( 4.553261556744875094, 35.33793455049291765, -26.09156851415253087 ) ) ;
#51043 = CARTESIAN_POINT ( 'NONE',  ( -25.39999999999999858, 0.000000000000000000, 0.000000000000000000 ) ) ;
#51044 = CARTESIAN_POINT ( 'NONE',  ( 2.281448460670565392, -32.98023336626259550, 34.83871297539693046 ) ) ;
#51045 = CARTESIAN_POINT ( 'NONE',  ( 0.9762797500689124330, 9.222352665238926051, -40.88120590813907285 ) ) ;
#51046 = CARTESIAN_POINT ( 'NONE',  ( 2.009741617377216460, -43.48179227669744051, 6.988405971978110642 ) ) ;
#51047 =( NAMED_UNIT ( * ) PLANE_ANGLE_UNIT ( ) SI_UNIT ( $, .RADIAN. ) );
#51048 = CIRCLE ( 'NONE', #27053, 43.08621763946400307 ) ;
#51049 = ORIENTED_EDGE ( 'NONE', *, *, #21358, .T. ) ;
#51050 = CARTESIAN_POINT ( 'NONE',  ( 0.1073791018717578927, 34.50606437925546999, -25.86618856530675714 ) ) ;
#51051 = DIRECTION ( 'NONE',  ( -1.000000000000000000, -0.000000000000000000, -0.000000000000000000 ) ) ;
#51052 = EDGE_CURVE ( 'NONE', #61727, #34766, #57501, .T. ) ;
#51053 = CARTESIAN_POINT ( 'NONE',  ( 2.526552050251864134, 36.59987178591183010, 22.53110080776668767 ) ) ;
#51054 = VECTOR ( 'NONE', #54900, 1000.000000000000000 ) ;
#51055 = CARTESIAN_POINT ( 'NONE',  ( 0.1103744047535531458, -16.46720136312954708, -39.85659247569254404 ) ) ;
#51056 = B_SPLINE_CURVE_WITH_KNOTS ( 'NONE', 3,
 ( #39495, #6224, #5919, #44203 ),
 .UNSPECIFIED., .F., .F.,
 ( 4, 4 ),
 ( 7.046480070129584215E-18, 0.005013413432710146778 ),
 .UNSPECIFIED. ) ;
#51057 = CARTESIAN_POINT ( 'NONE',  ( 4.303969348037258058, 20.38638383586119929, 43.57722561725964994 ) ) ;
#51058 = EDGE_CURVE ( 'NONE', #28220, #5855, #4467, .T. ) ;
#51059 = CARTESIAN_POINT ( 'NONE',  ( 3.678748215320119641, 34.27176725038954430, 34.98655147102398644 ) ) ;
#51060 = CARTESIAN_POINT ( 'NONE',  ( 4.956653778116475451, 47.27023054223744225, 8.845409907520236814 ) ) ;
#51061 = CARTESIAN_POINT ( 'NONE',  ( 5.960221823109900008, 5.317678907195437787, -19.82478916873570185 ) ) ;
#51062 = EDGE_CURVE ( 'NONE', #9975, #53201, #7472, .T. ) ;
#51063 = LINE ( 'NONE', #27272, #52246 ) ;
#51064 = FACE_OUTER_BOUND ( 'NONE', #38033, .T. ) ;
#51065 = ORIENTED_EDGE ( 'NONE', *, *, #54654, .F. ) ;
#51066 = CARTESIAN_POINT ( 'NONE',  ( 0.8557997880470606944, -24.73961900479280374, 41.02602466100771039 ) ) ;
#51067 = CARTESIAN_POINT ( 'NONE',  ( 2.706805983486680223, 23.80251637563394596, -37.01643320887944100 ) ) ;
#51068 = CARTESIAN_POINT ( 'NONE',  ( 2.648799415243708655, 9.556201303927180035, -48.09570126246647703 ) ) ;
#51069 = CARTESIAN_POINT ( 'NONE',  ( 0.8760168074887076939, -41.20610493656926820, 24.81951362746006495 ) ) ;
#51070 = VERTEX_POINT ( 'NONE', #38120 ) ;
#51071 = EDGE_CURVE ( 'NONE', #11856, #27102, #26129, .T. ) ;
#51072 = CARTESIAN_POINT ( 'NONE',  ( 4.975610109902397937, -28.45381238669758872, -39.78479568629688856 ) ) ;
#51073 = CARTESIAN_POINT ( 'NONE',  ( 0.6008122571543327295, 44.05373654283606299, -21.69845264252053951 ) ) ;
#51074 =( NAMED_UNIT ( * ) PLANE_ANGLE_UNIT ( ) SI_UNIT ( $, .RADIAN. ) );
#51075 = ORIENTED_EDGE ( 'NONE', *, *, #18019, .F. ) ;
#51076 = CARTESIAN_POINT ( 'NONE',  ( 0.6039202388192952409, -49.10736577297868166, -0.1741829149863120263 ) ) ;
#51077 = CARTESIAN_POINT ( 'NONE',  ( 5.917102823773431552, -18.51268610137626425, 7.859400191086610477 ) ) ;
#51078 = CARTESIAN_POINT ( 'NONE',  ( 0.6254087463353941168, 24.64672211239907185, 41.31312313681416271 ) ) ;
#51079 = VERTEX_POINT ( 'NONE', #42501 ) ;
#51080 = CARTESIAN_POINT ( 'NONE',  ( 0.6031356755773454870, 29.28597628606495462, 38.16618524502131748 ) ) ;
#51081 = ORIENTED_EDGE ( 'NONE', *, *, #41318, .F. ) ;
#51082 = ORIENTED_EDGE ( 'NONE', *, *, #29845, .F. ) ;
#51083 = CARTESIAN_POINT ( 'NONE',  ( 0.9756950546413946102, -5.504753251348003751, 42.55388731055339235 ) ) ;
#51084 = VERTEX_POINT ( 'NONE', #13997 ) ;
#51085 = DIRECTION ( 'NONE',  ( 1.000000000000000000, 0.000000000000000000, 0.000000000000000000 ) ) ;
#51086 = ORIENTED_EDGE ( 'NONE', *, *, #28172, .T. ) ;
#51087 = CARTESIAN_POINT ( 'NONE',  ( 4.956445790443987143, 47.01859095792193699, -2.605792484304513934 ) ) ;
#51088 = AXIS2_PLACEMENT_3D ( 'NONE', #12800, #21563, #46016 ) ;
#51089 = CARTESIAN_POINT ( 'NONE',  ( 4.962356264823593932, 7.429277797797228189, 41.42513040734459651 ) ) ;
#51090 = ORIENTED_EDGE ( 'NONE', *, *, #61415, .F. ) ;
#51091 = CARTESIAN_POINT ( 'NONE',  ( 0.1145239942831223490, 43.37176113481423556, -8.113927333251773177 ) ) ;
#51092 = CARTESIAN_POINT ( 'NONE',  ( 1.830465331921977246, -30.77164106904660912, -31.51955205576617658 ) ) ;
#51093 = CARTESIAN_POINT ( 'NONE',  ( 4.060580049360325461, -37.10466027576811854, 23.55232218230391084 ) ) ;
#51094 = CARTESIAN_POINT ( 'NONE',  ( -1.114299999999999846, 0.000000000000000000, 0.000000000000000000 ) ) ;
#51095 = ORIENTED_EDGE ( 'NONE', *, *, #30468, .F. ) ;
#51096 = EDGE_CURVE ( 'NONE', #55183, #5605, #44154, .T. ) ;
#51097 = FACE_OUTER_BOUND ( 'NONE', #50572, .T. ) ;
#51098 = EDGE_LOOP ( 'NONE', ( #32903, #5928, #1030, #56623 ) ) ;
#51099 = CARTESIAN_POINT ( 'NONE',  ( 2.526464513654346433, 22.53107770806421684, 36.59988118252409350 ) ) ;
#51100 = EDGE_CURVE ( 'NONE', #9101, #22050, #41393, .T. ) ;
#51101 = ORIENTED_EDGE ( 'NONE', *, *, #22156, .F. ) ;
#51102 = CARTESIAN_POINT ( 'NONE',  ( 0.1152339509894530906, -12.34020981180770526, 42.36345019301198533 ) ) ;
#51103 = B_SPLINE_CURVE_WITH_KNOTS ( 'NONE', 3,
 ( #45635, #54999, #12128, #25896 ),
 .UNSPECIFIED., .F., .F.,
 ( 4, 4 ),
 ( 4.336808689942017736E-19, 0.004444878191956859459 ),
 .UNSPECIFIED. ) ;
#51104 = CARTESIAN_POINT ( 'NONE',  ( 0.1073791018717483448, 11.62916352156094035, 41.52698815987171344 ) ) ;
#51105 = ORIENTED_EDGE ( 'NONE', *, *, #28188, .F. ) ;
#51106 = CARTESIAN_POINT ( 'NONE',  ( 0.5839879882012690704, -46.26395995854825571, -12.39635945869009781 ) ) ;
#51107 = CARTESIAN_POINT ( 'NONE',  ( 4.960386119450144626, -43.29863790797085699, 6.297969513007277698 ) ) ;
#51108 = ADVANCED_FACE ( 'NONE', ( #56868 ), #61865, .F. ) ;
#51109 = LINE ( 'NONE', #26698, #25657 ) ;
#51110 = CARTESIAN_POINT ( 'NONE',  ( 4.975610109902397937, 30.04451009524474969, 38.59762713269442713 ) ) ;
#51111 = ORIENTED_EDGE ( 'NONE', *, *, #54004, .T. ) ;
#51112 = ORIENTED_EDGE ( 'NONE', *, *, #13583, .F. ) ;
#51113 = CARTESIAN_POINT ( 'NONE',  ( 0.8560838555295158248, 44.99141268455571208, 13.27198623905747432 ) ) ;
#51114 = FACE_OUTER_BOUND ( 'NONE', #25492, .T. ) ;
#51115 = DIRECTION ( 'NONE',  ( 0.000000000000000000, 0.000000000000000000, -1.000000000000000000 ) ) ;
#51116 = CARTESIAN_POINT ( 'NONE',  ( 0.5980271706414734822, 46.38528005876716520, -16.13861941776310260 ) ) ;
#51117 =( BOUNDED_SURFACE ( )  B_SPLINE_SURFACE ( 3, 1, ( 
 ( #51, #52366 ),
 ( #9462, #4734 ),
 ( #23882, #38932 ),
 ( #38311, #57063 ) ),
 .UNSPECIFIED., .F., .F., .F. ) 
 B_SPLINE_SURFACE_WITH_KNOTS ( ( 4, 4 ),
 ( 2, 2 ),
 ( 0.000000000000000000, 1.000000000000000000 ),
 ( 0.000000000000000000, 1.000000000000000000 ),
 .UNSPECIFIED. ) 
 GEOMETRIC_REPRESENTATION_ITEM ( )  RATIONAL_B_SPLINE_SURFACE ( (
 ( 1.000000000000000000, 1.000000000000000000),
 ( 0.7223157951917480446, 0.9931996967497186413),
 ( 0.7223157951917480446, 0.9931996967497186413),
 ( 1.000000000000000000, 1.000000000000000000) ) ) 
 REPRESENTATION_ITEM ( '' )  SURFACE ( )  );
#51118 = CARTESIAN_POINT ( 'NONE',  ( -6.077587904424778920, 5.472951620448459842, 18.46192898789725945 ) ) ;
#51119 = CARTESIAN_POINT ( 'NONE',  ( -5.272380000000000067, 1.534410185170483674E-15, -12.49999999999999822 ) ) ;
#51120 = B_SPLINE_CURVE_WITH_KNOTS ( 'NONE', 3,
 ( #43117, #19300, #58398, #19612, #44062, #33714 ),
 .UNSPECIFIED., .F., .F.,
 ( 4, 2, 4 ),
 ( 3.252606517456513302E-18, 0.0002447193893791695454, 0.0004894387787583358383 ),
 .UNSPECIFIED. ) ;
#51121 = CARTESIAN_POINT ( 'NONE',  ( 0.5838002273316424962, -46.29900743592988022, 12.26477999444052180 ) ) ;
#51122 = EDGE_CURVE ( 'NONE', #60647, #35431, #43353, .T. ) ;
#51123 = CARTESIAN_POINT ( 'NONE',  ( 0.8760168074886960365, -5.394043284319175235, -47.80016357497247981 ) ) ;
#51124 = B_SPLINE_CURVE_WITH_KNOTS ( 'NONE', 3,
 ( #57476, #10834, #25531, #58409, #29928, #48722 ),
 .UNSPECIFIED., .F., .F.,
 ( 4, 2, 4 ),
 ( 1.870429930157025393E-17, 0.0002293755540694321859, 0.0004587511081388456692 ),
 .UNSPECIFIED. ) ;
#51125 = CARTESIAN_POINT ( 'NONE',  ( -2.739355103387247858, -2.122549901523845151, -14.77641190771826274 ) ) ;
#51126 = EDGE_CURVE ( 'NONE', #2175, #45275, #32140, .T. ) ;
#51127 = CARTESIAN_POINT ( 'NONE',  ( 0.9762797500689124330, 32.57381952463229169, 26.36799322592426975 ) ) ;
#51128 = CARTESIAN_POINT ( 'NONE',  ( 3.782542959838397056, -36.71077845802598461, -20.48308078396187426 ) ) ;
#51129 = CARTESIAN_POINT ( 'NONE',  ( 0.8557997880470599172, -0.9121262075949487791, 47.89938907511593413 ) ) ;
#51130 = CARTESIAN_POINT ( 'NONE',  ( 4.962356264823596597, 37.75702904547799932, 18.59145920903680249 ) ) ;
#51131 = CARTESIAN_POINT ( 'NONE',  ( 1.227938101723756947, 4.762198645645047357, -42.65467462194912684 ) ) ;
#51132 = CARTESIAN_POINT ( 'NONE',  ( 1.830465331921978134, -16.69450186282941928, -40.76358256373419664 ) ) ;
#51133 = EDGE_CURVE ( 'NONE', #9776, #4961, #18715, .T. ) ;
#51134 =( BOUNDED_SURFACE ( )  B_SPLINE_SURFACE ( 3, 1, ( 
 ( #28525, #28223 ),
 ( #37973, #5014 ),
 ( #57946, #631 ),
 ( #14454, #10054 ) ),
 .UNSPECIFIED., .F., .F., .F. ) 
 B_SPLINE_SURFACE_WITH_KNOTS ( ( 4, 4 ),
 ( 2, 2 ),
 ( 0.000000000000000000, 1.000000000000000000 ),
 ( 0.000000000000000000, 1.000000000000000000 ),
 .UNSPECIFIED. ) 
 GEOMETRIC_REPRESENTATION_ITEM ( )  RATIONAL_B_SPLINE_SURFACE ( (
 ( 1.000000000000000000, 1.000000000000000000),
 ( 0.9953390228620291325, 0.8624445117760984880),
 ( 0.9953390228620291325, 0.8624445117760984880),
 ( 1.000000000000000000, 1.000000000000000000) ) ) 
 REPRESENTATION_ITEM ( '' )  SURFACE ( )  );
#51135 = AXIS2_PLACEMENT_3D ( 'NONE', #33134, #52518, #9301 ) ;
#51136 = CARTESIAN_POINT ( 'NONE',  ( 5.959547316686252039, 10.26589671991363417, -17.77392908783923531 ) ) ;
#51137 = CARTESIAN_POINT ( 'NONE',  ( 0.7056759521544971880, -13.08829070999385102, -45.03826678956104246 ) ) ;
#51138 = DIRECTION ( 'NONE',  ( 1.000000000000000000, 0.000000000000000000, 0.000000000000000000 ) ) ;
#51140 = ORIENTED_EDGE ( 'NONE', *, *, #52630, .F. ) ;
#51139 = CARTESIAN_POINT ( 'NONE',  ( 2.301430502907646503, 25.12309903330020688, -40.93949994354160538 ) ) ;
#51141 = EDGE_LOOP ( 'NONE', ( #24705, #25046, #49187, #40136 ) ) ;
#51142 = CARTESIAN_POINT ( 'NONE',  ( 0.6024113833632039894, -39.48520517600478286, 29.19692520300162641 ) ) ;
#51143 = CARTESIAN_POINT ( 'NONE',  ( 1.479689385636123067, 3.059513055334726950, -43.95706115212809095 ) ) ;
#51144 = FACE_OUTER_BOUND ( 'NONE', #15317, .T. ) ;
#51145 = ORIENTED_EDGE ( 'NONE', *, *, #31486, .T. ) ;
#51146 = EDGE_CURVE ( 'NONE', #55001, #9995, #55296, .T. ) ;
#51147 = ORIENTED_EDGE ( 'NONE', *, *, #22354, .F. ) ;
#51148 = CARTESIAN_POINT ( 'NONE',  ( 4.999999999999986677, 56.56854249492371878, 56.56854249492391062 ) ) ;
#51150 = DIRECTION ( 'NONE',  ( 0.07500201931887537365, 0.9374924185315435254, 0.3398274007403879748 ) ) ;
#51149 = B_SPLINE_CURVE_WITH_KNOTS ( 'NONE', 3,
 ( #3001, #32773, #51230, #8311, #60312, #50924, #42188, #27432, #46562, #17127, #12745, #56550, #36240, #22742, #51851, #8950, #17425, #41875, #36549 ),
 .UNSPECIFIED., .F., .F.,
 ( 4, 3, 3, 3, 3, 3, 4 ),
 ( 0.000000000000000000, 0.0002732106629380697503, 0.0004098138914053829672, 0.0005464171197651475570, 0.0006830203481512520797, 0.0008196235766963617898, 0.001011968216111154388 ),
 .UNSPECIFIED. ) ;
#51151 = UNCERTAINTY_MEASURE_WITH_UNIT (LENGTH_MEASURE( 1.000000000000000082E-05 ), #53813, 'distance_accuracy_value', 'NONE');
#51152 = ORIENTED_EDGE ( 'NONE', *, *, #41906, .T. ) ;
#51153 = APPLICATION_CONTEXT ( 'automotive_design' ) ;
#51154 = ORIENTED_EDGE ( 'NONE', *, *, #10301, .T. ) ;
#51155 = CARTESIAN_POINT ( 'NONE',  ( 4.834790513006555379, -27.40943972694820019, -38.48781566650898611 ) ) ;
#51156 = CARTESIAN_POINT ( 'NONE',  ( 4.962356264823608143, 0.000000000000000000, 0.000000000000000000 ) ) ;
#51157 = CARTESIAN_POINT ( 'NONE',  ( 4.975610109902397937, 0.000000000000000000, 0.000000000000000000 ) ) ;
#51158 = ORIENTED_EDGE ( 'NONE', *, *, #18827, .F. ) ;
#51159 = CARTESIAN_POINT ( 'NONE',  ( 0.8751705887134553219, 24.81530984069150136, 41.19904111682516401 ) ) ;
#51160 = B_SPLINE_CURVE_WITH_KNOTS ( 'NONE', 3,
 ( #52583, #9059, #38518, #48213, #34126, #4960 ),
 .UNSPECIFIED., .F., .F.,
 ( 4, 2, 4 ),
 ( 9.543442895606953578E-18, 0.0002291978881530158890, 0.0004583957763060222371 ),
 .UNSPECIFIED. ) ;
#51161 = CARTESIAN_POINT ( 'NONE',  ( 0.8744876279028263033, -48.79802643035343834, 5.394688766001209501 ) ) ;
#51162 = PLANE ( 'NONE',  #14987 ) ;
#51163 = ORIENTED_EDGE ( 'NONE', *, *, #48494, .F. ) ;
#51164 = EDGE_LOOP ( 'NONE', ( #42095, #3183, #1063, #45805 ) ) ;
#51165 = EDGE_CURVE ( 'NONE', #4984, #22082, #6680, .T. ) ;
#51166 = CARTESIAN_POINT ( 'NONE',  ( 0.5997462898726536595, 44.46857747280041195, -20.83500054451300088 ) ) ;
#51167 = B_SPLINE_CURVE_WITH_KNOTS ( 'NONE', 3,
 ( #15065, #15991, #52945, #30069, #49179, #53857 ),
 .UNSPECIFIED., .F., .F.,
 ( 4, 2, 4 ),
 ( 8.551243849294126806E-17, 0.0002293366620881437108, 0.0004586733241762018781 ),
 .UNSPECIFIED. ) ;
#51168 = ORIENTED_EDGE ( 'NONE', *, *, #40273, .F. ) ;
#51169 = CARTESIAN_POINT ( 'NONE',  ( 1.088908134280559104, 20.77739698351986064, -37.54826033999239598 ) ) ;
#51170 = CARTESIAN_POINT ( 'NONE',  ( 2.281448460670567169, 30.23587867650755001, 37.24544744441590183 ) ) ;
#51171 = CARTESIAN_POINT ( 'NONE',  ( 4.553261556744875094, 0.000000000000000000, 0.000000000000000000 ) ) ;
#51172 = CARTESIAN_POINT ( 'NONE',  ( 3.238931869106854489, 29.07925862215132184, -31.66562935062907513 ) ) ;
#51173 = ADVANCED_FACE ( 'NONE', ( #61257 ), #57345, .F. ) ;
#51174 = EDGE_LOOP ( 'NONE', ( #4997, #35536, #215, #50459 ) ) ;
#51175 = CARTESIAN_POINT ( 'NONE',  ( 0.8760168074886960365, 13.30888447662080409, -46.22580377597773094 ) ) ;
#51176 = VECTOR ( 'NONE', #40998, 1000.000000000000000 ) ;
#51177 = FACE_OUTER_BOUND ( 'NONE', #21982, .T. ) ;
#51178 = EDGE_CURVE ( 'NONE', #61214, #25486, #25398, .T. ) ;
#51179 = CONICAL_SURFACE ( 'NONE', #14189, 43.08621763946400307, 1.568696531533066763 ) ;
#51180 = CARTESIAN_POINT ( 'NONE',  ( 5.895881250540457863, -18.51869114342256495, -7.847659520062246763 ) ) ;
#51181 = ORIENTED_EDGE ( 'NONE', *, *, #41318, .T. ) ;
#51182 = CARTESIAN_POINT ( 'NONE',  ( 0.1119899015040013296, 15.76451783742778900, -41.21214973215941058 ) ) ;
#51183 = CARTESIAN_POINT ( 'NONE',  ( 5.440000000000003055, -15.14599999999998658, 1.854850041988580043E-15 ) ) ;
#51184 = EDGE_CURVE ( 'NONE', #56408, #19218, #29124, .T. ) ;
#51185 = FACE_OUTER_BOUND ( 'NONE', #18858, .T. ) ;
#51186 = CARTESIAN_POINT ( 'NONE',  ( 0.6254311100348654007, 6.960804577576820584, -47.60023274471273425 ) ) ;
#51187 = ADVANCED_FACE ( 'NONE', ( #58707 ), #28540, .F. ) ;
#51188 = EDGE_LOOP ( 'NONE', ( #12218, #8643, #18909, #11852 ) ) ;
#51189 = FACE_OUTER_BOUND ( 'NONE', #44106, .T. ) ;
#51190 = CARTESIAN_POINT ( 'NONE',  ( -6.016761891674564211, 18.84319130225482297, -0.003433883959849463787 ) ) ;
#51191 = CARTESIAN_POINT ( 'NONE',  ( 1.157643937452369265, 40.63757547730140374, 10.27568654258122827 ) ) ;
#51192 = B_SPLINE_CURVE_WITH_KNOTS ( 'NONE', 3,
 ( #15766, #5702, #35187, #58961 ),
 .UNSPECIFIED., .F., .F.,
 ( 4, 4 ),
 ( 0.000000000000000000, 0.004442905043737213969 ),
 .UNSPECIFIED. ) ;
#51193 = CARTESIAN_POINT ( 'NONE',  ( 0.5804410086790514622, 32.99440095573996246, 33.33000686209445718 ) ) ;
#51194 = CARTESIAN_POINT ( 'NONE',  ( 5.959828726073459926, -5.316791119501226071, 19.82504517499703667 ) ) ;
#51195 = CARTESIAN_POINT ( 'NONE',  ( 0.7056555295713294873, -7.085402321211474508, -47.37451042924661948 ) ) ;
#51196 = CARTESIAN_POINT ( 'NONE',  ( 0.7954196712028458460, -46.22745629466061956, -13.28627209367561335 ) ) ;
#51197 = EDGE_CURVE ( 'NONE', #12367, #37726, #23393, .T. ) ;
#51198 = CARTESIAN_POINT ( 'NONE',  ( 4.975610109902397937, 13.36434394399761949, -47.05150069959838532 ) ) ;
#51199 = DIRECTION ( 'NONE',  ( 0.000000000000000000, 0.000000000000000000, 1.000000000000000000 ) ) ;
#51200 = EDGE_LOOP ( 'NONE', ( #36400, #19943 ) ) ;
#51201 = CARTESIAN_POINT ( 'NONE',  ( 0.5800708119828338338, 11.78915056783772819, -46.42229822050683907 ) ) ;
#51202 = CARTESIAN_POINT ( 'NONE',  ( -6.010958268070873523, -18.68034667844847618, -2.473955915502408676 ) ) ;
#51203 = CARTESIAN_POINT ( 'NONE',  ( 0.1157506346131639274, -35.41710508906525234, -26.31671193202034686 ) ) ;
#51204 = CARTESIAN_POINT ( 'NONE',  ( 3.680974057930774812, -4.423547572561986385, -47.77138393978994912 ) ) ;
#51205 = CARTESIAN_POINT ( 'NONE',  ( 3.727782113643637540, -24.59154922726513703, -36.44219371153403131 ) ) ;
#51206 = CARTESIAN_POINT ( 'NONE',  ( 0.1092565886968785704, 42.79503959566645932, 5.321013289171810712 ) ) ;
#51207 = APPLICATION_PROTOCOL_DEFINITION ( 'draft international standard', 'automotive_design', 1998, #9535 ) ;
#51208 = CARTESIAN_POINT ( 'NONE',  ( 0.2885697896453102707, 36.93108635218666791, 22.25146201964156845 ) ) ;
#51209 = EDGE_CURVE ( 'NONE', #52291, #51706, #2932, .T. ) ;
#51210 = LINE ( 'NONE', #18035, #22469 ) ;
#51211 = CARTESIAN_POINT ( 'NONE',  ( 0.6021448801613057400, -1.835062463808373678, 49.07314626535442414 ) ) ;
#51213 = ORIENTED_EDGE ( 'NONE', *, *, #60795, .T. ) ;
#51212 = CARTESIAN_POINT ( 'NONE',  ( 1.088313998177380837, -6.373602917100484433, 42.43756598879026143 ) ) ;
#51214 = VERTEX_POINT ( 'NONE', #9895 ) ;
#51215 = CARTESIAN_POINT ( 'NONE',  ( 5.895596859100789899, 10.82540956478658423, 16.95106754653271608 ) ) ;
#51216 = DIRECTION ( 'NONE',  ( -1.000000000000000000, -0.000000000000000000, -0.000000000000000000 ) ) ;
#51217 = DIRECTION ( 'NONE',  ( 0.000000000000000000, 0.000000000000000000, 1.000000000000000000 ) ) ;
#51218 = EDGE_CURVE ( 'NONE', #56041, #20493, #56741, .T. ) ;
#51219 = ORIENTED_EDGE ( 'NONE', *, *, #29079, .T. ) ;
#51220 = FACE_BOUND ( 'NONE', #17874, .T. ) ;
#51221 = CARTESIAN_POINT ( 'NONE',  ( -6.072942160501519027, -6.664073831083622501, 18.06638542329059760 ) ) ;
#51222 = CARTESIAN_POINT ( 'NONE',  ( 0.6031356755773454870, -44.44549206087170035, -18.40989784469844892 ) ) ;
#51223 = CIRCLE ( 'NONE', #54200, 47.09074272231896430 ) ;
#51224 = ADVANCED_BREP_SHAPE_REPRESENTATION ( '', ( #51018, #14677 ), #15707 ) ;
#51226 = EDGE_CURVE ( 'NONE', #27210, #37845, #15402, .T. ) ;
#51225 = VERTEX_POINT ( 'NONE', #5775 ) ;
#51227 = ORIENTED_EDGE ( 'NONE', *, *, #47889, .F. ) ;
#51228 = CARTESIAN_POINT ( 'NONE',  ( 4.553261556744875094, -43.07273893850278768, -8.618510669438375515 ) ) ;
#51229 = CARTESIAN_POINT ( 'NONE',  ( 1.296416391601052487, 37.53038082136637854, 23.10363368562124720 ) ) ;
#51230 = CARTESIAN_POINT ( 'NONE',  ( 0.9780303403264775097, 32.68824397619722077, -26.22629060976198900 ) ) ;
#51231 = CARTESIAN_POINT ( 'NONE',  ( 1.657374760986086271, -44.03814544053055613, 1.237818003957595669 ) ) ;
#51232 = CARTESIAN_POINT ( 'NONE',  ( 0.7246131072078599855, -23.33689307364222998, -42.06185227555107531 ) ) ;
#51233 =( BOUNDED_SURFACE ( )  B_SPLINE_SURFACE ( 3, 1, ( 
 ( #50119, #55108 ),
 ( #26612, #31628 ),
 ( #31944, #59817 ),
 ( #7808, #12233 ) ),
 .UNSPECIFIED., .F., .F., .F. ) 
 B_SPLINE_SURFACE_WITH_KNOTS ( ( 4, 4 ),
 ( 2, 2 ),
 ( 0.000000000000000000, 1.000000000000000000 ),
 ( 0.000000000000000000, 1.000000000000000000 ),
 .UNSPECIFIED. ) 
 GEOMETRIC_REPRESENTATION_ITEM ( )  RATIONAL_B_SPLINE_SURFACE ( (
 ( 1.000000000000000000, 1.000000000000000000),
 ( 0.9953390228620291325, 0.8624445117761032620),
 ( 0.9953390228620291325, 0.8624445117761032620),
 ( 1.000000000000000000, 1.000000000000000000) ) ) 
 REPRESENTATION_ITEM ( '' )  SURFACE ( )  );
#51234 = B_SPLINE_CURVE_WITH_KNOTS ( 'NONE', 3,
 ( #12877, #17258, #42007, #36381 ),
 .UNSPECIFIED., .F., .F.,
 ( 4, 4 ),
 ( 7.806255641895631925E-18, 0.005014147105413701254 ),
 .UNSPECIFIED. ) ;
#51235 = CARTESIAN_POINT ( 'NONE',  ( 4.453286895665903522, 10.93950075139880518, -2.758850769716832966E-15 ) ) ;
#51236 = ORIENTED_EDGE ( 'NONE', *, *, #52003, .T. ) ;
#51237 = B_SPLINE_CURVE_WITH_KNOTS ( 'NONE', 3,
 ( #28830, #23831, #37325, #14142 ),
 .UNSPECIFIED., .F., .F.,
 ( 4, 4 ),
 ( 0.000000000000000000, 0.004444103432399267029 ),
 .UNSPECIFIED. ) ;
#51238 = CARTESIAN_POINT ( 'NONE',  ( 5.880360259849752858, -47.86623372148048361, -3.184717612777768547 ) ) ;
#51239 = DIRECTION ( 'NONE',  ( 0.000000000000000000, 0.000000000000000000, 1.000000000000000000 ) ) ;
#51240 = ORIENTED_EDGE ( 'NONE', *, *, #33254, .F. ) ;
#51241 = DIRECTION ( 'NONE',  ( 0.000000000000000000, 0.000000000000000000, 1.000000000000000000 ) ) ;
#51242 = CARTESIAN_POINT ( 'NONE',  ( 0.9772918015221172539, 3.781849303984199828, -41.73768646670097837 ) ) ;
#51243 = CARTESIAN_POINT ( 'NONE',  ( 3.240649175237396040, -5.210370887173916721, -43.68199803827362615 ) ) ;
#51244 = EDGE_CURVE ( 'NONE', #18237, #26742, #2137, .T. ) ;
#51245 = VERTEX_POINT ( 'NONE', #24610 ) ;
#51246 = VERTEX_POINT ( 'NONE', #793 ) ;
#51247 = CARTESIAN_POINT ( 'NONE',  ( 0.1158403557922069033, -44.12413028490447431, -0.03786534820748153896 ) ) ;
#51248 = CARTESIAN_POINT ( 'NONE',  ( 0.6000166863083090663, 37.73145429715535215, -31.43502566135631682 ) ) ;
#51249 = EDGE_CURVE ( 'NONE', #21737, #32638, #43430, .T. ) ;
#51250 = VERTEX_POINT ( 'NONE', #34326 ) ;
#51251 = CARTESIAN_POINT ( 'NONE',  ( -6.017396004339686577, -2.460690056887663513, -18.68180398134252940 ) ) ;
#51252 = ORIENTED_EDGE ( 'NONE', *, *, #43584, .F. ) ;
#51254 = ORIENTED_EDGE ( 'NONE', *, *, #33078, .T. ) ;
#51253 = EDGE_CURVE ( 'NONE', #129, #7149, #53401, .T. ) ;
#51255 = CARTESIAN_POINT ( 'NONE',  ( 1.154321713695928064, -4.782433421669802343, -42.64911660416110095 ) ) ;
#51256 = CARTESIAN_POINT ( 'NONE',  ( 5.960721111146673579, 18.96557324978276071, 7.848955554238579602 ) ) ;
#51257 = EDGE_CURVE ( 'NONE', #14851, #24833, #61172, .T. ) ;
#51258 = DIRECTION ( 'NONE',  ( 0.000000000000000000, 0.000000000000000000, 1.000000000000000000 ) ) ;
#51259 = ORIENTED_EDGE ( 'NONE', *, *, #34000, .F. ) ;
#51260 = DIRECTION ( 'NONE',  ( -1.000000000000000000, 0.000000000000000000, 0.000000000000000000 ) ) ;
#51261 = EDGE_CURVE ( 'NONE', #46800, #355, #7637, .T. ) ;
#51262 = CARTESIAN_POINT ( 'NONE',  ( 0.9730545539215883499, 0.5054011016612682816, 42.90536227157002003 ) ) ;
#51263 = CARTESIAN_POINT ( 'NONE',  ( 0.5832655196449135770, -41.95774188719079945, 20.94714965576949339 ) ) ;
#51264 = AXIS2_PLACEMENT_3D ( 'NONE', #6273, #25409, #30411 ) ;
#51265 = VERTEX_POINT ( 'NONE', #17071 ) ;
#51266 = CARTESIAN_POINT ( 'NONE',  ( -20.06025149405489216, -12.49772002914247437, 0.2740165342859215980 ) ) ;
#51267 = AXIS2_PLACEMENT_3D ( 'NONE', #27069, #37414, #22369 ) ;
#51268 = DIRECTION ( 'NONE',  ( 0.000000000000000000, 0.000000000000000000, -1.000000000000000000 ) ) ;
#51269 = CARTESIAN_POINT ( 'NONE',  ( 0.8560838555295158248, 21.73747136795142154, 41.56747734237938374 ) ) ;
#51270 = EDGE_CURVE ( 'NONE', #37539, #6666, #49985, .T. ) ;
#51271 = CARTESIAN_POINT ( 'NONE',  ( 2.526464513654345989, 41.81190200959800052, 9.948146339971373209 ) ) ;
#51272 = CARTESIAN_POINT ( 'NONE',  ( 0.6067099128993244106, 23.33192673707591069, -41.82996792600754077 ) ) ;
#51273 = EDGE_LOOP ( 'NONE', ( #18287, #29442, #25976, #10925 ) ) ;
#51274 = CARTESIAN_POINT ( 'NONE',  ( 0.8551540677456834771, 7.157691013574357441, 47.37911285756623414 ) ) ;
#51275 = CARTESIAN_POINT ( 'NONE',  ( 5.880360259849752858, -47.05949693022714087, 9.312491912827331575 ) ) ;
#51276 = ORIENTED_EDGE ( 'NONE', *, *, #8669, .F. ) ;
#51277 = CARTESIAN_POINT ( 'NONE',  ( 5.959828726073459926, -7.858992891710265383, 18.96145866559658799 ) ) ;
#51278 = CARTESIAN_POINT ( 'NONE',  ( -6.072942160501519027, -18.27985097084440014, 6.054024345238414817 ) ) ;
#51279 = CARTESIAN_POINT ( 'NONE',  ( 5.860006189529234355, 3.171667470662518085, 48.12869875779310291 ) ) ;
#51280 = CARTESIAN_POINT ( 'NONE',  ( 0.9756950546413947212, 5.504753251348322607, -42.55388731055334972 ) ) ;
#51281 = CARTESIAN_POINT ( 'NONE',  ( 4.553261556744875094, 27.21079963941838997, 34.48350256002230196 ) ) ;
#51282 = CARTESIAN_POINT ( 'NONE',  ( 0.5998501479064699549, -41.39809967730504781, 24.50586714782532027 ) ) ;
#51283 = CARTESIAN_POINT ( 'NONE',  ( 0.6029442701453591180, 4.802144870275323107, 48.87212528428824498 ) ) ;
#51284 =( LENGTH_UNIT ( ) NAMED_UNIT ( * ) SI_UNIT ( .MILLI., .METRE. ) );
#51285 = DIRECTION ( 'NONE',  ( 0.000000000000000000, 0.000000000000000000, 1.000000000000000000 ) ) ;
#51286 = CARTESIAN_POINT ( 'NONE',  ( 5.959547316686252039, 14.51632612601508754, 14.51128755440546314 ) ) ;
#51287 = DIRECTION ( 'NONE',  ( 0.000000000000000000, 0.000000000000000000, -1.000000000000000000 ) ) ;
#51288 = CARTESIAN_POINT ( 'NONE',  ( 0.5997462898726536595, 48.29911994996575686, -8.873930482211887849 ) ) ;
#51289 = CARTESIAN_POINT ( 'NONE',  ( 4.553261556744873317, -41.61700166486752295, 14.05577241741092998 ) ) ;
#51290 = B_SPLINE_CURVE_WITH_KNOTS ( 'NONE', 3,
 ( #54655, #7986, #2035, #27100 ),
 .UNSPECIFIED., .F., .F.,
 ( 4, 4 ),
 ( 5.421010862427521207E-19, 0.004444878191957673044 ),
 .UNSPECIFIED. ) ;
#51291 = CARTESIAN_POINT ( 'NONE',  ( 2.528190830796654076, 35.48724657021211470, 22.42564306810345442 ) ) ;
#51292 = CARTESIAN_POINT ( 'NONE',  ( 0.6016118706126976079, -1.225776398925409572, -49.09224508009149446 ) ) ;
#51293 = CARTESIAN_POINT ( 'NONE',  ( 0.5804410086790514622, 40.62771722849963396, 23.42879520283685935 ) ) ;
#51294 = CARTESIAN_POINT ( 'NONE',  ( 3.680882792899937250, -44.99870212802630220, -16.63701193713973936 ) ) ;
#51295 = CARTESIAN_POINT ( 'NONE',  ( 4.962356264823593932, 7.429277797797228189, 41.42513040734459651 ) ) ;
#51296 = CARTESIAN_POINT ( 'NONE',  ( 3.221118495291109607, 32.23766403744527764, -29.92481306659339779 ) ) ;
#51297 = EDGE_CURVE ( 'NONE', #13208, #57613, #8815, .T. ) ;
#51298 = ORIENTED_EDGE ( 'NONE', *, *, #13597, .T. ) ;
#51299 = LINE ( 'NONE', #23125, #32328 ) ;
#51300 = CARTESIAN_POINT ( 'NONE',  ( 5.880360259849739535, 31.59460303415982807, -36.09847387447826605 ) ) ;
#51301 = CARTESIAN_POINT ( 'NONE',  ( 3.678748215320119641, 31.53400377379299258, -37.47291582321680892 ) ) ;
#51302 = CARTESIAN_POINT ( 'NONE',  ( 30.00000000000001066, 4.342925291379521108E-15, -1.386669559958810165E-30 ) ) ;
#51303 = ORIENTED_EDGE ( 'NONE', *, *, #61543, .F. ) ;
#51304 = CARTESIAN_POINT ( 'NONE',  ( -6.077587904424778920, 13.82827771187065302, 13.40055061993020935 ) ) ;
#51305 = B_SPLINE_CURVE_WITH_KNOTS ( 'NONE', 3,
 ( #30406, #11021, #53895, #30102 ),
 .UNSPECIFIED., .F., .F.,
 ( 4, 4 ),
 ( 0.000000000000000000, 0.005014147105413698652 ),
 .UNSPECIFIED. ) ;
#51306 = CONICAL_SURFACE ( 'NONE', #37342, 43.92652462719577500, 1.486293639869522343 ) ;
#51307 = CARTESIAN_POINT ( 'NONE',  ( 0.5809828226811617480, 5.711058609465307967, 47.55412398569209387 ) ) ;
#51308 =( BOUNDED_SURFACE ( )  B_SPLINE_SURFACE ( 3, 1, ( 
 ( #35450, #31662 ),
 ( #21645, #12265 ),
 ( #56065, #46701 ),
 ( #51362, #2828 ) ),
 .UNSPECIFIED., .F., .F., .F. ) 
 B_SPLINE_SURFACE_WITH_KNOTS ( ( 4, 4 ),
 ( 2, 2 ),
 ( 0.000000000000000000, 1.000000000000000000 ),
 ( 0.000000000000000000, 1.000000000000000000 ),
 .UNSPECIFIED. ) 
 GEOMETRIC_REPRESENTATION_ITEM ( )  RATIONAL_B_SPLINE_SURFACE ( (
 ( 1.000000000000000000, 1.000000000000000000),
 ( 0.9953390228620291325, 0.8624445117761032620),
 ( 0.9953390228620291325, 0.8624445117761032620),
 ( 1.000000000000000000, 1.000000000000000000) ) ) 
 REPRESENTATION_ITEM ( '' )  SURFACE ( )  );
#51309 = ORIENTED_EDGE ( 'NONE', *, *, #3667, .F. ) ;
#51310 = DIRECTION ( 'NONE',  ( 3.273063162220391312E-16, -1.000000000000000000, -5.236901059552626099E-15 ) ) ;
#51311 = EDGE_LOOP ( 'NONE', ( #29988, #39246, #53605, #4498 ) ) ;
#51312 = CARTESIAN_POINT ( 'NONE',  ( 0.7048096507298635682, 29.95256433478676072, 37.64898672361963605 ) ) ;
#51313 = CARTESIAN_POINT ( 'NONE',  ( 0.1073791018717483448, 21.98088480513615295, 37.10214135362896570 ) ) ;
#51314 = ORIENTED_EDGE ( 'NONE', *, *, #45446, .T. ) ;
#51315 = CARTESIAN_POINT ( 'NONE',  ( 4.335381028904201628, 42.17650767838711090, -24.91784596868873791 ) ) ;
#51316 = CARTESIAN_POINT ( 'NONE',  ( 3.680974057930774812, 43.58300585207893363, 20.05478739720751236 ) ) ;
#51317 = ORIENTED_EDGE ( 'NONE', *, *, #10559, .F. ) ;
#51318 = CARTESIAN_POINT ( 'NONE',  ( 0.9752132459055856684, 21.65565338840816167, 37.04276540031517584 ) ) ;
#51319 = CARTESIAN_POINT ( 'NONE',  ( -2.708315649062910779, 13.61924161399633526, -5.356004933109328014 ) ) ;
#51320 = VECTOR ( 'NONE', #60399, 1000.000000000000114 ) ;
#51321 = ORIENTED_EDGE ( 'NONE', *, *, #37597, .T. ) ;
#51322 = CARTESIAN_POINT ( 'NONE',  ( -5.995132425357893702, 9.414704407578033951, -16.32377331145310606 ) ) ;
#51323 = EDGE_CURVE ( 'NONE', #22556, #55806, #12375, .T. ) ;
#51324 = EDGE_LOOP ( 'NONE', ( #1711, #21361, #10955, #60117 ) ) ;
#51325 = CARTESIAN_POINT ( 'NONE',  ( 5.960221823109900008, 12.49951306783089322, -16.28072933292535041 ) ) ;
#51327 = EDGE_CURVE ( 'NONE', #1476, #8791, #46391, .T. ) ;
#51326 = ORIENTED_EDGE ( 'NONE', *, *, #16007, .T. ) ;
#51328 = ORIENTED_EDGE ( 'NONE', *, *, #56900, .T. ) ;
#51329 = CARTESIAN_POINT ( 'NONE',  ( 0.6028777368367060907, -42.74543088850748518, -24.17370404937778616 ) ) ;
#51330 = FACE_OUTER_BOUND ( 'NONE', #59020, .T. ) ;
#51331 = FACE_OUTER_BOUND ( 'NONE', #50436, .T. ) ;
#51332 = EDGE_CURVE ( 'NONE', #3794, #18605, #32386, .T. ) ;
#51333 = CARTESIAN_POINT ( 'NONE',  ( 4.694002226626921015, 1.116723307532544451, 45.57452907601513203 ) ) ;
#51334 = ORIENTED_EDGE ( 'NONE', *, *, #9824, .T. ) ;
#51335 = CARTESIAN_POINT ( 'NONE',  ( 1.657374760986086493, 5.460774167333708462, 43.71579111426014208 ) ) ;
#51336 = EDGE_CURVE ( 'NONE', #49382, #31306, #46229, .T. ) ;
#51337 = CARTESIAN_POINT ( 'NONE',  ( 4.956653778116966613, 0.000000000000000000, 0.000000000000000000 ) ) ;
#51338 = CARTESIAN_POINT ( 'NONE',  ( 3.390910168358336918, 0.5608886540481926586, 43.97479437645385048 ) ) ;
#51339 = B_SPLINE_CURVE_WITH_KNOTS ( 'NONE', 3,
 ( #60899, #18012, #13312, #32415 ),
 .UNSPECIFIED., .F., .F.,
 ( 4, 4 ),
 ( 7.152448122690996019E-18, 0.005013413432710146778 ),
 .UNSPECIFIED. ) ;
#51340 = ORIENTED_EDGE ( 'NONE', *, *, #38715, .F. ) ;
#51341 = ORIENTED_EDGE ( 'NONE', *, *, #23256, .F. ) ;
#51342 = CARTESIAN_POINT ( 'NONE',  ( 0.9756354156337444516, 34.12075394380545390, -26.01752520779878353 ) ) ;
#51343 = CARTESIAN_POINT ( 'NONE',  ( 4.335381028904201628, 14.90794766671141858, 46.66379693114287619 ) ) ;
#51344 = CARTESIAN_POINT ( 'NONE',  ( 1.091591847532192627, 40.21132067974347279, 11.82407206281648548 ) ) ;
#51345 = CARTESIAN_POINT ( 'NONE',  ( 0.1100247026804066219, -34.31594964380199997, 26.11768802553187641 ) ) ;
#51346 = CARTESIAN_POINT ( 'NONE',  ( 0.6001305935487422083, 41.92422178329168503, -23.60027211631787125 ) ) ;
#51347 = EDGE_CURVE ( 'NONE', #48086, #19405, #54391, .T. ) ;
#51348 = ORIENTED_EDGE ( 'NONE', *, *, #38917, .T. ) ;
#51349 = CARTESIAN_POINT ( 'NONE',  ( 4.975610109902397937, 13.36434394399692316, 47.05150069959858428 ) ) ;
#51350 = EDGE_CURVE ( 'NONE', #47069, #1293, #7350, .T. ) ;
#51351 = CARTESIAN_POINT ( 'NONE',  ( 0.1073791018717483448, 33.91564619577807349, -26.63563652260133097 ) ) ;
#51352 = CARTESIAN_POINT ( 'NONE',  ( 0.9756354156337436745, -34.12075394380529048, 26.01752520779901445 ) ) ;
#51353 = CARTESIAN_POINT ( 'NONE',  ( 2.533389852662419894, -39.10406001682097354, -20.20700427907317831 ) ) ;
#51354 = LINE ( 'NONE', #32274, #14824 ) ;
#51355 = SURFACE_STYLE_USAGE ( .BOTH. , #27564 ) ;
#51356 = VERTEX_POINT ( 'NONE', #36807 ) ;
#51357 = CARTESIAN_POINT ( 'NONE',  ( 1.000433927950263424, 41.61836910708317561, 4.932548075734225712 ) ) ;
#51358 = FACE_OUTER_BOUND ( 'NONE', #8065, .T. ) ;
#51359 = DIRECTION ( 'NONE',  ( -1.000000000000000000, -1.836909530733573776E-16, 1.925929944387235306E-32 ) ) ;
#51360 = CARTESIAN_POINT ( 'NONE',  ( 0.1102847568649952675, 21.48234084756696305, -37.39286109091555943 ) ) ;
#51361 = CARTESIAN_POINT ( 'NONE',  ( 0.6000166863083090663, -1.051715750663601012, -49.09905676984293876 ) ) ;
#51362 = CARTESIAN_POINT ( 'NONE',  ( 5.960721111146673579, 18.96073515164548340, -7.860635756377695849 ) ) ;
#51363 = B_SPLINE_CURVE_WITH_KNOTS ( 'NONE', 3,
 ( #54271, #29567, #30478, #58666 ),
 .UNSPECIFIED., .F., .F.,
 ( 4, 4 ),
 ( 0.000000000000000000, 0.005004948556313810505 ),
 .UNSPECIFIED. ) ;
#51364 = CARTESIAN_POINT ( 'NONE',  ( 0.6021447746440204973, -49.10674983770864088, 0.2612651243270994184 ) ) ;
#51365 = VECTOR ( 'NONE', #39343, 999.9999999999998863 ) ;
#51366 = CARTESIAN_POINT ( 'NONE',  ( 0.5807400328401637335, -11.87003418057275539, 46.40483864045141615 ) ) ;
#51367 = EDGE_CURVE ( 'NONE', #39717, #40072, #13390, .T. ) ;
#51368 = CARTESIAN_POINT ( 'NONE',  ( -6.010958268070873523, 14.95835081545489409, -11.45964880703811595 ) ) ;
#51369 = ORIENTED_EDGE ( 'NONE', *, *, #45923, .F. ) ;
#51370 = CARTESIAN_POINT ( 'NONE',  ( 3.660087539127323542, -43.62750476736565730, 20.10768839917389883 ) ) ;
#51371 = CARTESIAN_POINT ( 'NONE',  ( 0.9789889208857691649, 20.22481679127239218, 36.70547212340194676 ) ) ;
#51372 = LINE ( 'NONE', #32921, #21143 ) ;
#51373 = CARTESIAN_POINT ( 'NONE',  ( 5.860006189529234355, 43.25137511473280938, -21.34829429597422035 ) ) ;
#51374 = ORIENTED_EDGE ( 'NONE', *, *, #61843, .F. ) ;
#51375 = CARTESIAN_POINT ( 'NONE',  ( 0.7056555295713292653, -46.04438433984162771, 13.20840017675001832 ) ) ;
#51376 = CARTESIAN_POINT ( 'NONE',  ( 0.1145239942831223490, 3.911746048396175901, 43.95046897994981805 ) ) ;
#51377 = ORIENTED_EDGE ( 'NONE', *, *, #16839, .T. ) ;
#51378 = CARTESIAN_POINT ( 'NONE',  ( 8.000000000000007105, -54.69470952477976766, 58.44237546506786884 ) ) ;
#51379 = CARTESIAN_POINT ( 'NONE',  ( -6.015611763856276717, 18.68122482568280063, 2.465697960551114232 ) ) ;
#51380 = CARTESIAN_POINT ( 'NONE',  ( -6.078457390727109555, 17.84708778612949587, 7.230212209312759875 ) ) ;
#51382 = ORIENTED_EDGE ( 'NONE', *, *, #9451, .T. ) ;
#51381 =( BOUNDED_SURFACE ( )  B_SPLINE_SURFACE ( 3, 1, ( 
 ( #30501, #16739 ),
 ( #1680, #45564 ),
 ( #20819, #17055 ),
 ( #54298, #35855 ) ),
 .UNSPECIFIED., .F., .F., .F. ) 
 B_SPLINE_SURFACE_WITH_KNOTS ( ( 4, 4 ),
 ( 2, 2 ),
 ( 0.000000000000000000, 1.000000000000000000 ),
 ( 0.000000000000000000, 1.000000000000000000 ),
 .UNSPECIFIED. ) 
 GEOMETRIC_REPRESENTATION_ITEM ( )  RATIONAL_B_SPLINE_SURFACE ( (
 ( 1.000000000000000000, 1.000000000000000000),
 ( 0.9953485035131437453, 0.8621029689291523912),
 ( 0.9953485035131437453, 0.8621029689291523912),
 ( 1.000000000000000000, 1.000000000000000000) ) ) 
 REPRESENTATION_ITEM ( '' )  SURFACE ( )  );
#51383 = CARTESIAN_POINT ( 'NONE',  ( 0.7246131072078553226, 46.24389631750668883, 13.24054562911141808 ) ) ;
#51384 = ORIENTED_EDGE ( 'NONE', *, *, #23018, .F. ) ;
#51385 = VERTEX_POINT ( 'NONE', #57944 ) ;
#51386 = DIRECTION ( 'NONE',  ( -1.000000000000000000, -0.000000000000000000, -0.000000000000000000 ) ) ;
#51387 = VERTEX_POINT ( 'NONE', #32403 ) ;
#51388 = CARTESIAN_POINT ( 'NONE',  ( 5.896278296736517710, 5.953715084307799721, -19.21146158701282758 ) ) ;
#51389 = AXIS2_PLACEMENT_3D ( 'NONE', #45853, #47682, #23255 ) ;
#51390 = ORIENTED_EDGE ( 'NONE', *, *, #47396, .F. ) ;
#51391 = CARTESIAN_POINT ( 'NONE',  ( 4.960386119450151732, 43.68547429165921159, -2.452712903118141607 ) ) ;
#51392 = CARTESIAN_POINT ( 'NONE',  ( 0.6000166863083106206, 5.235566842225154005, -48.83044461756462340 ) ) ;
#51393 = CARTESIAN_POINT ( 'NONE',  ( 0.9747592971366236814, 16.71904224817905771, 39.51726118357597528 ) ) ;
#51394 = EDGE_CURVE ( 'NONE', #10420, #11294, #23035, .T. ) ;
#51395 = ORIENTED_EDGE ( 'NONE', *, *, #58378, .T. ) ;
#51396 = CARTESIAN_POINT ( 'NONE',  ( 42.00000000000000711, 0.000000000000000000, 0.000000000000000000 ) ) ;
#51397 = CARTESIAN_POINT ( 'NONE',  ( 0.5549461598389366923, -37.99084232143810169, 22.40342820138097579 ) ) ;
#51398 = CARTESIAN_POINT ( 'NONE',  ( 0.5797568665920715958, 46.89167813730860956, -0.6291502753107942603 ) ) ;
#51399 = VERTEX_POINT ( 'NONE', #17677 ) ;
#51400 = EDGE_CURVE ( 'NONE', #10739, #42739, #37417, .T. ) ;
#51401 = DIRECTION ( 'NONE',  ( 0.8660254037844371533, 0.5000000000000025535, 0.000000000000000000 ) ) ;
#51402 = CARTESIAN_POINT ( 'NONE',  ( 0.1129192098497447394, -32.03190746134960420, -30.34647742609823595 ) ) ;
#51403 = AXIS2_PLACEMENT_3D ( 'NONE', #26302, #41060, #41356 ) ;
#51404 = ORIENTED_EDGE ( 'NONE', *, *, #37497, .T. ) ;
#51405 = DIRECTION ( 'NONE',  ( 0.000000000000000000, 0.000000000000000000, 1.000000000000000000 ) ) ;
#51406 = ORIENTED_EDGE ( 'NONE', *, *, #16060, .F. ) ;
#51407 = CARTESIAN_POINT ( 'NONE',  ( 4.960386119450153508, 0.9915941002484534028, 43.74303608361783802 ) ) ;
#51408 = CARTESIAN_POINT ( 'NONE',  ( 0.5807400328401637335, -23.47602859900684535, -41.75144119563910294 ) ) ;
#51409 = ORIENTED_EDGE ( 'NONE', *, *, #60869, .T. ) ;
#51410 = DIRECTION ( 'NONE',  ( 0.000000000000000000, 0.000000000000000000, 1.000000000000000000 ) ) ;
#51411 = CARTESIAN_POINT ( 'NONE',  ( -6.077587904424778920, 7.800189710370847074, -17.60548385805273242 ) ) ;
#51412 = CARTESIAN_POINT ( 'NONE',  ( 0.5997462898726536595, 27.66511329191589397, 40.57330571557817223 ) ) ;
#51413 = DIRECTION ( 'NONE',  ( 0.000000000000000000, 0.000000000000000000, 1.000000000000000000 ) ) ;
#51414 = ORIENTED_EDGE ( 'NONE', *, *, #35586, .F. ) ;
#51415 = CARTESIAN_POINT ( 'NONE',  ( 4.553261556744875094, -20.11719049292643646, -39.04917684785361587 ) ) ;
#51416 = CARTESIAN_POINT ( 'NONE',  ( 5.965394784446460541, 18.96850062921634361, -7.841344330024745624 ) ) ;
#51417 = CARTESIAN_POINT ( 'NONE',  ( 0.9741495583595177754, -16.78504838919912245, 39.48917442789116450 ) ) ;
#51418 = EDGE_CURVE ( 'NONE', #61199, #56898, #61487, .T. ) ;
#51419 = CARTESIAN_POINT ( 'NONE',  ( 0.5782707292762423457, 45.03824936633927223, -13.08787407194379604 ) ) ;
#51420 = B_SPLINE_CURVE_WITH_KNOTS ( 'NONE', 3,
 ( #57198, #14333, #61898, #33439 ),
 .UNSPECIFIED., .F., .F.,
 ( 4, 4 ),
 ( 2.602085213965210642E-18, 0.004050076154993004218 ),
 .UNSPECIFIED. ) ;
#51421 = CARTESIAN_POINT ( 'NONE',  ( 0.5997462898726536595, 44.01516392039482639, 21.77652348757905898 ) ) ;
#51422 = DIRECTION ( 'NONE',  ( 0.000000000000000000, 0.000000000000000000, -1.000000000000000000 ) ) ;
#51423 = CARTESIAN_POINT ( 'NONE',  ( 1.157644175074337367, 41.90847804166124035, 0.8256777281599040341 ) ) ;
#51424 = B_SPLINE_CURVE_WITH_KNOTS ( 'NONE', 3,
 ( #53221, #52919, #29730, #29117 ),
 .UNSPECIFIED., .F., .F.,
 ( 4, 4 ),
 ( 3.496446946337351263E-17, 0.005004948556313842598 ),
 .UNSPECIFIED. ) ;
#51425 = CARTESIAN_POINT ( 'NONE',  ( 0.5839254288179547281, -46.28738487712336536, 12.30867641975561178 ) ) ;
#51426 = CARTESIAN_POINT ( 'NONE',  ( -6.078075953587585900, -19.21681836813549182, -1.228440496412561478 ) ) ;
#51427 = CARTESIAN_POINT ( 'NONE',  ( 1.227938101723748288, 4.762198645644436290, 42.65467462194920500 ) ) ;
#51428 = CARTESIAN_POINT ( 'NONE',  ( -6.057079549204054558, 13.82732400278046470, 13.40284828019289698 ) ) ;
#51429 = DIRECTION ( 'NONE',  ( -1.000000000000000000, -0.000000000000000000, 1.925929944387235853E-32 ) ) ;
#51430 = CARTESIAN_POINT ( 'NONE',  ( 2.643462169533613793, 17.09809940585662247, -44.89050350746133944 ) ) ;
#51431 = CARTESIAN_POINT ( 'NONE',  ( 0.5806925824938499181, 46.54710689580866756, -5.708695295225145294 ) ) ;
#51432 = CARTESIAN_POINT ( 'NONE',  ( 0.9736507210033064075, 36.93248879681210184, 21.84312502845804005 ) ) ;
#51433 = CARTESIAN_POINT ( 'NONE',  ( 4.549368137175248350, 0.000000000000000000, 0.000000000000000000 ) ) ;
#51434 = CARTESIAN_POINT ( 'NONE',  ( 0.9747592971366237924, -37.32069240268756971, -21.17324310849270930 ) ) ;
#51435 = ADVANCED_FACE ( 'NONE', ( #13927 ), #34977, .F. ) ;
#51436 = CARTESIAN_POINT ( 'NONE',  ( 5.895596859100789899, -4.659086063546006073, 19.56581458219818259 ) ) ;
#51437 = CARTESIAN_POINT ( 'NONE',  ( 4.958415959904820092, -10.03736369554633079, -44.29960816831192716 ) ) ;
#51439 = VERTEX_POINT ( 'NONE', #41502 ) ;
#51438 = FACE_OUTER_BOUND ( 'NONE', #20750, .T. ) ;
#51440 = ORIENTED_EDGE ( 'NONE', *, *, #48935, .T. ) ;
#51441 = CARTESIAN_POINT ( 'NONE',  ( 0.6027444965799114707, -39.43333548727365923, 29.26688518164454322 ) ) ;
#51442 = CARTESIAN_POINT ( 'NONE',  ( 4.335381028904201628, 45.01666255113143933, -19.31985870605438294 ) ) ;
#51443 = CARTESIAN_POINT ( 'NONE',  ( 0.5809828226811617480, -34.25055090842177208, 33.48000389720603920 ) ) ;
#51444 = ORIENTED_EDGE ( 'NONE', *, *, #21547, .T. ) ;
#51445 = VERTEX_POINT ( 'NONE', #55878 ) ;
#51446 = CARTESIAN_POINT ( 'NONE',  ( 4.956653778116992370, 27.17045123668527751, -39.67974989265010777 ) ) ;
#51447 = AXIS2_PLACEMENT_3D ( 'NONE', #7188, #59204, #16308 ) ;
#51448 = CARTESIAN_POINT ( 'NONE',  ( 0.1073791018717578927, 21.14095454447508615, 37.58707531572213156 ) ) ;
#51449 = B_SPLINE_CURVE_WITH_KNOTS ( 'NONE', 3,
 ( #40914, #59042, #36199, #59348 ),
 .UNSPECIFIED., .F., .F.,
 ( 4, 4 ),
 ( 5.553824967135426632E-18, 0.004566006591234645501 ),
 .UNSPECIFIED. ) ;
#51450 = EDGE_CURVE ( 'NONE', #55332, #29824, #38890, .T. ) ;
#51451 = ORIENTED_EDGE ( 'NONE', *, *, #844, .F. ) ;
#51452 = ORIENTED_EDGE ( 'NONE', *, *, #53084, .T. ) ;
#51453 = CARTESIAN_POINT ( 'NONE',  ( 0.9756354156337452288, -10.97961179198170356, -41.47994205070126128 ) ) ;
#51454 = EDGE_CURVE ( 'NONE', #19355, #35035, #43241, .T. ) ;
#51455 = CARTESIAN_POINT ( 'NONE',  ( 0.7764146366350244133, 3.807011318490865825, -46.74983570548722156 ) ) ;
#51456 = DIRECTION ( 'NONE',  ( -0.9848077530122077983, -0.1736481776669316079, 1.387778780781445367E-17 ) ) ;
#51457 = ORIENTED_EDGE ( 'NONE', *, *, #20886, .T. ) ;
#51458 = ORIENTED_EDGE ( 'NONE', *, *, #14232, .F. ) ;
#51459 = ORIENTED_EDGE ( 'NONE', *, *, #17947, .T. ) ;
#51460 = CARTESIAN_POINT ( 'NONE',  ( 5.331199999999999051, 15.38217999999999996, 0.000000000000000000 ) ) ;
#51461 = DIRECTION ( 'NONE',  ( -1.000000000000000000, -0.000000000000000000, -0.000000000000000000 ) ) ;
#51462 = ORIENTED_EDGE ( 'NONE', *, *, #50248, .F. ) ;
#51463 = CIRCLE ( 'NONE', #27474, 43.92652462719577500 ) ;
#51464 = CARTESIAN_POINT ( 'NONE',  ( 0.1102847568649952675, 21.64199720113191105, 37.30068345220698944 ) ) ;
#51465 = VERTEX_POINT ( 'NONE', #37116 ) ;
#51466 = EDGE_CURVE ( 'NONE', #37333, #59460, #45412, .T. ) ;
#51467 = ORIENTED_EDGE ( 'NONE', *, *, #12836, .F. ) ;
#51468 = CARTESIAN_POINT ( 'NONE',  ( 0.9722240750034587542, -29.92651530838607954, 30.74950257331008885 ) ) ;
#51469 = ORIENTED_EDGE ( 'NONE', *, *, #13855, .F. ) ;
#51470 = CARTESIAN_POINT ( 'NONE',  ( 0.6016118706126978299, -48.74769260159513351, 5.934098145827796600 ) ) ;
#51471 = CARTESIAN_POINT ( 'NONE',  ( 4.691466044806102964, 14.64802401911229701, -42.11359095667474861 ) ) ;
#51472 = CARTESIAN_POINT ( 'NONE',  ( 4.967162193818130511, 0.000000000000000000, 0.000000000000000000 ) ) ;
#51473 = CARTESIAN_POINT ( 'NONE',  ( 0.5817217712918331118, -38.91886904608055175, 26.16403229975087186 ) ) ;
#51474 = DIRECTION ( 'NONE',  ( 0.1011922191286468292, -0.9849719771322142936, 0.1399654923617842661 ) ) ;
#51475 = ADVANCED_FACE ( 'NONE', ( #46824, #3863 ), #47124, .T. ) ;
#51476 = ORIENTED_EDGE ( 'NONE', *, *, #41415, .F. ) ;
#51477 = CARTESIAN_POINT ( 'NONE',  ( 2.643462169533600914, 13.76277278785560654, -46.02269433264218179 ) ) ;
#51478 = CARTESIAN_POINT ( 'NONE',  ( 0.5988103622719992414, 24.57719485303637796, -41.35593060299647306 ) ) ;
#51479 = ADVANCED_FACE ( 'NONE', ( #32712 ), #39372, .F. ) ;
#51480 =( BOUNDED_SURFACE ( )  B_SPLINE_SURFACE ( 3, 1, ( 
 ( #29707, #43850 ),
 ( #44165, #1195 ),
 ( #20329, #7114 ),
 ( #60354, #54735 ) ),
 .UNSPECIFIED., .F., .F., .F. ) 
 B_SPLINE_SURFACE_WITH_KNOTS ( ( 4, 4 ),
 ( 2, 2 ),
 ( 0.000000000000000000, 1.000000000000000000 ),
 ( 0.000000000000000000, 1.000000000000000000 ),
 .UNSPECIFIED. ) 
 GEOMETRIC_REPRESENTATION_ITEM ( )  RATIONAL_B_SPLINE_SURFACE ( (
 ( 1.000000000000000000, 1.000000000000000000),
 ( 0.9952954269826590483, 0.8620686068821307169),
 ( 0.9952954269826590483, 0.8620686068821307169),
 ( 1.000000000000000000, 1.000000000000000000) ) ) 
 REPRESENTATION_ITEM ( '' )  SURFACE ( )  );
#51481 = CARTESIAN_POINT ( 'NONE',  ( -6.016761891674565099, -18.68243340030204536, 2.456125503350645278 ) ) ;
#51482 = VECTOR ( 'NONE', #12786, 1000.000000000000000 ) ;
#51483 = VERTEX_POINT ( 'NONE', #53554 ) ;
#51484 = CARTESIAN_POINT ( 'NONE',  ( 0.1097557419366048670, 42.72583172879053137, -5.849988371690637123 ) ) ;
#51485 = DIRECTION ( 'NONE',  ( 0.000000000000000000, 0.000000000000000000, 1.000000000000000000 ) ) ;
#51486 = CARTESIAN_POINT ( 'NONE',  ( 0.9754642270333676590, 30.21634823122169777, 30.46484943293168257 ) ) ;
#51487 = CARTESIAN_POINT ( 'NONE',  ( 1.227938101723748288, 42.65467462194924764, -4.762198645644009076 ) ) ;
#51489 = ORIENTED_EDGE ( 'NONE', *, *, #38579, .T. ) ;
#51488 = CIRCLE ( 'NONE', #24492, 43.08621763946400307 ) ;
#51490 = CARTESIAN_POINT ( 'NONE',  ( 4.967162193818130511, 18.65818244221310351, -38.83676580803746958 ) ) ;
#51491 = PLANE ( 'NONE',  #26680 ) ;
#51492 = CARTESIAN_POINT ( 'NONE',  ( 5.958863334805807099, -10.26388325355075359, -17.77512673691315470 ) ) ;
#51493 = EDGE_CURVE ( 'NONE', #10204, #32930, #21378, .T. ) ;
#51494 = VECTOR ( 'NONE', #53693, 1000.000000000000114 ) ;
#51495 = B_SPLINE_CURVE_WITH_KNOTS ( 'NONE', 3,
 ( #55632, #41575, #50942, #31230 ),
 .UNSPECIFIED., .F., .F.,
 ( 4, 4 ),
 ( 0.000000000000000000, 0.005004741218457409331 ),
 .UNSPECIFIED. ) ;
#51496 = CARTESIAN_POINT ( 'NONE',  ( 0.1147471544378676350, -18.14425483850216025, -40.22111640455466386 ) ) ;
#51497 = CARTESIAN_POINT ( 'NONE',  ( 0.2940135542859022566, 10.59968125873896305, 42.82391044620469955 ) ) ;
#51498 =( BOUNDED_SURFACE ( )  B_SPLINE_SURFACE ( 3, 1, ( 
 ( #37334, #18848 ),
 ( #47961, #52018 ),
 ( #9115, #38575 ),
 ( #28221, #28524 ) ),
 .UNSPECIFIED., .F., .F., .F. ) 
 B_SPLINE_SURFACE_WITH_KNOTS ( ( 4, 4 ),
 ( 2, 2 ),
 ( 0.000000000000000000, 1.000000000000000000 ),
 ( 0.000000000000000000, 1.000000000000000000 ),
 .UNSPECIFIED. ) 
 GEOMETRIC_REPRESENTATION_ITEM ( )  RATIONAL_B_SPLINE_SURFACE ( (
 ( 1.000000000000000000, 1.000000000000000000),
 ( 0.9952954269826590483, 0.8620686068821307169),
 ( 0.9952954269826590483, 0.8620686068821307169),
 ( 1.000000000000000000, 1.000000000000000000) ) ) 
 REPRESENTATION_ITEM ( '' )  SURFACE ( )  );
#51499 = CARTESIAN_POINT ( 'NONE',  ( 5.958863334805807099, 12.49425770716487527, -16.28483817244726950 ) ) ;
#51500 = CARTESIAN_POINT ( 'NONE',  ( -48.95476116535499500, 0.000000000000000000, 0.000000000000000000 ) ) ;
#51501 = CARTESIAN_POINT ( 'NONE',  ( 0.8751705887134553219, 29.98056538504910051, 37.60752970653838645 ) ) ;
#51502 = CARTESIAN_POINT ( 'NONE',  ( 0.9762797500689124330, -1.905951756780080775, -41.86516610604251554 ) ) ;
#51503 = CARTESIAN_POINT ( 'NONE',  ( 0.1129192098497447394, -17.41650932123218354, 40.54154647825593827 ) ) ;
#51504 = VERTEX_POINT ( 'NONE', #10670 ) ;
#51505 = CARTESIAN_POINT ( 'NONE',  ( 0.5806925824938494740, -46.75147433417404841, 3.677228565731047283 ) ) ;
#51506 = CARTESIAN_POINT ( 'NONE',  ( 0.1073791018717578927, -42.68962945260949482, -6.109314776652552403 ) ) ;
#51507 = CARTESIAN_POINT ( 'NONE',  ( 2.624215991343608501, -13.78323291683815377, 45.98641578154027343 ) ) ;
#51508 = CARTESIAN_POINT ( 'NONE',  ( 0.5817216825391108292, -35.08429596696358743, -31.11795508560874524 ) ) ;
#51509 = CARTESIAN_POINT ( 'NONE',  ( 1.296416391601052265, -23.78941374985365442, -37.09947664744655782 ) ) ;
#51510 = CARTESIAN_POINT ( 'NONE',  ( 0.1103310638050661735, 42.74468893497609656, 5.710544932889072278 ) ) ;
#51511 = CONTEXT_DEPENDENT_SHAPE_REPRESENTATION ( #35172, #49764 ) ;
#51512 = CARTESIAN_POINT ( 'NONE',  ( 3.680974057930773036, -22.36814223828938353, -42.44218549341202618 ) ) ;
#51513 = AXIS2_PLACEMENT_3D ( 'NONE', #38167, #37862, #33457 ) ;
#51514 = CARTESIAN_POINT ( 'NONE',  ( 0.8554163680231816613, 9.985124899324974379, -45.84215040611314862 ) ) ;
#51515 = CARTESIAN_POINT ( 'NONE',  ( 0.8560838555295158248, -18.91252766612255698, -42.92655508376930129 ) ) ;
#51517 = ORIENTED_EDGE ( 'NONE', *, *, #17610, .T. ) ;
#51516 = CARTESIAN_POINT ( 'NONE',  ( 1.227938101723756947, -36.73927144310528092, 22.18841447410706635 ) ) ;
#51518 = ORIENTED_EDGE ( 'NONE', *, *, #44539, .F. ) ;
#51519 = B_SPLINE_CURVE_WITH_KNOTS ( 'NONE', 3,
 ( #30945, #17166, #50653, #60061, #20930, #11537 ),
 .UNSPECIFIED., .F., .F.,
 ( 4, 2, 4 ),
 ( 9.872790465222285426E-18, 0.0002448709889506573193, 0.0004897419779013047723 ),
 .UNSPECIFIED. ) ;
#51520 = DIRECTION ( 'NONE',  ( 0.000000000000000000, 0.000000000000000000, -1.000000000000000000 ) ) ;
#51521 = CARTESIAN_POINT ( 'NONE',  ( 0.1102144999581332746, 39.79340763430485595, 16.61938362665564028 ) ) ;
#51522 = CARTESIAN_POINT ( 'NONE',  ( 5.917102823773431552, 17.95415397368203614, -9.063005745394821844 ) ) ;
#51523 = ADVANCED_FACE ( 'NONE', ( #44827 ), #56531, .F. ) ;
#51524 = VERTEX_POINT ( 'NONE', #21302 ) ;
#51525 = DIRECTION ( 'NONE',  ( -0.000000000000000000, 1.000000000000000000, 1.224646799147353207E-16 ) ) ;
#51526 = DIRECTION ( 'NONE',  ( 0.000000000000000000, 0.000000000000000000, 1.000000000000000000 ) ) ;
#51527 = CARTESIAN_POINT ( 'NONE',  ( 3.407937589446178528, 6.447869442558332942, -12.08659953757602068 ) ) ;
#51528 = EDGE_CURVE ( 'NONE', #593, #30431, #20686, .T. ) ;
#51529 = ORIENTED_EDGE ( 'NONE', *, *, #22135, .F. ) ;
#51530 = ORIENTED_EDGE ( 'NONE', *, *, #45996, .F. ) ;
#51531 = CARTESIAN_POINT ( 'NONE',  ( 0.9730545539215883499, 41.57420493492384850, 10.61654491617579055 ) ) ;
#51532 = EDGE_CURVE ( 'NONE', #5852, #18698, #54473, .T. ) ;
#51534 = CARTESIAN_POINT ( 'NONE',  ( 3.221118495291108719, 37.86046104227076370, 22.39077732747234251 ) ) ;
#51533 = CIRCLE ( 'NONE', #10556, 42.92674063221959813 ) ;
#51535 = CARTESIAN_POINT ( 'NONE',  ( 0.6023143664670691511, 41.53077189784229972, 24.28012784216892683 ) ) ;
#51537 = CARTESIAN_POINT ( 'NONE',  ( 4.960386119450139297, 39.26151414358965042, 19.31243050019988772 ) ) ;
#51536 = CIRCLE ( 'NONE', #4529, 15.99999999999999645 ) ;
#51538 = CARTESIAN_POINT ( 'NONE',  ( 3.678748215320120973, 26.48317992319705283, -41.19774260144669853 ) ) ;
#51539 = CARTESIAN_POINT ( 'NONE',  ( -6.078457390727109555, -6.646245994447285810, 18.07268450504245294 ) ) ;
#51540 = ORIENTED_EDGE ( 'NONE', *, *, #33800, .F. ) ;
#51541 = EDGE_CURVE ( 'NONE', #10414, #58260, #29016, .T. ) ;
#51542 = CARTESIAN_POINT ( 'NONE',  ( 1.827326673878744145, 41.88502433275003511, -9.946825761454068271 ) ) ;
#51543 = CARTESIAN_POINT ( 'NONE',  ( -6.016104459813374383, -18.84322058118302223, -0.005335450885264243250 ) ) ;
#51544 = VERTEX_POINT ( 'NONE', #34791 ) ;
#51545 = CARTESIAN_POINT ( 'NONE',  ( 0.8753041380234524160, -45.17330286263802464, 19.24866323549142422 ) ) ;
#51546 = EDGE_CURVE ( 'NONE', #38319, #5144, #59187, .T. ) ;
#51547 = CARTESIAN_POINT ( 'NONE',  ( -2.739355103387248747, 14.08251715046648833, -4.952805029257079994 ) ) ;
#51548 = CARTESIAN_POINT ( 'NONE',  ( 0.9790320750461898314, 4.280404874073830968, -41.68951027124445119 ) ) ;
#51549 = CARTESIAN_POINT ( 'NONE',  ( 4.963659409799330291, -13.93274247732050597, 42.53037318520990340 ) ) ;
#51550 = ORIENTED_EDGE ( 'NONE', *, *, #52464, .T. ) ;
#51551 = ORIENTED_EDGE ( 'NONE', *, *, #31323, .T. ) ;
#51552 = CARTESIAN_POINT ( 'NONE',  ( 0.9757619758474603833, 0.06449181910581339161, 42.90842306541549789 ) ) ;
#51553 = CARTESIAN_POINT ( 'NONE',  ( 0.5839879882012685153, 41.47913983251949332, 23.94795769224401027 ) ) ;
#51554 = ADVANCED_FACE ( 'NONE', ( #49487 ), #44148, .F. ) ;
#51555 = DIRECTION ( 'NONE',  ( 0.09722883295013595717, 0.08804304236304483222, 0.9913601649928313053 ) ) ;
#51556 = ORIENTED_EDGE ( 'NONE', *, *, #11123, .T. ) ;
#51557 = DIRECTION ( 'NONE',  ( 0.000000000000000000, 0.000000000000000000, -1.000000000000000000 ) ) ;
#51558 = ORIENTED_EDGE ( 'NONE', *, *, #1833, .F. ) ;
#51559 = CARTESIAN_POINT ( 'NONE',  ( 0.8760168074886960365, 46.22580377597767409, 13.30888447662096397 ) ) ;
#51560 = CARTESIAN_POINT ( 'NONE',  ( 0.6016117650947689910, -25.15845835820325149, 42.17348725541975085 ) ) ;
#51561 = CARTESIAN_POINT ( 'NONE',  ( 0.1129192098497447394, 36.71339784380064231, -24.47607416535520741 ) ) ;
#51562 = ORIENTED_EDGE ( 'NONE', *, *, #40365, .T. ) ;
#51563 = CARTESIAN_POINT ( 'NONE',  ( -79.49999999999975842, 2.999999999999995559, -1.499999999999999778 ) ) ;
#51564 = CARTESIAN_POINT ( 'NONE',  ( 40.00000000000000000, 4.422198837962619519E-47, 12.50000000000000000 ) ) ;
#51565 = CARTESIAN_POINT ( 'NONE',  ( 0.5835226383429291674, -41.77317149982144429, 21.31301521119128140 ) ) ;
#51566 = EDGE_CURVE ( 'NONE', #23307, #472, #34402, .T. ) ;
#51567 = EDGE_LOOP ( 'NONE', ( #7512, #7144, #55715, #12116 ) ) ;
#51568 = CARTESIAN_POINT ( 'NONE',  ( 0.6009452777970412107, -29.63106797105387713, -37.89911497740560975 ) ) ;
#51569 = FACE_BOUND ( 'NONE', #37090, .T. ) ;
#51570 = FACE_OUTER_BOUND ( 'NONE', #40591, .T. ) ;
#51571 = EDGE_CURVE ( 'NONE', #42948, #61884, #47407, .T. ) ;
#51572 = CARTESIAN_POINT ( 'NONE',  ( 0.1102847568649952675, 26.17930421801151297, -34.26895182984672061 ) ) ;
#51573 = CARTESIAN_POINT ( 'NONE',  ( 0.1119899015040012602, -38.71871408100971479, 21.16181674869922702 ) ) ;
#51574 = ORIENTED_EDGE ( 'NONE', *, *, #47326, .F. ) ;
#51575 =( BOUNDED_SURFACE ( )  B_SPLINE_SURFACE ( 3, 1, ( 
 ( #42190, #61247 ),
 ( #23365, #42488 ),
 ( #23977, #61551 ),
 ( #43105, #37803 ) ),
 .UNSPECIFIED., .F., .F., .F. ) 
 B_SPLINE_SURFACE_WITH_KNOTS ( ( 4, 4 ),
 ( 2, 2 ),
 ( 0.000000000000000000, 1.000000000000000000 ),
 ( 0.000000000000000000, 1.000000000000000000 ),
 .UNSPECIFIED. ) 
 GEOMETRIC_REPRESENTATION_ITEM ( )  RATIONAL_B_SPLINE_SURFACE ( (
 ( 1.000000000000000000, 1.000000000000000000),
 ( 0.9953040768229005630, 0.8617119497784937465),
 ( 0.9953040768229005630, 0.8617119497784937465),
 ( 1.000000000000000000, 1.000000000000000000) ) ) 
 REPRESENTATION_ITEM ( '' )  SURFACE ( )  );
#51576 = FACE_OUTER_BOUND ( 'NONE', #31395, .T. ) ;
#51577 = EDGE_LOOP ( 'NONE', ( #32926, #33863, #8495, #35728 ) ) ;
#51578 = CIRCLE ( 'NONE', #17575, 2.649999999999999467 ) ;
#51579 = CARTESIAN_POINT ( 'NONE',  ( 4.553261556744875094, 0.000000000000000000, 0.000000000000000000 ) ) ;
#51580 = CARTESIAN_POINT ( 'NONE',  ( 0.9785694773339250752, -27.22697983396325583, 31.85948798765653223 ) ) ;
#51581 = CARTESIAN_POINT ( 'NONE',  ( 4.549368137175248350, 3.018832571116558672, -42.82045902618769873 ) ) ;
#51582 = AXIS2_PLACEMENT_3D ( 'NONE', #15794, #11094, #53969 ) ;
#51583 = CARTESIAN_POINT ( 'NONE',  ( 0.9736507210033064075, 6.046964561328548982, -42.48017254354716954 ) ) ;
#51584 = CARTESIAN_POINT ( 'NONE',  ( 5.960221823109900008, -10.26751639438355923, -17.77295928189551688 ) ) ;
#51585 = CARTESIAN_POINT ( 'NONE',  ( 4.967162193818130511, 14.26841313271282097, 40.65506779172170582 ) ) ;
#51586 = CARTESIAN_POINT ( 'NONE',  ( 0.3622758884714730732, -0.8252992914325094631, -43.10531414739105571 ) ) ;
#51587 =( NAMED_UNIT ( * ) PLANE_ANGLE_UNIT ( ) SI_UNIT ( $, .RADIAN. ) );
#51588 = LINE ( 'NONE', #27802, #3704 ) ;
#51589 = CARTESIAN_POINT ( 'NONE',  ( 5.959828726073459926, -17.77796293532179916, 10.25888482581828676 ) ) ;
#51590 = CARTESIAN_POINT ( 'NONE',  ( 3.270143674763207553, 1.514386915940589384, 13.60381564321234826 ) ) ;
#51591 = CIRCLE ( 'NONE', #7590, 5.633200000000004870 ) ;
#51592 = CARTESIAN_POINT ( 'NONE',  ( 0.1101816497532063510, -5.494186916736032877, 42.77304337559933600 ) ) ;
#51593 = ORIENTED_EDGE ( 'NONE', *, *, #34454, .T. ) ;
#51594 = CARTESIAN_POINT ( 'NONE',  ( 5.960721111146673579, -10.26825948882913586, -17.77250458025988422 ) ) ;
#51595 = CARTESIAN_POINT ( 'NONE',  ( 5.959828726073459926, 18.96145866559661286, 7.858992891710209427 ) ) ;
#51596 = CARTESIAN_POINT ( 'NONE',  ( 1.296416391601052265, 16.25883182415322281, 40.96288273290907966 ) ) ;
#51597 = EDGE_CURVE ( 'NONE', #32701, #50567, #36421, .T. ) ;
#51598 = B_SPLINE_CURVE_WITH_KNOTS ( 'NONE', 3,
 ( #21637, #59844, #40165, #55132 ),
 .UNSPECIFIED., .F., .F.,
 ( 4, 4 ),
 ( 2.602085213965210642E-18, 0.004042984057420973693 ),
 .UNSPECIFIED. ) ;
#51599 = CARTESIAN_POINT ( 'NONE',  ( -2.708315649062910779, 7.544341609839976037, -12.54007339125007547 ) ) ;
#51600 = DIRECTION ( 'NONE',  ( 0.000000000000000000, 0.000000000000000000, 1.000000000000000000 ) ) ;
#51601 = CARTESIAN_POINT ( 'NONE',  ( 2.009741617377216460, 32.62915352493547516, -29.57773517139599306 ) ) ;
#51602 = ADVANCED_FACE ( 'NONE', ( #6233 ), #20147, .F. ) ;
#51603 = B_SPLINE_CURVE_WITH_KNOTS ( 'NONE', 3,
 ( #18984, #38101, #52457, #47786 ),
 .UNSPECIFIED., .F., .F.,
 ( 4, 4 ),
 ( 0.000000000000000000, 0.004444878191957690391 ),
 .UNSPECIFIED. ) ;
#51604 =( BOUNDED_SURFACE ( )  B_SPLINE_SURFACE ( 3, 1, ( 
 ( #52553, #1162 ),
 ( #20296, #24065 ),
 ( #48187, #24680 ),
 ( #39418, #29072 ) ),
 .UNSPECIFIED., .F., .F., .F. ) 
 B_SPLINE_SURFACE_WITH_KNOTS ( ( 4, 4 ),
 ( 2, 2 ),
 ( 0.000000000000000000, 1.000000000000000000 ),
 ( 0.000000000000000000, 1.000000000000000000 ),
 .UNSPECIFIED. ) 
 GEOMETRIC_REPRESENTATION_ITEM ( )  RATIONAL_B_SPLINE_SURFACE ( (
 ( 1.000000000000000000, 1.000000000000000000),
 ( 0.9952954269826590483, 0.8620686068821307169),
 ( 0.9952954269826590483, 0.8620686068821307169),
 ( 1.000000000000000000, 1.000000000000000000) ) ) 
 REPRESENTATION_ITEM ( '' )  SURFACE ( )  );
#51605 = ORIENTED_EDGE ( 'NONE', *, *, #4023, .F. ) ;
#51606 = CARTESIAN_POINT ( 'NONE',  ( 0.9754402186311945666, 10.92425836141477014, -41.49454543482920599 ) ) ;
#51607 = ADVANCED_FACE ( 'NONE', ( #20080 ), #52392, .T. ) ;
#51608 = EDGE_CURVE ( 'NONE', #58555, #24987, #44804, .T. ) ;
#51609 = CARTESIAN_POINT ( 'NONE',  ( 0.1129192098497455998, -42.55567333040708888, -11.66046547873770756 ) ) ;
#51610 = LINE ( 'NONE', #50998, #19551 ) ;
#51611 = CARTESIAN_POINT ( 'NONE',  ( 0.5804410086790514622, -25.69437916690352353, -39.23415261073942162 ) ) ;
#51612 = EDGE_CURVE ( 'NONE', #26084, #20677, #15603, .T. ) ;
#51613 = ORIENTED_EDGE ( 'NONE', *, *, #58726, .F. ) ;
#51614 = DIRECTION ( 'NONE',  ( -0.1736481776669312471, 0.9848077530122077983, -5.551115123125779621E-17 ) ) ;
#51615 = B_SPLINE_CURVE_WITH_KNOTS ( 'NONE', 3,
 ( #25281, #16826, #49392, #6446 ),
 .UNSPECIFIED., .F., .F.,
 ( 4, 4 ),
 ( 9.868122050982122734E-17, 0.005004741218457526425 ),
 .UNSPECIFIED. ) ;
#51616 = B_SPLINE_CURVE_WITH_KNOTS ( 'NONE', 3,
 ( #37714, #37396, #42113, #13903 ),
 .UNSPECIFIED., .F., .F.,
 ( 4, 4 ),
 ( 0.000000000000000000, 0.004447772540403824131 ),
 .UNSPECIFIED. ) ;
#51617 = CARTESIAN_POINT ( 'NONE',  ( 1.399999999999999023, 9.062386313690441984E-16, 7.400000000000022560 ) ) ;
#51618 = ORIENTED_EDGE ( 'NONE', *, *, #24500, .F. ) ;
#51619 = EDGE_CURVE ( 'NONE', #55695, #49511, #59814, .T. ) ;
#51620 = CARTESIAN_POINT ( 'NONE',  ( 0.5980271706414734822, 17.61704905854934822, 45.84417984117861522 ) ) ;
#51621 = VERTEX_POINT ( 'NONE', #41656 ) ;
#51622 = CARTESIAN_POINT ( 'NONE',  ( 0.8753041380234471980, -29.91468680897799004, -38.93905290314260270 ) ) ;
#51623 = CARTESIAN_POINT ( 'NONE',  ( 1.827326673878743923, -43.03225468313002011, -1.232746109312025329 ) ) ;
#51624 = AXIS2_PLACEMENT_3D ( 'NONE', #27070, #17069, #8566 ) ;
#51625 = EDGE_LOOP ( 'NONE', ( #61805, #41473, #42715, #3695 ) ) ;
#51626 = CIRCLE ( 'NONE', #42672, 12.55882000000000076 ) ;
#51627 = CARTESIAN_POINT ( 'NONE',  ( 5.901764892641288895, 42.64666365787720537, -24.06768676652523808 ) ) ;
#51628 = CARTESIAN_POINT ( 'NONE',  ( 0.1102847568649952675, 26.32556309315071275, 34.15672344772096380 ) ) ;
#51629 = ORIENTED_EDGE ( 'NONE', *, *, #36793, .T. ) ;
#51630 = CARTESIAN_POINT ( 'NONE',  ( 0.9745511491811742477, 21.15859207114749196, 37.32887948083607910 ) ) ;
#51631 = DIRECTION ( 'NONE',  ( 0.000000000000000000, 1.224646799147361835E-16, 1.000000000000000000 ) ) ;
#51632 = ORIENTED_EDGE ( 'NONE', *, *, #333, .F. ) ;
#51633 = CARTESIAN_POINT ( 'NONE',  ( 0.8557997880470690211, -34.51495345639526136, -33.22501220301936797 ) ) ;
#51634 = ORIENTED_EDGE ( 'NONE', *, *, #17354, .T. ) ;
#51635 = DIRECTION ( 'NONE',  ( -0.1011922191286467460, -0.8906890386588581787, -0.4432078194264840176 ) ) ;
#51636 = ORIENTED_EDGE ( 'NONE', *, *, #10329, .T. ) ;
#51637 = ORIENTED_EDGE ( 'NONE', *, *, #45096, .F. ) ;
#51638 = CARTESIAN_POINT ( 'NONE',  ( 0.1129192098497455998, 25.64022107388826655, -35.91003830501005467 ) ) ;
#51640 = CONICAL_SURFACE ( 'NONE', #19694, 42.08604991992415023, 1.569615340895231137 ) ;
#51639 = CARTESIAN_POINT ( 'NONE',  ( 2.281448460670565836, 46.66132715497963090, 11.14236343022389164 ) ) ;
#51641 = CARTESIAN_POINT ( 'NONE',  ( 0.5809828226811548646, 29.58751527316178809, 37.66417181417562432 ) ) ;
#51642 = DIRECTION ( 'NONE',  ( -1.000000000000000000, -0.000000000000000000, -0.000000000000000000 ) ) ;
#51643 = CARTESIAN_POINT ( 'NONE',  ( 0.8551540677456715978, -37.45266983663474747, -29.88829867897853632 ) ) ;
#51644 = EDGE_LOOP ( 'NONE', ( #9464, #12222, #45159, #32370 ) ) ;
#51645 = CARTESIAN_POINT ( 'NONE',  ( 0.9757787079277443487, 11.06737752163097355, 41.45659305953925866 ) ) ;
#51646 = FACE_OUTER_BOUND ( 'NONE', #7092, .T. ) ;
#51647 = B_SPLINE_CURVE_WITH_KNOTS ( 'NONE', 3,
 ( #60532, #32991, #37379, #46470, #56759, #37081, #3516, #61448, #32674, #13885, #52065, #18570, #23567, #42393, #17643, #22651, #41783, #37695, #8225 ),
 .UNSPECIFIED., .F., .F.,
 ( 4, 3, 3, 3, 3, 3, 4 ),
 ( 3.469446951953614189E-18, 0.0002724573126191831823, 0.0004086839781548642523, 0.0005449106435901963398, 0.0006811373090491628420, 0.0008459866663933848785, 0.001010840725717215751 ),
 .UNSPECIFIED. ) ;
#51648 = CARTESIAN_POINT ( 'NONE',  ( 2.394385881922565851, 0.1126610846915976627, 44.02256615367562631 ) ) ;
#51650 = ORIENTED_EDGE ( 'NONE', *, *, #39532, .F. ) ;
#51649 = EDGE_CURVE ( 'NONE', #34790, #9403, #374, .T. ) ;
#51651 = ORIENTED_EDGE ( 'NONE', *, *, #28444, .F. ) ;
#51652 = CARTESIAN_POINT ( 'NONE',  ( 0.5987334363312686314, -49.10393658271619444, -0.6052425568828397884 ) ) ;
#51654 = EDGE_CURVE ( 'NONE', #23158, #21513, #55181, .T. ) ;
#51653 = CARTESIAN_POINT ( 'NONE',  ( -5.720000000000000639, 3.469446951953614189E-15, 0.000000000000000000 ) ) ;
#51655 = CARTESIAN_POINT ( 'NONE',  ( 5.974727161628367256, -5.297264154381075230, 19.82959049719566380 ) ) ;
#51656 = CARTESIAN_POINT ( 'NONE',  ( 0.7245667037590743931, -34.58857005974929422, -33.42814706018009474 ) ) ;
#51657 = CARTESIAN_POINT ( 'NONE',  ( 2.359973842542475886, -34.35832655684843218, 27.52528457337841772 ) ) ;
#51658 = ORIENTED_EDGE ( 'NONE', *, *, #14789, .F. ) ;
#51659 = CARTESIAN_POINT ( 'NONE',  ( 0.5809828226811544205, 47.55412398569205834, 5.711058609465488267 ) ) ;
#51660 = PRODUCT_DEFINITION ( 'UNKNOWN', '', #38942, #16042 ) ;
#51661 = CARTESIAN_POINT ( 'NONE',  ( -6.015611763856276717, -11.46610900684713030, -14.95313250337441424 ) ) ;
#51662 = CARTESIAN_POINT ( 'NONE',  ( 3.894904216938897434, 42.66483338720180996, -10.57526947734715783 ) ) ;
#51663 = CARTESIAN_POINT ( 'NONE',  ( -2.739355103387248747, -0.2155581815329185580, 14.92652342715446956 ) ) ;
#51664 = CARTESIAN_POINT ( 'NONE',  ( 3.514385190458181096, -13.03453477240704039, -1.199999999999999956 ) ) ;
#51665 =( NAMED_UNIT ( * ) SI_UNIT ( $, .STERADIAN. ) SOLID_ANGLE_UNIT ( ) );
#51666 = CARTESIAN_POINT ( 'NONE',  ( 0.1073791018717578927, -30.14884492832369745, -30.83464511437127697 ) ) ;
#51667 = EDGE_LOOP ( 'NONE', ( #3924, #39440, #40965, #56519 ) ) ;
#51668 = CARTESIAN_POINT ( 'NONE',  ( 0.3622758884714600280, 34.70015533914828865, -25.58609868863731407 ) ) ;
#51669 = FACE_OUTER_BOUND ( 'NONE', #59346, .T. ) ;
#51670 = CIRCLE ( 'NONE', #41732, 47.91270532121795611 ) ;
#51671 = CARTESIAN_POINT ( 'NONE',  ( 3.376099380956838925, -12.16518930220327555, 5.631745100199947451 ) ) ;
#51672 = DIRECTION ( 'NONE',  ( -1.836909530733573776E-16, 1.000000000000000000, 0.000000000000000000 ) ) ;
#51673 = AXIS2_PLACEMENT_3D ( 'NONE', #30087, #49199, #34501 ) ;
#51674 = CARTESIAN_POINT ( 'NONE',  ( 5.959547316686252039, -7.851524054666535690, 18.96456592444086908 ) ) ;
#51675 = CARTESIAN_POINT ( 'NONE',  ( 0.5836750258453350382, 6.431686642655440878, -47.46217286060748108 ) ) ;
#51676 = CARTESIAN_POINT ( 'NONE',  ( 4.553261556744873317, 1.633632119646958980, 43.89613664004264848 ) ) ;
#51677 = CARTESIAN_POINT ( 'NONE',  ( 0.5835226383429301666, 22.37749966153948478, -41.21274054759963690 ) ) ;
#51678 = EDGE_CURVE ( 'NONE', #30264, #22007, #11929, .T. ) ;
#51679 =( BOUNDED_SURFACE ( )  B_SPLINE_SURFACE ( 3, 1, ( 
 ( #27050, #21732 ),
 ( #46175, #35538 ),
 ( #59936, #36159 ),
 ( #22047, #16731 ) ),
 .UNSPECIFIED., .F., .F., .F. ) 
 B_SPLINE_SURFACE_WITH_KNOTS ( ( 4, 4 ),
 ( 2, 2 ),
 ( 0.000000000000000000, 1.000000000000000000 ),
 ( 0.000000000000000000, 1.000000000000000000 ),
 .UNSPECIFIED. ) 
 GEOMETRIC_REPRESENTATION_ITEM ( )  RATIONAL_B_SPLINE_SURFACE ( (
 ( 1.000000000000000000, 1.000000000000000000),
 ( 0.9754377213608244057, 0.9999580625633939235),
 ( 0.9754377213608244057, 0.9999580625633939235),
 ( 1.000000000000000000, 1.000000000000000000) ) ) 
 REPRESENTATION_ITEM ( '' )  SURFACE ( )  );
#51680 = EDGE_CURVE ( 'NONE', #13139, #31407, #49454, .T. ) ;
#51681 = CARTESIAN_POINT ( 'NONE',  ( 5.910764540655178756, -13.99299321836462440, -14.44636214622783577 ) ) ;
#51682 = CONICAL_SURFACE ( 'NONE', #12678, 42.92674063221959813, 1.485477209440487556 ) ;
#51683 = ORIENTED_EDGE ( 'NONE', *, *, #52028, .T. ) ;
#51684 = EDGE_CURVE ( 'NONE', #52291, #52483, #21608, .T. ) ;
#51685 = CARTESIAN_POINT ( 'NONE',  ( 4.956653778116982600, -43.37017594958069111, 20.77844580450546985 ) ) ;
#51686 = CARTESIAN_POINT ( 'NONE',  ( 0.3676999524040323597, 44.06746933160595603, -2.002181318164867552 ) ) ;
#51687 = CARTESIAN_POINT ( 'NONE',  ( 0.9762797500689124330, 40.28286501695585997, -11.55922018180369548 ) ) ;
#51688 = FACE_OUTER_BOUND ( 'NONE', #20370, .T. ) ;
#51689 = EDGE_CURVE ( 'NONE', #55623, #11621, #31624, .T. ) ;
#51690 = ORIENTED_EDGE ( 'NONE', *, *, #12575, .F. ) ;
#51691 = FACE_OUTER_BOUND ( 'NONE', #19703, .T. ) ;
#51692 = CARTESIAN_POINT ( 'NONE',  ( 0.9780303403264775097, -41.83550024410291712, -2.475991260233099123 ) ) ;
#51693 = AXIS2_PLACEMENT_3D ( 'NONE', #4648, #52909, #10013 ) ;
#51694 = SURFACE_STYLE_FILL_AREA ( #22591 ) ;
#51695 = B_SPLINE_CURVE_WITH_KNOTS ( 'NONE', 3,
 ( #54868, #13218, #41432, #22612, #27613, #59887 ),
 .UNSPECIFIED., .F., .F.,
 ( 4, 2, 4 ),
 ( 1.275615807185303638E-16, 0.0002450741128632385221, 0.0004901482257263495420 ),
 .UNSPECIFIED. ) ;
#51696 = ORIENTED_EDGE ( 'NONE', *, *, #24546, .F. ) ;
#51697 = CARTESIAN_POINT ( 'NONE',  ( 3.238018933889920792, 9.507325605900218690, 9.434948446655496923 ) ) ;
#51698 = CARTESIAN_POINT ( 'NONE',  ( 9.999999999999994671, 56.56854249492450037, -56.56854249492312192 ) ) ;
#51699 = CARTESIAN_POINT ( 'NONE',  ( 3.782542959838389951, 26.30383675830739421, -32.79246903160672133 ) ) ;
#51700 = VERTEX_POINT ( 'NONE', #12848 ) ;
#51701 = CARTESIAN_POINT ( 'NONE',  ( 0.6029303876144825880, 29.18200390283997336, 38.24575311130009680 ) ) ;
#51702 = ORIENTED_EDGE ( 'NONE', *, *, #15287, .F. ) ;
#51703 = ORIENTED_EDGE ( 'NONE', *, *, #22474, .T. ) ;
#51704 = CARTESIAN_POINT ( 'NONE',  ( 4.335381028904201628, 24.52155563981625974, -42.40813785899753441 ) ) ;
#51705 = DIRECTION ( 'NONE',  ( 0.000000000000000000, 0.000000000000000000, -1.000000000000000000 ) ) ;
#51706 = VERTEX_POINT ( 'NONE', #31313 ) ;
#51707 = CARTESIAN_POINT ( 'NONE',  ( 1.231276596079887264, 24.17959027891153667, -34.24360064248551083 ) ) ;
#51708 = VERTEX_POINT ( 'NONE', #50416 ) ;
#51709 = DIRECTION ( 'NONE',  ( -1.000000000000000000, -0.000000000000000000, -0.000000000000000000 ) ) ;
#51710 = CARTESIAN_POINT ( 'NONE',  ( -6.078726893082806448, -1.845620846545631188, 19.16736092839899186 ) ) ;
#51711 = CARTESIAN_POINT ( 'NONE',  ( 4.975801465491694664, 47.84403947906843513, -2.564218696446985302 ) ) ;
#51712 = AXIS2_PLACEMENT_3D ( 'NONE', #40133, #29447, #59180 ) ;
#51713 = ORIENTED_EDGE ( 'NONE', *, *, #4216, .F. ) ;
#51714 = CARTESIAN_POINT ( 'NONE',  ( 4.975610109902397937, -46.23629923292386934, 15.95788333023201488 ) ) ;
#51715 = FACE_OUTER_BOUND ( 'NONE', #27945, .T. ) ;
#51716 = CARTESIAN_POINT ( 'NONE',  ( 4.975801465491695552, -31.15993731089151808, 36.39623109580413285 ) ) ;
#51717 = AXIS2_PLACEMENT_3D ( 'NONE', #23855, #28238, #42988 ) ;
#51718 = CARTESIAN_POINT ( 'NONE',  ( 0.8744876279028263033, 17.78802839418742110, -45.75954650373051891 ) ) ;
#51719 = VERTEX_POINT ( 'NONE', #36969 ) ;
#51720 = CARTESIAN_POINT ( 'NONE',  ( 5.272379999999998290, 0.000000000000000000, 0.000000000000000000 ) ) ;
#51721 = DIRECTION ( 'NONE',  ( 0.000000000000000000, 0.000000000000000000, 1.000000000000000000 ) ) ;
#51722 = ORIENTED_EDGE ( 'NONE', *, *, #53900, .F. ) ;
#51723 = CARTESIAN_POINT ( 'NONE',  ( 2.624215991343620935, -30.33228621715010576, -37.21129343241634047 ) ) ;
#51724 = ORIENTED_EDGE ( 'NONE', *, *, #61584, .T. ) ;
#51725 = CARTESIAN_POINT ( 'NONE',  ( 5.910764540655177868, 12.99683459030034349, -15.34873053713353563 ) ) ;
#51726 = EDGE_CURVE ( 'NONE', #1315, #19675, #13151, .T. ) ;
#51727 = CARTESIAN_POINT ( 'NONE',  ( 0.5806925824938511393, 10.33919002968708689, -45.74192291403568333 ) ) ;
#51728 = ORIENTED_EDGE ( 'NONE', *, *, #30537, .T. ) ;
#51729 = CARTESIAN_POINT ( 'NONE',  ( 0.9790320750461898314, -34.50252855204712432, -23.78891876604240707 ) ) ;
#51730 = CARTESIAN_POINT ( 'NONE',  ( -6.072942160501519027, 7.807899065004683337, -17.60229742049939006 ) ) ;
#51731 = CARTESIAN_POINT ( 'NONE',  ( 0.9730545539215883499, -41.31259007387239279, 11.59290486963492128 ) ) ;
#51732 = CARTESIAN_POINT ( 'NONE',  ( 0.8744876279028263033, -2.462621419133342204, 49.03351451941333750 ) ) ;
#51733 = ORIENTED_EDGE ( 'NONE', *, *, #49421, .F. ) ;
#51734 = CARTESIAN_POINT ( 'NONE',  ( 0.1139756605157203201, -40.74870632435499118, 16.92625630747966525 ) ) ;
#51735 = CARTESIAN_POINT ( 'NONE',  ( 5.959828726073459926, 17.77796293532173166, -10.25888482581841110 ) ) ;
#51736 = CARTESIAN_POINT ( 'NONE',  ( 0.9762797500689124330, 35.79768877047958853, 21.79105926469807741 ) ) ;
#51737 = CARTESIAN_POINT ( 'NONE',  ( 0.5819845079324660331, -44.42187385013350820, -17.90867223323933288 ) ) ;
#51738 = B_SPLINE_CURVE_WITH_KNOTS ( 'NONE', 3,
 ( #19484, #5346, #338, #58905 ),
 .UNSPECIFIED., .F., .F.,
 ( 4, 4 ),
 ( 0.000000000000000000, 0.004445488388166992516 ),
 .UNSPECIFIED. ) ;
#51739 = DIRECTION ( 'NONE',  ( 0.07906939808003034253, 0.9390317839750903506, 0.3346152103115173637 ) ) ;
#51740 = CARTESIAN_POINT ( 'NONE',  ( 2.282803330402963127, -26.37305679751943188, 38.87105327376399799 ) ) ;
#51741 = CARTESIAN_POINT ( 'NONE',  ( 0.7242003506639982380, 46.85218299671425513, 14.69301271245709195 ) ) ;
#51742 = CARTESIAN_POINT ( 'NONE',  ( 0.9787464366903569912, -12.58548318642580455, 39.97423677638705186 ) ) ;
#51743 = CARTESIAN_POINT ( 'NONE',  ( 0.6846871229502899947, -46.04462816497497357, 13.23224427737813258 ) ) ;
#51744 = DIRECTION ( 'NONE',  ( 0.09835009131224567436, -0.5042575517176746125, 0.8579344853044256203 ) ) ;
#51745 = CARTESIAN_POINT ( 'NONE',  ( 0.7764139734771229318, 33.24270203466717533, -33.09022865350438281 ) ) ;
#51746 = CARTESIAN_POINT ( 'NONE',  ( 4.967162193818130511, 28.07411493385295032, 32.68434214048178177 ) ) ;
#51747 = CARTESIAN_POINT ( 'NONE',  ( 4.962356264823608143, -40.70360067759239087, 10.69824704058788711 ) ) ;
#51748 = CARTESIAN_POINT ( 'NONE',  ( 0.2940133293162997541, -31.12576116254606973, -31.26383760241506593 ) ) ;
#51749 = EDGE_CURVE ( 'NONE', #929, #37705, #8118, .T. ) ;
#51750 = CARTESIAN_POINT ( 'NONE',  ( 5.959828726073459926, -14.51059719297107087, -14.51699876360195240 ) ) ;
#51751 = ADVANCED_FACE ( 'NONE', ( #51330 ), #45741, .T. ) ;
#51752 = AXIS2_PLACEMENT_3D ( 'NONE', #48038, #38345, #19848 ) ;
#51754 =( BOUNDED_SURFACE ( )  B_SPLINE_SURFACE ( 3, 1, ( 
 ( #33710, #4851 ),
 ( #57160, #61557 ),
 ( #10504, #9889 ),
 ( #37809, #52787 ) ),
 .UNSPECIFIED., .F., .F., .F. ) 
 B_SPLINE_SURFACE_WITH_KNOTS ( ( 4, 4 ),
 ( 2, 2 ),
 ( 0.000000000000000000, 1.000000000000000000 ),
 ( 0.000000000000000000, 1.000000000000000000 ),
 .UNSPECIFIED. ) 
 GEOMETRIC_REPRESENTATION_ITEM ( )  RATIONAL_B_SPLINE_SURFACE ( (
 ( 1.000000000000000000, 1.000000000000000000),
 ( 0.7211978278499970862, 0.9934217856018976445),
 ( 0.7211978278499970862, 0.9934217856018976445),
 ( 1.000000000000000000, 1.000000000000000000) ) ) 
 REPRESENTATION_ITEM ( '' )  SURFACE ( )  );
#51753 =( NAMED_UNIT ( * ) PLANE_ANGLE_UNIT ( ) SI_UNIT ( $, .RADIAN. ) );
#51755 = CARTESIAN_POINT ( 'NONE',  ( 4.960386119450151732, -9.684723978931470967, -42.66898857629802677 ) ) ;
#51757 = ORIENTED_EDGE ( 'NONE', *, *, #17684, .F. ) ;
#51756 = CARTESIAN_POINT ( 'NONE',  ( 4.553261556744875094, -36.69060082144763868, -24.15241969627107110 ) ) ;
#51758 = DIRECTION ( 'NONE',  ( -1.000000000000000000, -0.000000000000000000, -0.000000000000000000 ) ) ;
#51759 = CARTESIAN_POINT ( 'NONE',  ( -6.015611763856276717, 18.20278301740943405, -4.870987357967985432 ) ) ;
#51760 = VECTOR ( 'NONE', #5613, 1000.000000000000000 ) ;
#51761 = CARTESIAN_POINT ( 'NONE',  ( 50.15577769773999961, 9.539392014169456147, -3.000000000000000000 ) ) ;
#51762 = ADVANCED_FACE ( 'NONE', ( #22841 ), #56896, .F. ) ;
#51763 = ORIENTED_EDGE ( 'NONE', *, *, #32073, .F. ) ;
#51764 = ORIENTED_EDGE ( 'NONE', *, *, #505, .T. ) ;
#51765 = CARTESIAN_POINT ( 'NONE',  ( 4.967162193818130511, 24.30453456948160351, -35.57684288741949530 ) ) ;
#51766 = CARTESIAN_POINT ( 'NONE',  ( 0.1129192098497455998, 43.21532672376827833, 8.909956450124401073 ) ) ;
#51767 = ORIENTED_EDGE ( 'NONE', *, *, #49394, .T. ) ;
#51768 = EDGE_LOOP ( 'NONE', ( #51767, #41493, #24535, #16365 ) ) ;
#51769 = DIRECTION ( 'NONE',  ( -1.000000000000000000, -1.836909530733573776E-16, 0.000000000000000000 ) ) ;
#51770 = ADVANCED_FACE ( 'NONE', ( #50713 ), #45778, .F. ) ;
#51771 = CARTESIAN_POINT ( 'NONE',  ( 50.15577769773999961, 0.000000000000000000, 0.000000000000000000 ) ) ;
#51772 = CARTESIAN_POINT ( 'NONE',  ( 0.9747592971366241255, -41.36145845824417933, 11.41797089479118910 ) ) ;
#51773 = ORIENTED_EDGE ( 'NONE', *, *, #41099, .F. ) ;
#51774 = VERTEX_POINT ( 'NONE', #47892 ) ;
#51775 = CARTESIAN_POINT ( 'NONE',  ( 7.000000000000006217, 1.285836671513502038E-15, -1.348150961071066192E-31 ) ) ;
#51777 = ORIENTED_EDGE ( 'NONE', *, *, #27156, .F. ) ;
#51776 = ADVANCED_FACE ( 'NONE', ( #23155 ), #52142, .F. ) ;
#51778 = CARTESIAN_POINT ( 'NONE',  ( 0.2230388203127611768, 15.79641846944918449, -40.12182516270784305 ) ) ;
#51779 = CARTESIAN_POINT ( 'NONE',  ( 4.553261556744875094, 17.57396821678876364, 40.25785894628445760 ) ) ;
#51780 = CIRCLE ( 'NONE', #26796, 48.91267123290010943 ) ;
#51781 = CARTESIAN_POINT ( 'NONE',  ( 0.1102144999581333162, -30.40435207217207747, -30.58258619461911110 ) ) ;
#51782 = ORIENTED_EDGE ( 'NONE', *, *, #41339, .F. ) ;
#51783 = DIRECTION ( 'NONE',  ( 0.000000000000000000, 0.000000000000000000, 1.000000000000000000 ) ) ;
#51784 = ORIENTED_EDGE ( 'NONE', *, *, #2755, .T. ) ;
#51785 = VECTOR ( 'NONE', #45622, 1000.000000000000000 ) ;
#51786 = VERTEX_POINT ( 'NONE', #37579 ) ;
#51787 = B_SPLINE_CURVE_WITH_KNOTS ( 'NONE', 3,
 ( #61200, #46830, #50568, #18315, #17080, #13304 ),
 .UNSPECIFIED., .F., .F.,
 ( 4, 2, 4 ),
 ( 0.000000000000000000, 0.0002291459268755674972, 0.0004582918537511349944 ),
 .UNSPECIFIED. ) ;
#51788 = CARTESIAN_POINT ( 'NONE',  ( -6.078726893082806448, -16.14009859332537999, -10.50196451462564262 ) ) ;
#51789 = ORIENTED_EDGE ( 'NONE', *, *, #16715, .T. ) ;
#51790 = CARTESIAN_POINT ( 'NONE',  ( -6.010958268070873523, 17.40352239307067705, -7.224487401384108942 ) ) ;
#51791 = CARTESIAN_POINT ( 'NONE',  ( -6.017396004339686577, -13.32329839588564369, 13.32495836419619728 ) ) ;
#51792 = CARTESIAN_POINT ( 'NONE',  ( 3.407937589446174087, 6.447869442558164188, 12.08659953757610950 ) ) ;
#51793 = CARTESIAN_POINT ( 'NONE',  ( 0.5837799406558233928, -38.61146441179320732, 26.61575408576708313 ) ) ;
#51794 = CARTESIAN_POINT ( 'NONE',  ( 1.657374760986086271, -43.83488152824200057, -4.403817509528764162 ) ) ;
#51795 = ORIENTED_EDGE ( 'NONE', *, *, #36514, .F. ) ;
#51796 = CARTESIAN_POINT ( 'NONE',  ( 0.9736507210033050752, -30.02062799605179677, -30.65767007549946399 ) ) ;
#51797 = CARTESIAN_POINT ( 'NONE',  ( -6.063463321072276813, -1.833563764454537504, 19.16920698414906354 ) ) ;
#51798 = CARTESIAN_POINT ( 'NONE',  ( 0.9741495583595158880, -21.11077839432110892, -37.35596046161889205 ) ) ;
#51799 = EDGE_CURVE ( 'NONE', #6542, #25300, #58172, .T. ) ;
#51800 = ORIENTED_EDGE ( 'NONE', *, *, #37865, .F. ) ;
#51801 = CARTESIAN_POINT ( 'NONE',  ( 0.5997462898726536595, 41.43917033312096265, 26.35046094941977302 ) ) ;
#51802 = CARTESIAN_POINT ( 'NONE',  ( 5.894904586330512508, 3.344157678208643514, -19.83295291894076229 ) ) ;
#51803 = CARTESIAN_POINT ( 'NONE',  ( 4.390527457369401532, -4.537883182548267058, 43.69888960660402688 ) ) ;
#51804 = CIRCLE ( 'NONE', #5769, 2.500000000000000888 ) ;
#51805 = ORIENTED_EDGE ( 'NONE', *, *, #48384, .F. ) ;
#51806 = ORIENTED_EDGE ( 'NONE', *, *, #6537, .T. ) ;
#51807 = CARTESIAN_POINT ( 'NONE',  ( 3.783198216974386963, 18.05208553945200123, -39.06945274417374492 ) ) ;
#51808 = CARTESIAN_POINT ( 'NONE',  ( 0.5980894510889448457, -48.10766805928368939, -0.7015180096003186261 ) ) ;
#51809 = CARTESIAN_POINT ( 'NONE',  ( 0.5804410086790514622, 22.05813747677437320, 41.38790189066267544 ) ) ;
#51810 = CARTESIAN_POINT ( 'NONE',  ( 0.6008123274975392114, 32.69143758430389113, 36.64456930883510921 ) ) ;
#51811 = CARTESIAN_POINT ( 'NONE',  ( 0.5806925824938502512, -30.69245420804159252, -35.45695442407362208 ) ) ;
#51812 = CARTESIAN_POINT ( 'NONE',  ( 0.1158403557922069033, -17.82608841671577693, -40.36298897434691213 ) ) ;
#51813 = CARTESIAN_POINT ( 'NONE',  ( 0.1313383488274136313, 42.66669366003522867, -6.260443365526930037 ) ) ;
#51814 = CARTESIAN_POINT ( 'NONE',  ( 0.1073791018717578927, 42.81622261970994003, -5.147744207006430983 ) ) ;
#51815 = CARTESIAN_POINT ( 'NONE',  ( 4.956653778116975495, -36.51451553856441024, 31.29546495791839078 ) ) ;
#51816 = CARTESIAN_POINT ( 'NONE',  ( -5.995132425357893702, 2.468096378288389570, -18.68182899165008592 ) ) ;
#51817 = CARTESIAN_POINT ( 'NONE',  ( 0.6064782688330845328, 11.56181350407003983, -45.44952051359700107 ) ) ;
#51818 = ORIENTED_EDGE ( 'NONE', *, *, #31443, .T. ) ;
#51819 = TOROIDAL_SURFACE ( 'NONE', #12820, 5.633200000000004870, 0.02570000000000859444 ) ;
#51820 = DIRECTION ( 'NONE',  ( 1.000000000000000000, 1.558861125776144859E-16, -3.851859888774471706E-32 ) ) ;
#51821 = CARTESIAN_POINT ( 'NONE',  ( 0.6254311100348661778, -33.52633430496203459, -34.49956326955403796 ) ) ;
#51822 = CARTESIAN_POINT ( 'NONE',  ( 1.834102595619085285, -23.93815899361085187, -36.97515772588796779 ) ) ;
#51823 = CARTESIAN_POINT ( 'NONE',  ( 0.6001305935487315502, 44.24520387813801392, 18.89378601236080257 ) ) ;
#51824 = ITEM_DEFINED_TRANSFORMATION ( 'NONE', 'NONE', #34912,  #14677 ) ;
#51825 = CARTESIAN_POINT ( 'NONE',  ( -6.010958268070873523, 18.84344976839986785, -0.01451635840169805507 ) ) ;
#51826 = CARTESIAN_POINT ( 'NONE',  ( 0.5827357941260222773, 12.74691551863630679, 46.16863402900283120 ) ) ;
#51827 = B_SPLINE_CURVE_WITH_KNOTS ( 'NONE', 3,
 ( #54329, #44991, #54029, #2338, #26159, #2027 ),
 .UNSPECIFIED., .F., .F.,
 ( 4, 2, 4 ),
 ( 8.440430351524944310E-17, 0.0002293366620881450118, 0.0004586733241762056185 ),
 .UNSPECIFIED. ) ;
#51828 = EDGE_CURVE ( 'NONE', #20580, #3844, #4620, .T. ) ;
#51829 = AXIS2_PLACEMENT_3D ( 'NONE', #54031, #49046, #19634 ) ;
#51830 = DIRECTION ( 'NONE',  ( 0.000000000000000000, 0.000000000000000000, 1.000000000000000000 ) ) ;
#51832 = EDGE_LOOP ( 'NONE', ( #36103, #47189, #40334, #34918 ) ) ;
#51831 = CARTESIAN_POINT ( 'NONE',  ( 0.1119898979215348117, -35.69472108585459580, -25.93931754797872813 ) ) ;
#51833 = ORIENTED_EDGE ( 'NONE', *, *, #35542, .T. ) ;
#51834 = B_SPLINE_CURVE_WITH_KNOTS ( 'NONE', 3,
 ( #2397, #16837, #35954, #59409, #17143, #50325 ),
 .UNSPECIFIED., .F., .F.,
 ( 4, 2, 4 ),
 ( 8.673617379884035472E-19, 0.0002291966416970794309, 0.0004583932833941579943 ),
 .UNSPECIFIED. ) ;
#51835 = CARTESIAN_POINT ( 'NONE',  ( 5.896782393890504181, 5.952874097602693482, -19.21169895808549200 ) ) ;
#51836 = CARTESIAN_POINT ( 'NONE',  ( 0.6067375320500705271, 17.67235760802263655, 44.51755737952358771 ) ) ;
#51837 = EDGE_CURVE ( 'NONE', #27695, #37089, #41803, .T. ) ;
#51838 = ORIENTED_EDGE ( 'NONE', *, *, #40946, .F. ) ;
#51839 = CARTESIAN_POINT ( 'NONE',  ( 2.648799415243696664, 48.37728179772450687, -8.009748382636628250 ) ) ;
#51840 = DIRECTION ( 'NONE',  ( -1.000000000000000000, -0.000000000000000000, -0.000000000000000000 ) ) ;
#51841 = CARTESIAN_POINT ( 'NONE',  ( 0.6009452777970410997, -44.61081509289892466, -18.00606236585358033 ) ) ;
#51842 = B_SPLINE_CURVE_WITH_KNOTS ( 'NONE', 3,
 ( #6343, #24881, #15182, #25480 ),
 .UNSPECIFIED., .F., .F.,
 ( 4, 4 ),
 ( 2.323236804244109875E-17, 0.004564976165746189446 ),
 .UNSPECIFIED. ) ;
#51843 = EDGE_CURVE ( 'NONE', #6162, #35188, #49204, .T. ) ;
#51844 = VERTEX_POINT ( 'NONE', #9985 ) ;
#51845 = ORIENTED_EDGE ( 'NONE', *, *, #37704, .T. ) ;
#51846 = CARTESIAN_POINT ( 'NONE',  ( 0.9747592971366237924, 41.52905920980983012, 10.79247637456133369 ) ) ;
#51847 = VECTOR ( 'NONE', #25363, 1000.000000000000114 ) ;
#51848 = AXIS2_PLACEMENT_3D ( 'NONE', #30869, #21170, #45309 ) ;
#51849 = CARTESIAN_POINT ( 'NONE',  ( 0.7948878604505670298, -20.66454813869003360, -44.53846761533425536 ) ) ;
#51850 = DIRECTION ( 'NONE',  ( -1.000000000000000000, -0.000000000000000000, -0.000000000000000000 ) ) ;
#51851 = CARTESIAN_POINT ( 'NONE',  ( 0.9783242366443551941, 33.05536268497406382, -25.76193874636278380 ) ) ;
#51852 = EDGE_CURVE ( 'NONE', #46940, #31990, #9587, .T. ) ;
#51853 = CARTESIAN_POINT ( 'NONE',  ( 0.8751705887134553219, -17.57879340691572878, 44.76769609654206050 ) ) ;
#51854 = B_SPLINE_CURVE_WITH_KNOTS ( 'NONE', 3,
 ( #14381, #37578, #61041, #60723 ),
 .UNSPECIFIED., .F., .F.,
 ( 4, 4 ),
 ( 0.000000000000000000, 0.005004948556313805301 ),
 .UNSPECIFIED. ) ;
#51855 = CARTESIAN_POINT ( 'NONE',  ( 4.956445790443988031, 0.000000000000000000, 0.000000000000000000 ) ) ;
#51856 =( BOUNDED_SURFACE ( )  B_SPLINE_SURFACE ( 3, 1, ( 
 ( #57055, #38302 ),
 ( #46775, #14181 ),
 ( #33589, #52667 ),
 ( #5649, #34512 ) ),
 .UNSPECIFIED., .F., .F., .F. ) 
 B_SPLINE_SURFACE_WITH_KNOTS ( ( 4, 4 ),
 ( 2, 2 ),
 ( 0.000000000000000000, 1.000000000000000000 ),
 ( 0.000000000000000000, 1.000000000000000000 ),
 .UNSPECIFIED. ) 
 GEOMETRIC_REPRESENTATION_ITEM ( )  RATIONAL_B_SPLINE_SURFACE ( (
 ( 1.000000000000000000, 1.000000000000000000),
 ( 0.7269869731126821222, 0.9931720237060910339),
 ( 0.7269869731126821222, 0.9931720237060910339),
 ( 1.000000000000000000, 1.000000000000000000) ) ) 
 REPRESENTATION_ITEM ( '' )  SURFACE ( )  );
#51857 = B_SPLINE_CURVE_WITH_KNOTS ( 'NONE', 3,
 ( #23405, #52202, #61594, #18714, #19645, #42843, #37847, #9933, #24022, #33130 ),
 .UNSPECIFIED., .F., .F.,
 ( 4, 3, 3, 4 ),
 ( 1.095097866269904594E-17, 0.0002724568934985559807, 0.0004086836638483803638, 0.0005448802484329447627 ),
 .UNSPECIFIED. ) ;
#51858 = CARTESIAN_POINT ( 'NONE',  ( 0.5980271706414711508, 17.61704905855000547, -45.84417984117837364 ) ) ;
#51859 = ORIENTED_EDGE ( 'NONE', *, *, #17688, .F. ) ;
#51860 = FILL_AREA_STYLE_COLOUR ( '', #9556 ) ;
#51861 = AXIS2_PLACEMENT_3D ( 'NONE', #10153, #43694, #15171 ) ;
#51862 = VERTEX_POINT ( 'NONE', #58796 ) ;
#51863 = CARTESIAN_POINT ( 'NONE',  ( 0.9789233960466705575, -37.34478551170388272, -19.01850998151991234 ) ) ;
#51864 = CARTESIAN_POINT ( 'NONE',  ( 0.6000166863083090663, 44.47108027094602534, 20.83618250168510144 ) ) ;
#51865 = CARTESIAN_POINT ( 'NONE',  ( 5.917102823773431552, -13.97547681749000681, -14.46291000371437718 ) ) ;
#51866 = CARTESIAN_POINT ( 'NONE',  ( 0.1365634738349414679, -34.97642399247558842, -26.89818552099423954 ) ) ;
#51867 = ORIENTED_EDGE ( 'NONE', *, *, #19576, .T. ) ;
#51868 = ORIENTED_EDGE ( 'NONE', *, *, #51165, .F. ) ;
#51869 = CARTESIAN_POINT ( 'NONE',  ( 0.1140933569871964842, -44.12262566372946537, -0.3792817189201296291 ) ) ;
#51870 = CARTESIAN_POINT ( 'NONE',  ( -6.078457390727109555, -14.65958194562101546, 12.48563847855327680 ) ) ;
#51871 = CARTESIAN_POINT ( 'NONE',  ( 3.407937589446174087, -2.242416846335690828, 13.51415833181187232 ) ) ;
#51872 = AXIS2_PLACEMENT_3D ( 'NONE', #1129, #25560, #39384 ) ;
#51873 =( BOUNDED_SURFACE ( )  B_SPLINE_SURFACE ( 3, 1, ( 
 ( #44532, #53876 ),
 ( #15392, #2177 ),
 ( #6554, #29465 ),
 ( #957, #49194 ) ),
 .UNSPECIFIED., .F., .F., .F. ) 
 B_SPLINE_SURFACE_WITH_KNOTS ( ( 4, 4 ),
 ( 2, 2 ),
 ( 0.000000000000000000, 1.000000000000000000 ),
 ( 0.000000000000000000, 1.000000000000000000 ),
 .UNSPECIFIED. ) 
 GEOMETRIC_REPRESENTATION_ITEM ( )  RATIONAL_B_SPLINE_SURFACE ( (
 ( 1.000000000000000000, 1.000000000000000000),
 ( 0.7223157951917480446, 0.9931996967497186413),
 ( 0.7223157951917480446, 0.9931996967497186413),
 ( 1.000000000000000000, 1.000000000000000000) ) ) 
 REPRESENTATION_ITEM ( '' )  SURFACE ( )  );
#51874 = ORIENTED_EDGE ( 'NONE', *, *, #24538, .T. ) ;
#51875 = CARTESIAN_POINT ( 'NONE',  ( 5.965394784446458765, -12.48356622107688985, 16.29267539192321479 ) ) ;
#51876 = ORIENTED_EDGE ( 'NONE', *, *, #28397, .T. ) ;
#51877 = DIRECTION ( 'NONE',  ( -1.000000000000000000, 0.000000000000000000, 0.000000000000000000 ) ) ;
#51878 = CARTESIAN_POINT ( 'NONE',  ( 0.5824936645240093025, 27.52370025514170848, 37.96951544733510531 ) ) ;
#51879 = CARTESIAN_POINT ( 'NONE',  ( 0.1154773475650540532, 36.88152504251267771, -24.22182364283563416 ) ) ;
#51880 = ORIENTED_EDGE ( 'NONE', *, *, #58418, .F. ) ;
#51881 = B_SPLINE_CURVE_WITH_KNOTS ( 'NONE', 3,
 ( #40118, #21904, #59798, #45117 ),
 .UNSPECIFIED., .F., .F.,
 ( 4, 4 ),
 ( 0.000000000000000000, 0.005004948556313800097 ),
 .UNSPECIFIED. ) ;
#51883 = AXIS2_PLACEMENT_3D ( 'NONE', #32987, #18887, #60840 ) ;
#51882 = CARTESIAN_POINT ( 'NONE',  ( 4.956445790444010235, -22.15545010017738647, -41.55326799420456751 ) ) ;
#51884 = ADVANCED_FACE ( 'NONE', ( #43835 ), #14120, .F. ) ;
#51885 = CARTESIAN_POINT ( 'NONE',  ( -6.078726893082806448, -4.281536037414130469, 18.77398440472997265 ) ) ;
#51886 = CARTESIAN_POINT ( 'NONE',  ( 4.962356264823608143, 0.000000000000000000, 0.000000000000000000 ) ) ;
#51887 = B_SPLINE_CURVE_WITH_KNOTS ( 'NONE', 3,
 ( #8121, #27237, #56960, #37273 ),
 .UNSPECIFIED., .F., .F.,
 ( 4, 4 ),
 ( 0.000000000000000000, 0.004442905043737215703 ),
 .UNSPECIFIED. ) ;
#51888 = ADVANCED_FACE ( 'NONE', ( #1175, #1790 ), #15001, .T. ) ;
#51889 = CARTESIAN_POINT ( 'NONE',  ( -2.569797478183790229, 6.011723966604152203, -13.34095667500598736 ) ) ;
#51890 = CARTESIAN_POINT ( 'NONE',  ( 0.1154773475650540115, 33.48131017346754845, -28.73926754658474891 ) ) ;
#51891 = CARTESIAN_POINT ( 'NONE',  ( 2.618530812446111078, 44.94501346709284206, 13.77216590232064952 ) ) ;
#51892 = CARTESIAN_POINT ( 'NONE',  ( 0.1097557419366048670, 26.07515889977818446, -34.34829179474809280 ) ) ;
#51893 = B_SPLINE_CURVE_WITH_KNOTS ( 'NONE', 3,
 ( #57763, #48693, #42480, #43408, #19281, #14278 ),
 .UNSPECIFIED., .F., .F.,
 ( 4, 2, 4 ),
 ( 1.474357996003774831E-17, 0.0002293319059085077857, 0.0004586638118170008262 ),
 .UNSPECIFIED. ) ;
#51894 = CARTESIAN_POINT ( 'NONE',  ( -2.569797478183790229, -13.34095667500600868, -6.011723966604104241 ) ) ;
#51895 = ORIENTED_EDGE ( 'NONE', *, *, #55301, .T. ) ;
#51896 = EDGE_CURVE ( 'NONE', #61564, #50838, #16222, .T. ) ;
#51897 = CARTESIAN_POINT ( 'NONE',  ( 5.895596859100789899, 19.70914391261467102, 4.009716878325924050 ) ) ;
#51898 = VECTOR ( 'NONE', #45477, 1000.000000000000000 ) ;
#51899 = CARTESIAN_POINT ( 'NONE',  ( 0.8560838555295158248, 39.88643293834648063, 24.68694597426990001 ) ) ;
#51900 = EDGE_LOOP ( 'NONE', ( #18685, #17760, #28881, #27794 ) ) ;
#51901 = VECTOR ( 'NONE', #57723, 1000.000000000000000 ) ;
#51902 = DIRECTION ( 'NONE',  ( -0.07906939808003035641, 0.4719801263062105012, -0.8780562571152461526 ) ) ;
#51903 = CARTESIAN_POINT ( 'NONE',  ( 4.960156602257181468, 26.21519897043426894, 38.31207700265959915 ) ) ;
#51904 = CARTESIAN_POINT ( 'NONE',  ( 5.981074661064941900, -2.687517936919858297, -20.34795181394747843 ) ) ;
#51905 = CARTESIAN_POINT ( 'NONE',  ( 3.782625744892853081, 31.89518695616269639, -27.38494391315110832 ) ) ;
#51906 = CARTESIAN_POINT ( 'NONE',  ( 0.1073791018717483448, 5.147744207006859973, -42.81622261970989030 ) ) ;
#51907 = CARTESIAN_POINT ( 'NONE',  ( 5.880360259849739535, 47.87242051977161594, 3.090325311465030200 ) ) ;
#51909 = B_SPLINE_CURVE_WITH_KNOTS ( 'NONE', 3,
 ( #34575, #725, #1034, #39287 ),
 .UNSPECIFIED., .F., .F.,
 ( 4, 4 ),
 ( 2.266397508114618048E-17, 0.004559932413162186803 ),
 .UNSPECIFIED. ) ;
#51908 = CARTESIAN_POINT ( 'NONE',  ( 0.2285344041767106704, 3.479521872102009361, -43.98174732587396818 ) ) ;
#51910 = CARTESIAN_POINT ( 'NONE',  ( -67.98106116535524279, 2.453007415248453782E-15, -1.665530453207987265E-16 ) ) ;
#51911 = DIRECTION ( 'NONE',  ( 1.000000000000000000, 0.000000000000000000, 0.000000000000000000 ) ) ;
#51912 = CARTESIAN_POINT ( 'NONE',  ( -6.063463321072278589, 3.057971819381483325, 19.01234495877188024 ) ) ;
#51913 = DIRECTION ( 'NONE',  ( 1.000000000000000000, 0.000000000000000000, 0.000000000000000000 ) ) ;
#51914 = B_SPLINE_CURVE_WITH_KNOTS ( 'NONE', 3,
 ( #50596, #16804, #25879, #12728 ),
 .UNSPECIFIED., .F., .F.,
 ( 4, 4 ),
 ( 1.084202172485504434E-18, 0.004444878191957692126 ),
 .UNSPECIFIED. ) ;
#51915 = EDGE_CURVE ( 'NONE', #43985, #42350, #35026, .T. ) ;
#51916 = CARTESIAN_POINT ( 'NONE',  ( 0.7056313189692671184, 31.99428634539452077, -34.29452267063153670 ) ) ;
#51917 = B_SPLINE_CURVE_WITH_KNOTS ( 'NONE', 3,
 ( #57231, #47256, #14368, #61628 ),
 .UNSPECIFIED., .F., .F.,
 ( 4, 4 ),
 ( 3.469446951953614189E-18, 0.005004948556313816577 ),
 .UNSPECIFIED. ) ;
#51918 = CARTESIAN_POINT ( 'NONE',  ( -6.016489644550737204, -9.425415887801202430, 16.31649074174274361 ) ) ;
#51919 = VERTEX_POINT ( 'NONE', #49727 ) ;
#51920 = AXIS2_PLACEMENT_3D ( 'NONE', #5426, #30472, #33979 ) ;
#51921 = CARTESIAN_POINT ( 'NONE',  ( 0.2279481005628775647, 40.07358784552179287, -18.45565074063110700 ) ) ;
#51922 = CARTESIAN_POINT ( 'NONE',  ( -3.344563996438217224, -2.687817229851499068, -0.1586754815285013609 ) ) ;
#51923 = CARTESIAN_POINT ( 'NONE',  ( 0.5830082357119558134, 46.44034146464806412, 6.521251381845879713 ) ) ;
#51924 = CARTESIAN_POINT ( 'NONE',  ( 4.967162193818130511, -24.30453456948135482, 35.57684288741969425 ) ) ;
#51925 = EDGE_CURVE ( 'NONE', #7001, #26439, #5791, .T. ) ;
#51926 = ORIENTED_EDGE ( 'NONE', *, *, #49536, .F. ) ;
#51927 = CARTESIAN_POINT ( 'NONE',  ( 2.299746137290199943, 32.00013501491892498, -37.15202143508611954 ) ) ;
#51928 = ORIENTED_EDGE ( 'NONE', *, *, #40913, .F. ) ;
#51929 = CARTESIAN_POINT ( 'NONE',  ( 0.9968887458511677124, -25.59699785741763733, -34.43855515351798147 ) ) ;
#51930 = EDGE_CURVE ( 'NONE', #51399, #11906, #58127, .T. ) ;
#51931 = CARTESIAN_POINT ( 'NONE',  ( 0.5804410086790514622, 45.08525424748425792, 12.91664435118884846 ) ) ;
#51932 = ORIENTED_EDGE ( 'NONE', *, *, #37386, .T. ) ;
#51933 = B_SPLINE_CURVE_WITH_KNOTS ( 'NONE', 3,
 ( #14598, #9563, #57453, #4229, #23366, #23978 ),
 .UNSPECIFIED., .F., .F.,
 ( 4, 2, 4 ),
 ( 8.525499192591780946E-17, 0.0002293366620881443342, 0.0004586733241762034501 ),
 .UNSPECIFIED. ) ;
#51934 = CARTESIAN_POINT ( 'NONE',  ( 2.359973842542476330, -26.25271817560583898, 35.34021339812076690 ) ) ;
#51935 = EDGE_LOOP ( 'NONE', ( #30392, #43130, #23592, #40255 ) ) ;
#51936 = CARTESIAN_POINT ( 'NONE',  ( -6.017396004339686577, 17.40836349643177527, -7.212050743683987797 ) ) ;
#51938 = CARTESIAN_POINT ( 'NONE',  ( 0.7948878604505664747, 17.76850119055459132, 45.77094070193091113 ) ) ;
#51937 = VECTOR ( 'NONE', #6019, 1000.000000000000114 ) ;
#51939 = ORIENTED_EDGE ( 'NONE', *, *, #8550, .T. ) ;
#51940 = CARTESIAN_POINT ( 'NONE',  ( 4.967162193818130511, -23.56777426397153974, -36.06913038482822742 ) ) ;
#51941 = LINE ( 'NONE', #9972, #19597 ) ;
#51942 = CARTESIAN_POINT ( 'NONE',  ( 0.5997462898726536595, -43.04230894295718457, -23.64130434225950950 ) ) ;
#51943 = CARTESIAN_POINT ( 'NONE',  ( 1.827326673878742813, 22.58371678864582321, -36.65065268305635726 ) ) ;
#51944 = B_SPLINE_CURVE_WITH_KNOTS ( 'NONE', 3,
 ( #50195, #35499, #31093, #35190 ),
 .UNSPECIFIED., .F., .F.,
 ( 4, 4 ),
 ( 1.517883041479706208E-18, 0.004048833967417075214 ),
 .UNSPECIFIED. ) ;
#51945 = ORIENTED_EDGE ( 'NONE', *, *, #22654, .T. ) ;
#51946 = CARTESIAN_POINT ( 'NONE',  ( 5.910764540655177868, 16.59011036809723905, -11.36967354164205624 ) ) ;
#51947 = ORIENTED_EDGE ( 'NONE', *, *, #54584, .T. ) ;
#51948 = CARTESIAN_POINT ( 'NONE',  ( -2.601141883200662974, 7.298105880293700665, 13.02048685838633091 ) ) ;
#51949 = ORIENTED_EDGE ( 'NONE', *, *, #1960, .T. ) ;
#51950 = ORIENTED_EDGE ( 'NONE', *, *, #6632, .T. ) ;
#51951 = CARTESIAN_POINT ( 'NONE',  ( -2.601141883200665639, 6.503674101140891395, 13.43494140871250231 ) ) ;
#51952 = CARTESIAN_POINT ( 'NONE',  ( 0.6025881611877910160, -34.17105830828438684, 33.86250327239836366 ) ) ;
#51953 = VECTOR ( 'NONE', #13165, 1000.000000000000114 ) ;
#51954 = CARTESIAN_POINT ( 'NONE',  ( 0.1064266418746775134, 21.07422140941954680, 37.62465821955109391 ) ) ;
#51955 = CARTESIAN_POINT ( 'NONE',  ( 2.879087469061463622, -28.76677455459574162, -33.29526030095637168 ) ) ;
#51956 = ORIENTED_EDGE ( 'NONE', *, *, #51930, .T. ) ;
#51957 = CARTESIAN_POINT ( 'NONE',  ( 0.5800708057587364852, -46.09746469244091571, -13.00144577271090185 ) ) ;
#51958 = EDGE_CURVE ( 'NONE', #49082, #27245, #45364, .T. ) ;
#51959 = CARTESIAN_POINT ( 'NONE',  ( 0.5848930533535030563, 45.18167862054202999, -12.56538894812305784 ) ) ;
#51960 = CARTESIAN_POINT ( 'NONE',  ( 0.7044674535452954967, 48.35836311421829237, -8.559873814742601894 ) ) ;
#51961 = ORIENTED_EDGE ( 'NONE', *, *, #31491, .F. ) ;
#51962 = EDGE_CURVE ( 'NONE', #7385, #6350, #50442, .T. ) ;
#51963 = VERTEX_POINT ( 'NONE', #50954 ) ;
#51964 = CARTESIAN_POINT ( 'NONE',  ( 0.1103744047535531458, -21.52865142340111504, -37.36621271144529999 ) ) ;
#51965 = DIRECTION ( 'NONE',  ( 1.000000000000000000, 1.836909530733573776E-16, 0.000000000000000000 ) ) ;
#51966 = CARTESIAN_POINT ( 'NONE',  ( 5.272379999999998290, 0.000000000000000000, 15.38217999999999996 ) ) ;
#51967 = CARTESIAN_POINT ( 'NONE',  ( 4.975610109902397937, 7.237810502494805398, -48.37420290059309025 ) ) ;
#51968 = CARTESIAN_POINT ( 'NONE',  ( 5.959547316686252039, 12.49238070347976226, -16.28624005235086614 ) ) ;
#51969 = EDGE_CURVE ( 'NONE', #59715, #37650, #46896, .T. ) ;
#51970 = EDGE_LOOP ( 'NONE', ( #54632, #47653, #22839, #47701 ) ) ;
#51971 = ADVANCED_FACE ( 'NONE', ( #17765 ), #1272, .F. ) ;
#51972 = CARTESIAN_POINT ( 'NONE',  ( 1.827119703190778877, -9.946884032291396949, 41.88501940447977745 ) ) ;
#51973 = CARTESIAN_POINT ( 'NONE',  ( 3.221118495291108719, 42.77391066528618779, -10.25446176353823802 ) ) ;
#51974 = CARTESIAN_POINT ( 'NONE',  ( 3.390910168358336474, -39.24745467111843311, -19.84274271294525960 ) ) ;
#51975 = CARTESIAN_POINT ( 'NONE',  ( 4.960156602257182357, 46.35381625054452570, -2.524999074837725566 ) ) ;
#51976 = DIRECTION ( 'NONE',  ( -0.1011922191286467460, 0.9172554449906634710, 0.3852305587862932534 ) ) ;
#51977 = EDGE_CURVE ( 'NONE', #43585, #18698, #44676, .T. ) ;
#51978 =( BOUNDED_SURFACE ( )  B_SPLINE_SURFACE ( 3, 1, ( 
 ( #51835, #37159 ),
 ( #23654, #28047 ),
 ( #13973, #61533 ),
 ( #42476, #46868 ) ),
 .UNSPECIFIED., .F., .F., .F. ) 
 B_SPLINE_SURFACE_WITH_KNOTS ( ( 4, 4 ),
 ( 2, 2 ),
 ( 0.000000000000000000, 1.000000000000000000 ),
 ( 0.000000000000000000, 1.000000000000000000 ),
 .UNSPECIFIED. ) 
 GEOMETRIC_REPRESENTATION_ITEM ( )  RATIONAL_B_SPLINE_SURFACE ( (
 ( 1.000000000000000000, 1.000000000000000000),
 ( 0.7282232189291694135, 0.9929344683865672927),
 ( 0.7282232189291694135, 0.9929344683865672927),
 ( 1.000000000000000000, 1.000000000000000000) ) ) 
 REPRESENTATION_ITEM ( '' )  SURFACE ( )  );
#51979 = B_SPLINE_CURVE_WITH_KNOTS ( 'NONE', 3,
 ( #61356, #37600, #56665, #18794 ),
 .UNSPECIFIED., .F., .F.,
 ( 4, 4 ),
 ( 0.000000000000000000, 0.005013413432710140706 ),
 .UNSPECIFIED. ) ;
#51980 = ORIENTED_EDGE ( 'NONE', *, *, #14332, .T. ) ;
#51981 = CARTESIAN_POINT ( 'NONE',  ( 5.974727161628369032, 0.01551142186649469810, -20.52494643607030156 ) ) ;
#51982 = FACE_OUTER_BOUND ( 'NONE', #382, .T. ) ;
#51983 = EDGE_CURVE ( 'NONE', #5475, #58971, #13340, .T. ) ;
#51984 = CARTESIAN_POINT ( 'NONE',  ( 0.8551540677456739292, 47.37911285756620572, 7.157691013574519978 ) ) ;
#51985 = CARTESIAN_POINT ( 'NONE',  ( 4.956653778116982600, -47.27023054223759857, 8.845409907520762616 ) ) ;
#51986 = AXIS2_PLACEMENT_3D ( 'NONE', #38254, #10345, #52933 ) ;
#51987 = CARTESIAN_POINT ( 'NONE',  ( 0.9769922540276048117, 28.81531089420057157, 30.43040277677394201 ) ) ;
#51988 = CARTESIAN_POINT ( 'NONE',  ( 4.956653778116982600, -45.71126949320260735, 14.93973939759871072 ) ) ;
#51989 = CARTESIAN_POINT ( 'NONE',  ( 3.376099380956838925, 8.317686564981734421, -10.51306205816314332 ) ) ;
#51990 = CARTESIAN_POINT ( 'NONE',  ( 4.975610109902397937, -48.77192499014908833, -3.707929326867496655 ) ) ;
#51991 = CARTESIAN_POINT ( 'NONE',  ( 2.339468227445713921, 3.268109542640642573, 2.447078184617672891E-15 ) ) ;
#51992 = VERTEX_POINT ( 'NONE', #16529 ) ;
#51993 = AXIS2_PLACEMENT_3D ( 'NONE', #46378, #23175, #22867 ) ;
#51994 = CARTESIAN_POINT ( 'NONE',  ( 0.5997462898726536595, 48.29911994996563607, 8.873930482212578852 ) ) ;
#51995 = CARTESIAN_POINT ( 'NONE',  ( 4.060580049360325461, 23.21117414920292177, -37.31901779220056881 ) ) ;
#51996 = CARTESIAN_POINT ( 'NONE',  ( 0.8760168074887076939, 13.30888447662016461, 46.22580377597790147 ) ) ;
#51997 = CARTESIAN_POINT ( 'NONE',  ( 0.6064782688330873084, -2.277226958765353526, 46.84174082799485461 ) ) ;
#51998 = VERTEX_POINT ( 'NONE', #54715 ) ;
#51999 = CARTESIAN_POINT ( 'NONE',  ( 4.962356264823602814, -29.56943756613081931, -29.94802096775409339 ) ) ;
#52000 = CARTESIAN_POINT ( 'NONE',  ( -4.000000000000000000, 2.309401076758496263, -5.599999999999999645 ) ) ;
#52001 = EDGE_CURVE ( 'NONE', #49846, #60982, #24519, .T. ) ;
#52002 = ORIENTED_EDGE ( 'NONE', *, *, #36572, .F. ) ;
#52003 = EDGE_CURVE ( 'NONE', #4753, #22282, #21533, .T. ) ;
#52004 = CARTESIAN_POINT ( 'NONE',  ( 0.8760168074886965917, -33.37827814204101173, -34.63873394077476320 ) ) ;
#52005 = CARTESIAN_POINT ( 'NONE',  ( -3.273824404110865061, -10.31197987581545306, 5.906186990413314898E-14 ) ) ;
#52006 = ORIENTED_EDGE ( 'NONE', *, *, #14088, .T. ) ;
#52007 = CARTESIAN_POINT ( 'NONE',  ( -13.59350196068899841, -12.08345367038093521, -2.999999999999984013 ) ) ;
#52008 = ORIENTED_EDGE ( 'NONE', *, *, #5018, .T. ) ;
#52009 = ORIENTED_EDGE ( 'NONE', *, *, #12102, .T. ) ;
#52010 = CARTESIAN_POINT ( 'NONE',  ( -6.078457390727109555, 5.474669697364079823, -18.46137867934762866 ) ) ;
#52011 = ORIENTED_EDGE ( 'NONE', *, *, #36242, .F. ) ;
#52012 = ORIENTED_EDGE ( 'NONE', *, *, #14095, .F. ) ;
#52013 = LINE ( 'NONE', #57021, #13744 ) ;
#52014 = DIRECTION ( 'NONE',  ( 1.000000000000000000, 0.000000000000000000, 0.000000000000000000 ) ) ;
#52015 = CARTESIAN_POINT ( 'NONE',  ( 4.549368137175248350, 3.018832571115968033, 42.82045902618773425 ) ) ;
#52016 = B_SPLINE_CURVE_WITH_KNOTS ( 'NONE', 3,
 ( #16962, #45779, #31349, #31040, #7516, #50150, #51360, #36682, #2824, #13181, #21955, #60149, #32280, #31975, #8445, #27569, #46696, #3742, #22877 ),
 .UNSPECIFIED., .F., .F.,
 ( 4, 3, 3, 3, 3, 3, 4 ),
 ( 1.149162571898268292E-16, 0.0002618519381806238568, 0.0003927759815485961921, 0.0005237000248299452732, 0.0006546240681324992346, 0.0007855481115631317334, 0.0009699050456655165797 ),
 .UNSPECIFIED. ) ;
#52017 = EDGE_LOOP ( 'NONE', ( #8549, #45949, #48029, #54103 ) ) ;
#52018 = CARTESIAN_POINT ( 'NONE',  ( 0.6845945791218023269, -46.73791075327836353, 3.996776092368905964 ) ) ;
#52019 = LINE ( 'NONE', #32320, #471 ) ;
#52020 = CARTESIAN_POINT ( 'NONE',  ( 2.526552050251864578, -42.75269566045969327, 4.405466163647149713 ) ) ;
#52021 = CARTESIAN_POINT ( 'NONE',  ( -6.078457390727109555, 15.43466132010174618, 11.51371968441402238 ) ) ;
#52022 = ORIENTED_EDGE ( 'NONE', *, *, #38452, .T. ) ;
#52023 = CARTESIAN_POINT ( 'NONE',  ( 0.5804410086790514622, -1.020940616196085671, 46.88792522722238942 ) ) ;
#52024 = B_SPLINE_CURVE_WITH_KNOTS ( 'NONE', 3,
 ( #48765, #9951, #842, #43480 ),
 .UNSPECIFIED., .F., .F.,
 ( 4, 4 ),
 ( 0.000000000000000000, 0.005014147105413699519 ),
 .UNSPECIFIED. ) ;
#52025 = CARTESIAN_POINT ( 'NONE',  ( 0.1154773475650540254, -31.82144335153932246, -30.56696538864947499 ) ) ;
#52026 = VERTEX_POINT ( 'NONE', #23693 ) ;
#52027 = CARTESIAN_POINT ( 'NONE',  ( 2.000000000000010658, -3.464101615137748169, -5.600000000000000533 ) ) ;
#52028 = EDGE_CURVE ( 'NONE', #61623, #22696, #43132, .T. ) ;
#52029 = ORIENTED_EDGE ( 'NONE', *, *, #19449, .F. ) ;
#52030 = CIRCLE ( 'NONE', #60042, 42.08604991992415023 ) ;
#52031 = CARTESIAN_POINT ( 'NONE',  ( 0.8557997880470599172, 5.347802024197243043, 47.60865952217000796 ) ) ;
#52032 = CARTESIAN_POINT ( 'NONE',  ( 0.6029442701453591180, 46.57822130577238084, -15.55681603506220512 ) ) ;
#52033 = ORIENTED_EDGE ( 'NONE', *, *, #5166, .T. ) ;
#52034 = CARTESIAN_POINT ( 'NONE',  ( 0.9789233960466710016, -34.47665692943588311, -23.82638986087320632 ) ) ;
#52035 = CARTESIAN_POINT ( 'NONE',  ( 0.1129192098497455998, 25.64022107388826655, -35.91003830501005467 ) ) ;
#52036 = FACE_OUTER_BOUND ( 'NONE', #60653, .T. ) ;
#52037 = CARTESIAN_POINT ( 'NONE',  ( -6.079354080745853928, -18.27463532918897826, 6.068826808644322668 ) ) ;
#52038 = EDGE_CURVE ( 'NONE', #4083, #19166, #18695, .T. ) ;
#52039 = EDGE_CURVE ( 'NONE', #56918, #20008, #49936, .T. ) ;
#52040 = VECTOR ( 'NONE', #48961, 1000.000000000000000 ) ;
#52041 = ORIENTED_EDGE ( 'NONE', *, *, #23190, .T. ) ;
#52042 = CARTESIAN_POINT ( 'NONE',  ( 3.238931869106855821, -27.59912060131749456, -32.96367555688102868 ) ) ;
#52043 = EDGE_CURVE ( 'NONE', #48086, #39870, #26422, .T. ) ;
#52044 = CARTESIAN_POINT ( 'NONE',  ( 5.959828726073459926, -16.28130559351256323, -12.49879082830562460 ) ) ;
#52045 = CARTESIAN_POINT ( 'NONE',  ( -6.001507490154111224, -17.41542759839268939, 7.196845540359109172 ) ) ;
#52046 = CARTESIAN_POINT ( 'NONE',  ( 5.896278296736517710, 10.81775449038677905, -16.95591835908926726 ) ) ;
#52047 = B_SPLINE_CURVE_WITH_KNOTS ( 'NONE', 3,
 ( #20542, #55891, #36198, #26463 ),
 .UNSPECIFIED., .F., .F.,
 ( 4, 4 ),
 ( 0.000000000000000000, 0.005013413432710143308 ),
 .UNSPECIFIED. ) ;
#52048 = B_SPLINE_CURVE_WITH_KNOTS ( 'NONE', 3,
 ( #18999, #13992, #57781, #19296 ),
 .UNSPECIFIED., .F., .F.,
 ( 4, 4 ),
 ( 2.059984127722458425E-18, 0.004446298630425059815 ),
 .UNSPECIFIED. ) ;
#52049 = CYLINDRICAL_SURFACE ( 'NONE', #33321, 8.000000000000000000 ) ;
#52050 =( BOUNDED_SURFACE ( )  B_SPLINE_SURFACE ( 3, 1, ( 
 ( #32750, #41855 ),
 ( #60922, #8930 ),
 ( #57134, #32437 ),
 ( #14268, #28041 ) ),
 .UNSPECIFIED., .F., .F., .F. ) 
 B_SPLINE_SURFACE_WITH_KNOTS ( ( 4, 4 ),
 ( 2, 2 ),
 ( 0.000000000000000000, 1.000000000000000000 ),
 ( 0.000000000000000000, 1.000000000000000000 ),
 .UNSPECIFIED. ) 
 GEOMETRIC_REPRESENTATION_ITEM ( )  RATIONAL_B_SPLINE_SURFACE ( (
 ( 1.000000000000000000, 1.000000000000000000),
 ( 0.7282232189291693025, 0.9929344683865674037),
 ( 0.7282232189291693025, 0.9929344683865674037),
 ( 1.000000000000000000, 1.000000000000000000) ) ) 
 REPRESENTATION_ITEM ( '' )  SURFACE ( )  );
#52051 = EDGE_CURVE ( 'NONE', #18005, #3387, #47203, .T. ) ;
#52052 = DIRECTION ( 'NONE',  ( 0.000000000000000000, 0.000000000000000000, -1.000000000000000000 ) ) ;
#52053 = CARTESIAN_POINT ( 'NONE',  ( 4.975610109902397937, 5.990074626311793528E-15, -48.91267123290010943 ) ) ;
#52054 = CARTESIAN_POINT ( 'NONE',  ( 0.5830082357119558134, 40.48789625336803510, -23.66352239027072457 ) ) ;
#52055 = CARTESIAN_POINT ( 'NONE',  ( 4.833616638992208614, -35.06988470649548617, -30.15290813935891023 ) ) ;
#52056 = CARTESIAN_POINT ( 'NONE',  ( 0.9741495583595158880, 30.61921547032197566, -30.05988007970366027 ) ) ;
#52057 = B_SPLINE_CURVE_WITH_KNOTS ( 'NONE', 3,
 ( #41978, #41358, #61044, #7172 ),
 .UNSPECIFIED., .F., .F.,
 ( 4, 4 ),
 ( 8.384297404680615914E-17, 0.005004741218457495200 ),
 .UNSPECIFIED. ) ;
#52058 = CARTESIAN_POINT ( 'NONE',  ( 0.1102144999581333301, -21.67128446981406142, 37.28370465375319043 ) ) ;
#52059 = FACE_OUTER_BOUND ( 'NONE', #34053, .T. ) ;
#52060 = CARTESIAN_POINT ( 'NONE',  ( 5.959547316686252039, -7.858107265727618085, -18.96183906913540795 ) ) ;
#52061 = CARTESIAN_POINT ( 'NONE',  ( 0.9752570700956822991, -37.04395688491829475, -21.65368877244790724 ) ) ;
#52062 = CARTESIAN_POINT ( 'NONE',  ( 0.5830082357119558134, 45.30112170676081718, -12.12602189704361955 ) ) ;
#52063 = AXIS2_PLACEMENT_3D ( 'NONE', #11181, #7688, #40635 ) ;
#52064 = CARTESIAN_POINT ( 'NONE',  ( 0.6252788684277214015, -39.76148085432274115, -28.81785855064513768 ) ) ;
#52066 = ORIENTED_EDGE ( 'NONE', *, *, #50640, .F. ) ;
#52065 = CARTESIAN_POINT ( 'NONE',  ( 0.9757402383260944667, 39.60970160107532934, 16.49876987395742489 ) ) ;
#52067 = DIRECTION ( 'NONE',  ( -1.000000000000000000, -0.000000000000000000, -0.000000000000000000 ) ) ;
#52068 = CARTESIAN_POINT ( 'NONE',  ( 0.5806925824938499181, -19.24316026636448029, -42.76591101925195204 ) ) ;
#52069 = CARTESIAN_POINT ( 'NONE',  ( 0.7057020205114975520, -34.46103118762814432, 33.27137945725707624 ) ) ;
#52070 = ORIENTED_EDGE ( 'NONE', *, *, #8204, .T. ) ;
#52071 = CARTESIAN_POINT ( 'NONE',  ( 2.879087469061463622, -30.37913392544255586, 31.83095818104449748 ) ) ;
#52072 = CARTESIAN_POINT ( 'NONE',  ( 0.6000166863083090663, -39.66797998683874482, 28.95297645272786724 ) ) ;
#52074 = ORIENTED_EDGE ( 'NONE', *, *, #5624, .F. ) ;
#52073 = AXIS2_PLACEMENT_3D ( 'NONE', #19220, #25128, #44270 ) ;
#52075 = VERTEX_POINT ( 'NONE', #37505 ) ;
#52076 = EDGE_CURVE ( 'NONE', #17824, #36573, #49866, .T. ) ;
#52077 = DIRECTION ( 'NONE',  ( -0.000000000000000000, -0.000000000000000000, 1.000000000000000000 ) ) ;
#52078 = ORIENTED_EDGE ( 'NONE', *, *, #34604, .T. ) ;
#52079 = CARTESIAN_POINT ( 'NONE',  ( 4.553261556744873317, 12.71466023209499419, 42.04612920360230532 ) ) ;
#52080 = CARTESIAN_POINT ( 'NONE',  ( 0.1129192098497447394, 29.30421273086510681, -32.98810246148386227 ) ) ;
#52081 = ORIENTED_EDGE ( 'NONE', *, *, #44649, .F. ) ;
#52082 = EDGE_LOOP ( 'NONE', ( #7577, #4746, #16925, #28065 ) ) ;
#52083 = CARTESIAN_POINT ( 'NONE',  ( 0.5839254288179539509, -12.30867641975545546, -46.28738487712342220 ) ) ;
#52084 = ORIENTED_EDGE ( 'NONE', *, *, #33294, .T. ) ;
#52085 = CARTESIAN_POINT ( 'NONE',  ( 1.154321713695928731, 11.90271797554071398, -41.23280394713380304 ) ) ;
#52086 = CARTESIAN_POINT ( 'NONE',  ( 4.958415959904820092, 40.30989464198759720, 20.93600601295518970 ) ) ;
#52087 = B_SPLINE_CURVE_WITH_KNOTS ( 'NONE', 3,
 ( #50900, #51204, #18341, #17713 ),
 .UNSPECIFIED., .F., .F.,
 ( 4, 4 ),
 ( 0.000000000000000000, 0.004445488388166992516 ),
 .UNSPECIFIED. ) ;
#52088 = CARTESIAN_POINT ( 'NONE',  ( 0.1101816497532063094, -30.58948775778066675, -30.39741055095849021 ) ) ;
#52089 = ORIENTED_EDGE ( 'NONE', *, *, #52548, .F. ) ;
#52090 = CARTESIAN_POINT ( 'NONE',  ( 0.1129192098497447394, 30.02178898772887550, 32.33641869102754640 ) ) ;
#52091 = ORIENTED_EDGE ( 'NONE', *, *, #22786, .T. ) ;
#52092 = EDGE_LOOP ( 'NONE', ( #48760, #16666, #32567 ) ) ;
#52093 = FACE_OUTER_BOUND ( 'NONE', #615, .T. ) ;
#52094 = VERTEX_POINT ( 'NONE', #38131 ) ;
#52095 = CARTESIAN_POINT ( 'NONE',  ( 3.727782113643637985, 34.82198584334466318, 26.83667412016397691 ) ) ;
#52096 = CARTESIAN_POINT ( 'NONE',  ( 0.6064782688330866423, -14.57168774873476380, 44.57578224296398162 ) ) ;
#52097 = DIRECTION ( 'NONE',  ( 0.9848077530122080203, 0.1736481776669314692, -5.551115123125783935E-17 ) ) ;
#52098 = CARTESIAN_POINT ( 'NONE',  ( 4.956445790444038657, 44.30493387627053181, -15.95653108789415953 ) ) ;
#52099 = CARTESIAN_POINT ( 'NONE',  ( 0.5549461598389365813, -43.84610486898805704, -4.768310317555460642 ) ) ;
#52100 = EDGE_CURVE ( 'NONE', #11923, #60728, #32756, .T. ) ;
#52101 = ORIENTED_EDGE ( 'NONE', *, *, #12883, .T. ) ;
#52102 = CARTESIAN_POINT ( 'NONE',  ( 4.335381028904201628, -32.17603896083255677, 36.93858909670658619 ) ) ;
#52103 = DIRECTION ( 'NONE',  ( 0.000000000000000000, 0.000000000000000000, 1.000000000000000000 ) ) ;
#52104 = EDGE_CURVE ( 'NONE', #26869, #45900, #4553, .T. ) ;
#52105 = CARTESIAN_POINT ( 'NONE',  ( 0.5835871038041873238, 36.88843343318914236, -28.95648341471509823 ) ) ;
#52106 = EDGE_LOOP ( 'NONE', ( #54165, #46190, #43905, #30289 ) ) ;
#52107 = CARTESIAN_POINT ( 'NONE',  ( 0.8751705887134423323, -48.08707113907595243, -0.8911681664086732457 ) ) ;
#52108 = ADVANCED_FACE ( 'NONE', ( #24002 ), #3281, .F. ) ;
#52109 = CARTESIAN_POINT ( 'NONE',  ( 0.9757402383260944667, 30.28078671294527169, 30.40085236181960937 ) ) ;
#52110 = CARTESIAN_POINT ( 'NONE',  ( 0.8753041380234465318, -34.64850320773107484, -34.79395857525885560 ) ) ;
#52111 = EDGE_CURVE ( 'NONE', #22443, #7371, #54023, .T. ) ;
#52112 = VERTEX_POINT ( 'NONE', #19942 ) ;
#52113 = ORIENTED_EDGE ( 'NONE', *, *, #51178, .T. ) ;
#52114 = PLANE ( 'NONE',  #57875 ) ;
#52115 = ADVANCED_FACE ( 'NONE', ( #58720 ), #58528, .F. ) ;
#52116 = CARTESIAN_POINT ( 'NONE',  ( 0.8760168074886965917, -48.09529047980637273, -0.8912768426704601454 ) ) ;
#52117 = CARTESIAN_POINT ( 'NONE',  ( 4.553261556744873317, -33.30082861731504096, 28.64601855797499042 ) ) ;
#52118 = CARTESIAN_POINT ( 'NONE',  ( 0.5797568665920720399, -41.56795284195428053, 21.71014981825170409 ) ) ;
#52119 = DIRECTION ( 'NONE',  ( 0.000000000000000000, 0.000000000000000000, 1.000000000000000000 ) ) ;
#52120 = CARTESIAN_POINT ( 'NONE',  ( 0.1157991065609915438, -17.78625520842043883, -40.38058309631790621 ) ) ;
#52121 = CARTESIAN_POINT ( 'NONE',  ( 0.6028777368367060907, -42.83088177469218039, 24.02197734811634433 ) ) ;
#52122 = FACE_OUTER_BOUND ( 'NONE', #57110, .T. ) ;
#52123 = CARTESIAN_POINT ( 'NONE',  ( -6.078726893082806448, -8.909671472910670076, -17.07078778245227824 ) ) ;
#52124 = CARTESIAN_POINT ( 'NONE',  ( 0.5988103564986353433, 29.76496605343795920, 37.79415694022867456 ) ) ;
#52125 = DIRECTION ( 'NONE',  ( -0.000000000000000000, -0.000000000000000000, -1.000000000000000000 ) ) ;
#52126 =( BOUNDED_SURFACE ( )  B_SPLINE_SURFACE ( 3, 1, ( 
 ( #21468, #26787 ),
 ( #41220, #25857 ),
 ( #16786, #60279 ),
 ( #50278, #54964 ) ),
 .UNSPECIFIED., .F., .F., .F. ) 
 B_SPLINE_SURFACE_WITH_KNOTS ( ( 4, 4 ),
 ( 2, 2 ),
 ( 0.000000000000000000, 1.000000000000000000 ),
 ( 0.000000000000000000, 1.000000000000000000 ),
 .UNSPECIFIED. ) 
 GEOMETRIC_REPRESENTATION_ITEM ( )  RATIONAL_B_SPLINE_SURFACE ( (
 ( 1.000000000000000000, 1.000000000000000000),
 ( 0.9953390228620291325, 0.8624445117761032620),
 ( 0.9953390228620291325, 0.8624445117761032620),
 ( 1.000000000000000000, 1.000000000000000000) ) ) 
 REPRESENTATION_ITEM ( '' )  SURFACE ( )  );
#52127 = FACE_OUTER_BOUND ( 'NONE', #38879, .T. ) ;
#52129 = VERTEX_POINT ( 'NONE', #39667 ) ;
#52128 = EDGE_CURVE ( 'NONE', #21853, #20883, #44749, .T. ) ;
#52130 = CARTESIAN_POINT ( 'NONE',  ( 0.8744876279028263033, -38.80702141274021955, -30.07266432244763621 ) ) ;
#52131 = DIRECTION ( 'NONE',  ( -0.1011922191286467460, -0.8267003359790447981, -0.5534678755627595592 ) ) ;
#52133 = EDGE_CURVE ( 'NONE', #53370, #15459, #41682, .T. ) ;
#52132 = CARTESIAN_POINT ( 'NONE',  ( -99.50001199999974233, 2.999999999999994671, 1.500000000000001554 ) ) ;
#52134 = CARTESIAN_POINT ( 'NONE',  ( 0.6021447746440204973, -39.51108366771187264, -29.16188276657664602 ) ) ;
#52135 = B_SPLINE_CURVE_WITH_KNOTS ( 'NONE', 3,
 ( #35157, #16661, #7227, #11981 ),
 .UNSPECIFIED., .F., .F.,
 ( 4, 4 ),
 ( 2.230302957514598322E-17, 0.004564976165746185977 ),
 .UNSPECIFIED. ) ;
#52136 = CARTESIAN_POINT ( 'NONE',  ( 0.8751705887134423323, 44.76769609654235893, -17.57879340691497561 ) ) ;
#52137 = CARTESIAN_POINT ( 'NONE',  ( 4.962356264823608143, 0.000000000000000000, 0.000000000000000000 ) ) ;
#52138 = CONTEXT_DEPENDENT_SHAPE_REPRESENTATION ( #53972, #24348 ) ;
#52139 = CARTESIAN_POINT ( 'NONE',  ( 0.5830081025819933149, -25.00319000804665137, 39.67458284347498676 ) ) ;
#52140 = CARTESIAN_POINT ( 'NONE',  ( 0.5819845901640494645, 11.95725023767357875, 46.37938751183688169 ) ) ;
#52141 = CARTESIAN_POINT ( 'NONE',  ( 0.7044674535452954967, -8.668117436800997666, 48.33907801057787879 ) ) ;
#52142 =( BOUNDED_SURFACE ( )  B_SPLINE_SURFACE ( 3, 1, ( 
 ( #61340, #234 ),
 ( #43204, #41975 ),
 ( #47272, #4947 ),
 ( #18455, #18774 ) ),
 .UNSPECIFIED., .F., .F., .F. ) 
 B_SPLINE_SURFACE_WITH_KNOTS ( ( 4, 4 ),
 ( 2, 2 ),
 ( 0.000000000000000000, 1.000000000000000000 ),
 ( 0.000000000000000000, 1.000000000000000000 ),
 .UNSPECIFIED. ) 
 GEOMETRIC_REPRESENTATION_ITEM ( )  RATIONAL_B_SPLINE_SURFACE ( (
 ( 1.000000000000000000, 1.000000000000000000),
 ( 0.9953390228620291325, 0.8624445117761032620),
 ( 0.9953390228620291325, 0.8624445117761032620),
 ( 1.000000000000000000, 1.000000000000000000) ) ) 
 REPRESENTATION_ITEM ( '' )  SURFACE ( )  );
#52144 = ORIENTED_EDGE ( 'NONE', *, *, #8833, .F. ) ;
#52143 = CARTESIAN_POINT ( 'NONE',  ( 0.2940135542859013684, -35.83075920381577362, -25.73707915769758969 ) ) ;
#52145 = ORIENTED_EDGE ( 'NONE', *, *, #36715, .F. ) ;
#52146 = CARTESIAN_POINT ( 'NONE',  ( 0.1157506346131639274, -6.950611311771472067, 43.57326774750212905 ) ) ;
#52147 = CARTESIAN_POINT ( 'NONE',  ( 0.5997462898726536595, 49.03735788587799505, 2.624721264559015221 ) ) ;
#52148 = CARTESIAN_POINT ( 'NONE',  ( 5.896782393890504181, 17.95394716461052909, -9.065421561537322148 ) ) ;
#52149 =( BOUNDED_SURFACE ( )  B_SPLINE_SURFACE ( 3, 1, ( 
 ( #41504, #17374 ),
 ( #54628, #59965 ),
 ( #50564, #31150 ),
 ( #21759, #16144 ) ),
 .UNSPECIFIED., .F., .F., .F. ) 
 B_SPLINE_SURFACE_WITH_KNOTS ( ( 4, 4 ),
 ( 2, 2 ),
 ( 0.000000000000000000, 1.000000000000000000 ),
 ( 0.000000000000000000, 1.000000000000000000 ),
 .UNSPECIFIED. ) 
 GEOMETRIC_REPRESENTATION_ITEM ( )  RATIONAL_B_SPLINE_SURFACE ( (
 ( 1.000000000000000000, 1.000000000000000000),
 ( 0.7211978278499970862, 0.9934217856018976445),
 ( 0.7211978278499970862, 0.9934217856018976445),
 ( 1.000000000000000000, 1.000000000000000000) ) ) 
 REPRESENTATION_ITEM ( '' )  SURFACE ( )  );
#52150 = ORIENTED_EDGE ( 'NONE', *, *, #11544, .T. ) ;
#52151 = CARTESIAN_POINT ( 'NONE',  ( 4.691466044806102076, 33.74235639413328158, -29.14742760351073869 ) ) ;
#52152 = CARTESIAN_POINT ( 'NONE',  ( -5.719999999999997975, -15.71999999999999353, 1.925144768259639022E-15 ) ) ;
#52153 = B_SPLINE_CURVE_WITH_KNOTS ( 'NONE', 3,
 ( #12415, #49146, #55918, #29726, #12732, #25342, #15958, #44181, #48838, #39787, #5890, #20343, #54127, #31827, #53823, #36227, #55292, #25037, #60004, #49453, #17725, #44483, #40943, #50911, #58520 ),
 .UNSPECIFIED., .F., .F.,
 ( 4, 3, 3, 3, 3, 3, 3, 3, 4 ),
 ( 4.906538933386797396E-18, 0.0005656085177311379053, 0.001131215744874498538, 0.001696821861372765482, 0.002262427090022498151, 0.002828031679238745925, 0.003393635864401604429, 0.003977030878808131623, 0.004561030005651157265 ),
 .UNSPECIFIED. ) ;
#52154 = EDGE_LOOP ( 'NONE', ( #58544, #5303, #53265, #45521 ) ) ;
#52155 = ORIENTED_EDGE ( 'NONE', *, *, #15281, .T. ) ;
#52156 = EDGE_CURVE ( 'NONE', #15318, #30942, #22254, .T. ) ;
#52157 = DIRECTION ( 'NONE',  ( 1.000000000000000000, 0.000000000000000000, 0.000000000000000000 ) ) ;
#52158 = CARTESIAN_POINT ( 'NONE',  ( 3.221118495291109163, -40.02489484504095429, 18.24196295098654019 ) ) ;
#52159 = CARTESIAN_POINT ( 'NONE',  ( 0.9722240750034566448, -34.39263040572770791, -25.65687433776933446 ) ) ;
#52160 = CARTESIAN_POINT ( 'NONE',  ( 0.6252788684277210685, -47.66997436610286343, -11.79058417165001416 ) ) ;
#52161 = B_SPLINE_CURVE_WITH_KNOTS ( 'NONE', 3,
 ( #46361, #45441, #31946, #7488 ),
 .UNSPECIFIED., .F., .F.,
 ( 4, 4 ),
 ( 0.000000000000000000, 0.005004741218457418872 ),
 .UNSPECIFIED. ) ;
#52162 = CIRCLE ( 'NONE', #46203, 42.08604991992415023 ) ;
#52163 = CARTESIAN_POINT ( 'NONE',  ( 3.782625744892852193, -5.285730353412130711, 41.70490569136944714 ) ) ;
#52164 = AXIS2_PLACEMENT_3D ( 'NONE', #33693, #52769, #9873 ) ;
#52165 = DIRECTION ( 'NONE',  ( 0.000000000000000000, 0.000000000000000000, 1.000000000000000000 ) ) ;
#52166 = ORIENTED_EDGE ( 'NONE', *, *, #43586, .F. ) ;
#52167 = CARTESIAN_POINT ( 'NONE',  ( 4.956653778116966613, 0.000000000000000000, 0.000000000000000000 ) ) ;
#52168 = CARTESIAN_POINT ( 'NONE',  ( 3.894904216938897878, 43.95193974686379335, 0.5927267197078011085 ) ) ;
#52169 = ORIENTED_EDGE ( 'NONE', *, *, #48587, .T. ) ;
#52170 = CARTESIAN_POINT ( 'NONE',  ( 0.9780106845699496620, -37.26171966602630192, -19.18060202355250610 ) ) ;
#52171 = CARTESIAN_POINT ( 'NONE',  ( 4.962356264823608143, -38.57439820587617163, -16.83007429920747811 ) ) ;
#52172 = CARTESIAN_POINT ( 'NONE',  ( 2.359973842542475886, 38.98642570442579114, -20.44980453270367704 ) ) ;
#52173 = CARTESIAN_POINT ( 'NONE',  ( 4.553261556744873317, -43.82122302957819215, 3.039733214543990591 ) ) ;
#52174 = B_SPLINE_CURVE_WITH_KNOTS ( 'NONE', 3,
 ( #27302, #31390, #41738, #60801, #17923, #37043, #56106, #27612, #46740, #42052, #56411, #13527, #32632, #2559, #21679, #40823 ),
 .UNSPECIFIED., .F., .F.,
 ( 4, 3, 3, 3, 3, 4 ),
 ( 3.469446951953614189E-18, 0.0002732102107931864759, 0.0004098135523333763840, 0.0005464168938824969738, 0.0008195847345945471299, 0.001092771384553112637 ),
 .UNSPECIFIED. ) ;
#52175 = ORIENTED_EDGE ( 'NONE', *, *, #22921, .T. ) ;
#52176 = ORIENTED_EDGE ( 'NONE', *, *, #16564, .T. ) ;
#52177 = CARTESIAN_POINT ( 'NONE',  ( 5.960221823109900008, 7.859839668735214779, -18.96108896995707482 ) ) ;
#52178 = CARTESIAN_POINT ( 'NONE',  ( 0.3622758884714600280, -42.84426538328734324, 4.808133778521152202 ) ) ;
#52179 = CARTESIAN_POINT ( 'NONE',  ( 0.5797568665920715958, -2.195683281786883434, -46.84446908150365374 ) ) ;
#52180 = ORIENTED_EDGE ( 'NONE', *, *, #11200, .F. ) ;
#52181 = CARTESIAN_POINT ( 'NONE',  ( 0.5800708119828331677, 41.78924007434326882, 23.40241990038051867 ) ) ;
#52182 = EDGE_CURVE ( 'NONE', #25486, #47464, #10330, .T. ) ;
#52183 = VERTEX_POINT ( 'NONE', #53708 ) ;
#52184 = CARTESIAN_POINT ( 'NONE',  ( 0.6001305935487422083, -0.5236757026886095234, -48.10757715638248300 ) ) ;
#52185 = DIRECTION ( 'NONE',  ( -0.1011922191286467321, -0.9739806266819500680, -0.2027852894961952035 ) ) ;
#52186 = ORIENTED_EDGE ( 'NONE', *, *, #57510, .F. ) ;
#52187 = CARTESIAN_POINT ( 'NONE',  ( 0.5832366564991500191, -47.52097076201151538, -5.981458972434243293 ) ) ;
#52188 = EDGE_CURVE ( 'NONE', #34245, #15772, #42461, .T. ) ;
#52189 = CARTESIAN_POINT ( 'NONE',  ( -6.078726893082806448, -4.288195875146701752, 18.77246434022701749 ) ) ;
#52190 = CARTESIAN_POINT ( 'NONE',  ( -2.601141883200665639, 14.30071512379483245, -4.276093359300567442 ) ) ;
#52191 = EDGE_LOOP ( 'NONE', ( #41477, #8226, #4168, #11849 ) ) ;
#52192 = CARTESIAN_POINT ( 'NONE',  ( 0.2940135542859001472, 24.57542350531248232, -36.63726392931048537 ) ) ;
#52193 = CARTESIAN_POINT ( 'NONE',  ( 4.963659409799330291, 44.62477100936214214, 3.403493583737470018 ) ) ;
#52194 = CARTESIAN_POINT ( 'NONE',  ( 0.1073791018717483448, 26.63563652260123149, 33.91564619577815165 ) ) ;
#52195 = CARTESIAN_POINT ( 'NONE',  ( 0.6030672727741701600, 29.35514790473150626, -38.11303703924438224 ) ) ;
#52196 = CARTESIAN_POINT ( 'NONE',  ( 0.7764139734771262624, 36.25149465805695570, 29.76356171501883452 ) ) ;
#52197 = ORIENTED_EDGE ( 'NONE', *, *, #32790, .T. ) ;
#52198 = CARTESIAN_POINT ( 'NONE',  ( 0.9762797500689124330, 41.59901070109194876, 5.084003725032276932 ) ) ;
#52199 = CARTESIAN_POINT ( 'NONE',  ( 0.5797568599927144239, 4.067663806613229127, 46.71915474221869147 ) ) ;
#52200 = VERTEX_POINT ( 'NONE', #44986 ) ;
#52201 = CARTESIAN_POINT ( 'NONE',  ( 0.8560838555295223751, -29.58154842764516701, 36.40473632241573654 ) ) ;
#52202 = CARTESIAN_POINT ( 'NONE',  ( 0.5819845901640494645, 0.4540519722837509375, -47.89381229371849003 ) ) ;
#52204 = ADVANCED_FACE ( 'NONE', ( #31793 ), #2926, .F. ) ;
#52203 = CARTESIAN_POINT ( 'NONE',  ( 5.974727161628369032, 5.297264154380663115, 19.82959049719577749 ) ) ;
#52205 = CARTESIAN_POINT ( 'NONE',  ( 0.6001305935487422083, 37.84751346122816074, 29.70149728382448373 ) ) ;
#52206 = B_SPLINE_CURVE_WITH_KNOTS ( 'NONE', 3,
 ( #36584, #8354, #27475, #42223, #27172, #22779, #32814, #46600, #61585, #18706, #61281, #47213, #46296, #56589, #4260, #42523 ),
 .UNSPECIFIED., .F., .F.,
 ( 4, 3, 3, 3, 3, 4 ),
 ( 1.995049841954898532E-17, 0.0002618515315864436031, 0.0003927756766342006475, 0.0005236998216950585405, 0.0007855159896329922840, 0.001047349442285930039 ),
 .UNSPECIFIED. ) ;
#52207 = CARTESIAN_POINT ( 'NONE',  ( 2.282803330402959574, 46.95498684800680422, 1.313817932779367315 ) ) ;
#52208 = CARTESIAN_POINT ( 'NONE',  ( 4.967162193818129623, -13.42934394584134949, -40.93989340068622340 ) ) ;
#52209 = AXIS2_PLACEMENT_3D ( 'NONE', #60213, #7273, #59916 ) ;
#52210 = CARTESIAN_POINT ( 'NONE',  ( 1.827326673878745034, -25.21837361081565021, -34.89023127623411824 ) ) ;
#52211 = CARTESIAN_POINT ( 'NONE',  ( 0.000000000000000000, 0.000000000000000000, 0.000000000000000000 ) ) ;
#52212 = CARTESIAN_POINT ( 'NONE',  ( 0.5837800304671223461, 10.82717547783941292, 45.62904341920361873 ) ) ;
#52213 = AXIS2_PLACEMENT_3D ( 'NONE', #33847, #43876, #918 ) ;
#52214 = CARTESIAN_POINT ( 'NONE',  ( -6.015611763856276717, 18.19956619163665223, -4.882992715191109667 ) ) ;
#52215 = CARTESIAN_POINT ( 'NONE',  ( 0.9790724872846782167, 29.16362883271026263, -30.09680985236413164 ) ) ;
#52216 = DIRECTION ( 'NONE',  ( 0.000000000000000000, 1.000000000000000000, 0.000000000000000000 ) ) ;
#52217 = ORIENTED_EDGE ( 'NONE', *, *, #46212, .T. ) ;
#52218 = CYLINDRICAL_SURFACE ( 'NONE', #33509, 15.14599999999999369 ) ;
#52219 = CARTESIAN_POINT ( 'NONE',  ( 30.00000000000001066, 4.342925291379521108E-15, -1.386669559958810165E-30 ) ) ;
#52220 = CARTESIAN_POINT ( 'NONE',  ( 0.5797568665920712627, 23.08701827164173181, 40.81929563241816084 ) ) ;
#52221 = CARTESIAN_POINT ( 'NONE',  ( 0.6252788684277220677, -35.74989368885943009, -33.66584964632434662 ) ) ;
#52222 = DIRECTION ( 'NONE',  ( 0.09722883295013598492, 0.3366266327598188557, 0.9366050737423649020 ) ) ;
#52223 =( BOUNDED_SURFACE ( )  B_SPLINE_SURFACE ( 3, 1, ( 
 ( #12878, #31977 ),
 ( #3743, #22572 ),
 ( #61676, #56372 ),
 ( #60758, #42615 ) ),
 .UNSPECIFIED., .F., .F., .F. ) 
 B_SPLINE_SURFACE_WITH_KNOTS ( ( 4, 4 ),
 ( 2, 2 ),
 ( 0.000000000000000000, 1.000000000000000000 ),
 ( 0.000000000000000000, 1.000000000000000000 ),
 .UNSPECIFIED. ) 
 GEOMETRIC_REPRESENTATION_ITEM ( )  RATIONAL_B_SPLINE_SURFACE ( (
 ( 1.000000000000000000, 1.000000000000000000),
 ( 0.9729067724841187204, 0.9999501103223794596),
 ( 0.9729067724841187204, 0.9999501103223794596),
 ( 1.000000000000000000, 1.000000000000000000) ) ) 
 REPRESENTATION_ITEM ( '' )  SURFACE ( )  );
#52224 = ORIENTED_EDGE ( 'NONE', *, *, #55023, .T. ) ;
#52225 = FACE_OUTER_BOUND ( 'NONE', #52092, .T. ) ;
#52226 = CYLINDRICAL_SURFACE ( 'NONE', #17222, 18.99999999999999645 ) ;
#52227 = FACE_OUTER_BOUND ( 'NONE', #43682, .T. ) ;
#52228 = VERTEX_POINT ( 'NONE', #45291 ) ;
#52229 = CARTESIAN_POINT ( 'NONE',  ( 0.9722240750034571999, -11.66659272802828085, -41.29187379046135931 ) ) ;
#52230 = B_SPLINE_CURVE_WITH_KNOTS ( 'NONE', 3,
 ( #476, #9902, #38738, #38422, #10515, #57473, #9577, #33720, #10830, #24930, #47816, #4862, #14615, #19935, #43124, #52799, #57792, #14927, #27306 ),
 .UNSPECIFIED., .F., .F.,
 ( 4, 3, 3, 3, 3, 3, 4 ),
 ( 1.179660550279648157E-16, 0.0002618519381806238568, 0.0003927759815485961921, 0.0005237000248299418037, 0.0006546240681324958736, 0.0007855481115631319502, 0.0009699050456655096408 ),
 .UNSPECIFIED. ) ;
#52231 = EDGE_CURVE ( 'NONE', #11294, #38025, #33465, .T. ) ;
#52232 = CARTESIAN_POINT ( 'NONE',  ( 0.5830081025819919827, 43.28069043797167836, 18.05585416408522903 ) ) ;
#52233 = CARTESIAN_POINT ( 'NONE',  ( 0.5832367798473397924, 47.52096797443093834, -5.981481162905240012 ) ) ;
#52234 = EDGE_LOOP ( 'NONE', ( #13633, #45605, #36701, #26207 ) ) ;
#52235 = EDGE_CURVE ( 'NONE', #16817, #24773, #53607, .T. ) ;
#52236 = CARTESIAN_POINT ( 'NONE',  ( -4.467300000000000715, 5.741254171069846846E-15, 46.67105333295396719 ) ) ;
#52237 = ORIENTED_EDGE ( 'NONE', *, *, #31604, .F. ) ;
#52238 = CARTESIAN_POINT ( 'NONE',  ( 0.1368894036331251562, 42.07194175847984496, 13.29710654971273698 ) ) ;
#52239 = CARTESIAN_POINT ( 'NONE',  ( 0.5998501479064699549, 34.38546660123250120, 33.64490850298857083 ) ) ;
#52240 = ORIENTED_EDGE ( 'NONE', *, *, #41201, .F. ) ;
#52241 = CARTESIAN_POINT ( 'NONE',  ( 1.827119703190780653, 42.82501615430325614, 4.394694966566632388 ) ) ;
#52242 = CARTESIAN_POINT ( 'NONE',  ( 0.5832367798473391263, -29.37285281143867977, 37.83194459509899588 ) ) ;
#52243 = CARTESIAN_POINT ( 'NONE',  ( 0.9757892942422824456, 21.49867881049945950, 37.13414688883471371 ) ) ;
#52244 = CARTESIAN_POINT ( 'NONE',  ( -6.078075953587585900, 19.09727103821296623, -2.467673629183584350 ) ) ;
#52245 = MANIFOLD_SOLID_BREP ( 'CirPattern1', #48027 ) ;
#52246 = VECTOR ( 'NONE', #31983, 1000.000000000000000 ) ;
#52247 = ORIENTED_EDGE ( 'NONE', *, *, #3323, .T. ) ;
#52248 = CARTESIAN_POINT ( 'NONE',  ( 0.9790320750461909416, -6.885858362131810573, -41.33911086560582504 ) ) ;
#52249 = ORIENTED_EDGE ( 'NONE', *, *, #11013, .F. ) ;
#52250 = CARTESIAN_POINT ( 'NONE',  ( 0.9762797500689124330, -37.62962005162918899, 18.44821075214967721 ) ) ;
#52251 = VECTOR ( 'NONE', #48336, 1000.000000000000227 ) ;
#52252 = ORIENTED_EDGE ( 'NONE', *, *, #33145, .T. ) ;
#52253 = ADVANCED_FACE ( 'NONE', ( #30848 ), #41387, .F. ) ;
#52254 = ORIENTED_EDGE ( 'NONE', *, *, #20545, .T. ) ;
#52255 = CARTESIAN_POINT ( 'NONE',  ( 0.6029443199889047422, -42.78821616806403938, -24.09784635624990656 ) ) ;
#52256 = CARTESIAN_POINT ( 'NONE',  ( 5.960221823109900008, -20.34928172836732330, 2.684531185214074966 ) ) ;
#52257 = CARTESIAN_POINT ( 'NONE',  ( 4.975610109902397937, -32.45573888811600227, -36.59336579715246529 ) ) ;
#52258 = CARTESIAN_POINT ( 'NONE',  ( 1.834102595619085729, -28.46990526199986604, -33.61044836401974578 ) ) ;
#52259 = ORIENTED_EDGE ( 'NONE', *, *, #363, .T. ) ;
#52260 = CARTESIAN_POINT ( 'NONE',  ( -6.010958268070873523, 11.45964880703826339, 14.95835081545477863 ) ) ;
#52261 = EDGE_CURVE ( 'NONE', #2066, #47550, #10427, .T. ) ;
#52262 = CARTESIAN_POINT ( 'NONE',  ( 0.5797568665920721509, -46.07736677682986226, -8.723621926434374174 ) ) ;
#52263 = CARTESIAN_POINT ( 'NONE',  ( 0.1156495703730067298, -38.37914333307228532, 21.77118072706586105 ) ) ;
#52264 = ORIENTED_EDGE ( 'NONE', *, *, #55793, .F. ) ;
#52265 = EDGE_CURVE ( 'NONE', #49895, #27049, #55848, .T. ) ;
#52266 = VERTEX_POINT ( 'NONE', #9207 ) ;
#52267 = DIRECTION ( 'NONE',  ( 0.07836865515943411409, -0.9968932487286223942, -0.007886984708660975049 ) ) ;
#52268 = CARTESIAN_POINT ( 'NONE',  ( 0.5835226383429289454, -44.24119678963662494, 15.55503073499414413 ) ) ;
#52269 = CARTESIAN_POINT ( 'NONE',  ( 4.975610109902397937, -22.11219452748553138, -43.62912170003438916 ) ) ;
#52270 = CARTESIAN_POINT ( 'NONE',  ( -6.016489644550737204, -16.31649074174270808, -9.425415887801259274 ) ) ;
#52271 = ORIENTED_EDGE ( 'NONE', *, *, #42797, .T. ) ;
#52272 = EDGE_LOOP ( 'NONE', ( #6597, #28207, #48310, #15417 ) ) ;
#52273 = DIRECTION ( 'NONE',  ( 0.000000000000000000, 0.000000000000000000, -1.000000000000000000 ) ) ;
#52275 = EDGE_CURVE ( 'NONE', #57230, #39487, #2026, .T. ) ;
#52274 = CARTESIAN_POINT ( 'NONE',  ( 1.296416391601052487, 43.03271948257037138, -9.512750811966421693 ) ) ;
#52276 = CARTESIAN_POINT ( 'NONE',  ( 2.359973842542475886, -39.07714595377191813, -20.27591079927379525 ) ) ;
#52277 = DIRECTION ( 'NONE',  ( 1.000000000000000000, 0.000000000000000000, 0.000000000000000000 ) ) ;
#52278 = B_SPLINE_CURVE_WITH_KNOTS ( 'NONE', 3,
 ( #52866, #5235, #43497, #43187, #48183, #38184 ),
 .UNSPECIFIED., .F., .F.,
 ( 4, 2, 4 ),
 ( 1.764953265579307567E-18, 0.0002450742804987328209, 0.0004901485609974637987 ),
 .UNSPECIFIED. ) ;
#52279 = SURFACE_SIDE_STYLE ('',( #18798 ) ) ;
#52280 = CARTESIAN_POINT ( 'NONE',  ( 0.8557997880470690211, -34.51495345639526136, -33.22501220301936797 ) ) ;
#52281 = VERTEX_POINT ( 'NONE', #60893 ) ;
#52282 = CARTESIAN_POINT ( 'NONE',  ( 5.981074661064941900, 0.008585178657616161779, -20.52466374824937034 ) ) ;
#52283 = PLANE ( 'NONE',  #13617 ) ;
#52284 = CARTESIAN_POINT ( 'NONE',  ( 5.895596859100789899, 3.348897116308617417, -19.83212220910478507 ) ) ;
#52285 = CARTESIAN_POINT ( 'NONE',  ( 0.1102144999581333162, -16.38650952318882759, -39.88986724628629332 ) ) ;
#52286 = CARTESIAN_POINT ( 'NONE',  ( 0.9789233960466696693, 29.03992057262557935, 30.21621650650424584 ) ) ;
#52287 = CARTESIAN_POINT ( 'NONE',  ( 4.962356264823601926, -41.76635909427990612, -5.177532797579353918 ) ) ;
#52288 = CONICAL_SURFACE ( 'NONE', #13331, 43.08621763946400307, 1.568696531533066763 ) ;
#52289 = CARTESIAN_POINT ( 'NONE',  ( 2.299746137290199943, -48.77886755144294284, -4.990332462364070132 ) ) ;
#52290 = CARTESIAN_POINT ( 'NONE',  ( 2.643462169533613793, -37.25264019563434914, 30.32726672320737293 ) ) ;
#52291 = VERTEX_POINT ( 'NONE', #42742 ) ;
#52292 = EDGE_CURVE ( 'NONE', #19953, #16278, #8268, .T. ) ;
#52293 = CARTESIAN_POINT ( 'NONE',  ( 0.5806925824938499181, -2.112975627976999782, 46.84824112321762613 ) ) ;
#52294 = B_SPLINE_CURVE_WITH_KNOTS ( 'NONE', 3,
 ( #61925, #38175, #38791, #48174 ),
 .UNSPECIFIED., .F., .F.,
 ( 4, 4 ),
 ( 0.000000000000000000, 0.005014147105413700387 ),
 .UNSPECIFIED. ) ;
#52295 = CARTESIAN_POINT ( 'NONE',  ( 3.661933894777869902, -15.72363048476816161, 44.33281639293991816 ) ) ;
#52296 = DIRECTION ( 'NONE',  ( 0.000000000000000000, 0.000000000000000000, -1.000000000000000000 ) ) ;
#52297 = ORIENTED_EDGE ( 'NONE', *, *, #2185, .T. ) ;
#52298 = EDGE_CURVE ( 'NONE', #24004, #41667, #52858, .T. ) ;
#52299 = B_SPLINE_CURVE_WITH_KNOTS ( 'NONE', 3,
 ( #51017, #8109, #3392, #60711, #17832, #24067 ),
 .UNSPECIFIED., .F., .F.,
 ( 4, 2, 4 ),
 ( 1.870559545977334001E-17, 0.0002293319059085106317, 0.0004586638118170025609 ),
 .UNSPECIFIED. ) ;
#52300 = CARTESIAN_POINT ( 'NONE',  ( -6.078457390727109555, 5.483070842476203133, -18.45888526357686388 ) ) ;
#52301 = CARTESIAN_POINT ( 'NONE',  ( 5.895596859100789899, 18.99884588797239005, -6.600911917118875039 ) ) ;
#52302 = EDGE_CURVE ( 'NONE', #37338, #54112, #38685, .T. ) ;
#52303 = PLANE ( 'NONE',  #17530 ) ;
#52304 = VERTEX_POINT ( 'NONE', #51487 ) ;
#52305 = CARTESIAN_POINT ( 'NONE',  ( 5.974727161628369032, -19.82959049719579170, 5.297264154380593837 ) ) ;
#52306 = AXIS2_PLACEMENT_3D ( 'NONE', #59860, #25733, #16979 ) ;
#52307 = CARTESIAN_POINT ( 'NONE',  ( 4.549368137175248350, -38.59302160394766901, 18.79584381673463866 ) ) ;
#52308 = EDGE_CURVE ( 'NONE', #45323, #42702, #28314, .T. ) ;
#52309 = CARTESIAN_POINT ( 'NONE',  ( -6.016761891674564211, 2.462934516563804355, 18.68153697670642543 ) ) ;
#52310 = ORIENTED_EDGE ( 'NONE', *, *, #17195, .T. ) ;
#52311 = CARTESIAN_POINT ( 'NONE',  ( 1.227938101723756947, -6.439911493064287562, -42.43379953535192328 ) ) ;
#52312 = EDGE_LOOP ( 'NONE', ( #23136, #30618 ) ) ;
#52313 = CARTESIAN_POINT ( 'NONE',  ( 0.7954190325252770144, 33.39101560460801466, -34.61997719899450487 ) ) ;
#52314 = ORIENTED_EDGE ( 'NONE', *, *, #37798, .T. ) ;
#52315 = CARTESIAN_POINT ( 'NONE',  ( 0.5839254288179547281, -6.161657890844622010, -47.49799454719524050 ) ) ;
#52316 = DIRECTION ( 'NONE',  ( 0.000000000000000000, 0.000000000000000000, 1.000000000000000000 ) ) ;
#52317 = EDGE_LOOP ( 'NONE', ( #38203, #7164, #43540, #48778 ) ) ;
#52318 = CARTESIAN_POINT ( 'NONE',  ( 1.092182651088185130, 24.22945109136152908, -34.20080239195573313 ) ) ;
#52319 = ORIENTED_EDGE ( 'NONE', *, *, #16140, .F. ) ;
#52320 = FACE_OUTER_BOUND ( 'NONE', #9261, .T. ) ;
#52321 = CARTESIAN_POINT ( 'NONE',  ( 4.549368137175248350, -32.41327393324121431, -28.14399996863486209 ) ) ;
#52322 = CARTESIAN_POINT ( 'NONE',  ( 5.981074661064941900, -18.95903134304795401, 7.862380442163802385 ) ) ;
#52323 = B_SPLINE_CURVE_WITH_KNOTS ( 'NONE', 3,
 ( #15340, #14415, #908, #14722, #20643, #43240 ),
 .UNSPECIFIED., .F., .F.,
 ( 4, 2, 4 ),
 ( 4.336808689942017736E-19, 0.0002291459268755705330, 0.0004582918537511406322 ),
 .UNSPECIFIED. ) ;
#52324 = EDGE_CURVE ( 'NONE', #40762, #40551, #24453, .T. ) ;
#52325 = ORIENTED_EDGE ( 'NONE', *, *, #31930, .F. ) ;
#52326 = B_SPLINE_CURVE_WITH_KNOTS ( 'NONE', 3,
 ( #20781, #16087, #44921, #35201, #54259, #25782 ),
 .UNSPECIFIED., .F., .F.,
 ( 4, 2, 4 ),
 ( 8.560751122900633232E-17, 0.0002293366620881449847, 0.0004586733241762043717 ),
 .UNSPECIFIED. ) ;
#52327 = CARTESIAN_POINT ( 'NONE',  ( 0.9757402383260943557, -16.34189654378404555, -39.67468066200779475 ) ) ;
#52328 = CARTESIAN_POINT ( 'NONE',  ( 0.6000166863083106206, 37.73145429715492583, 31.43502566135684262 ) ) ;
#52329 = CARTESIAN_POINT ( 'NONE',  ( 0.9722240750034607526, 36.86535092060704244, -21.95618656573963179 ) ) ;
#52330 = CARTESIAN_POINT ( 'NONE',  ( 0.1156495703730067715, -22.99010713679044926, -37.66162406309594246 ) ) ;
#52331 = EDGE_LOOP ( 'NONE', ( #28370, #43144, #12310, #10102 ) ) ;
#52332 = ADVANCED_FACE ( 'NONE', ( #23017 ), #9700, .F. ) ;
#52333 = DIRECTION ( 'NONE',  ( 0.09722883295013592941, 0.1030875952483757685, 0.9899088350697055061 ) ) ;
#52334 = CARTESIAN_POINT ( 'NONE',  ( 0.1140933569871964287, -18.20692391496250906, 40.19275894534575855 ) ) ;
#52335 = EDGE_LOOP ( 'NONE', ( #16834, #12506, #50919, #11067, #24918 ) ) ;
#52336 = AXIS2_PLACEMENT_3D ( 'NONE', #43461, #42533, #29031 ) ;
#52337 = CARTESIAN_POINT ( 'NONE',  ( 4.303969348037246512, 39.44373910178647691, -27.54579249306170041 ) ) ;
#52338 = EDGE_CURVE ( 'NONE', #59093, #29930, #27519, .T. ) ;
#52339 = ORIENTED_EDGE ( 'NONE', *, *, #53303, .T. ) ;
#52340 = LINE ( 'NONE', #52960, #60513 ) ;
#52341 =( BOUNDED_SURFACE ( )  B_SPLINE_SURFACE ( 3, 1, ( 
 ( #10574, #42874 ),
 ( #61927, #14979 ),
 ( #19361, #14359 ),
 ( #24668, #853 ) ),
 .UNSPECIFIED., .F., .F., .F. ) 
 B_SPLINE_SURFACE_WITH_KNOTS ( ( 4, 4 ),
 ( 2, 2 ),
 ( 0.000000000000000000, 1.000000000000000000 ),
 ( 0.000000000000000000, 1.000000000000000000 ),
 .UNSPECIFIED. ) 
 GEOMETRIC_REPRESENTATION_ITEM ( )  RATIONAL_B_SPLINE_SURFACE ( (
 ( 1.000000000000000000, 1.000000000000000000),
 ( 0.7269869731126817891, 0.9931720237060910339),
 ( 0.7269869731126817891, 0.9931720237060910339),
 ( 1.000000000000000000, 1.000000000000000000) ) ) 
 REPRESENTATION_ITEM ( '' )  SURFACE ( )  );
#52342 = CARTESIAN_POINT ( 'NONE',  ( 0.1310142868023679297, -41.48473022063175364, -11.77532653407824270 ) ) ;
#52343 = ORIENTED_EDGE ( 'NONE', *, *, #20383, .T. ) ;
#52344 = CARTESIAN_POINT ( 'NONE',  ( 0.1073791018717483448, 6.109314776652144729, 42.68962945260955877 ) ) ;
#52345 = FACE_OUTER_BOUND ( 'NONE', #45465, .T. ) ;
#52346 = CARTESIAN_POINT ( 'NONE',  ( 2.282803330402964903, -42.50075538189024371, 20.00456696421370850 ) ) ;
#52347 = CARTESIAN_POINT ( 'NONE',  ( 0.9787284016396595732, -22.70791007621392410, -35.22338454634100202 ) ) ;
#52348 = EDGE_LOOP ( 'NONE', ( #19928, #44911, #57387, #13051 ) ) ;
#52349 = CARTESIAN_POINT ( 'NONE',  ( 0.1129192098497447394, -40.71518461128108157, 17.00663193740767909 ) ) ;
#52350 = CARTESIAN_POINT ( 'NONE',  ( 5.895596859100789899, -15.78680134203104579, -12.46214614742317295 ) ) ;
#52351 = EDGE_CURVE ( 'NONE', #20821, #52454, #58053, .T. ) ;
#52352 = CARTESIAN_POINT ( 'NONE',  ( -6.078075953587585900, 9.977648803905792008, 16.46941706901168345 ) ) ;
#52353 = CARTESIAN_POINT ( 'NONE',  ( 0.5809828226811544205, -34.25055090842130312, -33.48000389720652947 ) ) ;
#52354 = EDGE_CURVE ( 'NONE', #22119, #10972, #38761, .T. ) ;
#52355 = CARTESIAN_POINT ( 'NONE',  ( 0.5836750258453350382, -46.31062999473594743, 12.22088356912710339 ) ) ;
#52356 = CARTESIAN_POINT ( 'NONE',  ( 0.6067099128993201917, 33.36330296770442772, -34.36589933408209419 ) ) ;
#52357 = CARTESIAN_POINT ( 'NONE',  ( 0.5830081025819920937, 40.20945637685019136, -24.13362078637243968 ) ) ;
#52358 = FACE_OUTER_BOUND ( 'NONE', #18371, .T. ) ;
#52359 = CARTESIAN_POINT ( 'NONE',  ( 4.322998006666165516, 42.57894920390128135, -22.13465289016582460 ) ) ;
#52360 = CARTESIAN_POINT ( 'NONE',  ( 0.6064515330803595949, 33.10959316660201779, 33.21278633868569585 ) ) ;
#52361 = CARTESIAN_POINT ( 'NONE',  ( 0.1129192098497447394, 39.96249028893947752, 18.70698152272492365 ) ) ;
#52362 = CARTESIAN_POINT ( 'NONE',  ( 0.9972139404380295780, -41.61281131482456175, -10.46878911444719584 ) ) ;
#52363 = FACE_OUTER_BOUND ( 'NONE', #51024, .T. ) ;
#52364 = CARTESIAN_POINT ( 'NONE',  ( 10.00000000000000533, -2.774815975767171530E-13, 80.00000000000001421 ) ) ;
#52365 = CARTESIAN_POINT ( 'NONE',  ( -2.569797478183790229, 14.44232325624823687, 2.353985772484800787 ) ) ;
#52366 = CARTESIAN_POINT ( 'NONE',  ( 0.8760168074886960365, 47.80016357497249402, -5.394043284319009146 ) ) ;
#52367 = EDGE_LOOP ( 'NONE', ( #7724, #9089, #6226, #46489 ) ) ;
#52368 = CARTESIAN_POINT ( 'NONE',  ( 5.895596859100789899, -18.51552686702066808, 7.855154234585303819 ) ) ;
#52369 = DIRECTION ( 'NONE',  ( 0.000000000000000000, 8.881784197001252323E-16, 1.000000000000000000 ) ) ;
#52370 = FACE_OUTER_BOUND ( 'NONE', #45359, .T. ) ;
#52371 = ORIENTED_EDGE ( 'NONE', *, *, #45503, .F. ) ;
#52372 = ADVANCED_FACE ( 'NONE', ( #19859 ), #38437, .T. ) ;
#52373 = CARTESIAN_POINT ( 'NONE',  ( 0.5839879327111927587, -33.80333292213281737, 33.93179405280476146 ) ) ;
#52374 = CARTESIAN_POINT ( 'NONE',  ( 0.8560838555295223751, -13.02223058219873764, 45.06433561859954295 ) ) ;
#52375 = B_SPLINE_CURVE_WITH_KNOTS ( 'NONE', 3,
 ( #15416, #34528, #53595, #10719 ),
 .UNSPECIFIED., .F., .F.,
 ( 4, 4 ),
 ( 3.878959614448864246E-18, 0.004042984057420970223 ),
 .UNSPECIFIED. ) ;
#52376 = EDGE_CURVE ( 'NONE', #61495, #17545, #5082, .T. ) ;
#52377 = UNCERTAINTY_MEASURE_WITH_UNIT (LENGTH_MEASURE( 1.000000000000000082E-05 ), #27903, 'distance_accuracy_value', 'NONE');
#52378 = ORIENTED_EDGE ( 'NONE', *, *, #59757, .T. ) ;
#52379 = VERTEX_POINT ( 'NONE', #24854 ) ;
#52380 = CARTESIAN_POINT ( 'NONE',  ( 0.6017666602106489515, -38.37783452831185826, -29.00829887116056582 ) ) ;
#52381 = EDGE_CURVE ( 'NONE', #36178, #61953, #47609, .T. ) ;
#52382 = EDGE_LOOP ( 'NONE', ( #7315, #42893, #3319, #35194 ) ) ;
#52383 = EDGE_CURVE ( 'NONE', #10343, #52281, #9427, .T. ) ;
#52384 = LINE ( 'NONE', #9171, #28930 ) ;
#52385 = ADVANCED_FACE ( 'NONE', ( #6320, #25149 ), #43056, .T. ) ;
#52386 = ORIENTED_EDGE ( 'NONE', *, *, #35159, .T. ) ;
#52387 = EDGE_LOOP ( 'NONE', ( #61392, #37978, #54151, #38183 ) ) ;
#52388 = CARTESIAN_POINT ( 'NONE',  ( 4.956445790444036881, 42.27038699792232279, -20.75457619864872783 ) ) ;
#52389 = VERTEX_POINT ( 'NONE', #38358 ) ;
#52390 = DIRECTION ( 'NONE',  ( 1.000000000000000000, 0.000000000000000000, 0.000000000000000000 ) ) ;
#52391 = CARTESIAN_POINT ( 'NONE',  ( -6.063463321072276813, -8.920783457832165197, -17.06575738072992365 ) ) ;
#52392 = CONICAL_SURFACE ( 'NONE', #51403, 43.08621763946400307, 1.568696531533066763 ) ;
#52393 = CARTESIAN_POINT ( 'NONE',  ( 0.2940135542859012574, 9.030615564221935898, -43.18203945186763804 ) ) ;
#52394 = ORIENTED_EDGE ( 'NONE', *, *, #50904, .T. ) ;
#52396 = B_SPLINE_CURVE_WITH_KNOTS ( 'NONE', 3,
 ( #60175, #17285, #3161, #36405, #18209, #37321, #51701, #31688, #50775, #51080, #56090, #7867, #46724, #46413, #17590, #13204 ),
 .UNSPECIFIED., .F., .F.,
 ( 4, 3, 3, 3, 3, 4 ),
 ( 2.221635811791082109E-17, 0.0002618515315864412721, 0.0003927756766341965818, 0.0005236998216950529026, 0.0007855159896329868630, 0.001047349442285927870 ),
 .UNSPECIFIED. ) ;
#52395 = LINE ( 'NONE', #9488, #15710 ) ;
#52397 =( BOUNDED_SURFACE ( )  B_SPLINE_SURFACE ( 3, 1, ( 
 ( #6774, #40974 ),
 ( #12767, #60332 ),
 ( #21524, #2709 ),
 ( #59727, #32167 ) ),
 .UNSPECIFIED., .F., .F., .F. ) 
 B_SPLINE_SURFACE_WITH_KNOTS ( ( 4, 4 ),
 ( 2, 2 ),
 ( 0.000000000000000000, 1.000000000000000000 ),
 ( 0.000000000000000000, 1.000000000000000000 ),
 .UNSPECIFIED. ) 
 GEOMETRIC_REPRESENTATION_ITEM ( )  RATIONAL_B_SPLINE_SURFACE ( (
 ( 1.000000000000000000, 1.000000000000000000),
 ( 0.9952954269826590483, 0.8620686068821307169),
 ( 0.9952954269826590483, 0.8620686068821307169),
 ( 1.000000000000000000, 1.000000000000000000) ) ) 
 REPRESENTATION_ITEM ( '' )  SURFACE ( )  );
#52398 = EDGE_CURVE ( 'NONE', #42400, #26123, #14778, .T. ) ;
#52399 = CARTESIAN_POINT ( 'NONE',  ( 0.5998501479064699549, -48.10473956285919428, 0.5236536531313263909 ) ) ;
#52400 = EDGE_LOOP ( 'NONE', ( #37639, #19058, #18010, #11444 ) ) ;
#52401 = ORIENTED_EDGE ( 'NONE', *, *, #56209, .F. ) ;
#52402 = DIRECTION ( 'NONE',  ( 0.000000000000000000, -1.000000000000000000, 0.000000000000000000 ) ) ;
#52403 = ORIENTED_EDGE ( 'NONE', *, *, #7905, .F. ) ;
#52404 = CARTESIAN_POINT ( 'NONE',  ( 1.112077966505211180, 34.23546808238941708, 27.76622139053583993 ) ) ;
#52405 = DIRECTION ( 'NONE',  ( -1.000000000000000000, -0.000000000000000000, -0.000000000000000000 ) ) ;
#52406 = CARTESIAN_POINT ( 'NONE',  ( 0.8551540677456834771, -7.157691013574049244, -47.37911285756627677 ) ) ;
#52407 = CARTESIAN_POINT ( 'NONE',  ( 0.8560838555295158248, 43.53454501559585310, -17.46757637357826454 ) ) ;
#52408 = ORIENTED_EDGE ( 'NONE', *, *, #5964, .F. ) ;
#52409 = CARTESIAN_POINT ( 'NONE',  ( 0.6064782688330846439, 16.18998450771341524, 44.01384836683529755 ) ) ;
#52410 = CARTESIAN_POINT ( 'NONE',  ( 4.956445790444038657, 44.30493387627053181, -15.95653108789415953 ) ) ;
#52411 =( BOUNDED_SURFACE ( )  B_SPLINE_SURFACE ( 3, 1, ( 
 ( #43291, #37987 ),
 ( #56734, #48580 ),
 ( #14166, #15085 ),
 ( #34193, #47354 ) ),
 .UNSPECIFIED., .F., .F., .F. ) 
 B_SPLINE_SURFACE_WITH_KNOTS ( ( 4, 4 ),
 ( 2, 2 ),
 ( 0.000000000000000000, 1.000000000000000000 ),
 ( 0.000000000000000000, 1.000000000000000000 ),
 .UNSPECIFIED. ) 
 GEOMETRIC_REPRESENTATION_ITEM ( )  RATIONAL_B_SPLINE_SURFACE ( (
 ( 1.000000000000000000, 1.000000000000000000),
 ( 0.9754377213608244057, 0.9999580625633939235),
 ( 0.9754377213608244057, 0.9999580625633939235),
 ( 1.000000000000000000, 1.000000000000000000) ) ) 
 REPRESENTATION_ITEM ( '' )  SURFACE ( )  );
#52412 = CARTESIAN_POINT ( 'NONE',  ( 0.5782707292762442330, -46.10024953908504841, 8.631532085424261425 ) ) ;
#52413 = VERTEX_POINT ( 'NONE', #29234 ) ;
#52414 = DIRECTION ( 'NONE',  ( -1.000000000000000000, -0.000000000000000000, -0.000000000000000000 ) ) ;
#52415 = DIRECTION ( 'NONE',  ( 1.000000000000000000, 0.000000000000000000, 0.000000000000000000 ) ) ;
#52416 = CARTESIAN_POINT ( 'NONE',  ( 4.226256110419178924, -4.630474462406013458, 43.69652109997080203 ) ) ;
#52417 = VERTEX_POINT ( 'NONE', #14545 ) ;
#52418 = ORIENTED_EDGE ( 'NONE', *, *, #40265, .T. ) ;
#52419 = FACE_OUTER_BOUND ( 'NONE', #61469, .T. ) ;
#52420 = CARTESIAN_POINT ( 'NONE',  ( -6.015611763856276717, 18.84324252354755203, -0.006214430185207123029 ) ) ;
#52421 = CARTESIAN_POINT ( 'NONE',  ( 3.660087539127338641, 43.62750476736577809, -20.10768839917357553 ) ) ;
#52422 = CARTESIAN_POINT ( 'NONE',  ( 0.5806925824938502512, -41.60618895332704170, 21.63671424046659908 ) ) ;
#52423 = LINE ( 'NONE', #57115, #16553 ) ;
#52424 = LINE ( 'NONE', #13945, #59457 ) ;
#52425 =( LENGTH_UNIT ( ) NAMED_UNIT ( * ) SI_UNIT ( .MILLI., .METRE. ) );
#52426 = CARTESIAN_POINT ( 'NONE',  ( 0.8554163680231738898, -29.58718577084389523, -36.41159034254604165 ) ) ;
#52427 = EDGE_CURVE ( 'NONE', #58761, #59315, #43186, .T. ) ;
#52428 = CARTESIAN_POINT ( 'NONE',  ( 4.975801465491695552, 0.000000000000000000, 0.000000000000000000 ) ) ;
#52429 = CARTESIAN_POINT ( 'NONE',  ( 0.7246131072078515478, 19.16331062551085651, -44.12003537001155706 ) ) ;
#52430 = CARTESIAN_POINT ( 'NONE',  ( 0.9790850452238872847, 41.90864786853558854, -0.05063688658461517472 ) ) ;
#52431 = CARTESIAN_POINT ( 'NONE',  ( 0.5807400328401574052, 11.87003418057243387, 46.40483864045149431 ) ) ;
#52432 = VERTEX_POINT ( 'NONE', #35192 ) ;
#52433 = CARTESIAN_POINT ( 'NONE',  ( 4.967162193818131399, 42.16965968614193372, 8.839793687085363061 ) ) ;
#52434 = CARTESIAN_POINT ( 'NONE',  ( 0.6008123274975392114, 40.91732262123389319, 27.15377065286363845 ) ) ;
#52435 = PRODUCT_RELATED_PRODUCT_CATEGORY ( 'part', '', ( #8800 ) ) ;
#52436 = CARTESIAN_POINT ( 'NONE',  ( 0.1147471544378676905, -35.54663639407677067, -26.14170670672713825 ) ) ;
#52437 = CARTESIAN_POINT ( 'NONE',  ( -4.908599999999998964, 0.000000000000000000, 0.000000000000000000 ) ) ;
#52438 = AXIS2_PLACEMENT_3D ( 'NONE', #17528, #51026, #17842 ) ;
#52439 = CARTESIAN_POINT ( 'NONE',  ( 2.282803330402960462, 21.41355745235515684, 41.80856927343567975 ) ) ;
#52440 = B_SPLINE_CURVE_WITH_KNOTS ( 'NONE', 3,
 ( #4667, #38245, #10648, #57601 ),
 .UNSPECIFIED., .F., .F.,
 ( 4, 4 ),
 ( 0.000000000000000000, 0.005004741218457414535 ),
 .UNSPECIFIED. ) ;
#52441 = ITEM_DEFINED_TRANSFORMATION ( 'NONE', 'NONE', #30905,  #14677 ) ;
#52442 = CARTESIAN_POINT ( 'NONE',  ( 4.956653778116966613, 0.000000000000000000, 0.000000000000000000 ) ) ;
#52443 = CARTESIAN_POINT ( 'NONE',  ( 0.6016117650947688800, 48.13415862694574088, -9.729019864329799816 ) ) ;
#52444 = CARTESIAN_POINT ( 'NONE',  ( 0.7764146366350255235, 10.00418648031552138, -45.82528479492778217 ) ) ;
#52445 = CARTESIAN_POINT ( 'NONE',  ( -6.017396004339687465, 4.875835690939179123, 18.20140164570670649 ) ) ;
#52446 = B_SPLINE_CURVE_WITH_KNOTS ( 'NONE', 3,
 ( #23239, #57639, #28854, #61420, #32644, #325, #4397, #32962, #19172, #57335, #51729, #52034, #5028, #52649, #28236, #47353, #42663, #61728, #38284 ),
 .UNSPECIFIED., .F., .F.,
 ( 4, 3, 3, 3, 3, 3, 4 ),
 ( 9.813676791237317679E-18, 0.0002732106629380691540, 0.0004098138914053827504, 0.0005464171197651536286, 0.0006830203481512645480, 0.0008196235766963743665, 0.001011968216111141161 ),
 .UNSPECIFIED. ) ;
#52448 = EDGE_LOOP ( 'NONE', ( #48025, #58269, #23075, #20069 ) ) ;
#52447 = CARTESIAN_POINT ( 'NONE',  ( 4.962356264823597485, -14.71877352713633158, 39.42833123173257803 ) ) ;
#52449 = EDGE_LOOP ( 'NONE', ( #54280, #33005, #19017, #38251 ) ) ;
#52450 = CARTESIAN_POINT ( 'NONE',  ( 1.227938101723748288, -30.94118573761333479, 29.74462687941215222 ) ) ;
#52451 = CARTESIAN_POINT ( 'NONE',  ( 4.956445790444004018, -43.56224489968113289, 17.88487823385560205 ) ) ;
#52452 = CARTESIAN_POINT ( 'NONE',  ( 2.624215991343620935, 11.05657803851110721, -46.71702075422640377 ) ) ;
#52453 = MANIFOLD_SOLID_BREP ( 'Move Face1', #39064 ) ;
#52454 = VERTEX_POINT ( 'NONE', #55192 ) ;
#52455 = CARTESIAN_POINT ( 'NONE',  ( 4.335381028904201628, 48.44495715814558423, -7.269317272604295610 ) ) ;
#52456 = CARTESIAN_POINT ( 'NONE',  ( 0.5837800005270560311, -45.95628241222482302, 9.341058049793774742 ) ) ;
#52457 = CARTESIAN_POINT ( 'NONE',  ( 3.660087539127334200, 27.72868323267864810, -39.22752134874889407 ) ) ;
#52458 = EDGE_CURVE ( 'NONE', #32445, #54909, #4391, .T. ) ;
#52459 = VERTEX_POINT ( 'NONE', #11371 ) ;
#52460 = CIRCLE ( 'NONE', #57447, 47.09074272231896430 ) ;
#52461 = VERTEX_POINT ( 'NONE', #11689 ) ;
#52462 = EDGE_CURVE ( 'NONE', #3092, #8944, #43979, .T. ) ;
#52463 = CARTESIAN_POINT ( 'NONE',  ( -6.001507490154110336, 11.45906331631453234, -14.95933060264861858 ) ) ;
#52464 = EDGE_CURVE ( 'NONE', #29811, #32714, #7989, .T. ) ;
#52465 = DIRECTION ( 'NONE',  ( 0.000000000000000000, 0.000000000000000000, 1.000000000000000000 ) ) ;
#52466 = CARTESIAN_POINT ( 'NONE',  ( -6.077587904424778920, -16.13490349385120481, -10.51003856501195877 ) ) ;
#52467 = EDGE_CURVE ( 'NONE', #12616, #36851, #15551, .T. ) ;
#52468 = LINE ( 'NONE', #14597, #44082 ) ;
#52469 = B_SPLINE_CURVE_WITH_KNOTS ( 'NONE', 3,
 ( #35049, #6177, #30013, #15931, #15626, #35357, #34734, #7107, #49124, #16539, #59123, #21240, #11536, #25314, #49738, #6480, #25937, #25623, #44760, #2102, #1800, #45075, #16863, #54105, #59432 ),
 .UNSPECIFIED., .F., .F.,
 ( 4, 3, 3, 3, 3, 3, 3, 3, 4 ),
 ( 3.469446951953614189E-18, 0.0005656085177311399653, 0.001131215744874499839, 0.001696821861372763748, 0.002262427090022497284, 0.002828031679238744624, 0.003393635864401604429, 0.003977030878808131623, 0.004561030005651159000 ),
 .UNSPECIFIED. ) ;
#52470 = CARTESIAN_POINT ( 'NONE',  ( 0.7048096507298635682, 19.18768066167060127, 44.11842270945980715 ) ) ;
#52471 = CONICAL_SURFACE ( 'NONE', #44515, 43.92652462719577500, 1.486293639869522343 ) ;
#52472 = CARTESIAN_POINT ( 'NONE',  ( 2.299746137290198611, -34.31472549160143615, 35.02543293268731617 ) ) ;
#52473 = ORIENTED_EDGE ( 'NONE', *, *, #2414, .F. ) ;
#52474 = CARTESIAN_POINT ( 'NONE',  ( 4.691466044806103852, -44.46979273209137773, 3.249105306917663416 ) ) ;
#52475 = EDGE_CURVE ( 'NONE', #30590, #56316, #59570, .T. ) ;
#52476 = CARTESIAN_POINT ( 'NONE',  ( 1.834102595619085507, 44.02141804901769007, 1.520689912935467847 ) ) ;
#52477 = EDGE_LOOP ( 'NONE', ( #28598, #58504, #6321, #7495 ) ) ;
#52478 = DIRECTION ( 'NONE',  ( 0.000000000000000000, 1.000000000000000000, 0.000000000000000000 ) ) ;
#52479 = CARTESIAN_POINT ( 'NONE',  ( 0.5809828226811617480, -47.89273459658653564, -0.5448590168537535972 ) ) ;
#52480 = DIRECTION ( 'NONE',  ( 0.09835009131224567436, 0.9592125346408684194, 0.2650256080583793250 ) ) ;
#52481 = CARTESIAN_POINT ( 'NONE',  ( 0.3676999524040323597, -6.224421213753346116, -43.67158302462387098 ) ) ;
#52482 = ADVANCED_FACE ( 'NONE', ( #40520 ), #9333, .F. ) ;
#52483 = VERTEX_POINT ( 'NONE', #8199 ) ;
#52484 = B_SPLINE_CURVE_WITH_KNOTS ( 'NONE', 3,
 ( #56781, #52086, #14215, #47405 ),
 .UNSPECIFIED., .F., .F.,
 ( 4, 4 ),
 ( 0.000000000000000000, 0.005004948556313804434 ),
 .UNSPECIFIED. ) ;
#52485 = VERTEX_POINT ( 'NONE', #22624 ) ;
#52486 = CARTESIAN_POINT ( 'NONE',  ( 0.9754292580325127915, -31.46929222874847554, 27.67690577946956054 ) ) ;
#52487 = CARTESIAN_POINT ( 'NONE',  ( 0.9754402186311951217, -42.56545569314704380, -5.414674803234208689 ) ) ;
#52488 = CARTESIAN_POINT ( 'NONE',  ( 0.7764146366350248574, -2.458100050502026956, -46.84013469035808441 ) ) ;
#52489 = ORIENTED_EDGE ( 'NONE', *, *, #30542, .F. ) ;
#52490 = CARTESIAN_POINT ( 'NONE',  ( 0.6016118706126978299, 5.062064169927822377, -48.84594723335257527 ) ) ;
#52491 = ORIENTED_EDGE ( 'NONE', *, *, #22502, .T. ) ;
#52492 = CARTESIAN_POINT ( 'NONE',  ( 5.895881250540457863, -9.661888320804171926, 17.64016994489023915 ) ) ;
#52493 = CARTESIAN_POINT ( 'NONE',  ( 0.6029443199889047422, -25.45689510285765067, 41.99385828399795884 ) ) ;
#52494 =( BOUNDED_SURFACE ( )  B_SPLINE_SURFACE ( 3, 1, ( 
 ( #2899, #39930 ),
 ( #6338, #59294 ),
 ( #11711, #16396 ),
 ( #25476, #26101 ) ),
 .UNSPECIFIED., .F., .F., .F. ) 
 B_SPLINE_SURFACE_WITH_KNOTS ( ( 4, 4 ),
 ( 2, 2 ),
 ( 0.000000000000000000, 1.000000000000000000 ),
 ( 0.000000000000000000, 1.000000000000000000 ),
 .UNSPECIFIED. ) 
 GEOMETRIC_REPRESENTATION_ITEM ( )  RATIONAL_B_SPLINE_SURFACE ( (
 ( 1.000000000000000000, 1.000000000000000000),
 ( 0.9952954269826590483, 0.8620686068821307169),
 ( 0.9952954269826590483, 0.8620686068821307169),
 ( 1.000000000000000000, 1.000000000000000000) ) ) 
 REPRESENTATION_ITEM ( '' )  SURFACE ( )  );
#52495 = ORIENTED_EDGE ( 'NONE', *, *, #22187, .F. ) ;
#52496 = CARTESIAN_POINT ( 'NONE',  ( 0.5838002273316426072, -0.1361971433781400675, 47.89576566046788031 ) ) ;
#52497 = CARTESIAN_POINT ( 'NONE',  ( 0.1158516988532803382, -27.47246454191935428, 34.52833402910977156 ) ) ;
#52498 = CARTESIAN_POINT ( 'NONE',  ( 0.9752570700956804117, 26.30364510018356228, -33.90066715551942877 ) ) ;
#52499 = ORIENTED_EDGE ( 'NONE', *, *, #26465, .T. ) ;
#52500 = CARTESIAN_POINT ( 'NONE',  ( 0.5827357941260211671, -18.66407988912457938, -44.10984861950477409 ) ) ;
#52501 = CARTESIAN_POINT ( 'NONE',  ( 2.526464513654346433, 41.18424249084333866, -12.29060355381808201 ) ) ;
#52502 = CARTESIAN_POINT ( 'NONE',  ( 4.960156602257181468, -38.88108289790881855, 25.36362146861372935 ) ) ;
#52503 = CIRCLE ( 'NONE', #57491, 43.92652462719577500 ) ;
#52504 = CARTESIAN_POINT ( 'NONE',  ( 0.6023142530420679819, 29.07781306567101609, -38.32506243004162627 ) ) ;
#52505 = EDGE_CURVE ( 'NONE', #9955, #33012, #13428, .T. ) ;
#52506 = CARTESIAN_POINT ( 'NONE',  ( 0.1095718737110178698, 16.74012863188504596, -39.74279513315657653 ) ) ;
#52507 = EDGE_LOOP ( 'NONE', ( #60640, #9743 ) ) ;
#52508 = CARTESIAN_POINT ( 'NONE',  ( -5.995132425357893702, 14.95525565067274876, 11.46484027925372828 ) ) ;
#52509 =( BOUNDED_SURFACE ( )  B_SPLINE_SURFACE ( 3, 1, ( 
 ( #39700, #19655 ),
 ( #24965, #5212 ),
 ( #53443, #40015 ),
 ( #59067, #514 ) ),
 .UNSPECIFIED., .F., .F., .F. ) 
 B_SPLINE_SURFACE_WITH_KNOTS ( ( 4, 4 ),
 ( 2, 2 ),
 ( 0.000000000000000000, 1.000000000000000000 ),
 ( 0.000000000000000000, 1.000000000000000000 ),
 .UNSPECIFIED. ) 
 GEOMETRIC_REPRESENTATION_ITEM ( )  RATIONAL_B_SPLINE_SURFACE ( (
 ( 1.000000000000000000, 1.000000000000000000),
 ( 0.7223157951917480446, 0.9931996967497186413),
 ( 0.7223157951917480446, 0.9931996967497186413),
 ( 1.000000000000000000, 1.000000000000000000) ) ) 
 REPRESENTATION_ITEM ( '' )  SURFACE ( )  );
#52510 = CARTESIAN_POINT ( 'NONE',  ( 4.390527457369402420, -15.47389475202081321, 41.11865656647844958 ) ) ;
#52511 = ORIENTED_EDGE ( 'NONE', *, *, #15155, .T. ) ;
#52513 = CARTESIAN_POINT ( 'NONE',  ( 0.5806925824938502512, 16.34374012233117313, -43.95571090492413191 ) ) ;
#52512 =( BOUNDED_SURFACE ( )  B_SPLINE_SURFACE ( 3, 1, ( 
 ( #56187, #28306 ),
 ( #22688, #41818 ),
 ( #23308, #8571 ),
 ( #28004, #3866 ) ),
 .UNSPECIFIED., .F., .F., .F. ) 
 B_SPLINE_SURFACE_WITH_KNOTS ( ( 4, 4 ),
 ( 2, 2 ),
 ( 0.000000000000000000, 1.000000000000000000 ),
 ( 0.000000000000000000, 1.000000000000000000 ),
 .UNSPECIFIED. ) 
 GEOMETRIC_REPRESENTATION_ITEM ( )  RATIONAL_B_SPLINE_SURFACE ( (
 ( 1.000000000000000000, 1.000000000000000000),
 ( 0.9751682680413298332, 0.9999560080971552356),
 ( 0.9751682680413298332, 0.9999560080971552356),
 ( 1.000000000000000000, 1.000000000000000000) ) ) 
 REPRESENTATION_ITEM ( '' )  SURFACE ( )  );
#52514 = CARTESIAN_POINT ( 'NONE',  ( 0.8554163680231816613, 46.61139063278402972, 5.346376005279853239 ) ) ;
#52515 = CARTESIAN_POINT ( 'NONE',  ( 2.618530812446111078, -33.90288491188655229, -32.56257336037148775 ) ) ;
#52516 = LINE ( 'NONE', #9605, #5956 ) ;
#52517 = CARTESIAN_POINT ( 'NONE',  ( -6.015611763856276717, 9.416239407363303116, 16.32183393015600004 ) ) ;
#52518 = DIRECTION ( 'NONE',  ( -1.000000000000000000, -0.000000000000000000, -0.000000000000000000 ) ) ;
#52519 = CARTESIAN_POINT ( 'NONE',  ( 51.18913332871307631, 15.28638276972803034, 2.564700684161830502 ) ) ;
#52520 = DIRECTION ( 'NONE',  ( -8.743006318923107756E-16, 0.8294993580478400297, -0.5585076678061109412 ) ) ;
#52521 = CARTESIAN_POINT ( 'NONE',  ( 0.6009452777970409887, 47.75105029762383424, 5.846392105360695091 ) ) ;
#52522 = CARTESIAN_POINT ( 'NONE',  ( 2.643462169533600914, -46.73820883660214065, 11.09243630552451876 ) ) ;
#52523 = AXIS2_PLACEMENT_3D ( 'NONE', #30012, #29393, #15012 ) ;
#52524 = CARTESIAN_POINT ( 'NONE',  ( 0.2224561200757616264, -26.84793396061007087, 33.74134531362587097 ) ) ;
#52526 = ORIENTED_EDGE ( 'NONE', *, *, #26670, .F. ) ;
#52525 = CARTESIAN_POINT ( 'NONE',  ( 0.6001305935487315502, 23.60027211631829402, -41.92422178329146476 ) ) ;
#52527 = ORIENTED_EDGE ( 'NONE', *, *, #12879, .T. ) ;
#52528 = VECTOR ( 'NONE', #40485, 1000.000000000000114 ) ;
#52529 = CARTESIAN_POINT ( 'NONE',  ( 0.9762797500689124330, -1.905951756780688733, 41.86516610604248712 ) ) ;
#52530 = CARTESIAN_POINT ( 'NONE',  ( 5.896278296736517710, -19.93266788971478221, 2.686211163091445808 ) ) ;
#52531 = VECTOR ( 'NONE', #40822, 1000.000000000000000 ) ;
#52532 = CARTESIAN_POINT ( 'NONE',  ( 1.000110580585050979, -17.04223752418473481, -38.28811333744679501 ) ) ;
#52533 = CARTESIAN_POINT ( 'NONE',  ( 5.959547316686252039, -20.35048796920735015, -2.675599016784462769 ) ) ;
#52534 = CARTESIAN_POINT ( 'NONE',  ( 0.7762777257811902532, -11.53708189756908098, -46.49451973287614237 ) ) ;
#52535 = VERTEX_POINT ( 'NONE', #32965 ) ;
#52536 = EDGE_CURVE ( 'NONE', #39191, #8264, #41447, .T. ) ;
#52537 = CARTESIAN_POINT ( 'NONE',  ( 0.8560838555295223751, -38.14845555156087187, 27.29593693413575295 ) ) ;
#52538 = CARTESIAN_POINT ( 'NONE',  ( 0.8744876279028306332, -19.05609938969034545, 45.24616145519679122 ) ) ;
#52539 = B_SPLINE_CURVE_WITH_KNOTS ( 'NONE', 3,
 ( #55792, #2861, #60184, #46123, #27608, #17295, #3169, #22298, #41427, #3471, #60794, #44139, #5547 ),
 .UNSPECIFIED., .F., .F.,
 ( 4, 3, 3, 3, 4 ),
 ( 0.002715792992282060631, 0.002828031679238745925, 0.003393635864401604862, 0.003977030878808131623, 0.004561030005651158133 ),
 .UNSPECIFIED. ) ;
#52540 = LINE ( 'NONE', #44119, #37810 ) ;
#52541 = ORIENTED_EDGE ( 'NONE', *, *, #46846, .T. ) ;
#52542 = EDGE_CURVE ( 'NONE', #39332, #19355, #37197, .T. ) ;
#52543 = CARTESIAN_POINT ( 'NONE',  ( 0.5837799406558226156, 43.21036104660473143, 18.22383735109779224 ) ) ;
#52544 = CARTESIAN_POINT ( 'NONE',  ( 0.5817217712918331118, -24.84894824081227682, -39.77140587575206609 ) ) ;
#52545 = ORIENTED_EDGE ( 'NONE', *, *, #8672, .T. ) ;
#52546 = EDGE_LOOP ( 'NONE', ( #38041, #6930, #35964, #26415 ) ) ;
#52547 = FACE_OUTER_BOUND ( 'NONE', #1381, .T. ) ;
#52548 = EDGE_CURVE ( 'NONE', #13205, #36503, #47067, .T. ) ;
#52549 = CARTESIAN_POINT ( 'NONE',  ( 2.299746137290199943, 43.60338919182262885, -22.42823641467567342 ) ) ;
#52550 = B_SPLINE_CURVE_WITH_KNOTS ( 'NONE', 3,
 ( #53816, #10946, #6191, #12804, #50980, #12488, #55988, #7756, #26569, #2438, #3059, #54746, #22188, #45091, #31581, #31898, #36925, #40390, #11885 ),
 .UNSPECIFIED., .F., .F.,
 ( 4, 3, 3, 3, 3, 3, 4 ),
 ( 1.250973872328959318E-17, 0.0002724573126191757013, 0.0004086839781548398578, 0.0005449106435901728126, 0.0006811373090491394233, 0.0008459866663933642787, 0.001010840725717206644 ),
 .UNSPECIFIED. ) ;
#52551 = ORIENTED_EDGE ( 'NONE', *, *, #9547, .T. ) ;
#52552 = DIRECTION ( 'NONE',  ( -1.000000000000000000, -0.000000000000000000, -0.000000000000000000 ) ) ;
#52553 = CARTESIAN_POINT ( 'NONE',  ( 5.896782393890504181, 18.99788783847851548, 6.603510017755907846 ) ) ;
#52554 = CARTESIAN_POINT ( 'NONE',  ( 3.238018933889920792, -5.886379020808710116, 12.03154330877946876 ) ) ;
#52555 = CARTESIAN_POINT ( 'NONE',  ( 0.5838002273316440505, -38.08117724016823757, 29.04904228829596491 ) ) ;
#52556 = EDGE_CURVE ( 'NONE', #16923, #47251, #2399, .T. ) ;
#52557 = ORIENTED_EDGE ( 'NONE', *, *, #38628, .T. ) ;
#52558 = B_SPLINE_CURVE_WITH_KNOTS ( 'NONE', 3,
 ( #4794, #24548, #23935, #48054, #33044, #57412 ),
 .UNSPECIFIED., .F., .F.,
 ( 4, 2, 4 ),
 ( 9.543442895606953578E-18, 0.0002291978881530155367, 0.0004583957763060215324 ),
 .UNSPECIFIED. ) ;
#52559 = CARTESIAN_POINT ( 'NONE',  ( 0.9790724872846779947, -6.930766400444295705, -41.33158219913587317 ) ) ;
#52560 = VERTEX_POINT ( 'NONE', #4102 ) ;
#52561 = CARTESIAN_POINT ( 'NONE',  ( -6.063463321072276813, 17.84349906452544943, -7.240855861964748286 ) ) ;
#52562 = B_SPLINE_CURVE_WITH_KNOTS ( 'NONE', 3,
 ( #52098, #57099, #33337, #52407 ),
 .UNSPECIFIED., .F., .F.,
 ( 4, 4 ),
 ( 0.000000000000000000, 0.004447772540403838876 ),
 .UNSPECIFIED. ) ;
#52563 = CONICAL_SURFACE ( 'NONE', #34564, 42.08604991992415023, 1.569615340895231137 ) ;
#52564 = VERTEX_POINT ( 'NONE', #37989 ) ;
#52565 = VERTEX_POINT ( 'NONE', #51110 ) ;
#52566 = CARTESIAN_POINT ( 'NONE',  ( 0.6029443449137436017, -42.76684749053210055, -24.13578864891102072 ) ) ;
#52567 = CARTESIAN_POINT ( 'NONE',  ( 0.9788927965476035276, -37.34015262922740419, 19.02760137951648645 ) ) ;
#52568 = AXIS2_PLACEMENT_3D ( 'NONE', #17059, #55545, #60244 ) ;
#52569 = CARTESIAN_POINT ( 'NONE',  ( 0.9754402186311945666, 34.15542855230937391, 25.97197377940566554 ) ) ;
#52570 = CARTESIAN_POINT ( 'NONE',  ( 4.975801465491695552, 39.51822597168496287, -27.09127437476339395 ) ) ;
#52571 = ORIENTED_EDGE ( 'NONE', *, *, #60880, .F. ) ;
#52572 = CARTESIAN_POINT ( 'NONE',  ( 0.5782707292762423457, 11.57561326132651836, 45.45042938556048995 ) ) ;
#52573 = CARTESIAN_POINT ( 'NONE',  ( 0.7764146366350269668, -46.13398395504711402, -8.467348941942809404 ) ) ;
#52574 = CARTESIAN_POINT ( 'NONE',  ( 4.967162193818130511, 3.259922920618364639, -42.96271701169381885 ) ) ;
#52575 = VECTOR ( 'NONE', #3488, 1000.000000000000000 ) ;
#52576 = ORIENTED_EDGE ( 'NONE', *, *, #18746, .T. ) ;
#52577 = ORIENTED_EDGE ( 'NONE', *, *, #13530, .T. ) ;
#52578 = CARTESIAN_POINT ( 'NONE',  ( 0.5997462898726536595, -49.10477184366966696, -0.5225058138009923692 ) ) ;
#52579 = CARTESIAN_POINT ( 'NONE',  ( 0.7246131072078558777, 47.57651137777903472, 7.091231226024960144 ) ) ;
#52580 = DIRECTION ( 'NONE',  ( -1.000000000000000000, -3.135800716341471541E-16, -1.298891185607920445E-16 ) ) ;
#52581 = ADVANCED_FACE ( 'NONE', ( #28239, #14168 ), #17937, .T. ) ;
#52582 = CARTESIAN_POINT ( 'NONE',  ( -6.057079549204054558, -17.35362438320621337, -8.347631512370986329 ) ) ;
#52583 = CARTESIAN_POINT ( 'NONE',  ( 1.227938101723756947, -26.79402671879305231, -33.52879263017890565 ) ) ;
#52584 = ORIENTED_EDGE ( 'NONE', *, *, #30683, .F. ) ;
#52585 = ORIENTED_EDGE ( 'NONE', *, *, #19800, .T. ) ;
#52586 = CARTESIAN_POINT ( 'NONE',  ( 100.0000507999999968, 0.000000000000000000, 8.000000000000000000 ) ) ;
#52587 = CARTESIAN_POINT ( 'NONE',  ( 4.060580049360325461, 42.63592134878009432, -10.66048334269353859 ) ) ;
#52588 = CARTESIAN_POINT ( 'NONE',  ( -6.078726893082806448, -16.13637198556892827, -10.50768958487384808 ) ) ;
#52589 = CARTESIAN_POINT ( 'NONE',  ( 4.956653778116988818, -45.35992544608517818, -15.97476558431931082 ) ) ;
#52590 = CARTESIAN_POINT ( 'NONE',  ( 0.5987334363312686314, 37.78232946234383860, -31.36970651553788159 ) ) ;
#52591 =( NAMED_UNIT ( * ) SI_UNIT ( $, .STERADIAN. ) SOLID_ANGLE_UNIT ( ) );
#52592 = DIRECTION ( 'NONE',  ( 0.000000000000000000, 0.000000000000000000, -1.000000000000000000 ) ) ;
#52593 =( BOUNDED_SURFACE ( )  B_SPLINE_SURFACE ( 3, 1, ( 
 ( #8592, #23030 ),
 ( #61213, #8919 ),
 ( #18336, #45604 ),
 ( #2656, #33055 ) ),
 .UNSPECIFIED., .F., .F., .F. ) 
 B_SPLINE_SURFACE_WITH_KNOTS ( ( 4, 4 ),
 ( 2, 2 ),
 ( 0.000000000000000000, 1.000000000000000000 ),
 ( 0.000000000000000000, 1.000000000000000000 ),
 .UNSPECIFIED. ) 
 GEOMETRIC_REPRESENTATION_ITEM ( )  RATIONAL_B_SPLINE_SURFACE ( (
 ( 1.000000000000000000, 1.000000000000000000),
 ( 0.9732289882329797637, 0.9999525324661233672),
 ( 0.9732289882329797637, 0.9999525324661233672),
 ( 1.000000000000000000, 1.000000000000000000) ) ) 
 REPRESENTATION_ITEM ( '' )  SURFACE ( )  );
#52594 = EDGE_LOOP ( 'NONE', ( #34291, #965, #764, #4150 ) ) ;
#52595 = DIRECTION ( 'NONE',  ( 0.09722883295013592941, 0.9783250423059141054, 0.1828296082156442293 ) ) ;
#52596 = CARTESIAN_POINT ( 'NONE',  ( 0.8753041380234471980, 27.35839019124358984, 40.77568900725831469 ) ) ;
#52597 = DIRECTION ( 'NONE',  ( 0.07500201931887538753, 0.8960136144483816789, -0.4376463181854017281 ) ) ;
#52598 = CARTESIAN_POINT ( 'NONE',  ( 0.6845945791218034371, -46.73791075327830669, -3.996776092369579203 ) ) ;
#52599 = CARTESIAN_POINT ( 'NONE',  ( 3.238931869106854489, 35.19033040238034005, 24.69728751010298495 ) ) ;
#52600 = CARTESIAN_POINT ( 'NONE',  ( 0.9775691876210967912, -34.76360227320881791, 23.40567593512611566 ) ) ;
#52601 = DIRECTION ( 'NONE',  ( 0.09835009131224567436, -0.5996571005210353800, -0.7941905447268796658 ) ) ;
#52602 = ORIENTED_EDGE ( 'NONE', *, *, #60193, .F. ) ;
#52603 = EDGE_CURVE ( 'NONE', #450, #10386, #39467, .T. ) ;
#52604 = CARTESIAN_POINT ( 'NONE',  ( 3.673643420401899728, 2.497823135841253706, -0.2484800633749943699 ) ) ;
#52605 = FACE_OUTER_BOUND ( 'NONE', #32766, .T. ) ;
#52606 = AXIS2_PLACEMENT_3D ( 'NONE', #43047, #19536, #33945 ) ;
#52607 = FACE_OUTER_BOUND ( 'NONE', #55385, .T. ) ;
#52608 = CARTESIAN_POINT ( 'NONE',  ( 0.3676999524040366896, 40.09552319080398775, 18.39292264373822405 ) ) ;
#52609 = CARTESIAN_POINT ( 'NONE',  ( 1.231276596079887931, 40.64579686208652731, 10.25650859035686757 ) ) ;
#52610 = VERTEX_POINT ( 'NONE', #56119 ) ;
#52611 = ADVANCED_FACE ( 'NONE', ( #42368 ), #9924, .F. ) ;
#52612 = CARTESIAN_POINT ( 'NONE',  ( 0.9756008150404614776, -37.08855330282513307, 21.57722292874444392 ) ) ;
#52613 = CONICAL_SURFACE ( 'NONE', #36639, 42.08604991992415023, 1.569615340895231137 ) ;
#52614 = CARTESIAN_POINT ( 'NONE',  ( 3.680974057930773924, -44.99871514631803393, 16.63696281867780868 ) ) ;
#52615 = EDGE_CURVE ( 'NONE', #37408, #50941, #20436, .T. ) ;
#52616 = CARTESIAN_POINT ( 'NONE',  ( 0.9754292580325132356, 38.35198880093447116, 16.89533728331584328 ) ) ;
#52617 = ORIENTED_EDGE ( 'NONE', *, *, #46004, .F. ) ;
#52618 = CARTESIAN_POINT ( 'NONE',  ( 0.8760168074887076939, 47.80016357497242296, 5.394043284319666398 ) ) ;
#52619 = CARTESIAN_POINT ( 'NONE',  ( 0.8560838555295158248, 39.88643293834648063, 24.68694597426990001 ) ) ;
#52620 = EDGE_LOOP ( 'NONE', ( #30379, #36834, #39800, #15903 ) ) ;
#52621 = AXIS2_PLACEMENT_3D ( 'NONE', #61301, #17486, #18417 ) ;
#52622 = CARTESIAN_POINT ( 'NONE',  ( 0.5980271706414734822, 16.30306832862545008, -46.32773689609533818 ) ) ;
#52623 = VERTEX_POINT ( 'NONE', #8827 ) ;
#52624 = DIRECTION ( 'NONE',  ( -1.000000000000000000, -0.000000000000000000, -0.000000000000000000 ) ) ;
#52625 = ORIENTED_EDGE ( 'NONE', *, *, #34083, .T. ) ;
#52626 = DIRECTION ( 'NONE',  ( -0.07439287786467650709, -0.2708295585865000410, -0.9597484305373220614 ) ) ;
#52627 = CARTESIAN_POINT ( 'NONE',  ( 10.00000000000001599, -54.69470952477976766, 58.44237546506786884 ) ) ;
#52628 = ORIENTED_EDGE ( 'NONE', *, *, #30706, .F. ) ;
#52629 = CARTESIAN_POINT ( 'NONE',  ( 0.9754292589017206083, 24.38796673385399316, -34.08158660455394084 ) ) ;
#52630 = EDGE_CURVE ( 'NONE', #30850, #37991, #9543, .T. ) ;
#52631 = ORIENTED_EDGE ( 'NONE', *, *, #50077, .T. ) ;
#52632 = CARTESIAN_POINT ( 'NONE',  ( 0.8751705887134423323, -34.63284514348608667, 33.37254303619495488 ) ) ;
#52633 = B_SPLINE_CURVE_WITH_KNOTS ( 'NONE', 3,
 ( #13088, #17777, #50052, #22166, #7736, #32184 ),
 .UNSPECIFIED., .F., .F.,
 ( 4, 2, 4 ),
 ( 1.734723475976807094E-18, 0.0002447193893791697081, 0.0004894387787583376814 ),
 .UNSPECIFIED. ) ;
#52634 = CARTESIAN_POINT ( 'NONE',  ( 4.967162193818130511, 43.02067033766019932, -2.375726030842729486 ) ) ;
#52635 = B_SPLINE_CURVE_WITH_KNOTS ( 'NONE', 3,
 ( #48366, #422, #38684, #57426, #23334, #14873 ),
 .UNSPECIFIED., .F., .F.,
 ( 4, 2, 4 ),
 ( 1.553784678811103104E-17, 0.0002293755540694292585, 0.0004587511081388430129 ),
 .UNSPECIFIED. ) ;
#52636 = ORIENTED_EDGE ( 'NONE', *, *, #22281, .T. ) ;
#52637 = CARTESIAN_POINT ( 'NONE',  ( 4.962356264823603702, 41.96072444189417183, -3.245489512195726789 ) ) ;
#52638 = CARTESIAN_POINT ( 'NONE',  ( 4.549368137175248350, 42.82045902618768451, 3.018832571116707442 ) ) ;
#52639 = CARTESIAN_POINT ( 'NONE',  ( -6.077587904424778920, 15.43577113102525189, 11.51229738082446552 ) ) ;
#52640 = ORIENTED_EDGE ( 'NONE', *, *, #21700, .T. ) ;
#52641 = CARTESIAN_POINT ( 'NONE',  ( -2.739355103387248747, 1.694972997839557793, 14.83154184458284419 ) ) ;
#52642 = CARTESIAN_POINT ( 'NONE',  ( 0.1147471544378675934, -17.57640881104399355, 40.47248499635647789 ) ) ;
#52643 = ORIENTED_EDGE ( 'NONE', *, *, #36306, .T. ) ;
#52644 = CARTESIAN_POINT ( 'NONE',  ( 0.5797568665920720399, 46.38942905901759417, -6.873585685815319479 ) ) ;
#52645 = ORIENTED_EDGE ( 'NONE', *, *, #47788, .T. ) ;
#52646 = CARTESIAN_POINT ( 'NONE',  ( 0.6001305935487315502, -46.33281397023053927, -12.95698906763794334 ) ) ;
#52647 = FACE_OUTER_BOUND ( 'NONE', #30428, .T. ) ;
#52648 = VERTEX_POINT ( 'NONE', #34195 ) ;
#52649 = CARTESIAN_POINT ( 'NONE',  ( 0.9785694773339257413, -34.42478712511277195, -23.90124342174149774 ) ) ;
#52650 = CARTESIAN_POINT ( 'NONE',  ( 0.1157991065609915854, 25.31090088263283278, -36.14278160362363934 ) ) ;
#52651 = CARTESIAN_POINT ( 'NONE',  ( -1.500000000000001332, 0.000000000000000000, 0.000000000000000000 ) ) ;
#52652 = AXIS2_PLACEMENT_3D ( 'NONE', #20543, #39056, #43445 ) ;
#52653 = AXIS2_PLACEMENT_3D ( 'NONE', #27144, #61560, #23373 ) ;
#52654 = VERTEX_POINT ( 'NONE', #25085 ) ;
#52655 = LINE ( 'NONE', #39527, #40987 ) ;
#52656 = AXIS2_PLACEMENT_3D ( 'NONE', #35881, #49965, #30847 ) ;
#52657 = ADVANCED_FACE ( 'NONE', ( #39216 ), #57963, .F. ) ;
#52658 = CARTESIAN_POINT ( 'NONE',  ( 5.894904586330512508, -15.78536547177689364, -12.46401416013623376 ) ) ;
#52659 = CARTESIAN_POINT ( 'NONE',  ( 0.5782707292762442330, -25.84399470232805385, 39.13852694639462015 ) ) ;
#52660 = B_SPLINE_CURVE_WITH_KNOTS ( 'NONE', 3,
 ( #41825, #13614, #18316, #46511, #2953, #3562 ),
 .UNSPECIFIED., .F., .F.,
 ( 4, 2, 4 ),
 ( 0.000000000000000000, 0.0002291966416970790785, 0.0004583932833941581570 ),
 .UNSPECIFIED. ) ;
#52661 = EDGE_CURVE ( 'NONE', #58092, #48936, #40206, .T. ) ;
#52662 = CARTESIAN_POINT ( 'NONE',  ( 4.956445790444004018, -43.14021684453488348, -18.88014143872194950 ) ) ;
#52663 = CARTESIAN_POINT ( 'NONE',  ( 2.706805983486679779, -8.653164499869760107, -43.14972604151675029 ) ) ;
#52664 = EDGE_CURVE ( 'NONE', #19843, #15229, #25475, .T. ) ;
#52665 = CIRCLE ( 'NONE', #10657, 47.91270532121795611 ) ;
#52666 = DIRECTION ( 'NONE',  ( 0.07439287786467665975, 0.6174937095821756428, -0.7830499462674492817 ) ) ;
#52667 = CARTESIAN_POINT ( 'NONE',  ( 4.303969348037246512, -2.158280495710544589, 48.06163817123225357 ) ) ;
#52668 = DIRECTION ( 'NONE',  ( 0.09835009131224552170, 0.7091251765523974848, 0.6981896185982745529 ) ) ;
#52669 = CARTESIAN_POINT ( 'NONE',  ( 0.6017667736363750963, 48.10631678344240925, 0.3491025323182196938 ) ) ;
#52670 = CARTESIAN_POINT ( 'NONE',  ( -2.708315649062916552, 11.44805714186571777, -9.116606751444216172 ) ) ;
#52671 = CARTESIAN_POINT ( 'NONE',  ( 4.956653778116973719, 27.17045123668471973, 39.67974989265048436 ) ) ;
#52672 = AXIS2_PLACEMENT_3D ( 'NONE', #6120, #25261, #53138 ) ;
#52673 = CARTESIAN_POINT ( 'NONE',  ( 4.962356264823608143, 1.841560470688809792, -42.04574000888963781 ) ) ;
#52674 = CARTESIAN_POINT ( 'NONE',  ( 0.9762797500689124330, 10.20671408565980975, 40.64662068068264489 ) ) ;
#52675 = CARTESIAN_POINT ( 'NONE',  ( 0.7048096507298579061, 47.80151517212785706, -5.442192462018969223 ) ) ;
#52676 = B_SPLINE_CURVE_WITH_KNOTS ( 'NONE', 3,
 ( #10871, #58749, #35294, #15877, #34994, #1432 ),
 .UNSPECIFIED., .F., .F.,
 ( 4, 2, 4 ),
 ( 9.885284284422817346E-18, 0.0002448709889506582409, 0.0004897419779013066155 ),
 .UNSPECIFIED. ) ;
#52677 = EDGE_CURVE ( 'NONE', #29523, #4, #4301, .T. ) ;
#52678 = CARTESIAN_POINT ( 'NONE',  ( 4.956445790443996025, 14.46717203539371610, 44.81337951368942640 ) ) ;
#52679 = ORIENTED_EDGE ( 'NONE', *, *, #61298, .T. ) ;
#52680 = B_SPLINE_CURVE_WITH_KNOTS ( 'NONE', 3,
 ( #60877, #17997, #51169, #22068, #37113, #60253 ),
 .UNSPECIFIED., .F., .F.,
 ( 4, 2, 4 ),
 ( 1.015220885719448636E-17, 0.0002291978881530140188, 0.0004583957763060178461 ),
 .UNSPECIFIED. ) ;
#52681 = CARTESIAN_POINT ( 'NONE',  ( 0.1129192098497455998, -44.12161472487017733, -0.4846667466135657909 ) ) ;
#52682 = DIRECTION ( 'NONE',  ( 1.000000000000000000, 0.000000000000000000, 0.000000000000000000 ) ) ;
#52684 = EDGE_CURVE ( 'NONE', #23453, #8473, #60480, .T. ) ;
#52683 = DIRECTION ( 'NONE',  ( 0.8191520442889896891, 0.000000000000000000, 0.5735764363510490460 ) ) ;
#52685 = EDGE_LOOP ( 'NONE', ( #21203, #9268, #15438, #55617 ) ) ;
#52686 = CARTESIAN_POINT ( 'NONE',  ( 0.9754402186311951217, 5.786576363453547422, 42.51649392388753057 ) ) ;
#52687 = CARTESIAN_POINT ( 'NONE',  ( 3.270143674763207553, -11.71453292426874171, -7.080034332678387443 ) ) ;
#52688 = ADVANCED_FACE ( 'NONE', ( #9751 ), #7389, .F. ) ;
#52689 = EDGE_LOOP ( 'NONE', ( #57571, #17212, #21509, #298 ) ) ;
#52690 = ORIENTED_EDGE ( 'NONE', *, *, #11279, .T. ) ;
#52691 = CARTESIAN_POINT ( 'NONE',  ( 0.5809828226811553087, 46.11980934799357357, -12.92184523170154620 ) ) ;
#52692 = VECTOR ( 'NONE', #10307, 1000.000000000000114 ) ;
#52693 = ORIENTED_EDGE ( 'NONE', *, *, #58400, .T. ) ;
#52694 = DIRECTION ( 'NONE',  ( 0.000000000000000000, 0.000000000000000000, 1.000000000000000000 ) ) ;
#52695 = VECTOR ( 'NONE', #59203, 1000.000000000000114 ) ;
#52696 = ORIENTED_EDGE ( 'NONE', *, *, #30109, .T. ) ;
#52697 = ORIENTED_EDGE ( 'NONE', *, *, #50279, .F. ) ;
#52698 = CARTESIAN_POINT ( 'NONE',  ( 0.5836750258453341500, -12.22088356912694884, -46.31062999473600428 ) ) ;
#52699 = ORIENTED_EDGE ( 'NONE', *, *, #2787, .T. ) ;
#52700 = CARTESIAN_POINT ( 'NONE',  ( 1.227938101723747621, 30.94118573761354440, -29.74462687941193551 ) ) ;
#52701 = CARTESIAN_POINT ( 'NONE',  ( -5.995132425357893702, 11.47834865841095642, 14.94489030678155572 ) ) ;
#52702 = EDGE_CURVE ( 'NONE', #28193, #4544, #48379, .T. ) ;
#52703 = B_SPLINE_CURVE_WITH_KNOTS ( 'NONE', 3,
 ( #630, #30374, #29454, #20687, #54474, #49488, #48565, #1867, #10989, #5620, #20081, #19770, #20993, #59188, #30072, #11603 ),
 .UNSPECIFIED., .F., .F.,
 ( 4, 3, 3, 3, 3, 4 ),
 ( 9.813676791237319219E-18, 0.0002724568934985570649, 0.0004086836638483779785, 0.0005449104342063629345, 0.0008173270854453619028, 0.001089761613562689442 ),
 .UNSPECIFIED. ) ;
#52704 = DIRECTION ( 'NONE',  ( -0.000000000000000000, -0.000000000000000000, 1.000000000000000000 ) ) ;
#52705 = EDGE_LOOP ( 'NONE', ( #16828, #28750, #23383, #26135 ) ) ;
#52706 = CARTESIAN_POINT ( 'NONE',  ( 0.1084644655670281566, 0.3976617192052402938, 43.12277244437006374 ) ) ;
#52707 = B_SPLINE_CURVE_WITH_KNOTS ( 'NONE', 3,
 ( #36326, #56627, #9021, #60388 ),
 .UNSPECIFIED., .F., .F.,
 ( 4, 4 ),
 ( 0.000000000000000000, 0.004446090762761361649 ),
 .UNSPECIFIED. ) ;
#52708 =( BOUNDED_SURFACE ( )  B_SPLINE_SURFACE ( 3, 1, ( 
 ( #23081, #32479 ),
 ( #51875, #42211 ),
 ( #46905, #13075 ),
 ( #22152, #56575 ) ),
 .UNSPECIFIED., .F., .F., .F. ) 
 B_SPLINE_SURFACE_WITH_KNOTS ( ( 4, 4 ),
 ( 2, 2 ),
 ( 0.000000000000000000, 1.000000000000000000 ),
 ( 0.000000000000000000, 1.000000000000000000 ),
 .UNSPECIFIED. ) 
 GEOMETRIC_REPRESENTATION_ITEM ( )  RATIONAL_B_SPLINE_SURFACE ( (
 ( 1.000000000000000000, 1.000000000000000000),
 ( 0.7269869731126821222, 0.9931720237060910339),
 ( 0.7269869731126821222, 0.9931720237060910339),
 ( 1.000000000000000000, 1.000000000000000000) ) ) 
 REPRESENTATION_ITEM ( '' )  SURFACE ( )  );
#52709 = CARTESIAN_POINT ( 'NONE',  ( 0.9752132459055858904, -34.18286753639623043, -25.93579301218392530 ) ) ;
#52710 = ORIENTED_EDGE ( 'NONE', *, *, #32483, .T. ) ;
#52711 = VECTOR ( 'NONE', #19505, 1000.000000000000114 ) ;
#52712 = ORIENTED_EDGE ( 'NONE', *, *, #41906, .F. ) ;
#52713 = CARTESIAN_POINT ( 'NONE',  ( 5.958863334805807099, 18.96276366205793806, -7.855954700275424862 ) ) ;
#52714 = VERTEX_POINT ( 'NONE', #57642 ) ;
#52715 = CARTESIAN_POINT ( 'NONE',  ( 0.6026112563231247332, 46.55052957697731131, 15.63934752498222913 ) ) ;
#52716 = CARTESIAN_POINT ( 'NONE',  ( 0.9972139404380300221, -41.27214627875016362, 11.74016833743905863 ) ) ;
#52717 = CARTESIAN_POINT ( 'NONE',  ( -15.25000000000000711, -2.688986455804108555, -9.952330921218299798E-16 ) ) ;
#52718 = CARTESIAN_POINT ( 'NONE',  ( 0.5806925824938502512, 40.06810415365508504, -24.36738377166110325 ) ) ;
#52719 = ORIENTED_EDGE ( 'NONE', *, *, #56245, .F. ) ;
#52720 = DIRECTION ( 'NONE',  ( -1.000000000000000000, -0.000000000000000000, -0.000000000000000000 ) ) ;
#52721 = DIRECTION ( 'NONE',  ( 0.000000000000000000, 0.000000000000000000, -1.000000000000000000 ) ) ;
#52722 = EDGE_LOOP ( 'NONE', ( #27661, #55005 ) ) ;
#52723 = CARTESIAN_POINT ( 'NONE',  ( 5.896782393890504181, -19.93422257774822626, -2.674482585249919442 ) ) ;
#52724 = CARTESIAN_POINT ( 'NONE',  ( -6.016489644550736315, 18.19999694163070814, -4.881234076340183137 ) ) ;
#52725 = CARTESIAN_POINT ( 'NONE',  ( 0.6016118706126978299, -35.03315395170277924, -34.41263109644804530 ) ) ;
#52726 = ORIENTED_EDGE ( 'NONE', *, *, #11036, .T. ) ;
#52727 = B_SPLINE_CURVE_WITH_KNOTS ( 'NONE', 3,
 ( #3652, #12172, #30951, #26240 ),
 .UNSPECIFIED., .F., .F.,
 ( 4, 4 ),
 ( 0.000000000000000000, 0.004041751736740996880 ),
 .UNSPECIFIED. ) ;
#52728 = VERTEX_POINT ( 'NONE', #38910 ) ;
#52729 = CARTESIAN_POINT ( 'NONE',  ( 5.901463166500146684, -15.77541139567720130, 12.47614786854398083 ) ) ;
#52730 = CARTESIAN_POINT ( 'NONE',  ( 0.8560838555295223751, 43.53454501559562573, 17.46757637357886850 ) ) ;
#52731 = EDGE_CURVE ( 'NONE', #7613, #51786, #10469, .T. ) ;
#52732 = DIRECTION ( 'NONE',  ( 1.000000000000000000, 0.000000000000000000, 0.000000000000000000 ) ) ;
#52733 = CARTESIAN_POINT ( 'NONE',  ( 0.8760168074887076939, -24.81951362746049838, -41.20610493656901241 ) ) ;
#52734 = CARTESIAN_POINT ( 'NONE',  ( 0.5804410086790514622, -44.12183670707857175, -15.89916279082930295 ) ) ;
#52735 = EDGE_CURVE ( 'NONE', #22979, #10045, #17767, .T. ) ;
#52736 = CARTESIAN_POINT ( 'NONE',  ( 0.9749527285493325701, -42.57770849153627069, 5.317382389863026582 ) ) ;
#52737 = CARTESIAN_POINT ( 'NONE',  ( 0.2230388203127650348, -17.20066002792390236, -39.54016926433967427 ) ) ;
#52738 = CARTESIAN_POINT ( 'NONE',  ( 0.6039202388192953519, 22.86846745447336460, 43.45799016444136953 ) ) ;
#52739 = VECTOR ( 'NONE', #59288, 1000.000000000000114 ) ;
#52740 = EDGE_CURVE ( 'NONE', #16844, #34863, #3531, .T. ) ;
#52741 = CARTESIAN_POINT ( 'NONE',  ( -5.995132425357893702, -13.33084941932916756, 13.31880955509722497 ) ) ;
#52742 = ADVANCED_FACE ( 'NONE', ( #11006 ), #33512, .F. ) ;
#52743 = CARTESIAN_POINT ( 'NONE',  ( 0.5980894510889448457, -44.17723055703940105, -19.05812566676491215 ) ) ;
#52744 = ORIENTED_EDGE ( 'NONE', *, *, #21194, .T. ) ;
#52745 = AXIS2_PLACEMENT_3D ( 'NONE', #7720, #22145, #37821 ) ;
#52746 = EDGE_CURVE ( 'NONE', #21737, #4022, #26747, .T. ) ;
#52747 = DIRECTION ( 'NONE',  ( -1.850371707708593823E-16, 1.000000000000000000, 0.000000000000000000 ) ) ;
#52748 = CARTESIAN_POINT ( 'NONE',  ( 0.1104177457020372732, -34.21590786699023568, -26.24862037251720537 ) ) ;
#52749 = CARTESIAN_POINT ( 'NONE',  ( 0.5797568599927142019, -45.82673081884099986, -9.956708850242389275 ) ) ;
#52750 = CARTESIAN_POINT ( 'NONE',  ( 2.526552050251864134, 25.19159344346121543, 34.82218744039913361 ) ) ;
#52751 = CARTESIAN_POINT ( 'NONE',  ( 0.6028618097248863439, -23.90242650600305296, 41.74935807801004017 ) ) ;
#52752 = CARTESIAN_POINT ( 'NONE',  ( 0.6008122571543323964, 32.69143329158589495, -36.64457312900650976 ) ) ;
#52753 = ITEM_DEFINED_TRANSFORMATION ( 'NONE', 'NONE', #27875,  #14677 ) ;
#52754 = CARTESIAN_POINT ( 'NONE',  ( 4.549368137175248350, -42.06008734272390370, -8.582197505784284530 ) ) ;
#52755 = CARTESIAN_POINT ( 'NONE',  ( 0.3676999524040323597, -18.60775935196367925, 39.99627326667132365 ) ) ;
#52756 = EDGE_CURVE ( 'NONE', #33451, #52413, #28181, .T. ) ;
#52757 = CARTESIAN_POINT ( 'NONE',  ( 0.6016117650947691020, -30.34493361141474566, 38.61005126082236671 ) ) ;
#52758 = EDGE_CURVE ( 'NONE', #5676, #33419, #61768, .T. ) ;
#52759 = CYLINDRICAL_SURFACE ( 'NONE', #29225, 2.500000000000002220 ) ;
#52760 = CARTESIAN_POINT ( 'NONE',  ( 3.407937589446174087, -1.331713209622414240, -13.63405474014709817 ) ) ;
#52762 = VERTEX_POINT ( 'NONE', #1884 ) ;
#52761 = CARTESIAN_POINT ( 'NONE',  ( -2.739355103387248747, -2.641750642665895210, -14.69247155835230068 ) ) ;
#52763 = ORIENTED_EDGE ( 'NONE', *, *, #59672, .T. ) ;
#52764 = CARTESIAN_POINT ( 'NONE',  ( 0.1064266418746777076, -37.62465821955116496, 21.07422140941941180 ) ) ;
#52765 = CARTESIAN_POINT ( 'NONE',  ( 0.8560838555295223751, -44.00447048317975174, 16.24744323198866169 ) ) ;
#52766 = CARTESIAN_POINT ( 'NONE',  ( 0.1073791018717578927, -21.14095454447534550, -37.58707531572198235 ) ) ;
#52767 = ORIENTED_EDGE ( 'NONE', *, *, #55742, .F. ) ;
#52768 = CARTESIAN_POINT ( 'NONE',  ( 0.5837800304671211249, 22.49746046441963898, 41.14731588854093758 ) ) ;
#52769 = DIRECTION ( 'NONE',  ( -0.000000000000000000, -0.000000000000000000, 1.000000000000000000 ) ) ;
#52770 = CARTESIAN_POINT ( 'NONE',  ( 5.981074661064941900, 7.862380442163868111, 18.95903134304792559 ) ) ;
#52771 = VECTOR ( 'NONE', #30624, 1000.000000000000114 ) ;
#52772 =( BOUNDED_SURFACE ( )  B_SPLINE_SURFACE ( 3, 1, ( 
 ( #44441, #38812 ),
 ( #53177, #5546 ),
 ( #49407, #43826 ),
 ( #869, #11209 ) ),
 .UNSPECIFIED., .F., .F., .F. ) 
 B_SPLINE_SURFACE_WITH_KNOTS ( ( 4, 4 ),
 ( 2, 2 ),
 ( 0.000000000000000000, 1.000000000000000000 ),
 ( 0.000000000000000000, 1.000000000000000000 ),
 .UNSPECIFIED. ) 
 GEOMETRIC_REPRESENTATION_ITEM ( )  RATIONAL_B_SPLINE_SURFACE ( (
 ( 1.000000000000000000, 1.000000000000000000),
 ( 0.7282232189291693025, 0.9929344683865674037),
 ( 0.7282232189291693025, 0.9929344683865674037),
 ( 1.000000000000000000, 1.000000000000000000) ) ) 
 REPRESENTATION_ITEM ( '' )  SURFACE ( )  );
#52773 = ORIENTED_EDGE ( 'NONE', *, *, #57264, .T. ) ;
#52774 = ORIENTED_EDGE ( 'NONE', *, *, #49614, .T. ) ;
#52775 = CARTESIAN_POINT ( 'NONE',  ( 0.1064266418746776244, 17.02047513535232071, -39.62374465289877890 ) ) ;
#52776 = CARTESIAN_POINT ( 'NONE',  ( 4.963659409799326738, -43.79875484948441766, -9.199077662859362903 ) ) ;
#52777 = CARTESIAN_POINT ( 'NONE',  ( 0.1129192098497447394, -44.12161472487018443, 0.4846667466135898827 ) ) ;
#52778 = FACE_OUTER_BOUND ( 'NONE', #39623, .T. ) ;
#52779 = ADVANCED_FACE ( 'NONE', ( #40156 ), #2446, .F. ) ;
#52780 = DIRECTION ( 'NONE',  ( -0.000000000000000000, -0.000000000000000000, -1.000000000000000000 ) ) ;
#52781 =( BOUNDED_SURFACE ( )  B_SPLINE_SURFACE ( 3, 1, ( 
 ( #14946, #39679 ),
 ( #53123, #10229 ),
 ( #24950, #29323 ),
 ( #15548, #39068 ) ),
 .UNSPECIFIED., .F., .F., .F. ) 
 B_SPLINE_SURFACE_WITH_KNOTS ( ( 4, 4 ),
 ( 2, 2 ),
 ( 0.000000000000000000, 1.000000000000000000 ),
 ( 0.000000000000000000, 1.000000000000000000 ),
 .UNSPECIFIED. ) 
 GEOMETRIC_REPRESENTATION_ITEM ( )  RATIONAL_B_SPLINE_SURFACE ( (
 ( 1.000000000000000000, 1.000000000000000000),
 ( 0.7282232189291693025, 0.9929344683865674037),
 ( 0.7282232189291693025, 0.9929344683865674037),
 ( 1.000000000000000000, 1.000000000000000000) ) ) 
 REPRESENTATION_ITEM ( '' )  SURFACE ( )  );
#52782 = EDGE_CURVE ( 'NONE', #53617, #59362, #34979, .T. ) ;
#52783 = CARTESIAN_POINT ( 'NONE',  ( 3.678748215320120973, -33.87011174114093137, 35.37553314004060212 ) ) ;
#52784 = ORIENTED_EDGE ( 'NONE', *, *, #41067, .F. ) ;
#52785 = VERTEX_POINT ( 'NONE', #4257 ) ;
#52786 = CARTESIAN_POINT ( 'NONE',  ( 4.960386119450149955, 18.84353550694778434, -39.48870261569428664 ) ) ;
#52787 = CARTESIAN_POINT ( 'NONE',  ( 5.901764892641288895, -48.07448765165364080, -9.318535532511509345 ) ) ;
#52788 = AXIS2_PLACEMENT_3D ( 'NONE', #27326, #7268, #26396 ) ;
#52789 = ORIENTED_EDGE ( 'NONE', *, *, #33643, .T. ) ;
#52790 = CARTESIAN_POINT ( 'NONE',  ( 0.1135584504625008623, 42.01051332454492382, -13.49328804789572978 ) ) ;
#52791 = CARTESIAN_POINT ( 'NONE',  ( 0.6064515330803581517, -0.8565989750148934601, 46.88923729634646520 ) ) ;
#52792 = CARTESIAN_POINT ( 'NONE',  ( 0.6023143664670691511, 46.39980466492342970, 12.70384782338105545 ) ) ;
#52793 = CARTESIAN_POINT ( 'NONE',  ( 0.1157506346131639274, -40.93413843134928243, -16.47230920927504627 ) ) ;
#52794 = PRODUCT_RELATED_PRODUCT_CATEGORY ( 'part', '', ( #16255 ) ) ;
#52795 = ORIENTED_EDGE ( 'NONE', *, *, #13420, .F. ) ;
#52796 = VERTEX_POINT ( 'NONE', #24010 ) ;
#52797 = CARTESIAN_POINT ( 'NONE',  ( 3.678748215320120529, 48.72168477532871833, -4.980988551782284723 ) ) ;
#52798 = CARTESIAN_POINT ( 'NONE',  ( 5.896782393890504181, 5.965008392937153126, -19.20793486427423247 ) ) ;
#52799 = CARTESIAN_POINT ( 'NONE',  ( 0.1092355843206037486, -37.19569459163120229, -21.82203846347315590 ) ) ;
#52800 = CARTESIAN_POINT ( 'NONE',  ( 0.5836750258453350382, 29.01293504009540669, 38.10871351907198346 ) ) ;
#52801 = ORIENTED_EDGE ( 'NONE', *, *, #37427, .F. ) ;
#52802 = CARTESIAN_POINT ( 'NONE',  ( 0.5997462898726536595, 5.235280152387709940, -48.82769165002913070 ) ) ;
#52803 = ORIENTED_EDGE ( 'NONE', *, *, #52815, .T. ) ;
#52804 = FACE_OUTER_BOUND ( 'NONE', #25946, .T. ) ;
#52805 = CARTESIAN_POINT ( 'NONE',  ( 5.974727161628367256, 18.96851388233647384, 7.840226266082609641 ) ) ;
#52806 = B_SPLINE_CURVE_WITH_KNOTS ( 'NONE', 3,
 ( #29860, #48976, #15466, #19558 ),
 .UNSPECIFIED., .F., .F.,
 ( 4, 4 ),
 ( 0.000000000000000000, 0.005013413432710148512 ),
 .UNSPECIFIED. ) ;
#52807 = AXIS2_PLACEMENT_3D ( 'NONE', #42075, #42675, #57342 ) ;
#52808 = ORIENTED_EDGE ( 'NONE', *, *, #50405, .F. ) ;
#52809 = LINE ( 'NONE', #29014, #38924 ) ;
#52810 = CARTESIAN_POINT ( 'NONE',  ( 0.5980894510889448457, -42.01322166096935007, 23.44630161211513197 ) ) ;
#52811 = CARTESIAN_POINT ( 'NONE',  ( 4.549368137175248350, -23.67244292351614376, -35.80950303116092925 ) ) ;
#52812 = B_SPLINE_CURVE_WITH_KNOTS ( 'NONE', 3,
 ( #36934, #28119, #55997, #12814 ),
 .UNSPECIFIED., .F., .F.,
 ( 4, 4 ),
 ( 8.673617379884035472E-19, 0.004446298630425071091 ),
 .UNSPECIFIED. ) ;
#52813 = CIRCLE ( 'NONE', #54770, 47.91270532121795611 ) ;
#52814 = ORIENTED_EDGE ( 'NONE', *, *, #33773, .F. ) ;
#52815 = EDGE_CURVE ( 'NONE', #30127, #34543, #8662, .T. ) ;
#52816 = LINE ( 'NONE', #9591, #49495 ) ;
#52817 = DIRECTION ( 'NONE',  ( -1.000000000000000000, -0.000000000000000000, -0.000000000000000000 ) ) ;
#52818 = CARTESIAN_POINT ( 'NONE',  ( 1.092182651088185574, -40.91119942363535245, 9.112351297103435499 ) ) ;
#52819 = DIRECTION ( 'NONE',  ( 1.000000000000000000, 0.000000000000000000, 0.000000000000000000 ) ) ;
#52820 = CARTESIAN_POINT ( 'NONE',  ( -6.010958268070873523, -2.445171577615640857, -18.68413620842266454 ) ) ;
#52821 = ORIENTED_EDGE ( 'NONE', *, *, #51100, .F. ) ;
#52822 = CARTESIAN_POINT ( 'NONE',  ( 0.5827359174754828119, -24.26188383263398407, 41.29633904010504608 ) ) ;
#52823 = VECTOR ( 'NONE', #52906, 1000.000000000000114 ) ;
#52824 = CARTESIAN_POINT ( 'NONE',  ( -6.078726893082806448, 5.475592473157615991, -18.46109228449443052 ) ) ;
#52825 = EDGE_CURVE ( 'NONE', #17365, #15298, #22199, .T. ) ;
#52826 = CARTESIAN_POINT ( 'NONE',  ( 0.5830082357119575898, 28.03719174367731881, -37.59185967821500185 ) ) ;
#52827 = ORIENTED_EDGE ( 'NONE', *, *, #27029, .T. ) ;
#52828 = EDGE_CURVE ( 'NONE', #18299, #57911, #58774, .T. ) ;
#52829 = CARTESIAN_POINT ( 'NONE',  ( 4.962356264823608143, 0.000000000000000000, 0.000000000000000000 ) ) ;
#52830 = CARTESIAN_POINT ( 'NONE',  ( 5.910764540655177868, -19.93069368583278234, -2.696050383555225860 ) ) ;
#52831 = CARTESIAN_POINT ( 'NONE',  ( -6.072942160501519915, -14.67202460315899515, -12.47140153845257871 ) ) ;
#52832 = DIRECTION ( 'NONE',  ( -1.000000000000000000, -1.836909530733573776E-16, 2.465190328815655050E-32 ) ) ;
#52833 = CARTESIAN_POINT ( 'NONE',  ( 4.335381028904201628, -11.88755795484448363, -47.52307664213838478 ) ) ;
#52834 = CARTESIAN_POINT ( 'NONE',  ( 0.8760168074887076939, 44.77533136581857320, 17.58183840866416148 ) ) ;
#52835 = CARTESIAN_POINT ( 'NONE',  ( 52.79844894553458801, 15.44348932695818810, 1.330174488105935193 ) ) ;
#52836 = B_SPLINE_CURVE_WITH_KNOTS ( 'NONE', 3,
 ( #48632, #30757, #20444, #21062 ),
 .UNSPECIFIED., .F., .F.,
 ( 4, 4 ),
 ( 2.100108283942812283E-17, 0.004559932413162185068 ),
 .UNSPECIFIED. ) ;
#52837 =( NAMED_UNIT ( * ) PLANE_ANGLE_UNIT ( ) SI_UNIT ( $, .RADIAN. ) );
#52838 = CARTESIAN_POINT ( 'NONE',  ( 4.956445790444002242, -32.34643101787113295, 34.22347806032784234 ) ) ;
#52839 = CARTESIAN_POINT ( 'NONE',  ( 0.6031356755852232965, 4.336951783013129340E-16, 48.10744332413860747 ) ) ;
#52840 = TOROIDAL_SURFACE ( 'NONE', #11870, 2.700000000000000622, 0.2000000000000000111 ) ;
#52841 = CARTESIAN_POINT ( 'NONE',  ( 0.1064266418746774440, -25.80493189480207761, -34.55203617814582628 ) ) ;
#52843 = ORIENTED_EDGE ( 'NONE', *, *, #32032, .F. ) ;
#52842 = CARTESIAN_POINT ( 'NONE',  ( 3.407937589446178528, 13.63405474014708574, 1.331713209622550576 ) ) ;
#52844 = ORIENTED_EDGE ( 'NONE', *, *, #31836, .F. ) ;
#52845 = VECTOR ( 'NONE', #4903, 1000.000000000000000 ) ;
#52846 = CARTESIAN_POINT ( 'NONE',  ( 2.526552050251865911, -33.34585601411847477, -27.11558601691300652 ) ) ;
#52847 = CARTESIAN_POINT ( 'NONE',  ( 49.64180998113290144, 15.29505603208808395, -2.513117253861154143 ) ) ;
#52848 = PRODUCT_DEFINITION_SHAPE ( 'NONE', 'NONE',  #61994 ) ;
#52849 = CARTESIAN_POINT ( 'NONE',  ( 2.500000000000000444, 0.000000000000000000, 3.469446951953614189E-15 ) ) ;
#52850 = CARTESIAN_POINT ( 'NONE',  ( 0.7948878604505680290, -35.86813329665885419, -33.52872889197455208 ) ) ;
#52851 = CARTESIAN_POINT ( 'NONE',  ( 1.227938101723756947, -25.45152231597080927, 34.55893248994497924 ) ) ;
#52852 = ORIENTED_EDGE ( 'NONE', *, *, #14099, .T. ) ;
#52853 = DIRECTION ( 'NONE',  ( -1.000000000000000000, -1.836909530733573776E-16, 1.925929944387235853E-32 ) ) ;
#52854 = B_SPLINE_CURVE_WITH_KNOTS ( 'NONE', 3,
 ( #22789, #4269, #37216, #32506 ),
 .UNSPECIFIED., .F., .F.,
 ( 4, 4 ),
 ( 0.000000000000000000, 0.005014147105413709060 ),
 .UNSPECIFIED. ) ;
#52855 = AXIS2_PLACEMENT_3D ( 'NONE', #21091, #44010, #59600 ) ;
#52856 = CARTESIAN_POINT ( 'NONE',  ( 3.999999999999990674, -2.309401076758548221, -5.242734410091827613 ) ) ;
#52857 = ORIENTED_EDGE ( 'NONE', *, *, #30179, .T. ) ;
#52858 = B_SPLINE_CURVE_WITH_KNOTS ( 'NONE', 3,
 ( #13012, #61202, #4785, #46513, #46833, #33038 ),
 .UNSPECIFIED., .F., .F.,
 ( 4, 2, 4 ),
 ( 3.035766082959412415E-18, 0.0002447193893791692202, 0.0004894387787583354046 ),
 .UNSPECIFIED. ) ;
#52859 = CARTESIAN_POINT ( 'NONE',  ( 5.896782393890504181, -2.006887468070122527, -20.01245835894519587 ) ) ;
#52860 = DIRECTION ( 'NONE',  ( -0.07906939808003035641, 0.5848023231963220825, -0.8073129957280794633 ) ) ;
#52861 = EDGE_LOOP ( 'NONE', ( #53073, #49201, #15313, #30929 ) ) ;
#52862 = EDGE_CURVE ( 'NONE', #36737, #15825, #52816, .T. ) ;
#52863 = CARTESIAN_POINT ( 'NONE',  ( 3.678834586032787346, -46.87103877373264993, -14.20274951900528748 ) ) ;
#52864 = ORIENTED_EDGE ( 'NONE', *, *, #33052, .F. ) ;
#52865 =( BOUNDED_SURFACE ( )  B_SPLINE_SURFACE ( 3, 1, ( 
 ( #10489, #33386 ),
 ( #19908, #34300 ),
 ( #29584, #5749 ),
 ( #23971, #43097 ) ),
 .UNSPECIFIED., .F., .F., .F. ) 
 B_SPLINE_SURFACE_WITH_KNOTS ( ( 4, 4 ),
 ( 2, 2 ),
 ( 0.000000000000000000, 1.000000000000000000 ),
 ( 0.000000000000000000, 1.000000000000000000 ),
 .UNSPECIFIED. ) 
 GEOMETRIC_REPRESENTATION_ITEM ( )  RATIONAL_B_SPLINE_SURFACE ( (
 ( 1.000000000000000000, 1.000000000000000000),
 ( 0.9952954269826590483, 0.8620686068821339365),
 ( 0.9952954269826590483, 0.8620686068821339365),
 ( 1.000000000000000000, 1.000000000000000000) ) ) 
 REPRESENTATION_ITEM ( '' )  SURFACE ( )  );
#52866 = CARTESIAN_POINT ( 'NONE',  ( 0.5998501479064699549, -12.95623334615470057, -46.33007877220734372 ) ) ;
#52867 = FACE_OUTER_BOUND ( 'NONE', #54041, .T. ) ;
#52868 = ORIENTED_EDGE ( 'NONE', *, *, #3299, .T. ) ;
#52869 = CARTESIAN_POINT ( 'NONE',  ( 0.8554163680231738898, -44.01281378489782981, -16.25046755781900742 ) ) ;
#52870 = CARTESIAN_POINT ( 'NONE',  ( 0.5804410086790514622, 11.40290849443534960, -45.49168638029296119 ) ) ;
#52871 = CARTESIAN_POINT ( 'NONE',  ( 4.960156602257179692, 41.85906677498956441, 20.07163247083160584 ) ) ;
#52872 = CARTESIAN_POINT ( 'NONE',  ( -6.079354080745853928, -1.847856142170251736, -19.16711723045502325 ) ) ;
#52873 = B_SPLINE_CURVE_WITH_KNOTS ( 'NONE', 3,
 ( #3659, #22482, #47527, #13716, #46615, #56290 ),
 .UNSPECIFIED., .F., .F.,
 ( 4, 2, 4 ),
 ( 2.032850612904068153E-17, 0.0002293319059085106046, 0.0004586638118170008804 ),
 .UNSPECIFIED. ) ;
#52874 = VERTEX_POINT ( 'NONE', #56274 ) ;
#52875 = CARTESIAN_POINT ( 'NONE',  ( 5.838029081930957709, 19.90064824094122997, 42.83724148148714761 ) ) ;
#52876 = ORIENTED_EDGE ( 'NONE', *, *, #45708, .T. ) ;
#52877 = CARTESIAN_POINT ( 'NONE',  ( 0.1313383488274104394, 21.00709374781539651, -37.66088038379817249 ) ) ;
#52878 = VERTEX_POINT ( 'NONE', #24317 ) ;
#52879 = ORIENTED_EDGE ( 'NONE', *, *, #54240, .T. ) ;
#52880 = DIRECTION ( 'NONE',  ( 0.000000000000000000, 0.000000000000000000, 1.000000000000000000 ) ) ;
#52881 = CARTESIAN_POINT ( 'NONE',  ( 0.9762797500689124330, -37.62962005162918899, 18.44821075214967721 ) ) ;
#52882 = VECTOR ( 'NONE', #17891, 1000.000000000000227 ) ;
#52883 = CIRCLE ( 'NONE', #29897, 2.698940690764985550 ) ;
#52884 = CARTESIAN_POINT ( 'NONE',  ( 0.5804410086790514622, -24.77328595090390451, 39.82215658462187946 ) ) ;
#52885 = ORIENTED_EDGE ( 'NONE', *, *, #45387, .F. ) ;
#52886 = CARTESIAN_POINT ( 'NONE',  ( -6.001507490154111224, -7.196845540359040783, -17.41542759839272136 ) ) ;
#52887 = CARTESIAN_POINT ( 'NONE',  ( 4.549368137175248350, -24.02461520945298545, 35.57418903283073064 ) ) ;
#52888 =( BOUNDED_SURFACE ( )  B_SPLINE_SURFACE ( 3, 1, ( 
 ( #5477, #24613 ),
 ( #28688, #47814 ),
 ( #57472, #43750 ),
 ( #797, #20230 ) ),
 .UNSPECIFIED., .F., .F., .F. ) 
 B_SPLINE_SURFACE_WITH_KNOTS ( ( 4, 4 ),
 ( 2, 2 ),
 ( 0.000000000000000000, 1.000000000000000000 ),
 ( 0.000000000000000000, 1.000000000000000000 ),
 .UNSPECIFIED. ) 
 GEOMETRIC_REPRESENTATION_ITEM ( )  RATIONAL_B_SPLINE_SURFACE ( (
 ( 1.000000000000000000, 1.000000000000000000),
 ( 0.9751682680413298332, 0.9999560080971552356),
 ( 0.9751682680413298332, 0.9999560080971552356),
 ( 1.000000000000000000, 1.000000000000000000) ) ) 
 REPRESENTATION_ITEM ( '' )  SURFACE ( )  );
#52889 = CARTESIAN_POINT ( 'NONE',  ( 0.1152339509894530906, -38.33609478102006562, 21.84688827718698079 ) ) ;
#52890 = ORIENTED_EDGE ( 'NONE', *, *, #2163, .T. ) ;
#52891 = EDGE_CURVE ( 'NONE', #24440, #40711, #57339, .T. ) ;
#52892 = ORIENTED_EDGE ( 'NONE', *, *, #36892, .F. ) ;
#52893 = CARTESIAN_POINT ( 'NONE',  ( 0.5980271706414734822, 32.49685829779753021, -36.82395203688124496 ) ) ;
#52894 = CARTESIAN_POINT ( 'NONE',  ( 0.3622758884714600280, -26.89560658783410574, 33.69533458712297147 ) ) ;
#52895 = CARTESIAN_POINT ( 'NONE',  ( 4.999999999999986677, 56.56854249492450037, -56.56854249492312192 ) ) ;
#52896 = ORIENTED_EDGE ( 'NONE', *, *, #18393, .F. ) ;
#52897 = EDGE_CURVE ( 'NONE', #41881, #23427, #18475, .T. ) ;
#52898 = CIRCLE ( 'NONE', #19927, 42.92674063221959813 ) ;
#52899 = ORIENTED_EDGE ( 'NONE', *, *, #42743, .T. ) ;
#52900 = EDGE_CURVE ( 'NONE', #15368, #18903, #17495, .T. ) ;
#52901 = DIRECTION ( 'NONE',  ( 0.000000000000000000, 0.000000000000000000, -1.000000000000000000 ) ) ;
#52902 = CARTESIAN_POINT ( 'NONE',  ( 3.559346040607745287, 42.72017740054766932, -10.41233520434895610 ) ) ;
#52903 = CARTESIAN_POINT ( 'NONE',  ( 1.827119703190778877, -12.32825544177808119, -41.24693285842924695 ) ) ;
#52904 = CARTESIAN_POINT ( 'NONE',  ( 0.9730545539215892381, -21.89037132892461912, 36.90443313492323085 ) ) ;
#52905 = CARTESIAN_POINT ( 'NONE',  ( 0.7242486021783834937, 37.91429605804456315, -31.20124383413132563 ) ) ;
#52906 = DIRECTION ( 'NONE',  ( -0.9990097760809876215, 5.448601141171670962E-18, -0.04449120468828399177 ) ) ;
#52907 = AXIS2_PLACEMENT_3D ( 'NONE', #52211, #48151, #9000 ) ;
#52908 = ORIENTED_EDGE ( 'NONE', *, *, #26889, .T. ) ;
#52909 = DIRECTION ( 'NONE',  ( 1.000000000000000000, 0.000000000000000000, 0.000000000000000000 ) ) ;
#52910 = CARTESIAN_POINT ( 'NONE',  ( 1.091591847532195292, -39.84368319171721140, 13.00922367683450354 ) ) ;
#52911 = CARTESIAN_POINT ( 'NONE',  ( 0.6067099128993237445, -46.44339333106605494, -11.71051825714752148 ) ) ;
#52913 = EDGE_CURVE ( 'NONE', #41860, #2075, #25186, .T. ) ;
#52912 = CARTESIAN_POINT ( 'NONE',  ( 0.5850706913938533704, -41.56998471741244572, 23.79070617305366753 ) ) ;
#52914 = CARTESIAN_POINT ( 'NONE',  ( 0.7764139734771244861, 40.80384766507922478, -23.13193650846973881 ) ) ;
#52915 = EDGE_CURVE ( 'NONE', #60938, #48571, #31176, .T. ) ;
#52916 = CARTESIAN_POINT ( 'NONE',  ( 0.8753041380234471980, -19.05925361776887073, -45.25354328012939931 ) ) ;
#52917 = FACE_OUTER_BOUND ( 'NONE', #32780, .T. ) ;
#52918 = VERTEX_POINT ( 'NONE', #4562 ) ;
#52919 = CARTESIAN_POINT ( 'NONE',  ( 4.958415959904820980, -5.049385427348767941, 45.14097540626162441 ) ) ;
#52920 = CIRCLE ( 'NONE', #25928, 5.612499999999999822 ) ;
#52921 = CARTESIAN_POINT ( 'NONE',  ( 0.1102847568649952675, 37.39286109091547416, 21.48234084756709095 ) ) ;
#52922 = CARTESIAN_POINT ( 'NONE',  ( 0.6024113833632039894, -47.44569806650977739, -12.66679138860581055 ) ) ;
#52923 = CARTESIAN_POINT ( 'NONE',  ( 1.296416391601052709, 40.17668401393044775, 18.11467459605454522 ) ) ;
#52924 = CARTESIAN_POINT ( 'NONE',  ( 3.783278058412224976, -36.37891728069884323, 22.99727281874613638 ) ) ;
#52925 = ORIENTED_EDGE ( 'NONE', *, *, #11259, .F. ) ;
#52926 = DIRECTION ( 'NONE',  ( 0.000000000000000000, 0.000000000000000000, 1.000000000000000000 ) ) ;
#52927 = CARTESIAN_POINT ( 'NONE',  ( 0.1129192098497455998, 36.71339784380029414, 24.47607416535571545 ) ) ;
#52928 = B_SPLINE_CURVE_WITH_KNOTS ( 'NONE', 3,
 ( #26103, #54582, #21714, #45541 ),
 .UNSPECIFIED., .F., .F.,
 ( 4, 4 ),
 ( 0.000000000000000000, 0.004442905043737217438 ),
 .UNSPECIFIED. ) ;
#52929 = DIRECTION ( 'NONE',  ( -1.000000000000000000, -1.836909530733580185E-16, 1.836909530733574022E-16 ) ) ;
#52930 = ORIENTED_EDGE ( 'NONE', *, *, #6269, .T. ) ;
#52931 = CARTESIAN_POINT ( 'NONE',  ( 4.691466044806102076, -42.32811009116564804, 14.01607102724468490 ) ) ;
#52932 = EDGE_CURVE ( 'NONE', #57911, #4945, #5740, .T. ) ;
#52933 = DIRECTION ( 'NONE',  ( 1.000000000000000000, 0.000000000000000000, 0.000000000000000000 ) ) ;
#52934 = ORIENTED_EDGE ( 'NONE', *, *, #22606, .T. ) ;
#52935 = VECTOR ( 'NONE', #888, 1000.000000000000000 ) ;
#52936 = ORIENTED_EDGE ( 'NONE', *, *, #41327, .T. ) ;
#52937 = CARTESIAN_POINT ( 'NONE',  ( 0.8760168074887090262, -44.09317760313766144, 19.22870327415225233 ) ) ;
#52938 = ORIENTED_EDGE ( 'NONE', *, *, #8063, .F. ) ;
#52939 = CARTESIAN_POINT ( 'NONE',  ( 0.1158816050234199035, 29.66051085023697453, -32.66796806365733374 ) ) ;
#52940 = DIRECTION ( 'NONE',  ( -1.000000000000000000, -0.000000000000000000, -0.000000000000000000 ) ) ;
#52941 = ORIENTED_EDGE ( 'NONE', *, *, #48039, .T. ) ;
#52942 = DIRECTION ( 'NONE',  ( 0.000000000000000000, 0.000000000000000000, 1.000000000000000000 ) ) ;
#52943 = ORIENTED_EDGE ( 'NONE', *, *, #43581, .T. ) ;
#52944 = CARTESIAN_POINT ( 'NONE',  ( -2.708315649062910779, 5.842990691604599718, -13.41752550814504907 ) ) ;
#52945 = CARTESIAN_POINT ( 'NONE',  ( 0.2230388203127619540, 33.74101226470666859, -26.84831060237808131 ) ) ;
#52946 = DIRECTION ( 'NONE',  ( 0.000000000000000000, 0.000000000000000000, -1.000000000000000000 ) ) ;
#52947 = ORIENTED_EDGE ( 'NONE', *, *, #18369, .T. ) ;
#52948 = CARTESIAN_POINT ( 'NONE',  ( 0.9754402186311947887, -16.59348191374109405, -39.57010335554347336 ) ) ;
#52949 = DIRECTION ( 'NONE',  ( -0.9848077530122077983, -0.1736481776669316079, 1.387778780781445367E-17 ) ) ;
#52950 = CARTESIAN_POINT ( 'NONE',  ( 0.5997462898726536595, 27.66511329191646951, -40.57330571557777432 ) ) ;
#52951 = ORIENTED_EDGE ( 'NONE', *, *, #8369, .T. ) ;
#52952 = CARTESIAN_POINT ( 'NONE',  ( -6.016761891674565099, 9.418621820384494470, 16.32039929810260048 ) ) ;
#52953 = CARTESIAN_POINT ( 'NONE',  ( 0.9722240750034574219, -10.54237121715114966, 41.59310803641459131 ) ) ;
#52954 = B_SPLINE_CURVE_WITH_KNOTS ( 'NONE', 3,
 ( #36397, #6588, #26660, #31675 ),
 .UNSPECIFIED., .F., .F.,
 ( 4, 4 ),
 ( 1.734723475976807094E-18, 0.004048833967417084755 ),
 .UNSPECIFIED. ) ;
#52955 = ORIENTED_EDGE ( 'NONE', *, *, #34332, .T. ) ;
#52956 = CARTESIAN_POINT ( 'NONE',  ( 5.959828726073459926, 7.850628836606854399, -18.96492317065686350 ) ) ;
#52957 =( BOUNDED_SURFACE ( )  B_SPLINE_SURFACE ( 3, 1, ( 
 ( #24104, #23182 ),
 ( #53912, #38233 ),
 ( #42311, #13485 ),
 ( #19417, #28799 ) ),
 .UNSPECIFIED., .F., .F., .F. ) 
 B_SPLINE_SURFACE_WITH_KNOTS ( ( 4, 4 ),
 ( 2, 2 ),
 ( 0.000000000000000000, 1.000000000000000000 ),
 ( 0.000000000000000000, 1.000000000000000000 ),
 .UNSPECIFIED. ) 
 GEOMETRIC_REPRESENTATION_ITEM ( )  RATIONAL_B_SPLINE_SURFACE ( (
 ( 1.000000000000000000, 1.000000000000000000),
 ( 0.9754377213608244057, 0.9999580625633939235),
 ( 0.9754377213608244057, 0.9999580625633939235),
 ( 1.000000000000000000, 1.000000000000000000) ) ) 
 REPRESENTATION_ITEM ( '' )  SURFACE ( )  );
#52958 = VERTEX_POINT ( 'NONE', #25852 ) ;
#52959 = VECTOR ( 'NONE', #25116, 1000.000000000000114 ) ;
#52960 = CARTESIAN_POINT ( 'NONE',  ( 58.00000000000000000, 15.50000000000000888, 1.598617315530390651E-15 ) ) ;
#52961 = CARTESIAN_POINT ( 'NONE',  ( 0.1147471544378676905, 25.49827294024393609, 36.01097423755804527 ) ) ;
#52962 = VERTEX_POINT ( 'NONE', #1108 ) ;
#52963 = CARTESIAN_POINT ( 'NONE',  ( 0.5837800005270570303, 4.694119656474818214, 46.66048113010067766 ) ) ;
#52964 = CARTESIAN_POINT ( 'NONE',  ( 0.1149546198390367230, 25.46835312172088450, -36.03206286476739706 ) ) ;
#52965 = CARTESIAN_POINT ( 'NONE',  ( 0.6041374136657475802, 47.67304777898691270, 6.452348380036067255 ) ) ;
#52966 = DIRECTION ( 'NONE',  ( 0.000000000000000000, 0.000000000000000000, 1.000000000000000000 ) ) ;
#52967 = ADVANCED_FACE ( 'NONE', ( #810 ), #35911, .F. ) ;
#52968 = TOROIDAL_SURFACE ( 'NONE', #24992, 7.400000000000021672, 0.1000000000000001582 ) ;
#52969 = VERTEX_POINT ( 'NONE', #53117 ) ;
#52970 = DIRECTION ( 'NONE',  ( -0.1024043820194934645, 0.9946559125373960475, 0.01315135725336188596 ) ) ;
#52971 = ADVANCED_FACE ( 'NONE', ( #19633 ), #54710, .F. ) ;
#52972 = CARTESIAN_POINT ( 'NONE',  ( 2.282803330402966235, -46.27578309073107476, 8.065284049343492967 ) ) ;
#52973 = CARTESIAN_POINT ( 'NONE',  ( 3.598898625538307083, 0.2887647096731989493, -48.97398349821926189 ) ) ;
#52974 = CARTESIAN_POINT ( 'NONE',  ( 5.960721111146673579, -7.860635756378015593, 18.96073515164535195 ) ) ;
#52975 = CARTESIAN_POINT ( 'NONE',  ( -6.079354080745853928, 15.43270669589052524, 11.51627193525655279 ) ) ;
#52976 = CARTESIAN_POINT ( 'NONE',  ( 3.559346040607745287, -9.037736435379585487, -43.03196023499975098 ) ) ;
#52977 = CARTESIAN_POINT ( 'NONE',  ( 0.1129192098497455998, -41.07894348801367812, 16.10814047907867064 ) ) ;
#52978 = CIRCLE ( 'NONE', #36028, 1.000000000000000888 ) ;
#52979 = CARTESIAN_POINT ( 'NONE',  ( 3.783278058412226752, 14.86148287637788279, -40.39104487792928921 ) ) ;
#52980 = CARTESIAN_POINT ( 'NONE',  ( 0.2885700199627508344, -36.93108631019309485, 22.25146206940400972 ) ) ;
#52981 = CARTESIAN_POINT ( 'NONE',  ( 0.6023143664670691511, 48.10676742339276046, 0.2618215695309267232 ) ) ;
#52982 = EDGE_CURVE ( 'NONE', #45745, #15399, #5489, .T. ) ;
#52983 = CARTESIAN_POINT ( 'NONE',  ( 0.1156495703730067576, -43.77914071683246533, -5.507248979922001020 ) ) ;
#52985 = B_SPLINE_CURVE_WITH_KNOTS ( 'NONE', 3,
 ( #43142, #48135, #47836, #19026, #39065, #14322, #15242, #52195, #495, #814, #14943, #34051, #52504, #28396, #178, #5492 ),
 .UNSPECIFIED., .F., .F.,
 ( 4, 3, 3, 3, 3, 4 ),
 ( 1.962735358247463844E-17, 0.0002618515315864417600, 0.0003927756766342021112, 0.0005236998216950595163, 0.0007855159896329960787, 0.001047349442285930039 ),
 .UNSPECIFIED. ) ;
#52984 = CARTESIAN_POINT ( 'NONE',  ( 0.6001305935487422083, 44.64600790884030346, 17.92615948558555417 ) ) ;
#52986 = CARTESIAN_POINT ( 'NONE',  ( 0.5837157313716023754, -1.658013562071385394, 46.86670518193070478 ) ) ;
#52987 = CARTESIAN_POINT ( 'NONE',  ( 0.9784957157296378938, 9.941547056922068748, 40.71238999502944722 ) ) ;
#52988 = CARTESIAN_POINT ( 'NONE',  ( -2.739355103387247858, 11.19469682329918925, 9.875542009704176394 ) ) ;
#52989 = CARTESIAN_POINT ( 'NONE',  ( -6.079354080745853928, 19.09804277166047370, -2.461243088357813136 ) ) ;
#52990 = VERTEX_POINT ( 'NONE', #11153 ) ;
#52991 = CARTESIAN_POINT ( 'NONE',  ( 4.549368137175248350, 0.000000000000000000, 0.000000000000000000 ) ) ;
#52992 = CARTESIAN_POINT ( 'NONE',  ( 0.3676999524040366896, 19.66859742988788184, -39.48540057367844724 ) ) ;
#52993 = CARTESIAN_POINT ( 'NONE',  ( 4.549368137175248350, 28.14399996863453168, 32.41327393324149853 ) ) ;
#52994 = VERTEX_POINT ( 'NONE', #10223 ) ;
#52995 = CARTESIAN_POINT ( 'NONE',  ( 0.5997462898726536595, -14.47257175146309649, 46.92649887902422279 ) ) ;
#52996 = CARTESIAN_POINT ( 'NONE',  ( 2.009741617377216460, 26.30790974367969426, 35.31852152258708344 ) ) ;
#52997 = ORIENTED_EDGE ( 'NONE', *, *, #30610, .F. ) ;
#52998 = VERTEX_POINT ( 'NONE', #43768 ) ;
#52999 = CARTESIAN_POINT ( 'NONE',  ( -5.995132425357893702, 4.869002713216572076, 18.20425902871269486 ) ) ;
#53000 = ORIENTED_EDGE ( 'NONE', *, *, #29785, .T. ) ;
#53001 = VECTOR ( 'NONE', #26214, 999.9999999999997726 ) ;
#53002 = DIRECTION ( 'NONE',  ( 1.000000000000000000, 1.836970198721027962E-16, -2.033782021272921061E-31 ) ) ;
#53003 = VERTEX_POINT ( 'NONE', #57807 ) ;
#53004 = ADVANCED_FACE ( 'NONE', ( #16161 ), #22722, .F. ) ;
#53005 = ORIENTED_EDGE ( 'NONE', *, *, #12418, .T. ) ;
#53006 = ORIENTED_EDGE ( 'NONE', *, *, #24698, .F. ) ;
#53007 = CARTESIAN_POINT ( 'NONE',  ( -6.077587904424778920, -12.94128980615197477, 14.25899854643086329 ) ) ;
#53008 = DIRECTION ( 'NONE',  ( 1.000000000000000000, 0.000000000000000000, 0.000000000000000000 ) ) ;
#53009 = B_SPLINE_CURVE_WITH_KNOTS ( 'NONE', 3,
 ( #61262, #3936, #28078, #22761 ),
 .UNSPECIFIED., .F., .F.,
 ( 4, 4 ),
 ( 0.000000000000000000, 0.005004948556313802699 ),
 .UNSPECIFIED. ) ;
#53010 = EDGE_CURVE ( 'NONE', #19405, #47199, #34646, .T. ) ;
#53011 = CARTESIAN_POINT ( 'NONE',  ( 0.8760168074886960365, -46.22580377597776646, -13.30888447662064067 ) ) ;
#53012 = VERTEX_POINT ( 'NONE', #29621 ) ;
#53013 = CARTESIAN_POINT ( 'NONE',  ( 0.7245667037590795001, -44.74806999162976240, -17.64710816761245482 ) ) ;
#53014 = CLOSED_SHELL ( 'NONE', ( #53057, #32979, #5442, #29041, #4109, #31631, #45732, #27651, #19537, #7113, #48103, #58247, #27164, #37097, #40500, #20078, #54870, #13932, #58024, #53732, #34986, #54273, #6318, #43101, #56356, #32608, #36724, #28753, #1836, #12953, #50988, #48827, #8140, #5773, #18486, #37004, #31067, #45433, #37122, #7909, #54793, #22706, #44033, #11669, #8154, #31833, #25670, #15687, #16178, #40413, #12686, #41982, #42677, #25091, #7924, #41146, #7584, #26962, #42975, #51971, #2449, #46770, #30524, #6047, #54203, #56559, #33019, #11323, #19913, #47450, #29373, #45916, #37823, #24056, #24704, #16692, #39946, #57537, #2206, #20497, #9729, #18463, #35593, #27865, #18670, #26066, #17969, #30547, #58338, #15864, #5287, #10638, #24425, #3020, #53577, #59775, #42924, #56155, #29401, #37507, #39493, #50480, #7933, #32467, #14667, #52482, #57121, #6231, #32388, #20193, #6281, #4424, #7299, #58882, #12524, #38601, #48490, #24787, #24267, #44121, #25970, #24390, #61526, #32082, #26811, #18333, #9127, #33613, #56851, #24088, #57203, #2119, #54351, #23539, #16328, #40084, #6972, #3439, #37983, #43653, #44024, #4146, #40836, #314, #33201, #37908, #48171, #2055, #19987, #7771, #6129, #10143, #20727, #34645, #50377, #8992, #50397, #1184, #17973, #3121, #58593, #49435, #54083, #40216, #13908, #49618, #42184, #24814, #26898, #22833, #21119, #25050, #18265, #10321, #53720, #9914, #24666, #30261, #4377, #1682, #12221, #19849, #61442, #54133, #16768, #15655, #37913, #36288, #49084, #4149, #56132, #42390, #32855, #1081, #5585, #28231, #12701, #49646, #6694, #32977, #45638, #49859, #52967, #45484, #2668, #52779, #55500, #42632, #43222, #52253, #53211, #30098, #727, #18856, #25503, #16788, #53230, #19330, #28984, #46773, #40052, #26523, #38170, #28132, #44802, #27782, #37738, #5415, #51435, #52742, #14505, #22133, #34308, #1302, #58857, #49589, #31673, #57665, #54759, #26713, #50995, #12270, #39134, #40100, #35952, #47820, #19651, #1557, #32713, #913, #16487, #39359, #42882, #59909, #58935, #9463, #39579, #553, #61862, #20116, #24560, #37576, #5965, #14379, #13383, #18181, #20653, #36739, #60240, #52115, #41560, #11465, #27505, #53436, #46416, #4499, #36372, #28954, #9307, #60072, #36097, #7541, #23597, #14130, #12477, #4157, #30577, #59010, #6460, #47084, #25154, #42802, #52971, #59850, #9578, #11335, #36947, #54988, #17048, #37036 ) ) ;
#53015 = FACE_OUTER_BOUND ( 'NONE', #23620, .T. ) ;
#53016 = ORIENTED_EDGE ( 'NONE', *, *, #15091, .F. ) ;
#53017 = EDGE_CURVE ( 'NONE', #55454, #47659, #6401, .T. ) ;
#53018 = ORIENTED_EDGE ( 'NONE', *, *, #39772, .T. ) ;
#53019 = CARTESIAN_POINT ( 'NONE',  ( -6.015611763856276717, 14.94556629257441038, -11.47596948473795919 ) ) ;
#53020 = VECTOR ( 'NONE', #26038, 999.9999999999998863 ) ;
#53021 = VERTEX_POINT ( 'NONE', #5794 ) ;
#53022 = CARTESIAN_POINT ( 'NONE',  ( 49.17070544691794964, 12.28715003449873855, 2.299028855467196486 ) ) ;
#53023 = CARTESIAN_POINT ( 'NONE',  ( 0.9968887458511636046, -30.80284987750029657, 29.87314546208219568 ) ) ;
#53024 = CARTESIAN_POINT ( 'NONE',  ( 4.956653778116992370, 15.97476558431944937, -45.35992544608513555 ) ) ;
#53025 = CARTESIAN_POINT ( 'NONE',  ( 0.6064515330803591509, 39.98349652191225090, -24.50825048670992956 ) ) ;
#53026 = ORIENTED_EDGE ( 'NONE', *, *, #19122, .T. ) ;
#53027 = CARTESIAN_POINT ( 'NONE',  ( 0.6039202388192953519, -20.03711874569759743, -44.83388880322344505 ) ) ;
#53028 = CARTESIAN_POINT ( 'NONE',  ( 0.9754292580325135686, 41.45298142384850593, 6.162612918079117819 ) ) ;
#53029 = CARTESIAN_POINT ( 'NONE',  ( 5.901463166500146684, 10.83443963266005028, 16.94499301229958732 ) ) ;
#53030 = CARTESIAN_POINT ( 'NONE',  ( -6.016761891674565099, -2.462934516563935805, 18.68153697670640767 ) ) ;
#53031 = ORIENTED_EDGE ( 'NONE', *, *, #39766, .T. ) ;
#53032 = CARTESIAN_POINT ( 'NONE',  ( 0.7056555295713275999, -38.50897360867666919, -28.48870155114950364 ) ) ;
#53033 = CARTESIAN_POINT ( 'NONE',  ( 0.5997462898726536595, 33.39998138387845472, 35.99990102348730403 ) ) ;
#53034 = CARTESIAN_POINT ( 'NONE',  ( 4.960156602257185909, -9.558288641081436054, -45.42786611289324128 ) ) ;
#53035 = CARTESIAN_POINT ( 'NONE',  ( 0.9754292580325126805, 33.24763091048475161, -25.51318297947520364 ) ) ;
#53036 = EDGE_CURVE ( 'NONE', #18280, #45974, #46077, .T. ) ;
#53037 = ORIENTED_EDGE ( 'NONE', *, *, #32895, .T. ) ;
#53038 = ORIENTED_EDGE ( 'NONE', *, *, #10599, .F. ) ;
#53039 = FACE_OUTER_BOUND ( 'NONE', #21855, .T. ) ;
#53040 = CARTESIAN_POINT ( 'NONE',  ( 0.7057020205115046574, 13.20843872046553180, -46.04437542275030637 ) ) ;
#53041 = EDGE_CURVE ( 'NONE', #38521, #19675, #31066, .T. ) ;
#53042 = FACE_OUTER_BOUND ( 'NONE', #52017, .T. ) ;
#53043 = B_SPLINE_CURVE_WITH_KNOTS ( 'NONE', 3,
 ( #46713, #3753, #13499, #51997, #33226, #47622 ),
 .UNSPECIFIED., .F., .F.,
 ( 4, 2, 4 ),
 ( 1.193026433010871187E-16, 0.0002448718616795929879, 0.0004897437233590666052 ),
 .UNSPECIFIED. ) ;
#53044 = LINE ( 'NONE', #43687, #15574 ) ;
#53045 = EDGE_CURVE ( 'NONE', #27320, #23759, #14663, .T. ) ;
#53046 = CARTESIAN_POINT ( 'NONE',  ( -6.010958268070873523, -2.473955915502343395, 18.68034667844848329 ) ) ;
#53047 = CARTESIAN_POINT ( 'NONE',  ( 0.7762777257811904752, 47.60264404062384358, -5.369627942761147743 ) ) ;
#53048 = CARTESIAN_POINT ( 'NONE',  ( 0.8560838555295158248, -26.00596412780176081, 39.03924517540291106 ) ) ;
#53049 = CARTESIAN_POINT ( 'NONE',  ( 4.062725214796417461, -12.40828859588279798, 0.000000000000000000 ) ) ;
#53050 = CARTESIAN_POINT ( 'NONE',  ( 0.6027935024548037868, -18.24855952726199604, -44.51201578381220259 ) ) ;
#53051 = CARTESIAN_POINT ( 'NONE',  ( 1.227938101723748288, -22.18841447410744649, 36.73927144310504644 ) ) ;
#53052 = ORIENTED_EDGE ( 'NONE', *, *, #21493, .T. ) ;
#53053 = CARTESIAN_POINT ( 'NONE',  ( 1.227938101723756947, -42.43379953535190197, 6.439911493064418124 ) ) ;
#53054 = CARTESIAN_POINT ( 'NONE',  ( 3.407937589446178528, -13.69123696618924768, 0.4592810312471504175 ) ) ;
#53055 = CARTESIAN_POINT ( 'NONE',  ( 0.8753041380234524160, -43.21430456406316978, -23.31656511833100964 ) ) ;
#53056 = CARTESIAN_POINT ( 'NONE',  ( -6.016489644550736315, -0.004404229197644145798, -18.84320342686341121 ) ) ;
#53057 = ADVANCED_FACE ( 'NONE', ( #22390 ), #16456, .F. ) ;
#53058 = DIRECTION ( 'NONE',  ( 0.09722883295013594329, -0.8708738917981048155, 0.4817937511296480624 ) ) ;
#53059 = CARTESIAN_POINT ( 'NONE',  ( 0.5837374860065647209, -41.38807031854326368, 24.10515569139031555 ) ) ;
#53060 = CARTESIAN_POINT ( 'NONE',  ( 5.959828726073459926, -20.35060134307033053, -2.674641840416102312 ) ) ;
#53061 = DIRECTION ( 'NONE',  ( 0.000000000000000000, 0.000000000000000000, -1.000000000000000000 ) ) ;
#53062 = AXIS2_PLACEMENT_3D ( 'NONE', #42717, #27987, #61776 ) ;
#53063 = CARTESIAN_POINT ( 'NONE',  ( 5.959547316686252039, 12.49238070347954555, 16.28624005235103311 ) ) ;
#53064 = CARTESIAN_POINT ( 'NONE',  ( 1.227938101723748288, -4.762198645644156514, -42.65467462194923343 ) ) ;
#53065 = CARTESIAN_POINT ( 'NONE',  ( 4.833616638992205949, -45.44786513329603395, 8.578242093414962355 ) ) ;
#53066 = CARTESIAN_POINT ( 'NONE',  ( 4.549368137175248350, 28.14399996863497577, -32.41327393324110773 ) ) ;
#53068 = ORIENTED_EDGE ( 'NONE', *, *, #30077, .F. ) ;
#53067 = CARTESIAN_POINT ( 'NONE',  ( 0.1073791018717483448, -26.63563652260144821, -33.91564619577798823 ) ) ;
#53069 = ORIENTED_EDGE ( 'NONE', *, *, #58189, .F. ) ;
#53070 = LINE ( 'NONE', #43715, #18921 ) ;
#53071 = CARTESIAN_POINT ( 'NONE',  ( 2.706805983486679779, 43.78123907016031779, -4.469811942489746670 ) ) ;
#53072 = CARTESIAN_POINT ( 'NONE',  ( 6.189768672337906175, 1.091423221261470733, -2.362915713819767774E-16 ) ) ;
#53073 = ORIENTED_EDGE ( 'NONE', *, *, #49, .F. ) ;
#53074 = CARTESIAN_POINT ( 'NONE',  ( -6.078457390727109555, 0.6128065477896523783, 19.24627182527810731 ) ) ;
#53075 = FACE_OUTER_BOUND ( 'NONE', #32503, .T. ) ;
#53076 = ORIENTED_EDGE ( 'NONE', *, *, #8939, .F. ) ;
#53077 = ORIENTED_EDGE ( 'NONE', *, *, #44512, .F. ) ;
#53078 =( BOUNDED_SURFACE ( )  B_SPLINE_SURFACE ( 3, 1, ( 
 ( #31145, #7316 ),
 ( #59960, #55553 ),
 ( #31780, #17067 ),
 ( #36179, #3241 ) ),
 .UNSPECIFIED., .F., .F., .F. ) 
 B_SPLINE_SURFACE_WITH_KNOTS ( ( 4, 4 ),
 ( 2, 2 ),
 ( 0.000000000000000000, 1.000000000000000000 ),
 ( 0.000000000000000000, 1.000000000000000000 ),
 .UNSPECIFIED. ) 
 GEOMETRIC_REPRESENTATION_ITEM ( )  RATIONAL_B_SPLINE_SURFACE ( (
 ( 1.000000000000000000, 1.000000000000000000),
 ( 0.9952954269826590483, 0.8620686068821339365),
 ( 0.9952954269826590483, 0.8620686068821339365),
 ( 1.000000000000000000, 1.000000000000000000) ) ) 
 REPRESENTATION_ITEM ( '' )  SURFACE ( )  );
#53079 = CARTESIAN_POINT ( 'NONE',  ( 5.910764540655178756, -11.94262894392596408, -16.18254777149955004 ) ) ;
#53080 = CARTESIAN_POINT ( 'NONE',  ( -4.467299999999993609, 1.530808498934191521E-15, 12.50000000000000000 ) ) ;
#53081 = EDGE_CURVE ( 'NONE', #59128, #50838, #2340, .T. ) ;
#53082 = CARTESIAN_POINT ( 'NONE',  ( 1.231276596079881047, 41.42457922925067493, 6.425029704024775690 ) ) ;
#53083 = CARTESIAN_POINT ( 'NONE',  ( 0.5834584762367771571, 46.89565892744833775, 0.1821064897865646570 ) ) ;
#53084 = EDGE_CURVE ( 'NONE', #4099, #10045, #7652, .T. ) ;
#53085 = B_SPLINE_CURVE_WITH_KNOTS ( 'NONE', 3,
 ( #21598, #59806, #60111, #16917 ),
 .UNSPECIFIED., .F., .F.,
 ( 4, 4 ),
 ( 0.000000000000000000, 0.005004948556313801832 ),
 .UNSPECIFIED. ) ;
#53086 = CARTESIAN_POINT ( 'NONE',  ( 5.896782393890504181, 14.91246379622012874, 13.49609241241464375 ) ) ;
#53087 = EDGE_CURVE ( 'NONE', #36885, #60718, #23473, .T. ) ;
#53088 = CARTESIAN_POINT ( 'NONE',  ( 4.963659409799330291, 42.22332985082334034, -14.83726297270234973 ) ) ;
#53089 = CARTESIAN_POINT ( 'NONE',  ( 0.5786265663353153954, -6.967625775955401224, -47.39171391660399735 ) ) ;
#53090 = EDGE_LOOP ( 'NONE', ( #18051, #56247 ) ) ;
#53091 = EDGE_CURVE ( 'NONE', #23600, #53354, #21414, .T. ) ;
#53092 = ORIENTED_EDGE ( 'NONE', *, *, #48655, .T. ) ;
#53093 = CARTESIAN_POINT ( 'NONE',  ( 1.088908134280556883, 15.69861202536805145, -39.93902428011472949 ) ) ;
#53094 = CARTESIAN_POINT ( 'NONE',  ( 0.9722240741986376555, 42.46141200043700081, 6.177112427866004118 ) ) ;
#53095 = ORIENTED_EDGE ( 'NONE', *, *, #16481, .F. ) ;
#53096 = CARTESIAN_POINT ( 'NONE',  ( 0.1129192098497447394, 41.72114954716796120, -14.36305915353690743 ) ) ;
#53097 = CARTESIAN_POINT ( 'NONE',  ( 0.5997462898726536595, -34.91088276334750873, 34.53667463477217581 ) ) ;
#53098 = CARTESIAN_POINT ( 'NONE',  ( 0.8744876279028306332, -39.87136468799875644, -28.64654129726831044 ) ) ;
#53099 = CARTESIAN_POINT ( 'NONE',  ( 4.975610109902397937, 0.000000000000000000, 0.000000000000000000 ) ) ;
#53100 = ORIENTED_EDGE ( 'NONE', *, *, #14810, .T. ) ;
#53101 = ORIENTED_EDGE ( 'NONE', *, *, #43815, .T. ) ;
#53102 = CARTESIAN_POINT ( 'NONE',  ( 0.5837799406558235038, -13.80714289583679033, 44.81747822703933082 ) ) ;
#53103 = CARTESIAN_POINT ( 'NONE',  ( 4.956445790444040433, 44.65954324082233029, -14.93530206124928128 ) ) ;
#53104 = AXIS2_PLACEMENT_3D ( 'NONE', #24171, #15410, #29181 ) ;
#53105 = CARTESIAN_POINT ( 'NONE',  ( 5.860006189529246790, 40.11385274514719157, -26.78264244998056398 ) ) ;
#53106 = EDGE_LOOP ( 'NONE', ( #8111, #20849, #56940, #15327 ) ) ;
#53107 = CARTESIAN_POINT ( 'NONE',  ( 0.5806925824938499181, 22.05663578530122493, 41.38510819338441138 ) ) ;
#53108 = ORIENTED_EDGE ( 'NONE', *, *, #61708, .F. ) ;
#53109 = CARTESIAN_POINT ( 'NONE',  ( 0.8554163680231708922, 23.34472558242500284, -40.69679668712378628 ) ) ;
#53110 = CARTESIAN_POINT ( 'NONE',  ( 0.5838002273316424962, 24.06583301632262462, -41.41085122398227725 ) ) ;
#53111 = ADVANCED_FACE ( 'NONE', ( #13018 ), #48697, .F. ) ;
#53112 = ORIENTED_EDGE ( 'NONE', *, *, #13351, .T. ) ;
#53113 = EDGE_CURVE ( 'NONE', #27845, #19228, #30391, .T. ) ;
#53114 = CARTESIAN_POINT ( 'NONE',  ( -6.016489644550736315, 16.31649074174290703, -9.425415887800916437 ) ) ;
#53115 = CARTESIAN_POINT ( 'NONE',  ( 0.000000000000000000, 0.000000000000000000, -5.599999999999999645 ) ) ;
#53116 = EDGE_CURVE ( 'NONE', #40503, #42430, #26627, .T. ) ;
#53117 = CARTESIAN_POINT ( 'NONE',  ( 0.9730545539215883499, -11.59290486963477562, -41.31259007387244253 ) ) ;
#53118 = CARTESIAN_POINT ( 'NONE',  ( 0.1158816050234198758, 33.59448550014165136, -28.60686255579127035 ) ) ;
#53119 = CARTESIAN_POINT ( 'NONE',  ( 0.8753041380234465318, 21.91949880997691835, 43.93943445007457171 ) ) ;
#53120 = CARTESIAN_POINT ( 'NONE',  ( 3.660176727303420030, 46.85282580473592873, -10.60619300811821475 ) ) ;
#53121 = LINE ( 'NONE', #48432, #38810 ) ;
#53122 = ORIENTED_EDGE ( 'NONE', *, *, #29778, .T. ) ;
#53123 = CARTESIAN_POINT ( 'NONE',  ( 5.910764540655177868, -20.11221018249587544, -0.01549336220058925018 ) ) ;
#53124 = LINE ( 'NONE', #48437, #33834 ) ;
#53125 = ORIENTED_EDGE ( 'NONE', *, *, #4934, .T. ) ;
#53126 = DIRECTION ( 'NONE',  ( -0.000000000000000000, 0.000000000000000000, 1.000000000000000000 ) ) ;
#53127 = CARTESIAN_POINT ( 'NONE',  ( 1.827326673878741481, 29.55671596281165847, 31.30008222956393027 ) ) ;
#53128 = CARTESIAN_POINT ( 'NONE',  ( 0.5997462898726536595, 23.17609050332868037, 43.29457771044576475 ) ) ;
#53129 = CARTESIAN_POINT ( 'NONE',  ( 5.895596859100789899, 19.71057157537855176, 4.002693016503615198 ) ) ;
#53130 = EDGE_CURVE ( 'NONE', #19501, #16409, #16780, .T. ) ;
#53131 = B_SPLINE_CURVE_WITH_KNOTS ( 'NONE', 3,
 ( #36964, #61038, #23760, #14377, #37574, #32557 ),
 .UNSPECIFIED., .F., .F.,
 ( 4, 2, 4 ),
 ( 3.511543213478341086E-18, 0.0002448709889506563977, 0.0004897419779013092176 ),
 .UNSPECIFIED. ) ;
#53132 = CARTESIAN_POINT ( 'NONE',  ( 0.6027444965799114707, -19.99722852491714775, 44.85141432786352311 ) ) ;
#53133 = FACE_OUTER_BOUND ( 'NONE', #48195, .T. ) ;
#53134 = DIRECTION ( 'NONE',  ( 1.835788915976414184E-18, -2.775557561562891351E-17, -1.000000000000000000 ) ) ;
#53135 = CARTESIAN_POINT ( 'NONE',  ( 0.5988103622719989083, 17.84821742497932462, 44.67429504351065361 ) ) ;
#53136 =( BOUNDED_SURFACE ( )  B_SPLINE_SURFACE ( 3, 1, ( 
 ( #34727, #19698 ),
 ( #48203, #15006 ),
 ( #49418, #11221 ),
 ( #25617, #39437 ) ),
 .UNSPECIFIED., .F., .F., .F. ) 
 B_SPLINE_SURFACE_WITH_KNOTS ( ( 4, 4 ),
 ( 2, 2 ),
 ( 0.000000000000000000, 1.000000000000000000 ),
 ( 0.000000000000000000, 1.000000000000000000 ),
 .UNSPECIFIED. ) 
 GEOMETRIC_REPRESENTATION_ITEM ( )  RATIONAL_B_SPLINE_SURFACE ( (
 ( 1.000000000000000000, 1.000000000000000000),
 ( 0.7223157951917476005, 0.9931996967497186413),
 ( 0.7223157951917476005, 0.9931996967497186413),
 ( 1.000000000000000000, 1.000000000000000000) ) ) 
 REPRESENTATION_ITEM ( '' )  SURFACE ( )  );
#53137 = ADVANCED_FACE ( 'NONE', ( #26468 ), #54590, .F. ) ;
#53138 = DIRECTION ( 'NONE',  ( 0.000000000000000000, 0.000000000000000000, 1.000000000000000000 ) ) ;
#53139 = CARTESIAN_POINT ( 'NONE',  ( 0.1310142868023689289, -26.75450212504347292, 33.82067078731299858 ) ) ;
#53141 = ORIENTED_EDGE ( 'NONE', *, *, #37154, .T. ) ;
#53140 = CARTESIAN_POINT ( 'NONE',  ( 4.960386119450145515, -34.62801484853829237, -26.74578569273583994 ) ) ;
#53142 = ORIENTED_EDGE ( 'NONE', *, *, #53159, .T. ) ;
#53143 = CARTESIAN_POINT ( 'NONE',  ( 4.975801465491694664, -43.22084481528235500, 20.67815041659062913 ) ) ;
#53144 = CARTESIAN_POINT ( 'NONE',  ( 3.661921753702004789, -23.70324447415902114, 40.62988217103625033 ) ) ;
#53145 = CARTESIAN_POINT ( 'NONE',  ( 5.896782393890504181, -19.93252920631905667, 2.687073932226298201 ) ) ;
#53146 = CARTESIAN_POINT ( 'NONE',  ( 1.227938101723756947, 0.8460948827225182045, 42.91134962331487657 ) ) ;
#53147 = CARTESIAN_POINT ( 'NONE',  ( 0.9754402186311945666, 42.51649392388761584, -5.786576363453125538 ) ) ;
#53148 = CARTESIAN_POINT ( 'NONE',  ( 0.5848930533535030563, 27.96442382265512450, -37.64656800631999545 ) ) ;
#53149 =( BOUNDED_SURFACE ( )  B_SPLINE_SURFACE ( 3, 1, ( 
 ( #8443, #12565 ),
 ( #50746, #26956 ),
 ( #36679, #13484 ),
 ( #8149, #22566 ) ),
 .UNSPECIFIED., .F., .F., .F. ) 
 B_SPLINE_SURFACE_WITH_KNOTS ( ( 4, 4 ),
 ( 2, 2 ),
 ( 0.000000000000000000, 1.000000000000000000 ),
 ( 0.000000000000000000, 1.000000000000000000 ),
 .UNSPECIFIED. ) 
 GEOMETRIC_REPRESENTATION_ITEM ( )  RATIONAL_B_SPLINE_SURFACE ( (
 ( 1.000000000000000000, 1.000000000000000000),
 ( 0.9953390228620291325, 0.8624445117761032620),
 ( 0.9953390228620291325, 0.8624445117761032620),
 ( 1.000000000000000000, 1.000000000000000000) ) ) 
 REPRESENTATION_ITEM ( '' )  SURFACE ( )  );
#53150 = VECTOR ( 'NONE', #61538, 1000.000000000000000 ) ;
#53151 = VECTOR ( 'NONE', #15652, 1000.000000000000114 ) ;
#53152 = ORIENTED_EDGE ( 'NONE', *, *, #55793, .T. ) ;
#53153 = LINE ( 'NONE', #44420, #54292 ) ;
#53154 = B_SPLINE_CURVE_WITH_KNOTS ( 'NONE', 3,
 ( #16550, #59442, #57650, #29477 ),
 .UNSPECIFIED., .F., .F.,
 ( 4, 4 ),
 ( 0.000000000000000000, 0.004444103432399266161 ),
 .UNSPECIFIED. ) ;
#53155 = CARTESIAN_POINT ( 'NONE',  ( -19.36298947945248372, -7.842906756447401762, 1.580642502182497466 ) ) ;
#53156 = CYLINDRICAL_SURFACE ( 'NONE', #30743, 2.099999999999999645 ) ;
#53157 = ORIENTED_EDGE ( 'NONE', *, *, #53645, .F. ) ;
#53158 = EDGE_CURVE ( 'NONE', #47174, #19080, #56454, .T. ) ;
#53159 = EDGE_CURVE ( 'NONE', #61473, #10306, #41626, .T. ) ;
#53160 = CARTESIAN_POINT ( 'NONE',  ( 0.9722240750034539802, -30.74950257331004977, -29.92651530838623586 ) ) ;
#53161 = CARTESIAN_POINT ( 'NONE',  ( 0.5839879882012695145, 47.48620708510746624, -6.251708210201584848 ) ) ;
#53162 = B_SPLINE_CURVE_WITH_KNOTS ( 'NONE', 3,
 ( #35078, #30653, #30978, #11896, #26269, #7449, #10958, #44798, #25972, #39796, #40402, #16262, #49460, #21268, #12202, #59463, #50384, #25349, #50088 ),
 .UNSPECIFIED., .F., .F.,
 ( 4, 3, 3, 3, 3, 3, 4 ),
 ( 1.157434093048479169E-16, 0.0002618519381806257000, 0.0003927759815485975473, 0.0005237000248299427795, 0.0006546240681324977167, 0.0007855481115631319502, 0.0009699050456655103998 ),
 .UNSPECIFIED. ) ;
#53163 = ORIENTED_EDGE ( 'NONE', *, *, #32852, .T. ) ;
#53164 =( REPRESENTATION_RELATIONSHIP ('NONE','NONE', #44881, #6760 ) REPRESENTATION_RELATIONSHIP_WITH_TRANSFORMATION ( #48072 )SHAPE_REPRESENTATION_RELATIONSHIP( ) );
#53165 = DIRECTION ( 'NONE',  ( 1.000000000000000000, 0.000000000000000000, 0.000000000000000000 ) ) ;
#53166 = ORIENTED_EDGE ( 'NONE', *, *, #50669, .F. ) ;
#53167 = EDGE_CURVE ( 'NONE', #10577, #46370, #20481, .T. ) ;
#53168 = EDGE_CURVE ( 'NONE', #42991, #11351, #52424, .T. ) ;
#53169 = CARTESIAN_POINT ( 'NONE',  ( 2.600000000000000533, -11.64055411052240352, -1.199999999999999956 ) ) ;
#53170 = ORIENTED_EDGE ( 'NONE', *, *, #47612, .T. ) ;
#53171 = CARTESIAN_POINT ( 'NONE',  ( 0.5809828226811553087, -24.41822904836894637, -41.20389530892332886 ) ) ;
#53172 = EDGE_CURVE ( 'NONE', #48312, #3705, #3882, .T. ) ;
#53173 = CARTESIAN_POINT ( 'NONE',  ( 5.896782393890504181, -20.11283288166117345, 0.006352352428115353410 ) ) ;
#53174 = CARTESIAN_POINT ( 'NONE',  ( 0.9790850452238869517, 40.43297707001163843, 11.02323434927842172 ) ) ;
#53175 = CARTESIAN_POINT ( 'NONE',  ( 0.5839879327111913154, -37.94312859586436559, 29.22928252017501549 ) ) ;
#53176 = ORIENTED_EDGE ( 'NONE', *, *, #40986, .T. ) ;
#53177 = CARTESIAN_POINT ( 'NONE',  ( 5.910764540655177868, 14.90587032029957193, 13.50245416446859714 ) ) ;
#53178 = B_SPLINE_CURVE_WITH_KNOTS ( 'NONE', 3,
 ( #8469, #27599, #56699, #9099 ),
 .UNSPECIFIED., .F., .F.,
 ( 4, 4 ),
 ( 0.000000000000000000, 0.004442905043737214836 ),
 .UNSPECIFIED. ) ;
#53179 = ORIENTED_EDGE ( 'NONE', *, *, #19339, .F. ) ;
#53180 = DIRECTION ( 'NONE',  ( -1.000000000000000000, -0.000000000000000000, -0.000000000000000000 ) ) ;
#53181 = EDGE_CURVE ( 'NONE', #52962, #47950, #37083, .T. ) ;
#53182 = B_SPLINE_CURVE_WITH_KNOTS ( 'NONE', 3,
 ( #49070, #6423, #39699, #21180 ),
 .UNSPECIFIED., .F., .F.,
 ( 4, 4 ),
 ( 0.000000000000000000, 0.005004741218457413668 ),
 .UNSPECIFIED. ) ;
#53183 = VERTEX_POINT ( 'NONE', #42753 ) ;
#53184 = ORIENTED_EDGE ( 'NONE', *, *, #50087, .T. ) ;
#53185 = CARTESIAN_POINT ( 'NONE',  ( 0.8554163680231816613, -0.6539261334255772606, 46.91244881397518895 ) ) ;
#53186 = CARTESIAN_POINT ( 'NONE',  ( 0.6027444965799114707, -30.51574894146176220, -38.47502543766692895 ) ) ;
#53187 = CARTESIAN_POINT ( 'NONE',  ( 0.1073791018717578927, -21.14095454447534550, -37.58707531572198235 ) ) ;
#53188 = ORIENTED_EDGE ( 'NONE', *, *, #45632, .T. ) ;
#53189 = CARTESIAN_POINT ( 'NONE',  ( 0.1158516988532803660, 43.31986377834537905, 8.386391420533449548 ) ) ;
#53190 = DIRECTION ( 'NONE',  ( 0.07836865515943411409, 0.6006129930017333196, 0.7956898808744532481 ) ) ;
#53191 = CARTESIAN_POINT ( 'NONE',  ( 0.1158516988532803799, -38.42203224407807483, 21.69538192952180822 ) ) ;
#53192 = ORIENTED_EDGE ( 'NONE', *, *, #46972, .T. ) ;
#53193 = VECTOR ( 'NONE', #983, 1000.000000000000000 ) ;
#53194 = ORIENTED_EDGE ( 'NONE', *, *, #56701, .T. ) ;
#53195 = AXIS2_PLACEMENT_3D ( 'NONE', #12744, #42187, #50923 ) ;
#53196 = CARTESIAN_POINT ( 'NONE',  ( 0.5980894510889448457, 5.583794302584615288, 47.78766676462078067 ) ) ;
#53197 = DIRECTION ( 'NONE',  ( 0.07500201931887537365, 0.1525301372901526897, 0.9854487578338805287 ) ) ;
#53198 = CARTESIAN_POINT ( 'NONE',  ( 3.531714409328638116, 0.2975961151483291212, -47.02729187627043217 ) ) ;
#53199 = CARTESIAN_POINT ( 'NONE',  ( 4.291220156522060236, 14.90393520085178558, -44.69073408251991708 ) ) ;
#53200 = CARTESIAN_POINT ( 'NONE',  ( 0.3676999524040366896, -42.45338881270437525, 11.98584004733023534 ) ) ;
#53201 = VERTEX_POINT ( 'NONE', #18631 ) ;
#53202 = DIRECTION ( 'NONE',  ( -0.000000000000000000, -0.000000000000000000, 1.000000000000000000 ) ) ;
#53203 = EDGE_LOOP ( 'NONE', ( #57779, #13535, #58820, #5533 ) ) ;
#53204 = CARTESIAN_POINT ( 'NONE',  ( 0.6023143664670691511, 12.19804739160196938, 46.53533348214995868 ) ) ;
#53205 = CARTESIAN_POINT ( 'NONE',  ( 0.7057020205115018818, -38.50899875908074677, 28.48867101281811287 ) ) ;
#53206 = CARTESIAN_POINT ( 'NONE',  ( 4.553261556744875094, 42.54662847375985280, -10.92355122382294752 ) ) ;
#53207 = CARTESIAN_POINT ( 'NONE',  ( 0.1365634738349420230, -32.13563235107024951, 30.23514102861263098 ) ) ;
#53208 = CARTESIAN_POINT ( 'NONE',  ( 4.975801465491694664, 43.22084481528220579, -20.67815041659094888 ) ) ;
#53209 =( NAMED_UNIT ( * ) PLANE_ANGLE_UNIT ( ) SI_UNIT ( $, .RADIAN. ) );
#53210 = DIRECTION ( 'NONE',  ( 0.09835009131224567436, 0.9855991218957013134, 0.1375559175655325372 ) ) ;
#53211 = ADVANCED_FACE ( 'NONE', ( #32421 ), #10286, .F. ) ;
#53212 = CARTESIAN_POINT ( 'NONE',  ( 0.1149546198390368201, 20.65158036586270995, -38.99306083671213230 ) ) ;
#53213 = CARTESIAN_POINT ( 'NONE',  ( 0.9762797500689124330, 15.53330887509137703, -38.92352888134260525 ) ) ;
#53214 = CARTESIAN_POINT ( 'NONE',  ( 0.7242486021783854921, -47.69731273660525517, 11.66095279470975399 ) ) ;
#53215 = CARTESIAN_POINT ( 'NONE',  ( -2.708315649062916552, -10.53288422393049473, -10.16016146078285054 ) ) ;
#53216 = B_SPLINE_CURVE_WITH_KNOTS ( 'NONE', 3,
 ( #57360, #24177, #9773, #28878, #40709, #41320 ),
 .UNSPECIFIED., .F., .F.,
 ( 4, 2, 4 ),
 ( 0.000000000000000000, 0.0002447195606305753966, 0.0004894391212611507933 ),
 .UNSPECIFIED. ) ;
#53217 = DIRECTION ( 'NONE',  ( 0.1024043820194936311, 0.6159418278945496539, 0.7811075516170142841 ) ) ;
#53218 = PLANE ( 'NONE',  #45190 ) ;
#53219 = CARTESIAN_POINT ( 'NONE',  ( 3.661921753702022997, 9.064111102371878559, -46.15704728162205583 ) ) ;
#53220 = EDGE_LOOP ( 'NONE', ( #13918, #38092, #15492, #16991 ) ) ;
#53221 = CARTESIAN_POINT ( 'NONE',  ( 4.956445790443998689, -5.251077430596073903, 46.79705371022326688 ) ) ;
#53222 = CARTESIAN_POINT ( 'NONE',  ( 5.959547316686252039, -12.49803383497738807, -16.28190225198614627 ) ) ;
#53223 = CARTESIAN_POINT ( 'NONE',  ( -6.057079549204054558, -12.94019084496072125, -14.26123038155309786 ) ) ;
#53224 = CARTESIAN_POINT ( 'NONE',  ( 3.660087539127332423, 10.60624038924657953, -46.85281175970442291 ) ) ;
#53225 = CARTESIAN_POINT ( 'NONE',  ( 6.999999999999991118, 80.00000000000001421, -7.414830285890871171E-32 ) ) ;
#53226 = ORIENTED_EDGE ( 'NONE', *, *, #36977, .T. ) ;
#53227 = CARTESIAN_POINT ( 'NONE',  ( 0.9757787079277429054, -37.17954582422755294, 21.42002160630809016 ) ) ;
#53228 = CARTESIAN_POINT ( 'NONE',  ( 5.894904586330512508, 18.99964780500594941, -6.598696488502509006 ) ) ;
#53229 = VECTOR ( 'NONE', #1659, 1000.000000000000114 ) ;
#53230 = ADVANCED_FACE ( 'NONE', ( #43372 ), #14323, .F. ) ;
#53231 = CARTESIAN_POINT ( 'NONE',  ( 0.8753041380234524160, 17.79089796329306239, 45.76704357430872960 ) ) ;
#53232 = CIRCLE ( 'NONE', #26231, 48.91267123290010943 ) ;
#53233 = ORIENTED_EDGE ( 'NONE', *, *, #38380, .T. ) ;
#53234 = CARTESIAN_POINT ( 'NONE',  ( 0.2885700199627522222, -31.05173037893222343, -29.91358789498772097 ) ) ;
#53235 = EDGE_CURVE ( 'NONE', #55695, #11438, #7191, .T. ) ;
#53236 = CARTESIAN_POINT ( 'NONE',  ( 0.3676999524040323597, 9.009680404095913531, 43.18305503711946614 ) ) ;
#53237 = ORIENTED_EDGE ( 'NONE', *, *, #20241, .T. ) ;
#53238 = EDGE_CURVE ( 'NONE', #44212, #50189, #52806, .T. ) ;
#53239 = CARTESIAN_POINT ( 'NONE',  ( 4.958415959904820980, -35.95869674887559597, 27.75204644607389426 ) ) ;
#53240 = ORIENTED_EDGE ( 'NONE', *, *, #6561, .T. ) ;
#53241 = CARTESIAN_POINT ( 'NONE',  ( 0.5800708057587378175, -17.74761804745370952, -44.48635630048018186 ) ) ;
#53242 = EDGE_CURVE ( 'NONE', #26618, #14, #44528, .T. ) ;
#53243 = VERTEX_POINT ( 'NONE', #20469 ) ;
#53244 = CARTESIAN_POINT ( 'NONE',  ( 4.549368137175248350, 0.000000000000000000, 0.000000000000000000 ) ) ;
#53245 = CARTESIAN_POINT ( 'NONE',  ( 0.5807400328401574052, 41.75144119563885425, 23.47602859900729655 ) ) ;
#53246 = ORIENTED_EDGE ( 'NONE', *, *, #61568, .F. ) ;
#53247 = DIRECTION ( 'NONE',  ( -1.000000000000000000, -1.836909530733573776E-16, 1.925929944387235853E-32 ) ) ;
#53248 = EDGE_LOOP ( 'NONE', ( #1150, #34191 ) ) ;
#53249 = CARTESIAN_POINT ( 'NONE',  ( 4.962356264823608143, 0.000000000000000000, 0.000000000000000000 ) ) ;
#53250 = CARTESIAN_POINT ( 'NONE',  ( -2.708315649062916552, 7.544341609839809948, 12.54007339125017317 ) ) ;
#53251 = SHAPE_REPRESENTATION ( 'hex nut gradec_iso_ISO - 4034 - M5 - N', ( #14677 ), #12915 ) ;
#53252 = LINE ( 'NONE', #33870, #4787 ) ;
#53253 = VERTEX_POINT ( 'NONE', #57728 ) ;
#53254 = CARTESIAN_POINT ( 'NONE',  ( 0.5848930533535030563, -7.620589013869776274, -46.27309915565679432 ) ) ;
#53255 = CARTESIAN_POINT ( 'NONE',  ( 3.221118495291109163, -36.34809063562757103, -24.77050114159895244 ) ) ;
#53256 = EDGE_CURVE ( 'NONE', #55855, #56918, #60225, .T. ) ;
#53257 = CARTESIAN_POINT ( 'NONE',  ( 0.5830081025819927598, 32.40478957890073985, -33.89928681741567118 ) ) ;
#53258 = CARTESIAN_POINT ( 'NONE',  ( 0.9730545539215883499, -42.47233286818622133, 6.101350888304490461 ) ) ;
#53259 = ORIENTED_EDGE ( 'NONE', *, *, #55490, .F. ) ;
#53260 = CARTESIAN_POINT ( 'NONE',  ( 0.9762797500689124330, 40.55021165774366665, -10.58324712448374605 ) ) ;
#53261 = EDGE_CURVE ( 'NONE', #29768, #60647, #15481, .T. ) ;
#53262 = CARTESIAN_POINT ( 'NONE',  ( -6.078075953587585900, -1.843738688193722997, 19.16757162232069689 ) ) ;
#53263 = ORIENTED_EDGE ( 'NONE', *, *, #12828, .T. ) ;
#53264 = CARTESIAN_POINT ( 'NONE',  ( 0.7764146366350251904, 46.35884964802752961, -7.134250695114612739 ) ) ;
#53265 = ORIENTED_EDGE ( 'NONE', *, *, #57338, .F. ) ;
#53266 = CARTESIAN_POINT ( 'NONE',  ( 4.553261556744873317, 6.787618719204111528, -43.39893775135914922 ) ) ;
#53267 = CARTESIAN_POINT ( 'NONE',  ( 0.9788927965476030835, 40.38195116180627053, -11.20868560524691127 ) ) ;
#53268 = ORIENTED_EDGE ( 'NONE', *, *, #7494, .T. ) ;
#53269 = CARTESIAN_POINT ( 'NONE',  ( 3.270143674763207553, -7.080034332678176945, -11.71453292426886783 ) ) ;
#53270 = CARTESIAN_POINT ( 'NONE',  ( -6.078726893082806448, -12.94330610022628214, -14.25709887966570832 ) ) ;
#53271 = CARTESIAN_POINT ( 'NONE',  ( 4.975610109902397937, 0.000000000000000000, 0.000000000000000000 ) ) ;
#53272 = CARTESIAN_POINT ( 'NONE',  ( 0.5797568599927149791, -39.01551438537359218, 26.01951087003197927 ) ) ;
#53273 = ORIENTED_EDGE ( 'NONE', *, *, #16706, .T. ) ;
#53274 = DIRECTION ( 'NONE',  ( 1.000000000000000000, 0.000000000000000000, 0.000000000000000000 ) ) ;
#53275 = DIRECTION ( 'NONE',  ( 1.000000000000000000, -0.000000000000000000, -0.000000000000000000 ) ) ;
#53276 = B_SPLINE_CURVE_WITH_KNOTS ( 'NONE', 3,
 ( #29347, #48452, #39090, #1140 ),
 .UNSPECIFIED., .F., .F.,
 ( 4, 4 ),
 ( 2.226610509583310728E-17, 0.004564976165746187711 ),
 .UNSPECIFIED. ) ;
#53277 = CONICAL_SURFACE ( 'NONE', #56271, 43.92652462719577500, 1.486293639869522343 ) ;
#53278 = CARTESIAN_POINT ( 'NONE',  ( -6.015611763856276717, 0.006214430185141332774, 18.84324252354755203 ) ) ;
#53279 = DIRECTION ( 'NONE',  ( -1.000000000000000000, -0.000000000000000000, -0.000000000000000000 ) ) ;
#53280 = AXIS2_PLACEMENT_3D ( 'NONE', #7258, #59582, #16691 ) ;
#53281 = EDGE_CURVE ( 'NONE', #4853, #11136, #34850, .T. ) ;
#53282 = CARTESIAN_POINT ( 'NONE',  ( 0.7762783648524375080, 33.23866576554886620, -34.49689442177313481 ) ) ;
#53283 = CARTESIAN_POINT ( 'NONE',  ( 5.959547316686252039, 19.82715097195162457, -5.308980600728250288 ) ) ;
#53284 = CARTESIAN_POINT ( 'NONE',  ( 4.956653778116966613, 0.000000000000000000, -48.09070567114147110 ) ) ;
#53285 = CARTESIAN_POINT ( 'NONE',  ( 0.8560838555295223751, 33.26091945577352504, 33.07694168205818386 ) ) ;
#53286 = CARTESIAN_POINT ( 'NONE',  ( 0.1149546198390366536, 39.63494256384228720, 19.39118080427653013 ) ) ;
#53287 = CARTESIAN_POINT ( 'NONE',  ( -6.016489644550736315, 4.881234076340374095, 18.19999694163065840 ) ) ;
#53288 = B_SPLINE_CURVE_WITH_KNOTS ( 'NONE', 3,
 ( #14077, #23454, #8413, #42580, #46979, #42281 ),
 .UNSPECIFIED., .F., .F.,
 ( 4, 2, 4 ),
 ( 5.637851296924622286E-18, 0.0002291472222819946974, 0.0004582944445639837569 ),
 .UNSPECIFIED. ) ;
#53289 = B_SPLINE_CURVE_WITH_KNOTS ( 'NONE', 3,
 ( #1050, #25472, #45240, #44013 ),
 .UNSPECIFIED., .F., .F.,
 ( 4, 4 ),
 ( 0.000000000000000000, 0.005004948556313808770 ),
 .UNSPECIFIED. ) ;
#53290 = AXIS2_PLACEMENT_3D ( 'NONE', #31437, #7609, #60232 ) ;
#53291 = CARTESIAN_POINT ( 'NONE',  ( -6.078457390727109555, 17.85037638348237010, 7.222089310270451534 ) ) ;
#53292 = CARTESIAN_POINT ( 'NONE',  ( 0.6016117650947689910, -45.38673806846551173, 18.75086829320185444 ) ) ;
#53293 = ORIENTED_EDGE ( 'NONE', *, *, #26769, .F. ) ;
#53294 = CARTESIAN_POINT ( 'NONE',  ( 0.5834872094924182795, 29.33699246747753264, -37.85980081020191079 ) ) ;
#53295 = CARTESIAN_POINT ( 'NONE',  ( 0.9790320750461913857, -1.486294019886972739, 41.88231204970227850 ) ) ;
#53296 = CARTESIAN_POINT ( 'NONE',  ( 0.7954196712028466232, 28.58653687859115067, 38.68220069891179946 ) ) ;
#53297 = ORIENTED_EDGE ( 'NONE', *, *, #40157, .T. ) ;
#53298 = CARTESIAN_POINT ( 'NONE',  ( 0.5807400328401637335, 47.41494605191452649, -6.791881299635107005 ) ) ;
#53299 = CARTESIAN_POINT ( 'NONE',  ( 3.221118495291109607, 26.69097583632542481, 34.96216853352267862 ) ) ;
#53300 = ORIENTED_EDGE ( 'NONE', *, *, #11377, .T. ) ;
#53301 = VERTEX_POINT ( 'NONE', #53640 ) ;
#53302 = CARTESIAN_POINT ( 'NONE',  ( 4.322998006666179727, -14.45630056002908503, -45.75942687572293011 ) ) ;
#53303 = EDGE_CURVE ( 'NONE', #5698, #10566, #58460, .T. ) ;
#53304 = ORIENTED_EDGE ( 'NONE', *, *, #29484, .T. ) ;
#53305 = CARTESIAN_POINT ( 'NONE',  ( 1.000110580585050091, -41.85483763260385359, 2.142440085572930197 ) ) ;
#53306 = ORIENTED_EDGE ( 'NONE', *, *, #33899, .F. ) ;
#53307 = EDGE_CURVE ( 'NONE', #46926, #38023, #14503, .T. ) ;
#53308 = ORIENTED_EDGE ( 'NONE', *, *, #21095, .T. ) ;
#53309 = FACE_OUTER_BOUND ( 'NONE', #39832, .T. ) ;
#53310 = EDGE_LOOP ( 'NONE', ( #5593, #19297, #13953, #47953 ) ) ;
#53311 = CARTESIAN_POINT ( 'NONE',  ( 0.5804410086790514622, -46.82762660194600102, -2.587129429332121422 ) ) ;
#53312 = CARTESIAN_POINT ( 'NONE',  ( 1.154321713695926954, 39.32643513900330134, 17.18284946700643090 ) ) ;
#53313 = CARTESIAN_POINT ( 'NONE',  ( 1.227938101723756947, -17.20315230597815059, -39.32113113558984452 ) ) ;
#53314 = ORIENTED_EDGE ( 'NONE', *, *, #56980, .T. ) ;
#53315 = FACE_OUTER_BOUND ( 'NONE', #41749, .T. ) ;
#53316 =( BOUNDED_SURFACE ( )  B_SPLINE_SURFACE ( 3, 1, ( 
 ( #43217, #58498 ),
 ( #48503, #43846 ),
 ( #5567, #52893 ),
 ( #43526, #34736 ) ),
 .UNSPECIFIED., .F., .F., .F. ) 
 B_SPLINE_SURFACE_WITH_KNOTS ( ( 4, 4 ),
 ( 2, 2 ),
 ( 0.000000000000000000, 1.000000000000000000 ),
 ( 0.000000000000000000, 1.000000000000000000 ),
 .UNSPECIFIED. ) 
 GEOMETRIC_REPRESENTATION_ITEM ( )  RATIONAL_B_SPLINE_SURFACE ( (
 ( 1.000000000000000000, 1.000000000000000000),
 ( 0.9953485035131437453, 0.8621029689291515030),
 ( 0.9953485035131437453, 0.8621029689291515030),
 ( 1.000000000000000000, 1.000000000000000000) ) ) 
 REPRESENTATION_ITEM ( '' )  SURFACE ( )  );
#53317 = B_SPLINE_CURVE_WITH_KNOTS ( 'NONE', 3,
 ( #29662, #38789, #57849, #38174, #14976, #34087 ),
 .UNSPECIFIED., .F., .F.,
 ( 4, 2, 4 ),
 ( 8.525499192591780946E-17, 0.0002293366620881460689, 0.0004586733241762069196 ),
 .UNSPECIFIED. ) ;
#53318 = CARTESIAN_POINT ( 'NONE',  ( 5.896782393890504181, -9.660289833039602314, 17.64100017628490136 ) ) ;
#53319 = EDGE_LOOP ( 'NONE', ( #41809, #17809, #10765, #56073 ) ) ;
#53320 = ORIENTED_EDGE ( 'NONE', *, *, #39485, .T. ) ;
#53321 = CARTESIAN_POINT ( 'NONE',  ( 0.1119898979215349782, 43.41448053468967316, 7.883158513875082818 ) ) ;
#53322 = CARTESIAN_POINT ( 'NONE',  ( 0.1313383488274121880, 41.48452234694097740, -11.77600546273727034 ) ) ;
#53323 = CARTESIAN_POINT ( 'NONE',  ( 4.962356264823608143, 0.000000000000000000, 0.000000000000000000 ) ) ;
#53324 = FACE_OUTER_BOUND ( 'NONE', #5669, .T. ) ;
#53325 = CARTESIAN_POINT ( 'NONE',  ( 0.5806925824938499181, -1.020860314012482561, -46.88475452172953339 ) ) ;
#53326 = EDGE_CURVE ( 'NONE', #41860, #52183, #32471, .T. ) ;
#53327 = VECTOR ( 'NONE', #21804, 1000.000000000000114 ) ;
#53328 = ORIENTED_EDGE ( 'NONE', *, *, #30877, .F. ) ;
#53329 = CARTESIAN_POINT ( 'NONE',  ( 0.1156867017252035112, -1.289351019103671669, -44.10533279802707796 ) ) ;
#53330 = CARTESIAN_POINT ( 'NONE',  ( 0.7764139734771259294, 46.59651765548695579, -5.367030211277017848 ) ) ;
#53331 = B_SPLINE_CURVE_WITH_KNOTS ( 'NONE', 3,
 ( #56813, #19248, #38670, #52117 ),
 .UNSPECIFIED., .F., .F.,
 ( 4, 4 ),
 ( 2.306275401152138554E-17, 0.004559932413162185935 ),
 .UNSPECIFIED. ) ;
#53332 = CARTESIAN_POINT ( 'NONE',  ( 0.5806925824938499181, 37.13995815321135296, -28.63295078613577971 ) ) ;
#53333 = CARTESIAN_POINT ( 'NONE',  ( 4.962356264823609031, -3.779019546646985361, -41.91604238389410853 ) ) ;
#53334 = ORIENTED_EDGE ( 'NONE', *, *, #35814, .F. ) ;
#53335 = CARTESIAN_POINT ( 'NONE',  ( 5.860006189529234355, 40.11385274514681498, 26.78264244998112176 ) ) ;
#53336 = CARTESIAN_POINT ( 'NONE',  ( 0.7242003506640013466, 33.61306414422924149, 35.79348534247477431 ) ) ;
#53337 = DIRECTION ( 'NONE',  ( 0.000000000000000000, 0.000000000000000000, -1.000000000000000000 ) ) ;
#53338 = CARTESIAN_POINT ( 'NONE',  ( 21.00000000000000355, 0.000000000000000000, 0.000000000000000000 ) ) ;
#53339 = EDGE_LOOP ( 'NONE', ( #1232, #44531, #50607, #24399 ) ) ;
#53340 = ORIENTED_EDGE ( 'NONE', *, *, #55119, .F. ) ;
#53341 = DIRECTION ( 'NONE',  ( 0.9848077530122079093, 0.1736481776669314414, -5.551115123125783935E-17 ) ) ;
#53342 = CARTESIAN_POINT ( 'NONE',  ( 50.00005079999999680, 0.000000000000000000, 3.000000000000000000 ) ) ;
#53343 = CARTESIAN_POINT ( 'NONE',  ( 0.9787284016396611275, 14.88741976570966585, -39.17525662517586937 ) ) ;
#53344 = CARTESIAN_POINT ( 'NONE',  ( 5.901764892641288895, -44.10106349911009715, 21.28585600080809925 ) ) ;
#53345 = PRODUCT_DEFINITION_SHAPE ( 'NONE', 'NONE',  #61993 ) ;
#53346 = CARTESIAN_POINT ( 'NONE',  ( 0.6041374136657475802, 29.42442150067197204, -38.05989626241401425 ) ) ;
#53347 = CARTESIAN_POINT ( 'NONE',  ( 2.643462169533613793, 4.896978544602148098, -47.78621045426870495 ) ) ;
#53348 = CARTESIAN_POINT ( 'NONE',  ( 4.956653778116975495, 3.690426056929986043, 47.94889704119053420 ) ) ;
#53349 = CARTESIAN_POINT ( 'NONE',  ( 0.8560838555295158248, 33.26091945577399400, -33.07694168205770069 ) ) ;
#53350 = EDGE_CURVE ( 'NONE', #13656, #28634, #28513, .T. ) ;
#53351 = CARTESIAN_POINT ( 'NONE',  ( 2.624215991343608501, -47.39206852872452913, -7.662883702705155287 ) ) ;
#53352 = CARTESIAN_POINT ( 'NONE',  ( 0.1103878639767399417, 30.45925431905113356, -30.52789484587422564 ) ) ;
#53353 = CARTESIAN_POINT ( 'NONE',  ( -6.016104459813371719, 17.41090761020836553, 7.206059014950146668 ) ) ;
#53354 = VERTEX_POINT ( 'NONE', #42342 ) ;
#53355 = CARTESIAN_POINT ( 'NONE',  ( 4.975801465491694664, 36.39623109580467997, -31.15993731089085017 ) ) ;
#53356 = CARTESIAN_POINT ( 'NONE',  ( 4.975801465491694664, 45.55012473237754023, -14.85979367497125381 ) ) ;
#53357 = CARTESIAN_POINT ( 'NONE',  ( -6.063463321072278589, 16.77106408806596960, 9.463184550322056410 ) ) ;
#53358 = CARTESIAN_POINT ( 'NONE',  ( 0.6845945791218023269, 37.34424629630195369, 28.38685944719991738 ) ) ;
#53359 = CARTESIAN_POINT ( 'NONE',  ( 2.301529144917016101, -46.71331407887430487, -11.18385659262662024 ) ) ;
#53360 = CARTESIAN_POINT ( 'NONE',  ( 0.5998501479064699549, -46.33007877220747872, 12.95623334615421740 ) ) ;
#53361 = EDGE_CURVE ( 'NONE', #30048, #61623, #51237, .T. ) ;
#53362 = FACE_OUTER_BOUND ( 'NONE', #49196, .T. ) ;
#53363 = CARTESIAN_POINT ( 'NONE',  ( 0.8557997880470606944, 19.17299735372068525, -43.90420959842161608 ) ) ;
#53364 = CARTESIAN_POINT ( 'NONE',  ( 2.281448460670572942, 32.98023336626282287, -34.83871297539670309 ) ) ;
#53365 = EDGE_CURVE ( 'NONE', #51774, #14204, #61397, .T. ) ;
#53366 = CARTESIAN_POINT ( 'NONE',  ( 0.8760168074886965917, -13.30888447662113094, 46.22580377597762435 ) ) ;
#53367 = CARTESIAN_POINT ( 'NONE',  ( 2.301430502907645170, -43.86847929982172900, -19.56449039932716616 ) ) ;
#53369 = ORIENTED_EDGE ( 'NONE', *, *, #29679, .T. ) ;
#53368 = CARTESIAN_POINT ( 'NONE',  ( 0.9968887458511656030, 10.46947792236095154, 41.61262323391473927 ) ) ;
#53370 = VERTEX_POINT ( 'NONE', #8797 ) ;
#53371 = CARTESIAN_POINT ( 'NONE',  ( 0.6064515330803592619, -24.63255479555527572, 39.90703672638513666 ) ) ;
#53372 = DIRECTION ( 'NONE',  ( 0.000000000000000000, -1.000000000000000000, 1.287488025362403787E-15 ) ) ;
#53373 = CARTESIAN_POINT ( 'NONE',  ( 0.1147471544378676211, 41.97320617314998970, 13.60889973581589274 ) ) ;
#53374 = B_SPLINE_CURVE_WITH_KNOTS ( 'NONE', 3,
 ( #11780, #55900, #31171, #7342 ),
 .UNSPECIFIED., .F., .F.,
 ( 4, 4 ),
 ( 3.469446951953614189E-18, 0.005013413432710145043 ),
 .UNSPECIFIED. ) ;
#53375 = ORIENTED_EDGE ( 'NONE', *, *, #1209, .T. ) ;
#53376 = CARTESIAN_POINT ( 'NONE',  ( 2.526552050251864134, 22.53110080776707491, -36.59987178591158852 ) ) ;
#53378 = DIRECTION ( 'NONE',  ( 0.07500201931887537365, 0.1791611824599123881, -0.9809566594899373770 ) ) ;
#53377 = AXIS2_PLACEMENT_3D ( 'NONE', #8567, #56185, #27693 ) ;
#53379 = CARTESIAN_POINT ( 'NONE',  ( -6.016104459813374383, 17.40682403289248370, 7.215917642689130496 ) ) ;
#53380 = ORIENTED_EDGE ( 'NONE', *, *, #13780, .T. ) ;
#53381 = ORIENTED_EDGE ( 'NONE', *, *, #59980, .T. ) ;
#53382 = CARTESIAN_POINT ( 'NONE',  ( 0.6031357023905875581, -24.01594909943237610, -41.68407605450304487 ) ) ;
#53383 =( NAMED_UNIT ( * ) SI_UNIT ( $, .STERADIAN. ) SOLID_ANGLE_UNIT ( ) );
#53384 = ADVANCED_FACE ( 'NONE', ( #47036 ), #29480, .F. ) ;
#53385 = CARTESIAN_POINT ( 'NONE',  ( -4.000000000000000000, -1.933795701539610556, -0.2488376576622980119 ) ) ;
#53386 = CARTESIAN_POINT ( 'NONE',  ( 0.5998501479064699549, -46.33007877220747872, 12.95623334615421740 ) ) ;
#53387 = CARTESIAN_POINT ( 'NONE',  ( 4.975610109902397937, 30.04451009524474969, 38.59762713269442713 ) ) ;
#53388 = EDGE_CURVE ( 'NONE', #33185, #2469, #37642, .T. ) ;
#53389 = CARTESIAN_POINT ( 'NONE',  ( 0.9790320750461907195, -41.05168775549098825, -8.431848253370196389 ) ) ;
#53390 = CARTESIAN_POINT ( 'NONE',  ( 0.6039202388192953519, 41.06127625758664834, -26.93576256479739683 ) ) ;
#53391 = ADVANCED_FACE ( 'NONE', ( #56398 ), #3425, .F. ) ;
#53392 = CARTESIAN_POINT ( 'NONE',  ( 0.6846871229502899947, -7.109010606687077072, -47.37786444808401143 ) ) ;
#53393 = VERTEX_POINT ( 'NONE', #52627 ) ;
#53394 = ORIENTED_EDGE ( 'NONE', *, *, #58450, .F. ) ;
#53395 = CARTESIAN_POINT ( 'NONE',  ( 0.2940133293163013084, 43.44929869380207776, -7.641923357035950382 ) ) ;
#53396 = CARTESIAN_POINT ( 'NONE',  ( 0.9730545539215883499, 42.47233286818616449, 6.101350888304794218 ) ) ;
#53397 = ORIENTED_EDGE ( 'NONE', *, *, #17377, .F. ) ;
#53398 = CARTESIAN_POINT ( 'NONE',  ( -6.010958268070873523, -13.31406649671971998, 13.33459572764752998 ) ) ;
#53399 = CARTESIAN_POINT ( 'NONE',  ( 0.8554163680231720024, -2.480940174720139613, -46.85136507041474374 ) ) ;
#53400 = CARTESIAN_POINT ( 'NONE',  ( 5.901463166500145796, -13.97174733644455635, -14.46748584610301513 ) ) ;
#53401 = LINE ( 'NONE', #44063, #51365 ) ;
#53402 = ADVANCED_FACE ( 'NONE', ( #33553 ), #37446, .F. ) ;
#53403 = VECTOR ( 'NONE', #18881, 1000.000000000000114 ) ;
#53404 = ORIENTED_EDGE ( 'NONE', *, *, #59660, .T. ) ;
#53405 = CARTESIAN_POINT ( 'NONE',  ( 0.8560838555295223751, -46.14148336882287538, -8.446084690930739214 ) ) ;
#53406 = CARTESIAN_POINT ( 'NONE',  ( 0.8554163680231720024, -13.02474486562579514, 45.07284652978080430 ) ) ;
#53407 = CARTESIAN_POINT ( 'NONE',  ( 4.962356264823609919, 39.89814050050791394, -13.39305724859256763 ) ) ;
#53408 = CARTESIAN_POINT ( 'NONE',  ( -2.739355103387247858, -5.801236230415786288, -13.75475282038642177 ) ) ;
#53409 = B_SPLINE_CURVE_WITH_KNOTS ( 'NONE', 3,
 ( #13475, #22864, #41683, #56051, #3731, #32582 ),
 .UNSPECIFIED., .F., .F.,
 ( 4, 2, 4 ),
 ( 7.372574772901430151E-18, 0.0002291472222819920411, 0.0004582944445639767096 ),
 .UNSPECIFIED. ) ;
#53410 = ORIENTED_EDGE ( 'NONE', *, *, #17821, .T. ) ;
#53411 = CARTESIAN_POINT ( 'NONE',  ( -6.016761891674564211, 18.20023637398605842, -4.880293656734773222 ) ) ;
#53412 = ORIENTED_EDGE ( 'NONE', *, *, #48923, .T. ) ;
#53413 = CARTESIAN_POINT ( 'NONE',  ( 4.975610109902397937, 0.000000000000000000, 0.000000000000000000 ) ) ;
#53414 = CARTESIAN_POINT ( 'NONE',  ( 0.1155031312995260795, 9.654200663125585891, 43.05505826366879063 ) ) ;
#53415 = ORIENTED_EDGE ( 'NONE', *, *, #14867, .T. ) ;
#53416 = CARTESIAN_POINT ( 'NONE',  ( 1.227938101723748288, -39.96870412324346944, 15.63977281655828300 ) ) ;
#53417 = CARTESIAN_POINT ( 'NONE',  ( 5.896278296736517710, -11.93494920661357561, -16.18900759929210764 ) ) ;
#53418 = CARTESIAN_POINT ( 'NONE',  ( 5.974727161628367256, -20.34732802718249545, 2.694421823322574738 ) ) ;
#53419 = AXIS2_PLACEMENT_3D ( 'NONE', #26083, #36430, #16694 ) ;
#53420 = CARTESIAN_POINT ( 'NONE',  ( -6.063463321072278589, -19.21612852159693929, -1.249342675545178638 ) ) ;
#53421 = LINE ( 'NONE', #34048, #57814 ) ;
#53422 = CARTESIAN_POINT ( 'NONE',  ( 4.975801465491695552, 0.000000000000000000, 0.000000000000000000 ) ) ;
#53423 = CARTESIAN_POINT ( 'NONE',  ( 0.2230388203127658953, -20.89822698305293613, 37.71673103297332119 ) ) ;
#53424 = CARTESIAN_POINT ( 'NONE',  ( -6.010958268070873523, -2.445171577615893987, 18.68413620842263612 ) ) ;
#53425 = VERTEX_POINT ( 'NONE', #13832 ) ;
#53426 = CARTESIAN_POINT ( 'NONE',  ( 4.956445790444029775, 29.98832127573299289, -36.30755619981957949 ) ) ;
#53427 = CARTESIAN_POINT ( 'NONE',  ( 0.9762797500689124330, 14.58899758184696971, -39.28722355604386252 ) ) ;
#53428 = CARTESIAN_POINT ( 'NONE',  ( 0.8560838555295158248, 3.785103201470073397, 46.75516899590838449 ) ) ;
#53429 = ORIENTED_EDGE ( 'NONE', *, *, #10021, .T. ) ;
#53430 = EDGE_CURVE ( 'NONE', #45197, #9105, #18428, .T. ) ;
#53431 = CARTESIAN_POINT ( 'NONE',  ( 2.624215991343608501, 34.92983774303012723, -32.93378783738812388 ) ) ;
#53432 = CARTESIAN_POINT ( 'NONE',  ( 0.3676999524040323597, -11.75791688508830646, -42.51707861373114383 ) ) ;
#53433 = CARTESIAN_POINT ( 'NONE',  ( 0.6064515330803568194, -44.53023827495938747, -14.71027583740118772 ) ) ;
#53434 = CARTESIAN_POINT ( 'NONE',  ( 5.895881250540457863, -13.97904524590158459, 14.46077368681693898 ) ) ;
#53435 = CARTESIAN_POINT ( 'NONE',  ( 0.6023143664670691511, 38.32505149877513162, -29.07782746490714487 ) ) ;
#53436 = ADVANCED_FACE ( 'NONE', ( #9408 ), #48329, .F. ) ;
#53437 = DIRECTION ( 'NONE',  ( -1.000000000000000000, -5.380183451256437165E-17, -1.298891185607909845E-16 ) ) ;
#53438 = CARTESIAN_POINT ( 'NONE',  ( 2.618530812446115519, -46.97577780651594281, -1.732942200722220161 ) ) ;
#53439 = B_SPLINE_CURVE_WITH_KNOTS ( 'NONE', 3,
 ( #13049, #2994, #3912, #22116, #41244, #3293 ),
 .UNSPECIFIED., .F., .F.,
 ( 4, 2, 4 ),
 ( 9.885284284422818887E-18, 0.0002445244328975394624, 0.0004890488657950690585 ),
 .UNSPECIFIED. ) ;
#53440 = DIRECTION ( 'NONE',  ( 0.07836865515943411409, -0.2656332009267449723, 0.9608836331491514837 ) ) ;
#53441 = EDGE_CURVE ( 'NONE', #52994, #53665, #19875, .T. ) ;
#53442 = CARTESIAN_POINT ( 'NONE',  ( 0.9780303403264782869, 28.90096030599704946, -30.34920273724279127 ) ) ;
#53444 = ORIENTED_EDGE ( 'NONE', *, *, #51597, .F. ) ;
#53443 = CARTESIAN_POINT ( 'NONE',  ( -6.001507490154110336, -7.196845540359293913, 17.41542759839262189 ) ) ;
#53445 = ORIENTED_EDGE ( 'NONE', *, *, #45629, .F. ) ;
#53446 = CARTESIAN_POINT ( 'NONE',  ( 5.960721111146673579, 16.28787783074227136, -12.49016043756454231 ) ) ;
#53447 = PLANE ( 'NONE',  #30471 ) ;
#53448 = CARTESIAN_POINT ( 'NONE',  ( 0.9762797500689124330, 40.55021165774351743, 10.58324712448433580 ) ) ;
#53449 = LINE ( 'NONE', #44413, #6464 ) ;
#53450 = CARTESIAN_POINT ( 'NONE',  ( 0.2230388203127621483, 17.20066002792360038, 39.54016926433980927 ) ) ;
#53451 = CARTESIAN_POINT ( 'NONE',  ( 0.8751705887134553219, 11.58504748649199811, -46.67919521768876479 ) ) ;
#53452 = ORIENTED_EDGE ( 'NONE', *, *, #15524, .F. ) ;
#53453 = ORIENTED_EDGE ( 'NONE', *, *, #27880, .T. ) ;
#53454 = CARTESIAN_POINT ( 'NONE',  ( 0.7764146366350218598, -38.15852726313939058, 27.27576343161479500 ) ) ;
#53455 = ADVANCED_FACE ( 'NONE', ( #55094 ), #42502, .T. ) ;
#53456 = CARTESIAN_POINT ( 'NONE',  ( -6.015611763856276717, 11.47596948473832690, -14.94556629257413327 ) ) ;
#53457 = LINE ( 'NONE', #4916, #21816 ) ;
#53458 = ADVANCED_FACE ( 'NONE', ( #59803 ), #50691, .F. ) ;
#53459 = ORIENTED_EDGE ( 'NONE', *, *, #14284, .T. ) ;
#53460 = AXIS2_PLACEMENT_3D ( 'NONE', #35095, #6850, #54152 ) ;
#53461 = CARTESIAN_POINT ( 'NONE',  ( 1.231276596079881047, 25.54232633153377208, -33.23952972879584422 ) ) ;
#53462 = EDGE_CURVE ( 'NONE', #12539, #43595, #418, .T. ) ;
#53463 = CARTESIAN_POINT ( 'NONE',  ( 1.227938101723756947, -20.72293514920776758, 37.58536632582772086 ) ) ;
#53464 = EDGE_LOOP ( 'NONE', ( #6706, #52585 ) ) ;
#53465 = CARTESIAN_POINT ( 'NONE',  ( 7.000000000000006217, 8.392413579938656024E-13, -80.00000000000001421 ) ) ;
#53466 = EDGE_LOOP ( 'NONE', ( #33310, #2805, #9285, #3192, #38821, #13076, #48255, #55953, #33879, #34092, #11826, #48332, #3146, #55098, #5766, #11585, #17193, #1562, #12692, #9579, #50160, #26728, #25124, #38172, #21836, #35262, #31920, #12903, #46281, #2111, #10138, #32095, #547, #59197, #36591, #45761, #25765, #22737, #17517, #27985, #42593, #55169, #47656, #58842, #46192, #32021, #27766, #14985, #17552, #44115, #47309, #49824, #52726, #28296, #55570, #61694, #38636, #20461, #28509, #24020, #9501, #43523, #32259, #48093, #59568, #48880, #60161, #31706, #2511, #32816, #14343, #20054, #33407, #42968, #1073, #60497, #28988, #29368, #9525, #41483, #15325, #19285, #1559, #26128, #48470, #61304, #49173, #12171, #17314, #40996, #37019, #59700, #91, #38510, #46269, #27937, #48402, #61104, #59118, #13819, #48185, #2698, #35851, #42789, #36580, #46184, #12712, #50698, #35624, #53859, #6012, #25551, #303, #32952, #10439, #22762, #13066, #57104, #43284, #19552, #15941, #13014, #26201, #41049, #39335, #19991, #22908, #22932, #47219, #60157, #30756, #53592, #34732, #41140, #9783, #14708, #4866, #46673, #38877, #6748, #4607, #10538, #23513, #31924, #26280, #51019, #16431, #10736, #33481, #22785 ) ) ;
#53467 = CARTESIAN_POINT ( 'NONE',  ( 0.5837157313716023754, -34.84153614343021133, 31.38955913593036939 ) ) ;
#53468 = DIRECTION ( 'NONE',  ( -1.000000000000000000, -0.000000000000000000, -0.000000000000000000 ) ) ;
#53469 = ORIENTED_EDGE ( 'NONE', *, *, #40784, .T. ) ;
#53470 = CARTESIAN_POINT ( 'NONE',  ( 0.7762783648524397284, -41.92424098267925814, -23.17763242108799915 ) ) ;
#53471 = DIRECTION ( 'NONE',  ( -1.000000000000000000, -0.000000000000000000, -0.000000000000000000 ) ) ;
#53472 = CARTESIAN_POINT ( 'NONE',  ( 0.5809828226811553087, 18.83114015454698631, 44.03860873105701046 ) ) ;
#53473 = CARTESIAN_POINT ( 'NONE',  ( 0.5839880159502329748, -38.02605095487699316, 29.12121614504449951 ) ) ;
#53474 = ADVANCED_FACE ( 'NONE', ( #35719 ), #46337, .F. ) ;
#53475 = ORIENTED_EDGE ( 'NONE', *, *, #30805, .T. ) ;
#53476 = CARTESIAN_POINT ( 'NONE',  ( -2.569797478183790229, 0.4487456364278817333, -14.62602397812940858 ) ) ;
#53477 = CARTESIAN_POINT ( 'NONE',  ( 0.6031356755773454870, -2.564066905512520764E-05, -48.10744332413212021 ) ) ;
#53478 = EDGE_LOOP ( 'NONE', ( #3625, #41964, #7824, #2849 ) ) ;
#53479 = DIRECTION ( 'NONE',  ( -1.000000000000000000, -0.000000000000000000, -0.000000000000000000 ) ) ;
#53480 = ORIENTED_EDGE ( 'NONE', *, *, #43067, .T. ) ;
#53481 = CARTESIAN_POINT ( 'NONE',  ( 0.5786265663353196143, 34.37803667029857735, -33.35675271369502326 ) ) ;
#53482 = ORIENTED_EDGE ( 'NONE', *, *, #8152, .T. ) ;
#53483 = CARTESIAN_POINT ( 'NONE',  ( 5.896782393890504181, 0.6784186533441023403, -20.10138888258239120 ) ) ;
#53484 = CARTESIAN_POINT ( 'NONE',  ( 0.9785694773339239649, 36.17119032496986364, -21.16554738695601046 ) ) ;
#53485 = CARTESIAN_POINT ( 'NONE',  ( 0.1064266418746776799, -21.07422140941981326, -37.62465821955093759 ) ) ;
#53486 = ORIENTED_EDGE ( 'NONE', *, *, #10181, .T. ) ;
#53487 = CARTESIAN_POINT ( 'NONE',  ( 4.956653778116973719, 21.75875759808707244, 42.88673967249138741 ) ) ;
#53488 = CARTESIAN_POINT ( 'NONE',  ( 4.833616638992208614, -15.29495699393695674, -43.64812679991114663 ) ) ;
#53489 = CARTESIAN_POINT ( 'NONE',  ( 0.3676999524040323597, -28.14442808720941969, 33.96824621564581292 ) ) ;
#53490 = ORIENTED_EDGE ( 'NONE', *, *, #58446, .F. ) ;
#53491 =( BOUNDED_SURFACE ( )  B_SPLINE_SURFACE ( 3, 1, ( 
 ( #28714, #13399 ),
 ( #32501, #24017 ),
 ( #9293, #61891 ),
 ( #52824, #14024 ) ),
 .UNSPECIFIED., .F., .F., .F. ) 
 B_SPLINE_SURFACE_WITH_KNOTS ( ( 4, 4 ),
 ( 2, 2 ),
 ( 0.000000000000000000, 1.000000000000000000 ),
 ( 0.000000000000000000, 1.000000000000000000 ),
 .UNSPECIFIED. ) 
 GEOMETRIC_REPRESENTATION_ITEM ( )  RATIONAL_B_SPLINE_SURFACE ( (
 ( 1.000000000000000000, 1.000000000000000000),
 ( 0.9754377213608244057, 0.9999580625633939235),
 ( 0.9754377213608244057, 0.9999580625633939235),
 ( 1.000000000000000000, 1.000000000000000000) ) ) 
 REPRESENTATION_ITEM ( '' )  SURFACE ( )  );
#53492 = VERTEX_POINT ( 'NONE', #54461 ) ;
#53493 = CARTESIAN_POINT ( 'NONE',  ( 0.7048096507298579061, 5.442192462018821786, 47.80151517212787837 ) ) ;
#53494 = CARTESIAN_POINT ( 'NONE',  ( 0.2940133293162984773, 24.57542356339362399, 36.63726390245101783 ) ) ;
#53495 = CARTESIAN_POINT ( 'NONE',  ( 2.788021980277358036, 6.069845295522647588E-12, -46.99417130740492610 ) ) ;
#53496 = CARTESIAN_POINT ( 'NONE',  ( 5.917102823773431552, -7.236410236534137397, 18.76496962268593549 ) ) ;
#53498 = VECTOR ( 'NONE', #14162, 1000.000000000000114 ) ;
#53497 = DIRECTION ( 'NONE',  ( 0.07439287786467665975, -0.1432402660415362516, 0.9868880006907374547 ) ) ;
#53499 = VERTEX_POINT ( 'NONE', #30672 ) ;
#53500 = CARTESIAN_POINT ( 'NONE',  ( 0.000000000000000000, 0.000000000000000000, 3.469446951953614189E-15 ) ) ;
#53501 = EDGE_LOOP ( 'NONE', ( #37279, #27969, #60394, #2996 ) ) ;
#53502 = VECTOR ( 'NONE', #13571, 1000.000000000000114 ) ;
#53503 = EDGE_CURVE ( 'NONE', #49420, #4994, #57429, .T. ) ;
#53504 = CARTESIAN_POINT ( 'NONE',  ( 0.3676999524040323597, -42.87209381266892194, 10.38913641457044434 ) ) ;
#53505 = CARTESIAN_POINT ( 'NONE',  ( 0.5804410086790514622, -1.020940616195395556, -46.88792522722239653 ) ) ;
#53506 = CARTESIAN_POINT ( 'NONE',  ( -6.078457390727109555, -16.13585499094657649, -10.50850582854918969 ) ) ;
#53507 = CARTESIAN_POINT ( 'NONE',  ( 0.8753041380234524160, 11.79227530596866025, 47.66634631457734628 ) ) ;
#53508 = CARTESIAN_POINT ( 'NONE',  ( 4.975801465491695552, -36.39623109580445259, -31.15993731089111662 ) ) ;
#53509 = ADVANCED_FACE ( 'NONE', ( #1537 ), #998, .F. ) ;
#53510 = SURFACE_STYLE_FILL_AREA ( #49442 ) ;
#53511 = CARTESIAN_POINT ( 'NONE',  ( 0.6845945791218023269, 40.79463988471306379, 23.15607646797107577 ) ) ;
#53512 =( BOUNDED_SURFACE ( )  B_SPLINE_SURFACE ( 3, 1, ( 
 ( #53734, #20563 ),
 ( #49067, #48444 ),
 ( #29957, #49369 ),
 ( #20268, #39695 ) ),
 .UNSPECIFIED., .F., .F., .F. ) 
 B_SPLINE_SURFACE_WITH_KNOTS ( ( 4, 4 ),
 ( 2, 2 ),
 ( 0.000000000000000000, 1.000000000000000000 ),
 ( 0.000000000000000000, 1.000000000000000000 ),
 .UNSPECIFIED. ) 
 GEOMETRIC_REPRESENTATION_ITEM ( )  RATIONAL_B_SPLINE_SURFACE ( (
 ( 1.000000000000000000, 1.000000000000000000),
 ( 0.7282232189291693025, 0.9929344683865674037),
 ( 0.7282232189291693025, 0.9929344683865674037),
 ( 1.000000000000000000, 1.000000000000000000) ) ) 
 REPRESENTATION_ITEM ( '' )  SURFACE ( )  );
#53513 = CARTESIAN_POINT ( 'NONE',  ( 3.238931869106854489, -42.95312220797016067, 1.828840280769237658 ) ) ;
#53514 = CARTESIAN_POINT ( 'NONE',  ( 0.5800708119828326126, 44.00606550371088588, -18.90714262039425719 ) ) ;
#53515 = EDGE_CURVE ( 'NONE', #219, #8563, #46479, .T. ) ;
#53516 = EDGE_CURVE ( 'NONE', #18712, #26439, #30362, .T. ) ;
#53517 = CARTESIAN_POINT ( 'NONE',  ( -2.569797478183783568, 12.44213550320653461, -7.701637110048551449 ) ) ;
#53518 = ADVANCED_FACE ( 'NONE', ( #6527 ), #57088, .F. ) ;
#53519 = CARTESIAN_POINT ( 'NONE',  ( -2.601141883200662974, 11.07005473184238653, -10.01245802505072113 ) ) ;
#53520 = CARTESIAN_POINT ( 'NONE',  ( 0.8557997880470690211, -43.90420959842193582, 19.17299735371994629 ) ) ;
#53521 = B_SPLINE_CURVE_WITH_KNOTS ( 'NONE', 3,
 ( #27106, #23036, #42463, #60914 ),
 .UNSPECIFIED., .F., .F.,
 ( 4, 4 ),
 ( 0.000000000000000000, 0.004442905043737215703 ),
 .UNSPECIFIED. ) ;
#53522 = CARTESIAN_POINT ( 'NONE',  ( 0.5786265663353196143, -47.89572889566445468, -0.7221568112311492760 ) ) ;
#53523 = EDGE_CURVE ( 'NONE', #12972, #11409, #17645, .T. ) ;
#53524 = ORIENTED_EDGE ( 'NONE', *, *, #29751, .T. ) ;
#53525 = LINE ( 'NONE', #1215, #37301 ) ;
#53526 = CARTESIAN_POINT ( 'NONE',  ( 0.1084644655670283647, 37.54424727804272521, 21.21700107124061674 ) ) ;
#53527 = CARTESIAN_POINT ( 'NONE',  ( 0.6041374136657476912, 12.61972904329536505, 46.42299778158159995 ) ) ;
#53528 = CARTESIAN_POINT ( 'NONE',  ( 2.185380717157383135, 40.27445918234111133, 17.79853197983303659 ) ) ;
#53529 = CARTESIAN_POINT ( 'NONE',  ( 5.896278296736517710, -19.93266788971473957, -2.686211163091726029 ) ) ;
#53530 = EDGE_LOOP ( 'NONE', ( #11660, #19514, #9746, #6075 ) ) ;
#53531 = CARTESIAN_POINT ( 'NONE',  ( 0.9730545539215883499, -37.40983423658487794, 21.01499094264535472 ) ) ;
#53532 = CARTESIAN_POINT ( 'NONE',  ( 0.9756008150404607004, 16.28894658522385086, -39.69644259322190294 ) ) ;
#53533 = CARTESIAN_POINT ( 'NONE',  ( -4.923482091946717709, -0.9563062221994661494, -2.999999999999945377 ) ) ;
#53534 = ORIENTED_EDGE ( 'NONE', *, *, #4134, .T. ) ;
#53535 = FACE_OUTER_BOUND ( 'NONE', #54481, .T. ) ;
#53536 = AXIS2_PLACEMENT_3D ( 'NONE', #32782, #56561, #51239 ) ;
#53537 = CARTESIAN_POINT ( 'NONE',  ( 0.8557997880470599172, 23.15977007032323343, 41.93815086860265495 ) ) ;
#53538 = ORIENTED_EDGE ( 'NONE', *, *, #2826, .F. ) ;
#53539 = CARTESIAN_POINT ( 'NONE',  ( 0.2279481005628808121, 41.62610996520416506, 14.62089108904256385 ) ) ;
#53540 = CIRCLE ( 'NONE', #11550, 0.09999999999999939493 ) ;
#53541 = ORIENTED_EDGE ( 'NONE', *, *, #52536, .F. ) ;
#53542 = CARTESIAN_POINT ( 'NONE',  ( 4.322998006666179727, -43.48102276965716584, 20.30542865297572064 ) ) ;
#53543 = ORIENTED_EDGE ( 'NONE', *, *, #30877, .T. ) ;
#53544 = CARTESIAN_POINT ( 'NONE',  ( 0.1156867017252034419, 29.75710594952617072, -32.58001615689993713 ) ) ;
#53545 = CARTESIAN_POINT ( 'NONE',  ( 0.6254087463353918963, 41.31312313681408455, -24.64672211239920330 ) ) ;
#53546 = ORIENTED_EDGE ( 'NONE', *, *, #34459, .T. ) ;
#53547 = AXIS2_PLACEMENT_3D ( 'NONE', #41371, #11616, #36664 ) ;
#53548 = ADVANCED_FACE ( 'NONE', ( #32548 ), #56621, .F. ) ;
#53549 = ORIENTED_EDGE ( 'NONE', *, *, #1761, .T. ) ;
#53550 = CARTESIAN_POINT ( 'NONE',  ( 0.9775691876210979014, 20.47097313734579060, -36.56874304375333651 ) ) ;
#53551 = CARTESIAN_POINT ( 'NONE',  ( 0.6000166863083106206, -45.32251430608278753, 18.91277818522109655 ) ) ;
#53552 = ADVANCED_FACE ( 'NONE', ( #23140 ), #61476, .F. ) ;
#53553 = ORIENTED_EDGE ( 'NONE', *, *, #50830, .T. ) ;
#53554 = CARTESIAN_POINT ( 'NONE',  ( 0.5806925824938499181, -20.23436166722466467, 42.30594485723624132 ) ) ;
#53555 = CARTESIAN_POINT ( 'NONE',  ( 4.553261556744875094, -33.59363643963393997, 28.30206982864213217 ) ) ;
#53556 = CARTESIAN_POINT ( 'NONE',  ( 0.6031357023905875581, 24.01594909943208123, 41.68407605450320830 ) ) ;
#53557 = CARTESIAN_POINT ( 'NONE',  ( 1.157643937452369043, -18.38969994869442459, -37.66724320137780069 ) ) ;
#53558 = EDGE_LOOP ( 'NONE', ( #51390, #8259, #231, #51075 ) ) ;
#53559 = CARTESIAN_POINT ( 'NONE',  ( 4.833616638992208614, -14.43699082351744600, 43.93936707042075085 ) ) ;
#53560 = CARTESIAN_POINT ( 'NONE',  ( 4.322998006666165516, -42.57894920390143056, 22.13465289016552973 ) ) ;
#53561 = ORIENTED_EDGE ( 'NONE', *, *, #656, .T. ) ;
#53562 = CARTESIAN_POINT ( 'NONE',  ( 0.5832655196449141322, -46.77552346137193950, -3.359402906465947858 ) ) ;
#53563 = ORIENTED_EDGE ( 'NONE', *, *, #26289, .F. ) ;
#53564 = DIRECTION ( 'NONE',  ( 0.000000000000000000, -1.000000000000000000, 0.000000000000000000 ) ) ;
#53565 = LINE ( 'NONE', #58571, #26971 ) ;
#53566 = ORIENTED_EDGE ( 'NONE', *, *, #53896, .T. ) ;
#53567 = DIRECTION ( 'NONE',  ( -1.000000000000000000, -0.000000000000000000, -0.000000000000000000 ) ) ;
#53568 = DIRECTION ( 'NONE',  ( 0.000000000000000000, 0.000000000000000000, -1.000000000000000000 ) ) ;
#53569 = CARTESIAN_POINT ( 'NONE',  ( 3.270143674763207553, 13.14781761974174579, -3.806843787665778578 ) ) ;
#53570 = ORIENTED_EDGE ( 'NONE', *, *, #33523, .T. ) ;
#53571 = CARTESIAN_POINT ( 'NONE',  ( 0.1158403557922069033, -40.91360538020781235, 16.52323218914656877 ) ) ;
#53572 = CARTESIAN_POINT ( 'NONE',  ( 0.9775691876210995668, 41.58336652501495223, -5.211270232511006739 ) ) ;
#53573 = EDGE_CURVE ( 'NONE', #12846, #32685, #49821, .T. ) ;
#53574 = CARTESIAN_POINT ( 'NONE',  ( -48.95476116535499500, 0.000000000000000000, 8.000000000000000000 ) ) ;
#53575 = CARTESIAN_POINT ( 'NONE',  ( 0.8551540677456739292, 17.49081417858787901, 44.61036085020956676 ) ) ;
#53576 = CARTESIAN_POINT ( 'NONE',  ( 3.727782113643636652, -9.118766182490292138, -43.00727704953018815 ) ) ;
#53577 = ADVANCED_FACE ( 'NONE', ( #26916 ), #13842, .F. ) ;
#53578 =( BOUNDED_SURFACE ( )  B_SPLINE_SURFACE ( 3, 1, ( 
 ( #56475, #373 ),
 ( #14519, #9179 ),
 ( #32385, #61471 ),
 ( #52701, #9799 ) ),
 .UNSPECIFIED., .F., .F., .F. ) 
 B_SPLINE_SURFACE_WITH_KNOTS ( ( 4, 4 ),
 ( 2, 2 ),
 ( 0.000000000000000000, 1.000000000000000000 ),
 ( 0.000000000000000000, 1.000000000000000000 ),
 .UNSPECIFIED. ) 
 GEOMETRIC_REPRESENTATION_ITEM ( )  RATIONAL_B_SPLINE_SURFACE ( (
 ( 1.000000000000000000, 1.000000000000000000),
 ( 0.7223157951917480446, 0.9931996967497186413),
 ( 0.7223157951917480446, 0.9931996967497186413),
 ( 1.000000000000000000, 1.000000000000000000) ) ) 
 REPRESENTATION_ITEM ( '' )  SURFACE ( )  );
#53579 = CARTESIAN_POINT ( 'NONE',  ( 5.960221823109900008, -17.77295928189562702, 10.26751639438337271 ) ) ;
#53580 = ADVANCED_FACE ( 'NONE', ( #55703 ), #32236, .F. ) ;
#53581 = EDGE_CURVE ( 'NONE', #1395, #10414, #29616, .T. ) ;
#53582 = DIRECTION ( 'NONE',  ( -1.000000000000000000, -0.000000000000000000, -0.000000000000000000 ) ) ;
#53583 = LINE ( 'NONE', #10705, #50426 ) ;
#53584 = CARTESIAN_POINT ( 'NONE',  ( -6.016489644550737204, 9.425415887801317893, -16.31649074174267255 ) ) ;
#53585 = AXIS2_PLACEMENT_3D ( 'NONE', #31818, #7998, #36216 ) ;
#53586 = CARTESIAN_POINT ( 'NONE',  ( 1.231276596079881047, 40.64579686208666232, -10.25650859035628315 ) ) ;
#53587 = DIRECTION ( 'NONE',  ( 0.000000000000000000, 0.000000000000000000, -1.000000000000000000 ) ) ;
#53588 = FACE_OUTER_BOUND ( 'NONE', #60863, .T. ) ;
#53589 = B_SPLINE_CURVE_WITH_KNOTS ( 'NONE', 3,
 ( #47091, #3520, #56763, #4131, #37698, #47694, #4738, #32368, #13890, #43015, #28267, #23270, #47384, #4430, #19203, #22970 ),
 .UNSPECIFIED., .F., .F.,
 ( 4, 3, 3, 3, 3, 4 ),
 ( 6.938893903907228378E-18, 0.0002724568934985554386, 0.0004086836638483802011, 0.0005449104342063607661, 0.0008173270854453615775, 0.001089761613562689876 ),
 .UNSPECIFIED. ) ;
#53590 = CARTESIAN_POINT ( 'NONE',  ( 4.956445790444005794, -27.49627641100061837, -38.22947597953034204 ) ) ;
#53591 = CARTESIAN_POINT ( 'NONE',  ( 0.5804410086790514622, -46.82762660194600102, -2.587129429332111208 ) ) ;
#53592 = ORIENTED_EDGE ( 'NONE', *, *, #8402, .T. ) ;
#53593 = CARTESIAN_POINT ( 'NONE',  ( 0.5819845901640502417, 29.51612926147670990, -37.72030663501125503 ) ) ;
#53594 = CARTESIAN_POINT ( 'NONE',  ( 4.967162193818130511, 0.000000000000000000, 0.000000000000000000 ) ) ;
#53595 = CARTESIAN_POINT ( 'NONE',  ( 2.528100132419515145, 5.404255688820265746, 41.62989069264931175 ) ) ;
#53596 = ORIENTED_EDGE ( 'NONE', *, *, #35598, .T. ) ;
#53597 = CARTESIAN_POINT ( 'NONE',  ( 4.549368137175248350, 38.59302160394725689, 18.79584381673547711 ) ) ;
#53598 = CARTESIAN_POINT ( 'NONE',  ( 0.2230388203127605384, -39.54016926433985901, 17.20066002792346538 ) ) ;
#53599 = ORIENTED_EDGE ( 'NONE', *, *, #48344, .F. ) ;
#53600 = ORIENTED_EDGE ( 'NONE', *, *, #39855, .F. ) ;
#53601 = FACE_OUTER_BOUND ( 'NONE', #38698, .T. ) ;
#53602 = VERTEX_POINT ( 'NONE', #41642 ) ;
#53603 = CARTESIAN_POINT ( 'NONE',  ( 4.834790513006555379, 45.58586227964580928, -12.43054709759575971 ) ) ;
#53604 = ORIENTED_EDGE ( 'NONE', *, *, #37649, .T. ) ;
#53605 = ORIENTED_EDGE ( 'NONE', *, *, #58965, .F. ) ;
#53606 = CARTESIAN_POINT ( 'NONE',  ( 0.1100247026804066219, 10.99745200874637518, 41.69861001364777309 ) ) ;
#53607 = B_SPLINE_CURVE_WITH_KNOTS ( 'NONE', 3,
 ( #12086, #17083, #45590, #26460, #31161, #21152 ),
 .UNSPECIFIED., .F., .F.,
 ( 4, 2, 4 ),
 ( 3.471140604459641645E-18, 0.0002291966416970817348, 0.0004583932833941600001 ),
 .UNSPECIFIED. ) ;
#53608 = ORIENTED_EDGE ( 'NONE', *, *, #43149, .T. ) ;
#53609 = CARTESIAN_POINT ( 'NONE',  ( 2.618530812446115519, -9.204197330483806283, -46.09782576976612489 ) ) ;
#53610 = CARTESIAN_POINT ( 'NONE',  ( 50.15577769773999961, 9.539392014169456147, 3.000000000000000000 ) ) ;
#53611 = CARTESIAN_POINT ( 'NONE',  ( 0.5997462898726536595, 41.43917033312134635, -26.35046094941917971 ) ) ;
#53612 = ORIENTED_EDGE ( 'NONE', *, *, #53812, .F. ) ;
#53613 = CARTESIAN_POINT ( 'NONE',  ( 4.553261556744875094, 0.000000000000000000, 0.000000000000000000 ) ) ;
#53614 = EDGE_CURVE ( 'NONE', #53393, #43245, #48465, .T. ) ;
#53615 = ORIENTED_EDGE ( 'NONE', *, *, #6379, .T. ) ;
#53616 = AXIS2_PLACEMENT_3D ( 'NONE', #3787, #55801, #50796 ) ;
#53617 = VERTEX_POINT ( 'NONE', #36953 ) ;
#53618 = CARTESIAN_POINT ( 'NONE',  ( 0.6031356755773454870, -18.40989784469888946, 44.44549206087150850 ) ) ;
#53619 = CARTESIAN_POINT ( 'NONE',  ( 0.9762797500689124330, 14.58899758184639595, 39.28722355604407568 ) ) ;
#53620 = CARTESIAN_POINT ( 'NONE',  ( 5.959547316686252039, -14.51128755440551465, 14.51632612601503602 ) ) ;
#53621 = AXIS2_PLACEMENT_3D ( 'NONE', #45908, #39666, #59655 ) ;
#53622 = CARTESIAN_POINT ( 'NONE',  ( 0.2885697896453111588, 0.8047882042606538944, -43.10898998017122352 ) ) ;
#53623 = EDGE_LOOP ( 'NONE', ( #44832, #45348, #35082, #55854 ) ) ;
#53624 = CARTESIAN_POINT ( 'NONE',  ( 0.5998501479064699549, -11.94461217097501837, 46.60114184914296942 ) ) ;
#53625 = CARTESIAN_POINT ( 'NONE',  ( 5.958863334805807099, 10.26388325355087616, -17.77512673691308720 ) ) ;
#53626 = CARTESIAN_POINT ( 'NONE',  ( 4.322998006666179727, 42.57894920390098292, 22.13465289016641790 ) ) ;
#53627 = CARTESIAN_POINT ( 'NONE',  ( 3.376099380956838925, 12.51418204574271087, -4.806623696325517336 ) ) ;
#53628 = ORIENTED_EDGE ( 'NONE', *, *, #20886, .F. ) ;
#53629 = CARTESIAN_POINT ( 'NONE',  ( 0.8551540677456739292, 41.03346287276427518, 24.74404575822789454 ) ) ;
#53630 = CARTESIAN_POINT ( 'NONE',  ( 0.1064266418746774856, 42.67882141624136239, 6.185136754498480549 ) ) ;
#53631 = FACE_OUTER_BOUND ( 'NONE', #53749, .T. ) ;
#53632 = CARTESIAN_POINT ( 'NONE',  ( 0.6026112563231247332, -35.15491935172932614, -34.28808306507691839 ) ) ;
#53633 = ORIENTED_EDGE ( 'NONE', *, *, #40745, .F. ) ;
#53634 = ORIENTED_EDGE ( 'NONE', *, *, #19903, .T. ) ;
#53635 = DIRECTION ( 'NONE',  ( 0.000000000000000000, 0.000000000000000000, -1.000000000000000000 ) ) ;
#53636 = CARTESIAN_POINT ( 'NONE',  ( 0.6001305935487315502, -34.38748867424737199, 33.64689939321881695 ) ) ;
#53637 = CARTESIAN_POINT ( 'NONE',  ( 0.9787464366903572133, 15.22736283113052913, -39.04435188474212026 ) ) ;
#53638 = CARTESIAN_POINT ( 'NONE',  ( -6.078726893082806448, -19.21623043802547315, 1.237145513439503297 ) ) ;
#53639 = CARTESIAN_POINT ( 'NONE',  ( 0.1073791018717483448, 33.91564619577807349, -26.63563652260133097 ) ) ;
#53640 = CARTESIAN_POINT ( 'NONE',  ( 0.3676999524040366896, -18.60775935196311082, -39.99627326667158655 ) ) ;
#53641 = ADVANCED_FACE ( 'NONE', ( #13137 ), #20242, .F. ) ;
#53642 = LINE ( 'NONE', #29862, #11018 ) ;
#53643 = DIRECTION ( 'NONE',  ( -0.1011922191286467598, -0.9788975924247133031, 0.1775377096081844075 ) ) ;
#53644 = CARTESIAN_POINT ( 'NONE',  ( 4.833616638992208614, -43.93936707042090717, -14.43699082351698415 ) ) ;
#53645 = EDGE_CURVE ( 'NONE', #41497, #7082, #40095, .T. ) ;
#53646 = CARTESIAN_POINT ( 'NONE',  ( 0.1092565886968785149, 30.27341312544114160, -30.71235995742708980 ) ) ;
#53647 = CARTESIAN_POINT ( 'NONE',  ( 5.960721111146673579, -2.685391721746187343, 20.34914600876570390 ) ) ;
#53648 = VERTEX_POINT ( 'NONE', #38805 ) ;
#53649 = EDGE_CURVE ( 'NONE', #17098, #55047, #11657, .T. ) ;
#53650 = CARTESIAN_POINT ( 'NONE',  ( 0.1152339509894530906, -7.262667307842109565, -43.52236613548078026 ) ) ;
#53651 = CARTESIAN_POINT ( 'NONE',  ( 4.956445790444004018, -45.27177431812773278, -12.96165499572285817 ) ) ;
#53652 = CARTESIAN_POINT ( 'NONE',  ( -6.078726893082806448, -8.903615017412541022, 17.07394743140630666 ) ) ;
#53653 = CARTESIAN_POINT ( 'NONE',  ( -6.016761891674565099, -17.41015286184807209, 7.207804629151251419 ) ) ;
#53654 = B_SPLINE_CURVE_WITH_KNOTS ( 'NONE', 3,
 ( #24387, #49118, #53488, #58190 ),
 .UNSPECIFIED., .F., .F.,
 ( 4, 4 ),
 ( 0.000000000000000000, 0.005014147105413705591 ),
 .UNSPECIFIED. ) ;
#53655 = CARTESIAN_POINT ( 'NONE',  ( 0.6031356219577718170, -23.97811961689716753, 41.70591683999463584 ) ) ;
#53656 = CARTESIAN_POINT ( 'NONE',  ( 0.6026112563231247332, 33.14369577886151319, -36.23584447784382689 ) ) ;
#53657 = CARTESIAN_POINT ( 'NONE',  ( 0.7954190325252784577, 23.29293489839735187, -42.08256085583550288 ) ) ;
#53658 = CARTESIAN_POINT ( 'NONE',  ( 0.9972139404380291339, 6.252633471303369106, 42.45145681504340018 ) ) ;
#53659 = DIRECTION ( 'NONE',  ( 0.000000000000000000, 0.000000000000000000, -1.000000000000000000 ) ) ;
#53660 = CIRCLE ( 'NONE', #19674, 42.92674063221959813 ) ;
#53661 = CARTESIAN_POINT ( 'NONE',  ( 2.528100132419515145, -26.16755375504030212, 32.82549175730883917 ) ) ;
#53662 = CARTESIAN_POINT ( 'NONE',  ( 0.6028777368367060907, 48.18512964921514197, 9.472756198667941163 ) ) ;
#53664 = ORIENTED_EDGE ( 'NONE', *, *, #21371, .F. ) ;
#53663 = DIRECTION ( 'NONE',  ( 0.07500201931887537365, -0.5805833823197799060, -0.8107389427381760383 ) ) ;
#53665 = VERTEX_POINT ( 'NONE', #14990 ) ;
#53666 = EDGE_CURVE ( 'NONE', #13203, #38048, #28067, .T. ) ;
#53667 = VECTOR ( 'NONE', #12538, 1000.000000000000227 ) ;
#53668 = CARTESIAN_POINT ( 'NONE',  ( 0.8557997880470690211, -44.60232077416674201, -17.48760788519264153 ) ) ;
#53669 = CARTESIAN_POINT ( 'NONE',  ( 0.5988103564986356764, -48.10388392110853317, 0.6065102550371687107 ) ) ;
#53670 = CARTESIAN_POINT ( 'NONE',  ( 0.1152339509894530906, 41.94616134658625128, 13.69168502199042514 ) ) ;
#53671 = VERTEX_POINT ( 'NONE', #20000 ) ;
#53672 = ADVANCED_FACE ( 'NONE', ( #543 ), #31026, .F. ) ;
#53673 = ORIENTED_EDGE ( 'NONE', *, *, #4082, .F. ) ;
#53674 = CARTESIAN_POINT ( 'NONE',  ( 0.1073791018717483448, 43.12183934961191056, -0.4849339620928847516 ) ) ;
#53675 = CARTESIAN_POINT ( 'NONE',  ( 0.5809828226811553087, 34.25055090842153760, 33.48000389720628789 ) ) ;
#53676 = CARTESIAN_POINT ( 'NONE',  ( 0.5832367798473377940, -41.34221369670669333, -24.18350431151206337 ) ) ;
#53677 =( BOUNDED_SURFACE ( )  B_SPLINE_SURFACE ( 3, 1, ( 
 ( #12788, #46001 ),
 ( #17467, #22470 ),
 ( #3044, #31879 ),
 ( #37208, #32186 ) ),
 .UNSPECIFIED., .F., .F., .F. ) 
 B_SPLINE_SURFACE_WITH_KNOTS ( ( 4, 4 ),
 ( 2, 2 ),
 ( 0.000000000000000000, 1.000000000000000000 ),
 ( 0.000000000000000000, 1.000000000000000000 ),
 .UNSPECIFIED. ) 
 GEOMETRIC_REPRESENTATION_ITEM ( )  RATIONAL_B_SPLINE_SURFACE ( (
 ( 1.000000000000000000, 1.000000000000000000),
 ( 0.7282232189291693025, 0.9929344683865674037),
 ( 0.7282232189291693025, 0.9929344683865674037),
 ( 1.000000000000000000, 1.000000000000000000) ) ) 
 REPRESENTATION_ITEM ( '' )  SURFACE ( )  );
#53678 = ORIENTED_EDGE ( 'NONE', *, *, #55163, .F. ) ;
#53679 = VERTEX_POINT ( 'NONE', #47879 ) ;
#53680 = DIRECTION ( 'NONE',  ( -1.000000000000000000, -0.000000000000000000, -0.000000000000000000 ) ) ;
#53681 = CARTESIAN_POINT ( 'NONE',  ( 1.154321485836934169, -11.90271791109283761, -41.23280395520819042 ) ) ;
#53682 = CARTESIAN_POINT ( 'NONE',  ( 2.706805983486679779, -10.92573265357083301, 42.63102719032760035 ) ) ;
#53683 = CARTESIAN_POINT ( 'NONE',  ( 0.5988103564986355654, 18.96890181990826463, 44.21009236284890420 ) ) ;
#53684 = CONICAL_SURFACE ( 'NONE', #25677, 2.041999999999999815, 1.047197551196591858 ) ;
#53685 = CARTESIAN_POINT ( 'NONE',  ( 2.299652685299200972, 43.60340470841921956, 22.42821487974374151 ) ) ;
#53686 = EDGE_CURVE ( 'NONE', #48274, #19623, #26467, .T. ) ;
#53687 = CARTESIAN_POINT ( 'NONE',  ( 0.1156867017252034974, 15.35615507261531043, -41.36582295399159648 ) ) ;
#53688 = ORIENTED_EDGE ( 'NONE', *, *, #34496, .T. ) ;
#53689 = ORIENTED_EDGE ( 'NONE', *, *, #34816, .T. ) ;
#53690 = CARTESIAN_POINT ( 'NONE',  ( 1.231276596079881047, 36.49189576017899839, -20.63051901543672884 ) ) ;
#53691 = CARTESIAN_POINT ( 'NONE',  ( 4.975801465491694664, 45.18341283946434572, 15.94009207553066787 ) ) ;
#53692 = ORIENTED_EDGE ( 'NONE', *, *, #49097, .F. ) ;
#53693 = DIRECTION ( 'NONE',  ( 0.09835009131224549395, -0.5996571005210464822, 0.7941905447268713392 ) ) ;
#53694 = CARTESIAN_POINT ( 'NONE',  ( 0.6016117650947689910, -7.493478393550796923, 48.53245136823285577 ) ) ;
#53695 = CARTESIAN_POINT ( 'NONE',  ( 3.678748215320119197, -40.32774817307750226, -27.79002593716545277 ) ) ;
#53696 = CARTESIAN_POINT ( 'NONE',  ( 0.5804410086790514622, -8.338934868870371275, -46.15172821366643774 ) ) ;
#53697 = ORIENTED_EDGE ( 'NONE', *, *, #23190, .F. ) ;
#53698 = CARTESIAN_POINT ( 'NONE',  ( 0.1073791018717578927, 5.147744207006301309, 42.81622261970996135 ) ) ;
#53699 = CARTESIAN_POINT ( 'NONE',  ( 4.956653778116991482, -8.845409907520609849, -47.27023054223761989 ) ) ;
#53700 = CARTESIAN_POINT ( 'NONE',  ( 5.959547316686252039, 2.675599016784533823, -20.35048796920733949 ) ) ;
#53701 = DIRECTION ( 'NONE',  ( 0.000000000000000000, 0.000000000000000000, 1.000000000000000000 ) ) ;
#53702 = EDGE_LOOP ( 'NONE', ( #53984, #27909, #26970 ) ) ;
#53703 = CARTESIAN_POINT ( 'NONE',  ( 5.959547316686252039, 20.52562247508876681, 0.003562808152977453395 ) ) ;
#53704 = AXIS2_PLACEMENT_3D ( 'NONE', #23944, #33361, #56516 ) ;
#53705 = CARTESIAN_POINT ( 'NONE',  ( 1.657374760986086049, -28.42509966000220345, -33.65864163288807731 ) ) ;
#53706 = ORIENTED_EDGE ( 'NONE', *, *, #43944, .T. ) ;
#53707 = CARTESIAN_POINT ( 'NONE',  ( 5.895596859100789899, -9.662743138698489886, 17.63971593444811603 ) ) ;
#53708 = CARTESIAN_POINT ( 'NONE',  ( 4.956653778116893783, -15.97476558431863758, -45.35992544608534160 ) ) ;
#53709 = PRESENTATION_LAYER_ASSIGNMENT (  '', '', ( #43761 ) ) ;
#53710 = VECTOR ( 'NONE', #56111, 1000.000000000000114 ) ;
#53711 = ORIENTED_EDGE ( 'NONE', *, *, #579, .F. ) ;
#53712 = CARTESIAN_POINT ( 'NONE',  ( 5.895596859100789899, -11.93344155749883662, -16.19015613903236428 ) ) ;
#53713 = LINE ( 'NONE', #44078, #32850 ) ;
#53714 = CARTESIAN_POINT ( 'NONE',  ( 4.975610109902397937, -33.30777373088901072, 35.81957029655259817 ) ) ;
#53715 = CARTESIAN_POINT ( 'NONE',  ( 0.1156867017252034557, 33.67904051480007155, -28.50728042584282917 ) ) ;
#53716 = CARTESIAN_POINT ( 'NONE',  ( 4.960386119450142850, -42.07286811692948447, 12.01291942401176271 ) ) ;
#53717 = CARTESIAN_POINT ( 'NONE',  ( 0.1073791018717578927, 16.95003405440313315, -39.65380858626198091 ) ) ;
#53718 = ORIENTED_EDGE ( 'NONE', *, *, #36389, .T. ) ;
#53720 = ADVANCED_FACE ( 'NONE', ( #43820 ), #16687, .F. ) ;
#53719 = DIRECTION ( 'NONE',  ( -1.000000000000000000, -0.000000000000000000, -0.000000000000000000 ) ) ;
#53721 = LINE ( 'NONE', #10855, #649 ) ;
#53722 = CARTESIAN_POINT ( 'NONE',  ( 3.660087539127315992, 48.00143792263127551, -1.881558488211890090 ) ) ;
#53723 = ORIENTED_EDGE ( 'NONE', *, *, #41824, .T. ) ;
#53724 = EDGE_CURVE ( 'NONE', #7202, #57990, #38187, .T. ) ;
#53725 = CARTESIAN_POINT ( 'NONE',  ( 0.7764146366350244133, 16.02283669739539462, -44.08298059158165216 ) ) ;
#53726 = CARTESIAN_POINT ( 'NONE',  ( 0.9730545539215892381, -16.88610103448586131, 39.44597740938055352 ) ) ;
#53727 = B_SPLINE_CURVE_WITH_KNOTS ( 'NONE', 3,
 ( #55018, #2398, #11841, #30919 ),
 .UNSPECIFIED., .F., .F.,
 ( 4, 4 ),
 ( 0.000000000000000000, 0.004442905043737216571 ),
 .UNSPECIFIED. ) ;
#53728 = CARTESIAN_POINT ( 'NONE',  ( 0.6252788684277201803, 10.25662847928439803, -48.02338912875260490 ) ) ;
#53729 = CARTESIAN_POINT ( 'NONE',  ( 0.7056313189692677845, -44.57575722724908474, -14.58596968236639668 ) ) ;
#53730 = CARTESIAN_POINT ( 'NONE',  ( 0.7762783648524391733, -28.45155609988356105, 38.54028518467411857 ) ) ;
#53731 = CARTESIAN_POINT ( 'NONE',  ( 0.1064266379913941241, -0.5615183164814757655, -43.12102052820964104 ) ) ;
#53732 = ADVANCED_FACE ( 'NONE', ( #24371 ), #20529, .F. ) ;
#53733 = CARTESIAN_POINT ( 'NONE',  ( -1.599999999999940359, -56.56854249492332087, -56.56854249492429432 ) ) ;
#53734 = CARTESIAN_POINT ( 'NONE',  ( 5.917102823773431552, -11.92306321980329464, -16.19661327278996055 ) ) ;
#53735 = CARTESIAN_POINT ( 'NONE',  ( 0.9722240741986380996, 29.92651525529375434, 30.74950262511610788 ) ) ;
#53736 = VECTOR ( 'NONE', #6054, 1000.000000000000114 ) ;
#53737 = FACE_OUTER_BOUND ( 'NONE', #22922, .T. ) ;
#53739 = ORIENTED_EDGE ( 'NONE', *, *, #18558, .T. ) ;
#53738 = CARTESIAN_POINT ( 'NONE',  ( 4.962356264823608143, 41.15374796524913847, 8.809348799718396350 ) ) ;
#53740 = ORIENTED_EDGE ( 'NONE', *, *, #30404, .F. ) ;
#53741 = CARTESIAN_POINT ( 'NONE',  ( 0.7044674535452954967, -47.71057267246434463, 11.64061759858144285 ) ) ;
#53742 = CARTESIAN_POINT ( 'NONE',  ( 0.5806925824938494740, -35.14454992382308518, -31.04968555389040219 ) ) ;
#53743 = CARTESIAN_POINT ( 'NONE',  ( 4.960386119450151732, -40.09630699761650163, -17.51349850330398539 ) ) ;
#53744 = EDGE_CURVE ( 'NONE', #57079, #24422, #41514, .T. ) ;
#53745 = CARTESIAN_POINT ( 'NONE',  ( 0.1135584504625008068, -23.24200312127439005, 37.50681728760683598 ) ) ;
#53746 = CARTESIAN_POINT ( 'NONE',  ( 5.959547316686252039, -18.96183906913538308, -7.858107265727685586 ) ) ;
#53747 = CARTESIAN_POINT ( 'NONE',  ( 0.7057020205115016598, -11.58334423512203948, -46.47981817772236468 ) ) ;
#53748 = B_SPLINE_CURVE_WITH_KNOTS ( 'NONE', 3,
 ( #60585, #12394, #17700, #55898 ),
 .UNSPECIFIED., .F., .F.,
 ( 4, 4 ),
 ( 8.673617379884035472E-19, 0.004042984057420974560 ),
 .UNSPECIFIED. ) ;
#53749 = EDGE_LOOP ( 'NONE', ( #51845, #54248, #30593, #1072 ) ) ;
#53750 = ORIENTED_EDGE ( 'NONE', *, *, #39290, .T. ) ;
#53751 = CARTESIAN_POINT ( 'NONE',  ( 1.227938101723756947, -42.43379953535190197, 6.439911493064418124 ) ) ;
#53752 =( BOUNDED_SURFACE ( )  B_SPLINE_SURFACE ( 3, 1, ( 
 ( #44193, #1222 ),
 ( #6516, #1843 ),
 ( #20970, #7455 ),
 ( #22513, #50389 ) ),
 .UNSPECIFIED., .F., .F., .F. ) 
 B_SPLINE_SURFACE_WITH_KNOTS ( ( 4, 4 ),
 ( 2, 2 ),
 ( 0.000000000000000000, 1.000000000000000000 ),
 ( 0.000000000000000000, 1.000000000000000000 ),
 .UNSPECIFIED. ) 
 GEOMETRIC_REPRESENTATION_ITEM ( )  RATIONAL_B_SPLINE_SURFACE ( (
 ( 1.000000000000000000, 1.000000000000000000),
 ( 0.7269869731126821222, 0.9931720237060910339),
 ( 0.7269869731126821222, 0.9931720237060910339),
 ( 1.000000000000000000, 1.000000000000000000) ) ) 
 REPRESENTATION_ITEM ( '' )  SURFACE ( )  );
#53753 = CIRCLE ( 'NONE', #26776, 2.500000000000000444 ) ;
#53754 = CARTESIAN_POINT ( 'NONE',  ( -19.02783903667571508, -7.790278942242345295, 1.821455418571972684 ) ) ;
#53755 = VECTOR ( 'NONE', #43282, 1000.000000000000000 ) ;
#53756 = CARTESIAN_POINT ( 'NONE',  ( 4.691466044806102076, -9.025781474741773280, 43.66525414675626848 ) ) ;
#53757 = ORIENTED_EDGE ( 'NONE', *, *, #51002, .T. ) ;
#53758 = LINE ( 'NONE', #59708, #50599 ) ;
#53759 = CARTESIAN_POINT ( 'NONE',  ( 4.553261556744873317, 27.56395660609696563, 34.20186927699770507 ) ) ;
#53760 = EDGE_LOOP ( 'NONE', ( #11721, #36093, #14385, #32539 ) ) ;
#53761 = CARTESIAN_POINT ( 'NONE',  ( 0.6067375320500714153, 28.59217831627016082, 38.42671567536863364 ) ) ;
#53762 = ORIENTED_EDGE ( 'NONE', *, *, #25894, .T. ) ;
#53763 = CARTESIAN_POINT ( 'NONE',  ( 0.5806925824938506953, -38.96949031362410665, -26.08833430941730924 ) ) ;
#53764 = CARTESIAN_POINT ( 'NONE',  ( 5.959547316686252039, 0.003562808152622182027, 20.52562247508876681 ) ) ;
#53765 = VERTEX_POINT ( 'NONE', #43190 ) ;
#53766 = CARTESIAN_POINT ( 'NONE',  ( 4.956653778116992370, 15.97476558431944937, -45.35992544608513555 ) ) ;
#53767 = CARTESIAN_POINT ( 'NONE',  ( 0.6000166863083106206, 46.77044519531211364, 14.97828220927751808 ) ) ;
#53768 = CARTESIAN_POINT ( 'NONE',  ( 0.9775691876210974574, 40.31814568763066831, 11.43594496755648926 ) ) ;
#53769 = CARTESIAN_POINT ( 'NONE',  ( -6.078726893082806448, -1.852420388636412119, -19.16670498475114570 ) ) ;
#53770 = EDGE_CURVE ( 'NONE', #58714, #58688, #51917, .T. ) ;
#53771 = B_SPLINE_CURVE_WITH_KNOTS ( 'NONE', 3,
 ( #15838, #5779, #29306, #24614, #1095, #43751 ),
 .UNSPECIFIED., .F., .F.,
 ( 4, 2, 4 ),
 ( 3.469446951953614189E-18, 0.0002447193893791685696, 0.0004894387787583336698 ),
 .UNSPECIFIED. ) ;
#53772 = ORIENTED_EDGE ( 'NONE', *, *, #37311, .F. ) ;
#53773 = ADVANCED_FACE ( 'NONE', ( #28138, #33476, #19370, #38488, #33790, #9971, #43500, #15904, #30915, #44734 ), #11203, .F. ) ;
#53774 = CARTESIAN_POINT ( 'NONE',  ( 1.227938101723757836, -10.28900963485409292, 41.66816631169188412 ) ) ;
#53775 = CARTESIAN_POINT ( 'NONE',  ( 3.678834586032786458, -46.05790299361684959, 16.65178493312157570 ) ) ;
#53776 = ORIENTED_EDGE ( 'NONE', *, *, #52111, .F. ) ;
#53777 = DIRECTION ( 'NONE',  ( 1.000000000000000000, 0.000000000000000000, 0.000000000000000000 ) ) ;
#53778 = ORIENTED_EDGE ( 'NONE', *, *, #7987, .T. ) ;
#53779 = CARTESIAN_POINT ( 'NONE',  ( 0.8751705887134423323, 41.19904111682474479, 24.81530984069222256 ) ) ;
#53780 = EDGE_CURVE ( 'NONE', #36466, #1395, #43739, .T. ) ;
#53781 = CIRCLE ( 'NONE', #26804, 43.92652462719577500 ) ;
#53782 = ORIENTED_EDGE ( 'NONE', *, *, #5210, .T. ) ;
#53783 = CARTESIAN_POINT ( 'NONE',  ( 0.3676999524040366896, 36.51379593394493384, -24.75264207750488055 ) ) ;
#53784 = CARTESIAN_POINT ( 'NONE',  ( 0.6021448801613057400, -30.41330595987364660, -38.55608848441529091 ) ) ;
#53785 = CARTESIAN_POINT ( 'NONE',  ( -6.078075953587585900, 16.78075473395859518, 9.444651650847811553 ) ) ;
#53786 = VERTEX_POINT ( 'NONE', #53766 ) ;
#53787 = CARTESIAN_POINT ( 'NONE',  ( 2.299652685299201416, -49.01654791059075222, -1.288315096129431403 ) ) ;
#53788 = CARTESIAN_POINT ( 'NONE',  ( 0.2940135542859015905, -38.03800455849015805, 22.34615756455018243 ) ) ;
#53789 = CARTESIAN_POINT ( 'NONE',  ( 4.956653778116990594, -3.690426056929668075, -47.94889704119055551 ) ) ;
#53790 = ORIENTED_EDGE ( 'NONE', *, *, #19497, .T. ) ;
#53791 = B_SPLINE_CURVE_WITH_KNOTS ( 'NONE', 3,
 ( #32350, #33515, #52905, #60946, #52590, #8513 ),
 .UNSPECIFIED., .F., .F.,
 ( 4, 2, 4 ),
 ( 1.843143693225357538E-18, 0.0002447193893791656423, 0.0004894387787583359467 ),
 .UNSPECIFIED. ) ;
#53792 = ORIENTED_EDGE ( 'NONE', *, *, #23207, .F. ) ;
#53793 = CARTESIAN_POINT ( 'NONE',  ( 4.975801465491694664, 47.10002938642141856, -8.787181743659651545 ) ) ;
#53794 = CARTESIAN_POINT ( 'NONE',  ( 0.8744876279028306332, -35.88078294188929362, -33.50999053799506555 ) ) ;
#53795 = CARTESIAN_POINT ( 'NONE',  ( 3.238931869106854045, 24.69728751010286061, -35.19033040238042531 ) ) ;
#53796 = CARTESIAN_POINT ( 'NONE',  ( 0.2111111111111110827, -9.497654031326126400, -1.199999999999999956 ) ) ;
#53797 = CARTESIAN_POINT ( 'NONE',  ( 5.910764540655177868, -7.242942773736444906, 18.76275615269627650 ) ) ;
#53798 = CARTESIAN_POINT ( 'NONE',  ( 3.407937589446174087, 2.242416846335791192, -13.51415833181185633 ) ) ;
#53799 = VERTEX_POINT ( 'NONE', #21210 ) ;
#53800 = ADVANCED_FACE ( 'NONE', ( #54081 ), #24623, .F. ) ;
#53801 = FACE_BOUND ( 'NONE', #4661, .T. ) ;
#53802 = CIRCLE ( 'NONE', #42854, 7.400000000000022560 ) ;
#53803 = ORIENTED_EDGE ( 'NONE', *, *, #52982, .F. ) ;
#53804 = CIRCLE ( 'NONE', #12851, 48.91267123290010943 ) ;
#53805 = ADVANCED_FACE ( 'NONE', ( #16209 ), #34398, .F. ) ;
#53806 = CARTESIAN_POINT ( 'NONE',  ( 4.963659409799330291, -44.62477100936219898, 3.403493583737159600 ) ) ;
#53807 = CARTESIAN_POINT ( 'NONE',  ( 3.783198216974388739, 43.00370179234474932, 1.726720072276125340 ) ) ;
#53808 = DIRECTION ( 'NONE',  ( 0.000000000000000000, 0.000000000000000000, -1.000000000000000000 ) ) ;
#53809 = B_SPLINE_CURVE_WITH_KNOTS ( 'NONE', 3,
 ( #6208, #33848, #43250, #57292, #25045, #5901 ),
 .UNSPECIFIED., .F., .F.,
 ( 4, 2, 4 ),
 ( 1.823721537572523311E-17, 0.0002293755540694312914, 0.0004587511081388443140 ),
 .UNSPECIFIED. ) ;
#53810 = CARTESIAN_POINT ( 'NONE',  ( 4.975801465491695552, -21.70134120755170315, -42.71626295676257001 ) ) ;
#53811 = CARTESIAN_POINT ( 'NONE',  ( 3.238931869106853600, 32.96367555688112105, -27.59912060131738087 ) ) ;
#53812 = EDGE_CURVE ( 'NONE', #9480, #37185, #57108, .T. ) ;
#53813 =( LENGTH_UNIT ( ) NAMED_UNIT ( * ) SI_UNIT ( .MILLI., .METRE. ) );
#53814 = CARTESIAN_POINT ( 'NONE',  ( 5.860006189529234355, 47.30296539008838153, -9.426589201135005425 ) ) ;
#53815 = B_SPLINE_CURVE_WITH_KNOTS ( 'NONE', 3,
 ( #17817, #45411, #8096, #41631 ),
 .UNSPECIFIED., .F., .F.,
 ( 4, 4 ),
 ( 7.640664332323339286E-17, 0.005004741218457509078 ),
 .UNSPECIFIED. ) ;
#53816 = CARTESIAN_POINT ( 'NONE',  ( 0.9730545539215883499, -39.44597740938072405, 16.88610103448544209 ) ) ;
#53817 = CARTESIAN_POINT ( 'NONE',  ( -6.015611763856276717, -17.40650793417848519, 7.216738110653220239 ) ) ;
#53818 = CARTESIAN_POINT ( 'NONE',  ( 0.5804410086790514622, -41.60900809504538955, 21.63816760268401040 ) ) ;
#53819 = CARTESIAN_POINT ( 'NONE',  ( -2.000000000000009770, 3.464101615137749057, 0.000000000000000000 ) ) ;
#53820 = AXIS2_PLACEMENT_3D ( 'NONE', #37755, #32727, #5414 ) ;
#53821 = DIRECTION ( 'NONE',  ( 0.000000000000000000, 0.000000000000000000, -1.000000000000000000 ) ) ;
#53822 = ADVANCED_FACE ( 'NONE', ( #49711 ), #26626, .F. ) ;
#53823 = CARTESIAN_POINT ( 'NONE',  ( 2.185380717157383135, -19.12931034577501421, -39.65966828860555182 ) ) ;
#53824 = CARTESIAN_POINT ( 'NONE',  ( 0.5998501479064708430, 11.94461217097404493, 46.60114184914321811 ) ) ;
#53825 = CARTESIAN_POINT ( 'NONE',  ( 5.895881250540457863, 3.349849349787409114, 19.83194874292564336 ) ) ;
#53826 = EDGE_LOOP ( 'NONE', ( #24379, #16850 ) ) ;
#53827 = CONICAL_SURFACE ( 'NONE', #32859, 42.92674063221959813, 1.485477209440487556 ) ;
#53828 =( NAMED_UNIT ( * ) PLANE_ANGLE_UNIT ( ) SI_UNIT ( $, .RADIAN. ) );
#53829 = CARTESIAN_POINT ( 'NONE',  ( 0.5837157313716019313, -19.65754995710837960, -42.57719804385690310 ) ) ;
#53830 = CARTESIAN_POINT ( 'NONE',  ( 0.3676999524040366896, 24.55639947021014180, -36.64606156713571750 ) ) ;
#53831 = CARTESIAN_POINT ( 'NONE',  ( 0.1313383488274142974, -30.03864748494565973, 30.94058105930509939 ) ) ;
#53832 = CARTESIAN_POINT ( 'NONE',  ( 1.227938101723748288, 39.32113113558966688, 17.20315230597858047 ) ) ;
#53833 = VERTEX_POINT ( 'NONE', #5844 ) ;
#53834 = LINE ( 'NONE', #14429, #43317 ) ;
#53835 = DIRECTION ( 'NONE',  ( -1.000000000000000000, -1.836909530733573776E-16, 1.925929944387235853E-32 ) ) ;
#53836 = LINE ( 'NONE', #2140, #16549 ) ;
#53837 = ORIENTED_EDGE ( 'NONE', *, *, #61029, .F. ) ;
#53838 = CARTESIAN_POINT ( 'NONE',  ( -90.00000000000000000, 0.000000000000000000, 0.000000000000000000 ) ) ;
#53839 = CARTESIAN_POINT ( 'NONE',  ( 1.000433927950261870, 15.67543119259813267, 38.86771841231447411 ) ) ;
#53840 = ORIENTED_EDGE ( 'NONE', *, *, #12497, .F. ) ;
#53841 = AXIS2_PLACEMENT_3D ( 'NONE', #30340, #7681, #6504 ) ;
#53842 = DIRECTION ( 'NONE',  ( 0.1736481776669314137, -0.9848077530122077983, 5.551115123125779621E-17 ) ) ;
#53843 = CONICAL_SURFACE ( 'NONE', #2882, 42.08604991992415023, 1.569615340895231137 ) ;
#53844 = VERTEX_POINT ( 'NONE', #35327 ) ;
#53845 = CARTESIAN_POINT ( 'NONE',  ( 5.860006189529234355, 26.81109398084707252, 40.09484204000608543 ) ) ;
#53846 = ORIENTED_EDGE ( 'NONE', *, *, #39512, .F. ) ;
#53847 = DIRECTION ( 'NONE',  ( -0.07439287786467650709, 0.1432402660415221241, 0.9868880006907395641 ) ) ;
#53848 = FACE_OUTER_BOUND ( 'NONE', #23461, .T. ) ;
#53849 = EDGE_CURVE ( 'NONE', #33340, #20260, #31732, .T. ) ;
#53850 = ORIENTED_EDGE ( 'NONE', *, *, #14683, .F. ) ;
#53852 = CARTESIAN_POINT ( 'NONE',  ( 0.8554163680231720024, -18.91615390926536122, 42.93465493506153052 ) ) ;
#53851 = B_SPLINE_CURVE_WITH_KNOTS ( 'NONE', 3,
 ( #59612, #55217, #16720, #31117, #50225, #26413 ),
 .UNSPECIFIED., .F., .F.,
 ( 4, 2, 4 ),
 ( 1.176834411578111192E-16, 0.0002448718616795923374, 0.0004897437233590669304 ),
 .UNSPECIFIED. ) ;
#53853 = ORIENTED_EDGE ( 'NONE', *, *, #13738, .T. ) ;
#53854 = EDGE_CURVE ( 'NONE', #60939, #7367, #18319, .T. ) ;
#53855 = CARTESIAN_POINT ( 'NONE',  ( 0.1064266379913942490, -41.50637574965957555, 11.70292640078081803 ) ) ;
#53856 =( BOUNDED_SURFACE ( )  B_SPLINE_SURFACE ( 3, 1, ( 
 ( #46453, #37679 ),
 ( #47075, #56743 ),
 ( #47362, #4410 ),
 ( #23865, #3810 ) ),
 .UNSPECIFIED., .F., .F., .F. ) 
 B_SPLINE_SURFACE_WITH_KNOTS ( ( 4, 4 ),
 ( 2, 2 ),
 ( 0.000000000000000000, 1.000000000000000000 ),
 ( 0.000000000000000000, 1.000000000000000000 ),
 .UNSPECIFIED. ) 
 GEOMETRIC_REPRESENTATION_ITEM ( )  RATIONAL_B_SPLINE_SURFACE ( (
 ( 1.000000000000000000, 1.000000000000000000),
 ( 0.9952954269826590483, 0.8620686068821339365),
 ( 0.9952954269826590483, 0.8620686068821339365),
 ( 1.000000000000000000, 1.000000000000000000) ) ) 
 REPRESENTATION_ITEM ( '' )  SURFACE ( )  );
#53857 = CARTESIAN_POINT ( 'NONE',  ( 0.1073791018717483448, 33.91564619577807349, -26.63563652260133097 ) ) ;
#53858 = EDGE_CURVE ( 'NONE', #33488, #35234, #39416, .T. ) ;
#53859 = ORIENTED_EDGE ( 'NONE', *, *, #47385, .T. ) ;
#53861 = ADVANCED_FACE ( 'NONE', ( #30594 ), #33054, .F. ) ;
#53860 = CARTESIAN_POINT ( 'NONE',  ( 5.896278296736517710, 16.57877312360411892, 11.38732898139179284 ) ) ;
#53862 = CARTESIAN_POINT ( 'NONE',  ( 1.834102595619085063, -36.06423740592772731, -25.28969207377914685 ) ) ;
#53863 = VECTOR ( 'NONE', #9144, 1000.000000000000000 ) ;
#53864 = CARTESIAN_POINT ( 'NONE',  ( 0.6023143664670691511, 23.82663958122378389, 41.79259346737330816 ) ) ;
#53865 = CARTESIAN_POINT ( 'NONE',  ( 0.9762797500689124330, -18.09842611962761083, -37.79909730639192844 ) ) ;
#53867 = EDGE_CURVE ( 'NONE', #11621, #14410, #12439, .T. ) ;
#53866 = ORIENTED_EDGE ( 'NONE', *, *, #11057, .T. ) ;
#53868 = CARTESIAN_POINT ( 'NONE',  ( 3.407937589446174087, -7.970324840161883806, -11.14158115674381477 ) ) ;
#53869 = CARTESIAN_POINT ( 'NONE',  ( 4.335381028904201628, -37.95090345676129573, -30.97556737946744221 ) ) ;
#53870 = ORIENTED_EDGE ( 'NONE', *, *, #732, .F. ) ;
#53871 = CARTESIAN_POINT ( 'NONE',  ( 0.5817216825391124946, -46.81948311678352326, -2.677863492540627277 ) ) ;
#53872 = B_SPLINE_CURVE_WITH_KNOTS ( 'NONE', 3,
 ( #42944, #9710, #33537, #34154, #48244, #52612, #25048, #15353, #43252, #53227, #5297, #39477, #10337, #14735, #24739, #44192, #29429, #1221, #53531 ),
 .UNSPECIFIED., .F., .F.,
 ( 4, 3, 3, 3, 3, 3, 4 ),
 ( 9.813676791237319219E-18, 0.0002724573126191793876, 0.0004086839781548479893, 0.0005449106435901837631, 0.0006811373090491419169, 0.0008459866663933661218, 0.001010840725717210981 ),
 .UNSPECIFIED. ) ;
#53873 = ORIENTED_EDGE ( 'NONE', *, *, #48947, .T. ) ;
#53874 = AXIS2_PLACEMENT_3D ( 'NONE', #47228, #57825, #14959 ) ;
#53875 =( BOUNDED_SURFACE ( )  B_SPLINE_SURFACE ( 3, 1, ( 
 ( #39674, #39062 ),
 ( #34347, #58728 ),
 ( #10529, #1109 ),
 ( #29622, #9920 ) ),
 .UNSPECIFIED., .F., .F., .F. ) 
 B_SPLINE_SURFACE_WITH_KNOTS ( ( 4, 4 ),
 ( 2, 2 ),
 ( 0.000000000000000000, 1.000000000000000000 ),
 ( 0.000000000000000000, 1.000000000000000000 ),
 .UNSPECIFIED. ) 
 GEOMETRIC_REPRESENTATION_ITEM ( )  RATIONAL_B_SPLINE_SURFACE ( (
 ( 1.000000000000000000, 1.000000000000000000),
 ( 0.7282232189291694135, 0.9929344683865672927),
 ( 0.7282232189291694135, 0.9929344683865672927),
 ( 1.000000000000000000, 1.000000000000000000) ) ) 
 REPRESENTATION_ITEM ( '' )  SURFACE ( )  );
#53876 = CARTESIAN_POINT ( 'NONE',  ( 0.8760168074886960365, -33.37827814204101173, -34.63873394077476320 ) ) ;
#53877 = ADVANCED_FACE ( 'NONE', ( #31532 ), #39463, .F. ) ;
#53878 = CARTESIAN_POINT ( 'NONE',  ( 0.1139756605157202923, 25.56931991171277119, 35.96060481898923911 ) ) ;
#53879 = ORIENTED_EDGE ( 'NONE', *, *, #13268, .T. ) ;
#53880 = CARTESIAN_POINT ( 'NONE',  ( 0.9772918015221170318, -12.81218603359625519, -39.90218972426451671 ) ) ;
#53881 = CARTESIAN_POINT ( 'NONE',  ( 4.549368137175248350, 0.000000000000000000, 0.000000000000000000 ) ) ;
#53882 = CARTESIAN_POINT ( 'NONE',  ( 52.79846469724564884, 12.42986503907192564, 1.330138836193681895 ) ) ;
#53883 = CARTESIAN_POINT ( 'NONE',  ( 0.5987334363312694085, 49.04182530238752236, -2.542100997635586168 ) ) ;
#53884 = EDGE_CURVE ( 'NONE', #43795, #4007, #46270, .T. ) ;
#53885 = ORIENTED_EDGE ( 'NONE', *, *, #4848, .T. ) ;
#53886 = CARTESIAN_POINT ( 'NONE',  ( 0.1157506346131639274, -40.86450982400815235, 16.64429321558520058 ) ) ;
#53887 = CARTESIAN_POINT ( 'NONE',  ( 0.9784957157296378938, 41.50303087276166991, -5.816483935072919387 ) ) ;
#53888 = CYLINDRICAL_SURFACE ( 'NONE', #2822, 15.50000000000000000 ) ;
#53889 = CARTESIAN_POINT ( 'NONE',  ( 1.479689385636123067, -8.190458794601717329, -43.29549895776260371 ) ) ;
#53890 = AXIS2_PLACEMENT_3D ( 'NONE', #23885, #30113, #20120 ) ;
#53891 = CARTESIAN_POINT ( 'NONE',  ( 4.956445790443988031, 0.000000000000000000, 0.000000000000000000 ) ) ;
#53892 = AXIS2_PLACEMENT_3D ( 'NONE', #29976, #31211, #40033 ) ;
#53893 = CARTESIAN_POINT ( 'NONE',  ( -16.69218136511193151, -7.824295838635327627, 1.669278514306655969 ) ) ;
#53894 = CARTESIAN_POINT ( 'NONE',  ( 4.975610109902397937, -10.32228546579766260, 47.81108480154320972 ) ) ;
#53895 = CARTESIAN_POINT ( 'NONE',  ( 4.833616638992208614, 34.47248434257912919, -30.83411269743528038 ) ) ;
#53896 = EDGE_CURVE ( 'NONE', #43185, #9433, #16503, .T. ) ;
#53897 = CARTESIAN_POINT ( 'NONE',  ( 0.5786265663353153954, 46.45062944555893836, 11.69877690266672055 ) ) ;
#53898 = CARTESIAN_POINT ( 'NONE',  ( 4.975610109902397937, -10.32228546579766260, 47.81108480154320972 ) ) ;
#53899 = CARTESIAN_POINT ( 'NONE',  ( 0.5980894510889448457, -11.77356634613285813, -46.65000524237083113 ) ) ;
#53900 = EDGE_CURVE ( 'NONE', #22617, #22007, #46723, .T. ) ;
#53901 = CONICAL_SURFACE ( 'NONE', #39965, 4.000000000000000000, 1.047197551196595855 ) ;
#53902 = CARTESIAN_POINT ( 'NONE',  ( -6.078726893082806448, 17.85000270430350611, 7.222980321520863001 ) ) ;
#53903 = CARTESIAN_POINT ( 'NONE',  ( 0.6016118706126976079, -45.64818144247053766, 18.10509833663487811 ) ) ;
#53904 = ORIENTED_EDGE ( 'NONE', *, *, #30529, .F. ) ;
#53905 = VECTOR ( 'NONE', #12103, 1000.000000000000114 ) ;
#53906 = CARTESIAN_POINT ( 'NONE',  ( 0.2279481005628803125, -44.11266182516073542, -0.7593113800818089842 ) ) ;
#53907 = CARTESIAN_POINT ( 'NONE',  ( 0.9268187852002115479, 19.50810647315381274, -39.53717383350407744 ) ) ;
#53908 = CARTESIAN_POINT ( 'NONE',  ( 4.956445790443988031, 0.000000000000000000, 0.000000000000000000 ) ) ;
#53909 = VERTEX_POINT ( 'NONE', #60032 ) ;
#53910 = CARTESIAN_POINT ( 'NONE',  ( 0.9749527285493326811, 5.317382389863168690, 42.57770849153624226 ) ) ;
#53911 = CARTESIAN_POINT ( 'NONE',  ( 0.1157991065609916131, 4.155894141114022666, 43.92801963924112130 ) ) ;
#53912 = CARTESIAN_POINT ( 'NONE',  ( -6.079354080745853928, 3.074405391879413862, -19.00897121715283689 ) ) ;
#53913 = ORIENTED_EDGE ( 'NONE', *, *, #58669, .F. ) ;
#53914 = ORIENTED_EDGE ( 'NONE', *, *, #24745, .T. ) ;
#53915 = CARTESIAN_POINT ( 'NONE',  ( -6.078726893082806448, -8.909671472910916989, 17.07078778245215034 ) ) ;
#53916 = VERTEX_POINT ( 'NONE', #55944 ) ;
#53917 = CARTESIAN_POINT ( 'NONE',  ( 2.500000000000000000, -1.178949249685218748, -2.041999999999998039 ) ) ;
#53918 = B_SPLINE_CURVE_WITH_KNOTS ( 'NONE', 3,
 ( #19778, #29157, #636, #34184 ),
 .UNSPECIFIED., .F., .F.,
 ( 4, 4 ),
 ( 2.330832950083589181E-17, 0.004564976165746187711 ),
 .UNSPECIFIED. ) ;
#53919 = ORIENTED_EDGE ( 'NONE', *, *, #38793, .T. ) ;
#53920 = ORIENTED_EDGE ( 'NONE', *, *, #21945, .F. ) ;
#53921 = CARTESIAN_POINT ( 'NONE',  ( 0.6000166863083106206, -48.77118664543507975, -5.761495891223789023 ) ) ;
#53922 = ORIENTED_EDGE ( 'NONE', *, *, #5624, .T. ) ;
#53923 = CARTESIAN_POINT ( 'NONE',  ( 1.088313998177378839, 39.34193117255255601, 17.14007796983248966 ) ) ;
#53924 = CARTESIAN_POINT ( 'NONE',  ( 0.9790320750461900534, -17.56280114220697186, -38.05108603682009516 ) ) ;
#53925 = ORIENTED_EDGE ( 'NONE', *, *, #31397, .F. ) ;
#53926 = EDGE_CURVE ( 'NONE', #2469, #56932, #29497, .T. ) ;
#53927 = DIRECTION ( 'NONE',  ( 1.000000000000000000, 0.000000000000000000, 0.000000000000000000 ) ) ;
#53928 = AXIS2_PLACEMENT_3D ( 'NONE', #25417, #7222, #30420 ) ;
#53929 = CARTESIAN_POINT ( 'NONE',  ( 0.9722240750034584211, 39.86121765932399796, 15.88116978452995554 ) ) ;
#53930 = EDGE_CURVE ( 'NONE', #43245, #57549, #55014, .T. ) ;
#53931 = ORIENTED_EDGE ( 'NONE', *, *, #50777, .F. ) ;
#53932 = EDGE_CURVE ( 'NONE', #26593, #14707, #6276, .T. ) ;
#53933 = LINE ( 'NONE', #1013, #43614 ) ;
#53934 = VECTOR ( 'NONE', #47563, 1000.000000000000114 ) ;
#53935 = CARTESIAN_POINT ( 'NONE',  ( 4.958415959904820092, -4.043245302072359770, -45.24219403665024686 ) ) ;
#53936 = CARTESIAN_POINT ( 'NONE',  ( 0.5800708057587393718, 24.48933404430316685, -41.16170989303176952 ) ) ;
#53937 = CARTESIAN_POINT ( 'NONE',  ( 4.962356264823596597, 41.32726869310139506, 7.955655864260913646 ) ) ;
#53938 = EDGE_CURVE ( 'NONE', #41443, #20504, #42298, .T. ) ;
#53939 = ORIENTED_EDGE ( 'NONE', *, *, #141, .T. ) ;
#53940 = CARTESIAN_POINT ( 'NONE',  ( 0.1156495703730067298, -1.550490393351041218, -44.09692656831308710 ) ) ;
#53941 = CARTESIAN_POINT ( 'NONE',  ( -6.078726893082806448, 17.84743921491362073, -7.229312189875575889 ) ) ;
#53942 = B_SPLINE_CURVE_WITH_KNOTS ( 'NONE', 3,
 ( #7510, #8145, #21949, #13480, #32586, #7200 ),
 .UNSPECIFIED., .F., .F.,
 ( 4, 2, 4 ),
 ( 1.268633296668913999E-16, 0.0002450741128632347816, 0.0004901482257263427116 ),
 .UNSPECIFIED. ) ;
#53943 = CARTESIAN_POINT ( 'NONE',  ( 0.8560838555295158248, 45.47430759461114747, -11.50913475776619599 ) ) ;
#53944 = EDGE_CURVE ( 'NONE', #31779, #45251, #4849, .T. ) ;
#53945 = CARTESIAN_POINT ( 'NONE',  ( -6.017396004339686577, -2.458362590802920522, 18.68211039806562823 ) ) ;
#53946 = ORIENTED_EDGE ( 'NONE', *, *, #1116, .F. ) ;
#53947 = CARTESIAN_POINT ( 'NONE',  ( 5.960721111146673579, 14.50930005614996610, 14.51823969584104645 ) ) ;
#53948 = CARTESIAN_POINT ( 'NONE',  ( 2.526552050251863690, -25.19159344346098450, -34.82218744039929703 ) ) ;
#53949 = CARTESIAN_POINT ( 'NONE',  ( 2.009741617377216460, 8.458693230811739738, -43.21984019463820914 ) ) ;
#53950 = CARTESIAN_POINT ( 'NONE',  ( 0.9762797500689124330, 33.20096159360354449, -25.57383300261748360 ) ) ;
#53951 = AXIS2_PLACEMENT_3D ( 'NONE', #34427, #9999, #25019 ) ;
#53952 = ORIENTED_EDGE ( 'NONE', *, *, #16524, .F. ) ;
#53953 = VERTEX_POINT ( 'NONE', #22139 ) ;
#53954 = CARTESIAN_POINT ( 'NONE',  ( 0.5980894510889448457, -34.51330645350425641, 33.52121017007767279 ) ) ;
#53955 = CARTESIAN_POINT ( 'NONE',  ( 0.9780303403264770656, 14.75966257217395672, -39.22361500614967866 ) ) ;
#53956 = CARTESIAN_POINT ( 'NONE',  ( 0.8744876279028306332, -49.08725279547490317, 0.8897546699139438076 ) ) ;
#53957 = CARTESIAN_POINT ( 'NONE',  ( 0.1368894036331277653, 15.83533010450942768, 41.18377892331582046 ) ) ;
#53958 = CARTESIAN_POINT ( 'NONE',  ( 0.1158403557922069033, -31.72288257580944304, 30.66918695148641660 ) ) ;
#53959 = CARTESIAN_POINT ( 'NONE',  ( 5.960221823109900008, 17.77295928189555241, -10.26751639438349706 ) ) ;
#53960 = LINE ( 'NONE', #29553, #37835 ) ;
#53961 = CARTESIAN_POINT ( 'NONE',  ( 2.185380717157383135, -13.90069315816946904, -41.78026487218121332 ) ) ;
#53962 = CARTESIAN_POINT ( 'NONE',  ( 0.5998501479064699549, -18.89267974119636406, -44.24259072156078787 ) ) ;
#53963 = DIRECTION ( 'NONE',  ( 1.000000000000000000, 0.000000000000000000, 0.000000000000000000 ) ) ;
#53964 = B_SPLINE_CURVE_WITH_KNOTS ( 'NONE', 3,
 ( #16520, #21838, #16215, #2710, #40975, #7088, #55326, #40354, #26530, #50034, #30297, #44741, #22146, #35336, #60039, #31539, #1781, #35958, #25920 ),
 .UNSPECIFIED., .F., .F.,
 ( 4, 3, 3, 3, 3, 3, 4 ),
 ( 3.469552829456483146E-18, 0.0002612768053151684564, 0.0003919133833142928770, 0.0005225499612322577177, 0.0006531865391693348743, 0.0008112755173415179058, 0.0009693688056799707299 ),
 .UNSPECIFIED. ) ;
#53965 = CARTESIAN_POINT ( 'NONE',  ( 2.301529144917015213, 37.31001381748733792, -30.25186323939234612 ) ) ;
#53966 = CARTESIAN_POINT ( 'NONE',  ( 4.291220156522059348, 39.39367666905470600, 25.83654844981566967 ) ) ;
#53967 = LINE ( 'NONE', #11091, #15042 ) ;
#53968 = CARTESIAN_POINT ( 'NONE',  ( 5.880360259849752858, -15.46489389606785281, 45.41096578730621047 ) ) ;
#53969 = DIRECTION ( 'NONE',  ( 0.000000000000000000, 0.000000000000000000, -1.000000000000000000 ) ) ;
#53970 = CARTESIAN_POINT ( 'NONE',  ( 0.6064782688330851990, 45.41335037835364830, -11.70307881848435017 ) ) ;
#53971 = CARTESIAN_POINT ( 'NONE',  ( 0.9730545539215883499, -25.71816799638802920, 34.34678117142546938 ) ) ;
#53972 =( REPRESENTATION_RELATIONSHIP ('NONE','NONE', #44881, #19619 ) REPRESENTATION_RELATIONSHIP_WITH_TRANSFORMATION ( #47455 )SHAPE_REPRESENTATION_RELATIONSHIP( ) );
#53973 =( BOUNDED_SURFACE ( )  B_SPLINE_SURFACE ( 3, 1, ( 
 ( #6144, #54378 ),
 ( #54071, #2067 ),
 ( #40336, #45340 ),
 ( #58769, #11193 ) ),
 .UNSPECIFIED., .F., .F., .F. ) 
 B_SPLINE_SURFACE_WITH_KNOTS ( ( 4, 4 ),
 ( 2, 2 ),
 ( 0.000000000000000000, 1.000000000000000000 ),
 ( 0.000000000000000000, 1.000000000000000000 ),
 .UNSPECIFIED. ) 
 GEOMETRIC_REPRESENTATION_ITEM ( )  RATIONAL_B_SPLINE_SURFACE ( (
 ( 1.000000000000000000, 1.000000000000000000),
 ( 0.9953390228620291325, 0.8624445117761032620),
 ( 0.9953390228620291325, 0.8624445117761032620),
 ( 1.000000000000000000, 1.000000000000000000) ) ) 
 REPRESENTATION_ITEM ( '' )  SURFACE ( )  );
#53974 = EDGE_CURVE ( 'NONE', #47464, #38885, #45955, .T. ) ;
#53975 = CARTESIAN_POINT ( 'NONE',  ( 0.6021448801613057400, -30.82180960111880808, 38.23031770126069517 ) ) ;
#53976 = CARTESIAN_POINT ( 'NONE',  ( 0.5804410086790514622, 46.55025363952962181, 5.709092568075566199 ) ) ;
#53977 = CARTESIAN_POINT ( 'NONE',  ( 4.975610109902397937, -43.81605102859474954, 21.73943604138237973 ) ) ;
#53979 = VERTEX_POINT ( 'NONE', #152 ) ;
#53978 = CARTESIAN_POINT ( 'NONE',  ( 0.5809828226811553087, 41.20389530892342833, -24.41822904836879715 ) ) ;
#53980 = ORIENTED_EDGE ( 'NONE', *, *, #25662, .F. ) ;
#53981 = VECTOR ( 'NONE', #30358, 1000.000000000000000 ) ;
#53982 = CARTESIAN_POINT ( 'NONE',  ( 3.727782113643637096, 43.68415680130915035, -4.946940515572275210 ) ) ;
#53983 = CARTESIAN_POINT ( 'NONE',  ( 1.227938101723757836, 39.96870412324336996, 15.63977281655856366 ) ) ;
#53984 = ORIENTED_EDGE ( 'NONE', *, *, #42518, .T. ) ;
#53985 = ORIENTED_EDGE ( 'NONE', *, *, #45600, .T. ) ;
#53986 = CARTESIAN_POINT ( 'NONE',  ( 0.1102847568649952675, -11.07236323260782207, 41.67876919128903523 ) ) ;
#53987 = CARTESIAN_POINT ( 'NONE',  ( 0.6001305935487315502, 33.64689939321941381, -34.38748867424678224 ) ) ;
#53988 = CARTESIAN_POINT ( 'NONE',  ( 0.1102144999581333162, -37.40973521037476957, 21.45299314243928990 ) ) ;
#53989 = B_SPLINE_CURVE_WITH_KNOTS ( 'NONE', 3,
 ( #17097, #36208, #22396, #55903 ),
 .UNSPECIFIED., .F., .F.,
 ( 4, 4 ),
 ( 0.000000000000000000, 0.004446090762761374660 ),
 .UNSPECIFIED. ) ;
#53990 = ORIENTED_EDGE ( 'NONE', *, *, #14308, .T. ) ;
#53991 = ORIENTED_EDGE ( 'NONE', *, *, #3246, .T. ) ;
#53992 = CARTESIAN_POINT ( 'NONE',  ( 4.335381028904201628, 47.63237751920336649, 11.44174197980512631 ) ) ;
#53993 = CIRCLE ( 'NONE', #14063, 10.00000000000000000 ) ;
#53994 = CARTESIAN_POINT ( 'NONE',  ( 5.960721111146673579, -12.49016043756483363, 16.28787783074205819 ) ) ;
#53995 = CARTESIAN_POINT ( 'NONE',  ( 50.00005079999999680, 0.000000000000000000, 0.000000000000000000 ) ) ;
#53996 = CARTESIAN_POINT ( 'NONE',  ( 2.879087469061463178, -10.84989772776556016, 42.64248346520645327 ) ) ;
#53997 = CARTESIAN_POINT ( 'NONE',  ( 0.1129192098497447394, 4.719118110134695954, 43.87119455916095490 ) ) ;
#53998 = CARTESIAN_POINT ( 'NONE',  ( 0.8760168074887076939, -48.09529047980637273, 0.8912768426704632541 ) ) ;
#53999 = EDGE_CURVE ( 'NONE', #15275, #7236, #16885, .T. ) ;
#54000 = CARTESIAN_POINT ( 'NONE',  ( 0.1139756605157204311, 14.86525642157594440, -41.54490788551370173 ) ) ;
#54001 = EDGE_CURVE ( 'NONE', #22293, #19553, #44520, .T. ) ;
#54002 = VERTEX_POINT ( 'NONE', #29296 ) ;
#54003 = ORIENTED_EDGE ( 'NONE', *, *, #43161, .F. ) ;
#54004 = EDGE_CURVE ( 'NONE', #12663, #30079, #60522, .T. ) ;
#54005 = CARTESIAN_POINT ( 'NONE',  ( -6.078457390727109555, 7.798524762019481749, -17.60617853407368116 ) ) ;
#54006 = CARTESIAN_POINT ( 'NONE',  ( 1.231276596079881047, -2.246340108600348717, 41.85965512441018888 ) ) ;
#54007 = ORIENTED_EDGE ( 'NONE', *, *, #56055, .T. ) ;
#54008 = CARTESIAN_POINT ( 'NONE',  ( 4.322998006666165516, 35.39923696759012017, -32.40067585697761388 ) ) ;
#54009 = CARTESIAN_POINT ( 'NONE',  ( 0.5997462898726536595, -7.321308210775749004, 48.55872811583040516 ) ) ;
#54010 = EDGE_CURVE ( 'NONE', #34712, #48535, #16093, .T. ) ;
#54011 = CARTESIAN_POINT ( 'NONE',  ( 4.975801465491695552, 0.000000000000000000, 0.000000000000000000 ) ) ;
#54012 = CARTESIAN_POINT ( 'NONE',  ( 0.1147471544378675934, -41.01504251968592030, -16.27017134456798786 ) ) ;
#54013 = ORIENTED_EDGE ( 'NONE', *, *, #3030, .T. ) ;
#54014 = CARTESIAN_POINT ( 'NONE',  ( 0.9762797500689124330, -41.77809974471944088, 3.303810967046753255 ) ) ;
#54015 = CARTESIAN_POINT ( 'NONE',  ( 0.6008123274975391004, -35.57792977512935551, 33.84915750907875065 ) ) ;
#54016 = LINE ( 'NONE', #27003, #47805 ) ;
#54017 = CARTESIAN_POINT ( 'NONE',  ( -2.739355103387248747, 3.577672767447565683, 14.49302675496326565 ) ) ;
#54018 = ORIENTED_EDGE ( 'NONE', *, *, #15018, .T. ) ;
#54019 = CARTESIAN_POINT ( 'NONE',  ( 1.830465331921978800, -26.48837546677528110, -35.19576708937492526 ) ) ;
#54020 = CARTESIAN_POINT ( 'NONE',  ( 0.5998501479064699549, -47.76154736470754614, -5.759754759340617092 ) ) ;
#54021 = ORIENTED_EDGE ( 'NONE', *, *, #56554, .F. ) ;
#54022 = CARTESIAN_POINT ( 'NONE',  ( 4.549368137175248350, -42.82045902618770583, -3.018832571116409014 ) ) ;
#54023 = LINE ( 'NONE', #10216, #18433 ) ;
#54024 = ADVANCED_FACE ( 'NONE', ( #47492 ), #4540, .T. ) ;
#54025 = VERTEX_POINT ( 'NONE', #9569 ) ;
#54026 = DIRECTION ( 'NONE',  ( 1.000000000000000000, 0.000000000000000000, 0.000000000000000000 ) ) ;
#54027 = CARTESIAN_POINT ( 'NONE',  ( -6.015611763856276717, 16.31561949997088945, -9.427003116184000220 ) ) ;
#54028 = EDGE_CURVE ( 'NONE', #23595, #36860, #49692, .T. ) ;
#54029 = CARTESIAN_POINT ( 'NONE',  ( 0.2230388203127642022, 25.64246103889296435, -34.66629317821146117 ) ) ;
#54030 = CARTESIAN_POINT ( 'NONE',  ( -31.74999999999995737, 0.000000000000000000, 4.250000000000000000 ) ) ;
#54031 = CARTESIAN_POINT ( 'NONE',  ( 4.956445790443988031, 0.000000000000000000, 0.000000000000000000 ) ) ;
#54032 = CARTESIAN_POINT ( 'NONE',  ( 4.060580049360325461, 22.35095848363190285, 37.84048558385809002 ) ) ;
#54033 = AXIS2_PLACEMENT_3D ( 'NONE', #5598, #15359, #34466 ) ;
#54034 = CARTESIAN_POINT ( 'NONE',  ( 0.6845945791218023269, 16.04817208170968357, -44.07791616614580477 ) ) ;
#54035 = DIRECTION ( 'NONE',  ( 0.000000000000000000, 0.000000000000000000, -1.000000000000000000 ) ) ;
#54036 = CARTESIAN_POINT ( 'NONE',  ( 1.092182651088184464, 29.69432493936918505, 29.58053837977669787 ) ) ;
#54037 = DIRECTION ( 'NONE',  ( 1.000000000000000000, 1.836909530733573776E-16, 0.000000000000000000 ) ) ;
#54038 = DIRECTION ( 'NONE',  ( -1.000000000000000000, 0.000000000000000000, 0.000000000000000000 ) ) ;
#54039 = CARTESIAN_POINT ( 'NONE',  ( 1.830465331921978134, 16.36602852630565863, -40.89656667930132272 ) ) ;
#54040 = VECTOR ( 'NONE', #32332, 1000.000000000000000 ) ;
#54041 = EDGE_LOOP ( 'NONE', ( #12973, #46113, #25362, #61098 ) ) ;
#54042 = B_SPLINE_CURVE_WITH_KNOTS ( 'NONE', 3,
 ( #50702, #21912, #7792, #12219, #26597, #36336 ),
 .UNSPECIFIED., .F., .F.,
 ( 4, 2, 4 ),
 ( 1.182369072465671822E-16, 0.0002448718616795935842, 0.0004897437233590689904 ),
 .UNSPECIFIED. ) ;
#54043 = CARTESIAN_POINT ( 'NONE',  ( 4.962356264823600149, -32.75738977283805298, 26.42326651140453109 ) ) ;
#54044 = CARTESIAN_POINT ( 'NONE',  ( 0.6000166863083106206, 37.73145429715533794, -31.43502566135633458 ) ) ;
#54045 = CARTESIAN_POINT ( 'NONE',  ( 0.7948878604505663636, 48.93475821598755005, -4.010995592275964583 ) ) ;
#54046 = CARTESIAN_POINT ( 'NONE',  ( 0.1158403557922069033, 44.03589856812533299, -2.789255184022604972 ) ) ;
#54047 = B_SPLINE_CURVE_WITH_KNOTS ( 'NONE', 3,
 ( #47159, #51512, #38384, #61223 ),
 .UNSPECIFIED., .F., .F.,
 ( 4, 4 ),
 ( 0.000000000000000000, 0.004445488388166995118 ),
 .UNSPECIFIED. ) ;
#54048 = DIRECTION ( 'NONE',  ( 1.000000000000000000, 1.558861125776144859E-16, -3.851859888774471706E-32 ) ) ;
#54049 = CARTESIAN_POINT ( 'NONE',  ( 0.5998501479064699549, 17.92509395669108585, -44.64337787626229925 ) ) ;
#54050 =( NAMED_UNIT ( * ) PLANE_ANGLE_UNIT ( ) SI_UNIT ( $, .RADIAN. ) );
#54051 =( BOUNDED_SURFACE ( )  B_SPLINE_SURFACE ( 3, 1, ( 
 ( #60278, #36205 ),
 ( #59666, #7035 ),
 ( #2968, #17094 ),
 ( #12096, #17391 ) ),
 .UNSPECIFIED., .F., .F., .F. ) 
 B_SPLINE_SURFACE_WITH_KNOTS ( ( 4, 4 ),
 ( 2, 2 ),
 ( 0.000000000000000000, 1.000000000000000000 ),
 ( 0.000000000000000000, 1.000000000000000000 ),
 .UNSPECIFIED. ) 
 GEOMETRIC_REPRESENTATION_ITEM ( )  RATIONAL_B_SPLINE_SURFACE ( (
 ( 1.000000000000000000, 1.000000000000000000),
 ( 0.7211978278499968642, 0.9934217856018975334),
 ( 0.7211978278499968642, 0.9934217856018975334),
 ( 1.000000000000000000, 1.000000000000000000) ) ) 
 REPRESENTATION_ITEM ( '' )  SURFACE ( )  );
#54052 = EDGE_CURVE ( 'NONE', #47393, #47251, #10886, .T. ) ;
#54053 = CARTESIAN_POINT ( 'NONE',  ( 0.9730545539215892381, 29.98130006528861813, 30.69604515769660935 ) ) ;
#54054 = CARTESIAN_POINT ( 'NONE',  ( 0.5998501479064699549, -29.69975237324587169, -37.84527566984847624 ) ) ;
#54056 = VERTEX_POINT ( 'NONE', #38413 ) ;
#54055 = CARTESIAN_POINT ( 'NONE',  ( 4.975801465491695552, 0.000000000000000000, 0.000000000000000000 ) ) ;
#54057 = ORIENTED_EDGE ( 'NONE', *, *, #57977, .F. ) ;
#54058 = CARTESIAN_POINT ( 'NONE',  ( 0.5786265663353153954, -37.55861529268574373, 29.72999788434278656 ) ) ;
#54059 = CARTESIAN_POINT ( 'NONE',  ( 5.981074661064941900, -14.51919955600745737, 14.50705827991420804 ) ) ;
#54060 = CARTESIAN_POINT ( 'NONE',  ( 0.1102144999581333162, 16.38650952318852916, 39.88986724628640701 ) ) ;
#54061 = DIRECTION ( 'NONE',  ( 1.000000000000000000, 0.000000000000000000, 0.000000000000000000 ) ) ;
#54062 = CARTESIAN_POINT ( 'NONE',  ( 3.783278058412226308, -42.41041238787298795, 7.325100730114140646 ) ) ;
#54063 = CARTESIAN_POINT ( 'NONE',  ( 0.7954196712028472893, 41.21355366240430840, 24.79809944608789252 ) ) ;
#54064 = B_SPLINE_CURVE_WITH_KNOTS ( 'NONE', 3,
 ( #61574, #23083, #3328, #41583, #9275, #22459, #4552, #13381, #17764, #61876, #18694, #42213, #22766, #32801, #37829, #23386, #46908, #60967, #8975, #56880, #37195, #8651, #28084, #32481, #33110 ),
 .UNSPECIFIED., .F., .F.,
 ( 4, 3, 3, 3, 3, 3, 3, 3, 4 ),
 ( 5.057544569639794935E-18, 0.0005656085177311397484, 0.001131215744874499406, 0.001696821861372765699, 0.002262427090022498151, 0.002828031679238745492, 0.003393635864401604862, 0.003977030878808131623, 0.004561030005651158133 ),
 .UNSPECIFIED. ) ;
#54065 = ORIENTED_EDGE ( 'NONE', *, *, #14734, .F. ) ;
#54066 = VERTEX_POINT ( 'NONE', #44356 ) ;
#54067 = FACE_OUTER_BOUND ( 'NONE', #57326, .T. ) ;
#54068 = CARTESIAN_POINT ( 'NONE',  ( 0.1092565886968785843, -11.46097737058334864, -41.57372480460681174 ) ) ;
#54069 = CARTESIAN_POINT ( 'NONE',  ( 3.240649175237397372, -34.13167035129225013, -27.75417079338471282 ) ) ;
#54070 = ORIENTED_EDGE ( 'NONE', *, *, #26446, .F. ) ;
#54071 = CARTESIAN_POINT ( 'NONE',  ( 5.959828726073459926, -0.004526594003237118143, -20.52560994243598813 ) ) ;
#54072 = CARTESIAN_POINT ( 'NONE',  ( 0.5809828226811617480, 47.89273459658653564, 0.5448590168534191980 ) ) ;
#54073 = ORIENTED_EDGE ( 'NONE', *, *, #51454, .F. ) ;
#54074 = AXIS2_PLACEMENT_3D ( 'NONE', #54857, #51085, #2551 ) ;
#54075 = CARTESIAN_POINT ( 'NONE',  ( 7.000000000000016875, -56.56854249492410958, 56.56854249492351983 ) ) ;
#54076 = EDGE_CURVE ( 'NONE', #23849, #47109, #19105, .T. ) ;
#54077 = EDGE_LOOP ( 'NONE', ( #57011, #26449, #12816, #20963 ) ) ;
#54078 = CARTESIAN_POINT ( 'NONE',  ( 5.000000000000007994, -56.56854249492331377, -56.56854249492430142 ) ) ;
#54079 = DIRECTION ( 'NONE',  ( 0.09835009131224566048, 0.007732607185430591737, -0.9951218349151970122 ) ) ;
#54080 = ORIENTED_EDGE ( 'NONE', *, *, #22639, .T. ) ;
#54081 = FACE_OUTER_BOUND ( 'NONE', #24603, .T. ) ;
#54082 = CARTESIAN_POINT ( 'NONE',  ( 0.6039202388192953519, 46.66051417535179979, 15.30882522405896928 ) ) ;
#54083 = ADVANCED_FACE ( 'NONE', ( #21135 ), #12308, .F. ) ;
#54084 = CARTESIAN_POINT ( 'NONE',  ( 0.5838002273316443835, 41.54704836736078732, -23.82993264414519885 ) ) ;
#54085 = CARTESIAN_POINT ( 'NONE',  ( 0.5987334308729320709, 28.58958371212215610, 39.92741676764588021 ) ) ;
#54086 = ORIENTED_EDGE ( 'NONE', *, *, #37010, .T. ) ;
#54087 = CARTESIAN_POINT ( 'NONE',  ( 3.783198216974394068, -43.00370179234476353, -1.726720072276429541 ) ) ;
#54088 = CARTESIAN_POINT ( 'NONE',  ( 0.6023143664670691511, 44.54505257464859369, -18.16777128831346033 ) ) ;
#54089 = EDGE_LOOP ( 'NONE', ( #43114, #53445 ) ) ;
#54090 = CARTESIAN_POINT ( 'NONE',  ( 0.8751705887134553219, 47.79200036674271956, 5.393078191592866055 ) ) ;
#54091 = ORIENTED_EDGE ( 'NONE', *, *, #333, .T. ) ;
#54092 = CARTESIAN_POINT ( 'NONE',  ( 1.227938101723748288, -36.73927144310496828, -22.18841447410757795 ) ) ;
#54093 = ORIENTED_EDGE ( 'NONE', *, *, #30042, .F. ) ;
#54094 = CARTESIAN_POINT ( 'NONE',  ( -3.514385190458188646, -13.03453477240703862, -1.199999999999999956 ) ) ;
#54095 = CARTESIAN_POINT ( 'NONE',  ( 0.9789233960466692253, 36.12512514380552631, -21.24410648101569166 ) ) ;
#54096 = CARTESIAN_POINT ( 'NONE',  ( 0.9752570700956807448, 33.90066715551972010, 26.30364510018319280 ) ) ;
#54097 = ORIENTED_EDGE ( 'NONE', *, *, #4404, .T. ) ;
#54098 = CARTESIAN_POINT ( 'NONE',  ( 0.1129192098497447394, 41.72114954716796120, -14.36305915353690743 ) ) ;
#54099 = CARTESIAN_POINT ( 'NONE',  ( 2.500000000000000000, 2.357898499370431722, -2.818925648462311528E-15 ) ) ;
#54100 = EDGE_CURVE ( 'NONE', #46412, #37486, #21304, .T. ) ;
#54101 = CARTESIAN_POINT ( 'NONE',  ( 1.500000000000001332, 0.000000000000000000, 0.000000000000000000 ) ) ;
#54102 = ORIENTED_EDGE ( 'NONE', *, *, #18404, .F. ) ;
#54103 = ORIENTED_EDGE ( 'NONE', *, *, #12842, .F. ) ;
#54104 = CARTESIAN_POINT ( 'NONE',  ( 0.9772918015221172539, -31.35844505642634061, -27.80260382399047714 ) ) ;
#54105 = CARTESIAN_POINT ( 'NONE',  ( 0.5549461598389366923, 30.29548519724135858, 32.05310081927385113 ) ) ;
#54106 = CARTESIAN_POINT ( 'NONE',  ( 3.680882792899939915, 40.59250320379013033, -25.57189948075143704 ) ) ;
#54107 = CARTESIAN_POINT ( 'NONE',  ( 0.1081432562775997558, -5.208748643066400064, -42.80885385101080942 ) ) ;
#54108 = CARTESIAN_POINT ( 'NONE',  ( 0.9788927965476035276, -27.16546388611207519, -31.91197556535973234 ) ) ;
#54109 = CARTESIAN_POINT ( 'NONE',  ( -6.017396004339686577, 14.94857180792008577, -11.47192209077572045 ) ) ;
#54110 = ORIENTED_EDGE ( 'NONE', *, *, #13038, .F. ) ;
#54111 = FACE_OUTER_BOUND ( 'NONE', #57174, .T. ) ;
#54112 = VERTEX_POINT ( 'NONE', #29914 ) ;
#54113 = CARTESIAN_POINT ( 'NONE',  ( 7.999999999999986677, 58.44237546506882808, -54.69470952477875869 ) ) ;
#54114 = CARTESIAN_POINT ( 'NONE',  ( 0.6028777368367060907, -19.79822363375413374, -44.93962806097678708 ) ) ;
#54115 = CARTESIAN_POINT ( 'NONE',  ( 0.1140933569871964565, -42.77579569491688005, 10.82502899537159458 ) ) ;
#54116 = CARTESIAN_POINT ( 'NONE',  ( 0.5800708119828320575, -47.40012378203037002, 6.873289505980478609 ) ) ;
#54117 = CARTESIAN_POINT ( 'NONE',  ( 0.7413678028165009426, 10.71994208820953354, 42.77346061982449754 ) ) ;
#54118 = CARTESIAN_POINT ( 'NONE',  ( 0.9762797500689124330, -12.89881610234921006, -39.87411852747946028 ) ) ;
#54119 = CIRCLE ( 'NONE', #5110, 6.887500000000022382 ) ;
#54120 = EDGE_CURVE ( 'NONE', #20443, #40951, #1500, .T. ) ;
#54121 = CARTESIAN_POINT ( 'NONE',  ( 0.1157506346131639274, 20.32681236405533909, -39.16326542717449399 ) ) ;
#54122 = CARTESIAN_POINT ( 'NONE',  ( -6.016489644550736315, -17.40716454747933284, 7.215050741357980080 ) ) ;
#54123 =( BOUNDED_SURFACE ( )  B_SPLINE_SURFACE ( 3, 1, ( 
 ( #2146, #53311 ),
 ( #50399, #29515 ),
 ( #25985, #20139 ),
 ( #41042, #26591 ) ),
 .UNSPECIFIED., .F., .F., .F. ) 
 B_SPLINE_SURFACE_WITH_KNOTS ( ( 4, 4 ),
 ( 2, 2 ),
 ( 0.000000000000000000, 1.000000000000000000 ),
 ( 0.000000000000000000, 1.000000000000000000 ),
 .UNSPECIFIED. ) 
 GEOMETRIC_REPRESENTATION_ITEM ( )  RATIONAL_B_SPLINE_SURFACE ( (
 ( 1.000000000000000000, 1.000000000000000000),
 ( 0.9729067724841187204, 0.9999501103223794596),
 ( 0.9729067724841187204, 0.9999501103223794596),
 ( 1.000000000000000000, 1.000000000000000000) ) ) 
 REPRESENTATION_ITEM ( '' )  SURFACE ( )  );
#54124 = CARTESIAN_POINT ( 'NONE',  ( 5.959828726073459926, -20.52560994243598813, 0.004526594003308782171 ) ) ;
#54125 = CARTESIAN_POINT ( 'NONE',  ( 0.7048096507298635682, 46.24547838151369916, -13.26491767067467542 ) ) ;
#54126 = CARTESIAN_POINT ( 'NONE',  ( 4.975801465491694664, 45.18341283946434572, 15.94009207553066787 ) ) ;
#54127 = CARTESIAN_POINT ( 'NONE',  ( 2.533389852662419894, -19.25250431882765056, -39.58271856741450279 ) ) ;
#54128 = CARTESIAN_POINT ( 'NONE',  ( 0.5998501479064699549, -37.84527566984877467, 29.69975237324549155 ) ) ;
#54129 = CARTESIAN_POINT ( 'NONE',  ( 0.8744876279028263033, -34.64280934553510605, -34.78829991575325664 ) ) ;
#54130 = ADVANCED_FACE ( 'NONE', ( #49953 ), #39551, .T. ) ;
#54131 = B_SPLINE_CURVE_WITH_KNOTS ( 'NONE', 3,
 ( #61328, #33167, #37565, #52242, #51014, #18761, #32550, #56640, #27218, #46345, #3389, #13761, #17829, #36954, #56020, #8403 ),
 .UNSPECIFIED., .F., .F.,
 ( 4, 3, 3, 3, 3, 4 ),
 ( 3.469446951953614189E-18, 0.0002724568934985433497, 0.0004086836638483668654, 0.0005449104342063524177, 0.0008173270854453568070, 0.001089761613562690093 ),
 .UNSPECIFIED. ) ;
#54132 = EDGE_LOOP ( 'NONE', ( #54968, #39891, #17122, #27001 ) ) ;
#54133 = ADVANCED_FACE ( 'NONE', ( #15217 ), #33528, .F. ) ;
#54134 = CARTESIAN_POINT ( 'NONE',  ( 4.553261556744873317, 22.96401893593727550, 37.44587293859699173 ) ) ;
#54135 =( BOUNDED_SURFACE ( )  B_SPLINE_SURFACE ( 3, 1, ( 
 ( #55907, #23335 ),
 ( #13327, #51507 ),
 ( #47451, #4502 ),
 ( #23639, #42766 ) ),
 .UNSPECIFIED., .F., .F., .F. ) 
 B_SPLINE_SURFACE_WITH_KNOTS ( ( 4, 4 ),
 ( 2, 2 ),
 ( 0.000000000000000000, 1.000000000000000000 ),
 ( 0.000000000000000000, 1.000000000000000000 ),
 .UNSPECIFIED. ) 
 GEOMETRIC_REPRESENTATION_ITEM ( )  RATIONAL_B_SPLINE_SURFACE ( (
 ( 1.000000000000000000, 1.000000000000000000),
 ( 0.7269869731126821222, 0.9931720237060910339),
 ( 0.7269869731126821222, 0.9931720237060910339),
 ( 1.000000000000000000, 1.000000000000000000) ) ) 
 REPRESENTATION_ITEM ( '' )  SURFACE ( )  );
#54136 = CARTESIAN_POINT ( 'NONE',  ( 0.5830081025819934260, -19.98762393432967244, -42.42318851574051308 ) ) ;
#54137 = CARTESIAN_POINT ( 'NONE',  ( 0.9754402186311950107, -26.26956909363294201, -33.92707563620669475 ) ) ;
#54138 = CARTESIAN_POINT ( 'NONE',  ( 5.283180000000047727, 1.890854657883512518E-15, -15.43999999999999240 ) ) ;
#54139 = CARTESIAN_POINT ( 'NONE',  ( 0.1101816497532063371, -41.61967362528563541, 11.29256821151141388 ) ) ;
#54140 = ORIENTED_EDGE ( 'NONE', *, *, #19763, .T. ) ;
#54141 =( BOUNDED_SURFACE ( )  B_SPLINE_SURFACE ( 3, 1, ( 
 ( #34270, #52733 ),
 ( #38981, #33354 ),
 ( #5105, #5416 ),
 ( #61811, #9835 ) ),
 .UNSPECIFIED., .F., .F., .F. ) 
 B_SPLINE_SURFACE_WITH_KNOTS ( ( 4, 4 ),
 ( 2, 2 ),
 ( 0.000000000000000000, 1.000000000000000000 ),
 ( 0.000000000000000000, 1.000000000000000000 ),
 .UNSPECIFIED. ) 
 GEOMETRIC_REPRESENTATION_ITEM ( )  RATIONAL_B_SPLINE_SURFACE ( (
 ( 1.000000000000000000, 1.000000000000000000),
 ( 0.9953040768229005630, 0.8617119497784937465),
 ( 0.9953040768229005630, 0.8617119497784937465),
 ( 1.000000000000000000, 1.000000000000000000) ) ) 
 REPRESENTATION_ITEM ( '' )  SURFACE ( )  );
#54142 = CARTESIAN_POINT ( 'NONE',  ( 0.7056555295713258236, 17.55111680842097854, -44.57023068418411071 ) ) ;
#54143 = CARTESIAN_POINT ( 'NONE',  ( 0.9757402383260936896, 16.49876987395781569, -39.60970160107518012 ) ) ;
#54144 = CARTESIAN_POINT ( 'NONE',  ( 0.6026112563231247332, -14.13929437185411331, 47.02787842939825680 ) ) ;
#54145 = ORIENTED_EDGE ( 'NONE', *, *, #46543, .F. ) ;
#54146 = CARTESIAN_POINT ( 'NONE',  ( 4.962356264823596597, 37.75702904547799932, 18.59145920903680249 ) ) ;
#54147 = CARTESIAN_POINT ( 'NONE',  ( 4.956653778116992370, 21.75875759808766929, -42.88673967249108188 ) ) ;
#54148 = EDGE_CURVE ( 'NONE', #9101, #29673, #13887, .T. ) ;
#54149 = ORIENTED_EDGE ( 'NONE', *, *, #29476, .T. ) ;
#54150 = CARTESIAN_POINT ( 'NONE',  ( 4.553261556744873317, 31.39705178283683296, -30.72075365562339755 ) ) ;
#54151 = ORIENTED_EDGE ( 'NONE', *, *, #31072, .T. ) ;
#54152 = DIRECTION ( 'NONE',  ( 0.000000000000000000, 0.000000000000000000, -1.000000000000000000 ) ) ;
#54154 = ORIENTED_EDGE ( 'NONE', *, *, #17624, .T. ) ;
#54153 = EDGE_CURVE ( 'NONE', #55407, #25265, #790, .T. ) ;
#54155 = CARTESIAN_POINT ( 'NONE',  ( 2.618530812446111078, 42.70834099002623674, 19.63986759318516562 ) ) ;
#54156 = CARTESIAN_POINT ( 'NONE',  ( 7.000000000000016875, -56.56854249492410958, 56.56854249492351983 ) ) ;
#54157 = EDGE_LOOP ( 'NONE', ( #23585, #18143 ) ) ;
#54158 = VECTOR ( 'NONE', #41742, 1000.000000000000114 ) ;
#54159 = ORIENTED_EDGE ( 'NONE', *, *, #36955, .T. ) ;
#54160 = LINE ( 'NONE', #44511, #16775 ) ;
#54161 = EDGE_CURVE ( 'NONE', #55501, #16844, #3468, .T. ) ;
#54162 = CARTESIAN_POINT ( 'NONE',  ( 5.959547316686252039, 5.308980600728456345, -19.82715097195157128 ) ) ;
#54163 = AXIS2_PLACEMENT_3D ( 'NONE', #37546, #3067, #56616 ) ;
#54164 = ORIENTED_EDGE ( 'NONE', *, *, #60177, .T. ) ;
#54165 = ORIENTED_EDGE ( 'NONE', *, *, #56606, .T. ) ;
#54166 = CARTESIAN_POINT ( 'NONE',  ( -4.908599999999998964, 0.000000000000000000, 0.000000000000000000 ) ) ;
#54167 = CARTESIAN_POINT ( 'NONE',  ( 0.5549461598389363592, -35.86403770907894284, -25.67077121296841113 ) ) ;
#54168 = CARTESIAN_POINT ( 'NONE',  ( 2.282816707992314065, -39.45519661757836616, -25.49086946881566718 ) ) ;
#54169 = CARTESIAN_POINT ( 'NONE',  ( 0.9754292589017217185, -18.16743306764310617, -37.76601438632337704 ) ) ;
#54170 = ORIENTED_EDGE ( 'NONE', *, *, #56626, .T. ) ;
#54171 = CARTESIAN_POINT ( 'NONE',  ( -6.078457390727109555, -11.02028633642675182, 15.79075046033827867 ) ) ;
#54172 = EDGE_CURVE ( 'NONE', #4129, #41115, #30514, .T. ) ;
#54173 = B_SPLINE_CURVE_WITH_KNOTS ( 'NONE', 3,
 ( #58327, #15149, #58027, #38969 ),
 .UNSPECIFIED., .F., .F.,
 ( 4, 4 ),
 ( 0.000000000000000000, 0.004041751736740998614 ),
 .UNSPECIFIED. ) ;
#54174 = ORIENTED_EDGE ( 'NONE', *, *, #20858, .F. ) ;
#54175 = DIRECTION ( 'NONE',  ( -0.9848077530122077983, -0.1736481776669316079, 1.387778780781445367E-17 ) ) ;
#54176 = B_SPLINE_CURVE_WITH_KNOTS ( 'NONE', 3,
 ( #22005, #32024, #37051, #22618, #2873, #46750 ),
 .UNSPECIFIED., .F., .F.,
 ( 4, 2, 4 ),
 ( 1.578957240921675292E-17, 0.0002448709889506574277, 0.0004897419779012991345 ),
 .UNSPECIFIED. ) ;
#54177 = ORIENTED_EDGE ( 'NONE', *, *, #61480, .F. ) ;
#54178 = CARTESIAN_POINT ( 'NONE',  ( 0.8744876279028306332, 37.95405449045402690, 31.14225101233274273 ) ) ;
#54179 = B_SPLINE_CURVE_WITH_KNOTS ( 'NONE', 3,
 ( #48738, #15854, #5796, #24944, #1110, #20251 ),
 .UNSPECIFIED., .F., .F.,
 ( 4, 2, 4 ),
 ( 8.805430561888389713E-18, 0.0002448709889506567772, 0.0004897419779013047723 ),
 .UNSPECIFIED. ) ;
#54180 = CARTESIAN_POINT ( 'NONE',  ( 0.7056313189692735577, 36.27982945926389391, -29.72410836954218638 ) ) ;
#54181 = ORIENTED_EDGE ( 'NONE', *, *, #32456, .T. ) ;
#54182 = DIRECTION ( 'NONE',  ( 0.1011922191286468153, -0.04473873795207425341, -0.9938604429769180015 ) ) ;
#54183 = CARTESIAN_POINT ( 'NONE',  ( 0.8557997880470697982, 44.60232077416686991, 17.48760788519232889 ) ) ;
#54184 = CARTESIAN_POINT ( 'NONE',  ( 53.13270191851064084, 12.49630009966210054, 0.3485413523074348818 ) ) ;
#54185 = CARTESIAN_POINT ( 'NONE',  ( 0.8744876279028263033, 49.04340454744552602, -2.257104511335871422 ) ) ;
#54186 = ORIENTED_EDGE ( 'NONE', *, *, #639, .T. ) ;
#54187 = FACE_OUTER_BOUND ( 'NONE', #16937, .T. ) ;
#54188 = CARTESIAN_POINT ( 'NONE',  ( 4.975801465491695552, 27.09127437476327671, 39.51822597168504814 ) ) ;
#54189 = DIRECTION ( 'NONE',  ( -1.836909530733573776E-16, 1.000000000000000000, 0.000000000000000000 ) ) ;
#54190 = SHAPE_REPRESENTATION_RELATIONSHIP ( 'NONE' , 'NONE' ,  #8803, #25822 ) ;
#54191 = FACE_OUTER_BOUND ( 'NONE', #17541, .T. ) ;
#54192 = DIRECTION ( 'NONE',  ( -0.1024043820194934507, 0.3927886084231760888, -0.9139094329506565195 ) ) ;
#54193 = CARTESIAN_POINT ( 'NONE',  ( 1.154321713695927842, -42.64911660416107964, 4.782433421669931128 ) ) ;
#54194 = EDGE_CURVE ( 'NONE', #42473, #51079, #23506, .T. ) ;
#54195 = CARTESIAN_POINT ( 'NONE',  ( -17.83628007174841912, -7.719455939378114806, -2.099999999999997424 ) ) ;
#54196 = CARTESIAN_POINT ( 'NONE',  ( 5.910764540655178756, -17.29668172820431238, 10.26284754161173751 ) ) ;
#54197 = ADVANCED_FACE ( 'NONE', ( #26444 ), #29504, .T. ) ;
#54198 = CARTESIAN_POINT ( 'NONE',  ( -6.078075953587585900, -12.94978436788727549, -14.25125464906014372 ) ) ;
#54199 = CARTESIAN_POINT ( 'NONE',  ( 5.895596859100789899, 5.955534046174526530, -19.21092911436986128 ) ) ;
#54200 = AXIS2_PLACEMENT_3D ( 'NONE', #55515, #22329, #31733 ) ;
#54201 = DIRECTION ( 'NONE',  ( 0.07906939808003035641, 0.5431863341251763622, -0.8358807550762931138 ) ) ;
#54202 = ADVANCED_FACE ( 'NONE', ( #3548 ), #1473, .F. ) ;
#54203 = ADVANCED_FACE ( 'NONE', ( #32399 ), #7892, .F. ) ;
#54204 = CARTESIAN_POINT ( 'NONE',  ( 0.5832366564991501301, 34.05963937630803429, 33.67434452455926674 ) ) ;
#54205 = CARTESIAN_POINT ( 'NONE',  ( 0.6008123274975392114, -45.68025125636955863, 18.02412817068846707 ) ) ;
#54206 = ORIENTED_EDGE ( 'NONE', *, *, #387, .T. ) ;
#54207 = CARTESIAN_POINT ( 'NONE',  ( 4.956445790443991584, 30.81386304088947625, 35.60960396630300551 ) ) ;
#54208 = CARTESIAN_POINT ( 'NONE',  ( 5.896782393890504181, -4.668739246792323883, 19.56345983519973686 ) ) ;
#54209 = DIRECTION ( 'NONE',  ( 0.000000000000000000, 0.000000000000000000, 1.000000000000000000 ) ) ;
#54210 = ORIENTED_EDGE ( 'NONE', *, *, #37009, .T. ) ;
#54211 = DIRECTION ( 'NONE',  ( 0.1024043820194936172, -0.5950744814819302064, 0.7971196296869232922 ) ) ;
#54212 = DIRECTION ( 'NONE',  ( 0.07906939808003035641, 0.9951496949144252868, -0.05852448204801217330 ) ) ;
#54213 =( BOUNDED_SURFACE ( )  B_SPLINE_SURFACE ( 3, 1, ( 
 ( #138, #42792 ),
 ( #5145, #9557 ),
 ( #52463, #14285 ),
 ( #28665, #58081 ) ),
 .UNSPECIFIED., .F., .F., .F. ) 
 B_SPLINE_SURFACE_WITH_KNOTS ( ( 4, 4 ),
 ( 2, 2 ),
 ( 0.000000000000000000, 1.000000000000000000 ),
 ( 0.000000000000000000, 1.000000000000000000 ),
 .UNSPECIFIED. ) 
 GEOMETRIC_REPRESENTATION_ITEM ( )  RATIONAL_B_SPLINE_SURFACE ( (
 ( 1.000000000000000000, 1.000000000000000000),
 ( 0.7223157951917480446, 0.9931996967497186413),
 ( 0.7223157951917480446, 0.9931996967497186413),
 ( 1.000000000000000000, 1.000000000000000000) ) ) 
 REPRESENTATION_ITEM ( '' )  SURFACE ( )  );
#54214 = CARTESIAN_POINT ( 'NONE',  ( 0.6023143664670691511, -12.19804739160229623, -46.53533348214987342 ) ) ;
#54215 = EDGE_LOOP ( 'NONE', ( #38063, #20392 ) ) ;
#54216 = CARTESIAN_POINT ( 'NONE',  ( 2.528190830796658961, -5.786163172919478015, -41.57853354664349865 ) ) ;
#54217 = B_SPLINE_CURVE_WITH_KNOTS ( 'NONE', 3,
 ( #18960, #3271, #37772, #51821, #56215, #46532 ),
 .UNSPECIFIED., .F., .F.,
 ( 4, 2, 4 ),
 ( 1.268664800107929448E-16, 0.0002450741128632330469, 0.0004901482257263392421 ),
 .UNSPECIFIED. ) ;
#54218 = CARTESIAN_POINT ( 'NONE',  ( 0.5263152470540364281, 5.252319464604789579E-15, 42.88844316795388778 ) ) ;
#54219 = EDGE_CURVE ( 'NONE', #29673, #59493, #52680, .T. ) ;
#54220 = ORIENTED_EDGE ( 'NONE', *, *, #54219, .F. ) ;
#54221 = CARTESIAN_POINT ( 'NONE',  ( 0.8760168074886960365, -38.69913431881841603, 28.57146030081915100 ) ) ;
#54223 = VERTEX_POINT ( 'NONE', #17673 ) ;
#54222 = EDGE_CURVE ( 'NONE', #47387, #17907, #38520, .T. ) ;
#54224 = ORIENTED_EDGE ( 'NONE', *, *, #22179, .F. ) ;
#54225 = CARTESIAN_POINT ( 'NONE',  ( 0.6253024248130516494, -48.78635602192721166, 5.597829357832809549 ) ) ;
#54226 = EDGE_LOOP ( 'NONE', ( #47063, #8574, #3616, #58257, #633 ) ) ;
#54227 = CARTESIAN_POINT ( 'NONE',  ( -31.74999999999995737, 5.204748896376250699E-16, -4.250000000000000000 ) ) ;
#54228 = CARTESIAN_POINT ( 'NONE',  ( 0.9769922540276041456, -17.23900502197182050, -38.19879920807139939 ) ) ;
#54229 = ORIENTED_EDGE ( 'NONE', *, *, #14011, .T. ) ;
#54230 = CARTESIAN_POINT ( 'NONE',  ( 1.227938101723756947, 42.91134962331487657, -0.8460948827226678626 ) ) ;
#54231 = ADVANCED_FACE ( 'NONE', ( #35869 ), #53078, .F. ) ;
#54232 =( BOUNDED_SURFACE ( )  B_SPLINE_SURFACE ( 3, 1, ( 
 ( #6620, #25143 ),
 ( #34560, #29844 ),
 ( #44289, #25768 ),
 ( #44908, #48960 ) ),
 .UNSPECIFIED., .F., .F., .F. ) 
 B_SPLINE_SURFACE_WITH_KNOTS ( ( 4, 4 ),
 ( 2, 2 ),
 ( 0.000000000000000000, 1.000000000000000000 ),
 ( 0.000000000000000000, 1.000000000000000000 ),
 .UNSPECIFIED. ) 
 GEOMETRIC_REPRESENTATION_ITEM ( )  RATIONAL_B_SPLINE_SURFACE ( (
 ( 1.000000000000000000, 1.000000000000000000),
 ( 0.9953485035131437453, 0.8621029689291523912),
 ( 0.9953485035131437453, 0.8621029689291523912),
 ( 1.000000000000000000, 1.000000000000000000) ) ) 
 REPRESENTATION_ITEM ( '' )  SURFACE ( )  );
#54233 = CARTESIAN_POINT ( 'NONE',  ( -7.632783294297951215E-14, -4.618802153517020948, -0.3572655899081733644 ) ) ;
#54234 = ORIENTED_EDGE ( 'NONE', *, *, #7536, .F. ) ;
#54235 = CARTESIAN_POINT ( 'NONE',  ( 0.6031356219577718170, -18.32926896140859441, 44.47888959008666632 ) ) ;
#54236 = CARTESIAN_POINT ( 'NONE',  ( 1.157644175074338477, -37.03171702379126629, -19.63808060246803322 ) ) ;
#54237 = CARTESIAN_POINT ( 'NONE',  ( 3.238018933889920792, 13.39148516828231372, 0.2749861002446604696 ) ) ;
#54238 = CARTESIAN_POINT ( 'NONE',  ( 0.9790850452238883950, 36.08407221087763617, 21.31377636514384122 ) ) ;
#54239 = EDGE_LOOP ( 'NONE', ( #14094, #50197, #58804, #31380 ) ) ;
#54240 = EDGE_CURVE ( 'NONE', #3716, #51719, #60894, .T. ) ;
#54241 = ORIENTED_EDGE ( 'NONE', *, *, #48316, .F. ) ;
#54242 = STYLED_ITEM ( 'NONE', ( #32989 ), #30720 ) ;
#54243 = CARTESIAN_POINT ( 'NONE',  ( 0.1102847568649952675, 41.67876919128907076, 11.07236323260767641 ) ) ;
#54244 = AXIS2_PLACEMENT_3D ( 'NONE', #4622, #51642, #43205 ) ;
#54245 = EDGE_CURVE ( 'NONE', #1980, #36560, #7067, .T. ) ;
#54246 = CARTESIAN_POINT ( 'NONE',  ( -6.079354080745853928, -6.651439635596617883, 18.07073064439223131 ) ) ;
#54247 = CARTESIAN_POINT ( 'NONE',  ( 4.834790513006553603, -10.96306168285437899, 45.96085964668537116 ) ) ;
#54248 = ORIENTED_EDGE ( 'NONE', *, *, #45490, .F. ) ;
#54249 = CARTESIAN_POINT ( 'NONE',  ( 0.5807400328401637335, 41.20655774452968245, 24.41979442053184712 ) ) ;
#54250 = CYLINDRICAL_SURFACE ( 'NONE', #42318, 15.14599999999999369 ) ;
#54251 = CARTESIAN_POINT ( 'NONE',  ( 3.894904216938897878, 7.599853990351282285, -43.29395514158463243 ) ) ;
#54252 = ORIENTED_EDGE ( 'NONE', *, *, #61784, .F. ) ;
#54253 = ORIENTED_EDGE ( 'NONE', *, *, #20124, .F. ) ;
#54254 = CARTESIAN_POINT ( 'NONE',  ( 0.7764146366350259676, 21.75555901402215753, -41.55401455523356447 ) ) ;
#54255 = CARTESIAN_POINT ( 'NONE',  ( 2.706805983486679779, 42.25893709153612576, 12.28651086408780380 ) ) ;
#54256 = CARTESIAN_POINT ( 'NONE',  ( 4.956445790443988031, 0.000000000000000000, 0.000000000000000000 ) ) ;
#54257 = B_SPLINE_CURVE_WITH_KNOTS ( 'NONE', 3,
 ( #45743, #11933, #51333, #17531 ),
 .UNSPECIFIED., .F., .F.,
 ( 4, 4 ),
 ( 0.000000000000000000, 0.005013413432710140706 ),
 .UNSPECIFIED. ) ;
#54258 = CARTESIAN_POINT ( 'NONE',  ( 0.1129192098497455998, -17.41650932123162931, -40.54154647825617275 ) ) ;
#54259 = CARTESIAN_POINT ( 'NONE',  ( 0.1064266379913941102, -43.12102052820963394, 0.5615183164816264227 ) ) ;
#54260 = CARTESIAN_POINT ( 'NONE',  ( -6.078726893082806448, -17.35055002122446410, -8.351793533709264139 ) ) ;
#54261 = CARTESIAN_POINT ( 'NONE',  ( 3.390910168358337362, -14.38913369447737090, -41.55779070229905159 ) ) ;
#54262 = CARTESIAN_POINT ( 'NONE',  ( 0.5797568599927130917, -24.70127811531111917, -39.86316806453116612 ) ) ;
#54263 = CARTESIAN_POINT ( 'NONE',  ( 0.2885700199627515561, -6.424755504217940505, -42.63514063525625630 ) ) ;
#54264 = CARTESIAN_POINT ( 'NONE',  ( 0.6023142530420679819, -6.019593586345654224, 47.72938419887608319 ) ) ;
#54265 = CARTESIAN_POINT ( 'NONE',  ( 0.1073791018717578927, -40.02496097243069784, 16.05399293000745686 ) ) ;
#54266 = CARTESIAN_POINT ( 'NONE',  ( 5.000000000000012434, -80.00000000000001421, 2.649999999999992806 ) ) ;
#54267 = EDGE_CURVE ( 'NONE', #27055, #40756, #16750, .T. ) ;
#54268 = CARTESIAN_POINT ( 'NONE',  ( 0.5980894510889457338, 44.17723055703951474, -19.05812566676460307 ) ) ;
#54269 = CARTESIAN_POINT ( 'NONE',  ( 2.879087469061463622, 41.18158905594808061, -15.49769013790108652 ) ) ;
#54270 = CARTESIAN_POINT ( 'NONE',  ( 0.6028618097248863439, -34.14037999462347983, -33.89350006451816455 ) ) ;
#54271 = CARTESIAN_POINT ( 'NONE',  ( 4.962356264823601038, -35.98698831890646943, 21.82137185415336589 ) ) ;
#54273 = ADVANCED_FACE ( 'NONE', ( #43045 ), #46705, .F. ) ;
#54272 = CARTESIAN_POINT ( 'NONE',  ( 0.9730545539215883499, -36.90443313492315980, -21.89037132892475057 ) ) ;
#54274 = CARTESIAN_POINT ( 'NONE',  ( 5.860006189529246790, 45.66786516969929721, 15.52021937683292307 ) ) ;
#54275 = EDGE_CURVE ( 'NONE', #32480, #50058, #296, .T. ) ;
#54276 = CARTESIAN_POINT ( 'NONE',  ( 5.894904586330512508, -19.93362243062206218, -2.679572513488613250 ) ) ;
#54277 = CARTESIAN_POINT ( 'NONE',  ( 0.6021447746440204973, 48.98911543949576952, -3.407008591748049930 ) ) ;
#54278 = EDGE_CURVE ( 'NONE', #2911, #52228, #48155, .T. ) ;
#54280 = ORIENTED_EDGE ( 'NONE', *, *, #29200, .T. ) ;
#54279 = CARTESIAN_POINT ( 'NONE',  ( 5.895596859100789899, 17.94951300836806141, 9.074313526372865368 ) ) ;
#54281 = ORIENTED_EDGE ( 'NONE', *, *, #17990, .F. ) ;
#54282 = FACE_BOUND ( 'NONE', #57777, .T. ) ;
#54283 = DIRECTION ( 'NONE',  ( -0.07500201931887529039, -0.7304373162253511298, 0.6788490437229748320 ) ) ;
#54284 = EDGE_CURVE ( 'NONE', #48535, #19440, #1742, .T. ) ;
#54285 = CARTESIAN_POINT ( 'NONE',  ( 30.00000000000001421, -15.99999999999999289, 1.959434878635763159E-15 ) ) ;
#54286 = ORIENTED_EDGE ( 'NONE', *, *, #8490, .T. ) ;
#54287 = EDGE_LOOP ( 'NONE', ( #17608, #8697, #51111, #31051 ) ) ;
#54288 = CARTESIAN_POINT ( 'NONE',  ( 1.227938101723756947, -39.32113113558978057, 17.20315230597830336 ) ) ;
#54289 = CARTESIAN_POINT ( 'NONE',  ( -6.015611763856276717, -13.32857883366842700, 13.31979030221794424 ) ) ;
#54290 = CARTESIAN_POINT ( 'NONE',  ( 0.6031356219577718170, 6.365832241665933644, 47.68448279784256982 ) ) ;
#54291 = B_SPLINE_CURVE_WITH_KNOTS ( 'NONE', 3,
 ( #32666, #37069, #56136, #47079, #4118, #27031 ),
 .UNSPECIFIED., .F., .F.,
 ( 4, 2, 4 ),
 ( 9.745765416140531346E-18, 0.0002291978881530110101, 0.0004583957763060122624 ),
 .UNSPECIFIED. ) ;
#54292 = VECTOR ( 'NONE', #38473, 1000.000000000000000 ) ;
#54293 = EDGE_LOOP ( 'NONE', ( #7381, #32707, #52041, #18204 ) ) ;
#54294 = VERTEX_POINT ( 'NONE', #39894 ) ;
#54295 = EDGE_CURVE ( 'NONE', #715, #37468, #41400, .T. ) ;
#54296 = CARTESIAN_POINT ( 'NONE',  ( 0.6041374136657475802, 46.51335992032618805, -12.28249295041999289 ) ) ;
#54297 = CARTESIAN_POINT ( 'NONE',  ( -4.000000000000000000, -1.549102112939103826, -0.1578953385959410982 ) ) ;
#54298 = CARTESIAN_POINT ( 'NONE',  ( -6.077587904424778920, -18.27312872431383894, 6.073614082124997537 ) ) ;
#54299 = LINE ( 'NONE', #12285, #41959 ) ;
#54300 = ORIENTED_EDGE ( 'NONE', *, *, #61518, .F. ) ;
#54301 = CARTESIAN_POINT ( 'NONE',  ( 0.9788927965476039716, -41.09688267176417042, -8.208705579750407821 ) ) ;
#54302 = CIRCLE ( 'NONE', #40368, 44.12552607296456131 ) ;
#54303 = DIRECTION ( 'NONE',  ( 1.000000000000000000, 0.000000000000000000, 0.000000000000000000 ) ) ;
#54304 = DIRECTION ( 'NONE',  ( 0.07500201931887538753, 0.5478996815936139075, -0.8331750332359386668 ) ) ;
#54305 = ORIENTED_EDGE ( 'NONE', *, *, #55723, .T. ) ;
#54306 = ORIENTED_EDGE ( 'NONE', *, *, #42398, .T. ) ;
#54307 = CARTESIAN_POINT ( 'NONE',  ( 0.7246131072078527691, 44.74808308960848535, -17.64706930304248900 ) ) ;
#54308 = CARTESIAN_POINT ( 'NONE',  ( 3.660087539127321321, 20.10768839917405515, 43.62750476736560046 ) ) ;
#54309 = ORIENTED_EDGE ( 'NONE', *, *, #31052, .T. ) ;
#54310 = CARTESIAN_POINT ( 'NONE',  ( 0.5839254288179565044, 44.28478521851644700, -18.24509008251428455 ) ) ;
#54311 = CARTESIAN_POINT ( 'NONE',  ( 7.000000000000006217, 1.285836671513502038E-15, -1.348150961071066192E-31 ) ) ;
#54312 = CARTESIAN_POINT ( 'NONE',  ( 0.9730545539215883499, 29.98130006528905156, -30.69604515769618658 ) ) ;
#54313 = CARTESIAN_POINT ( 'NONE',  ( 1.231276596079887264, 41.65019306089983786, 4.747440258480190245 ) ) ;
#54314 = EDGE_CURVE ( 'NONE', #54358, #25579, #49570, .T. ) ;
#54315 = ORIENTED_EDGE ( 'NONE', *, *, #54314, .F. ) ;
#54316 = CARTESIAN_POINT ( 'NONE',  ( 0.9747592971366227932, -30.56898208368253123, -30.11108831501868011 ) ) ;
#54317 = CARTESIAN_POINT ( 'NONE',  ( 4.999999999999997335, -2.784000523420839360E-13, 80.00000000000001421 ) ) ;
#54318 = EDGE_CURVE ( 'NONE', #56168, #54683, #43981, .T. ) ;
#54319 = CARTESIAN_POINT ( 'NONE',  ( 4.960156602257180580, 14.43621227656528561, 44.12083041402467387 ) ) ;
#54320 = EDGE_LOOP ( 'NONE', ( #22503, #60853, #44224, #23447 ) ) ;
#54321 = CARTESIAN_POINT ( 'NONE',  ( 0.5786265663353196143, 46.45062944555908757, -11.69877690266605974 ) ) ;
#54322 = CARTESIAN_POINT ( 'NONE',  ( 5.917102823773431552, 10.81462311420893663, -16.95681706421814638 ) ) ;
#54323 = ORIENTED_EDGE ( 'NONE', *, *, #31967, .T. ) ;
#54324 = CARTESIAN_POINT ( 'NONE',  ( 0.8751705887134553219, 42.09020928323342758, 23.27176129838440488 ) ) ;
#54325 = FILL_AREA_STYLE ('',( #60267 ) ) ;
#54326 = ORIENTED_EDGE ( 'NONE', *, *, #22012, .F. ) ;
#54327 = CARTESIAN_POINT ( 'NONE',  ( 5.894904586330512508, 0.6708454810751377506, 20.10172575681410834 ) ) ;
#54328 = CARTESIAN_POINT ( 'NONE',  ( 5.896278296736517710, -15.78116101695085582, 12.46923961480628051 ) ) ;
#54329 = CARTESIAN_POINT ( 'NONE',  ( 0.3622758884714730732, 25.58609868863768355, -34.70015533914803285 ) ) ;
#54330 = AXIS2_PLACEMENT_3D ( 'NONE', #46522, #17389, #55577 ) ;
#54331 = CARTESIAN_POINT ( 'NONE',  ( 0.6017667736363749853, -41.83584368312207857, 23.75082673020790835 ) ) ;
#54332 = CARTESIAN_POINT ( 'NONE',  ( 0.6067099128993230783, 5.548253864791079515, -47.57459301987697131 ) ) ;
#54333 = APPLICATION_CONTEXT ( 'automotive_design' ) ;
#54334 = CARTESIAN_POINT ( 'NONE',  ( 0.5839879327111915375, 46.24044206955238678, -12.48412918464389065 ) ) ;
#54335 =( BOUNDED_SURFACE ( )  B_SPLINE_SURFACE ( 3, 1, ( 
 ( #54208, #36394 ),
 ( #12582, #41103 ),
 ( #31670, #60159 ),
 ( #16975, #3149 ) ),
 .UNSPECIFIED., .F., .F., .F. ) 
 B_SPLINE_SURFACE_WITH_KNOTS ( ( 4, 4 ),
 ( 2, 2 ),
 ( 0.000000000000000000, 1.000000000000000000 ),
 ( 0.000000000000000000, 1.000000000000000000 ),
 .UNSPECIFIED. ) 
 GEOMETRIC_REPRESENTATION_ITEM ( )  RATIONAL_B_SPLINE_SURFACE ( (
 ( 1.000000000000000000, 1.000000000000000000),
 ( 0.9952954269826590483, 0.8620686068821307169),
 ( 0.9952954269826590483, 0.8620686068821307169),
 ( 1.000000000000000000, 1.000000000000000000) ) ) 
 REPRESENTATION_ITEM ( '' )  SURFACE ( )  );
#54336 = CARTESIAN_POINT ( 'NONE',  ( 5.880360259849739535, 9.312491912828125606, -47.05949693022697744 ) ) ;
#54337 = CARTESIAN_POINT ( 'NONE',  ( 0.1098349054025746785, -41.59932877996191536, -11.36734385883990406 ) ) ;
#54338 = CARTESIAN_POINT ( 'NONE',  ( 4.962356264823608143, 0.000000000000000000, 0.000000000000000000 ) ) ;
#54339 = CARTESIAN_POINT ( 'NONE',  ( 1.827119703190778877, -40.22835835992454179, -15.32887915442582205 ) ) ;
#54340 = CARTESIAN_POINT ( 'NONE',  ( 0.9791128995231613841, 15.06706612816901369, 39.10653337404819752 ) ) ;
#54341 = ORIENTED_EDGE ( 'NONE', *, *, #18089, .T. ) ;
#54342 = CARTESIAN_POINT ( 'NONE',  ( 2.301529144917016101, 34.86298839095284308, 33.04216096093416155 ) ) ;
#54343 = DIRECTION ( 'NONE',  ( 0.000000000000000000, 0.000000000000000000, 1.000000000000000000 ) ) ;
#54344 = CARTESIAN_POINT ( 'NONE',  ( 4.834790513006555379, -42.36901421273586266, 20.91544825160024601 ) ) ;
#54345 = CARTESIAN_POINT ( 'NONE',  ( 0.1157506346131639274, 44.02745147267454229, -2.919619260130152050 ) ) ;
#54346 = CIRCLE ( 'NONE', #17400, 0.02570000000000176310 ) ;
#54347 = CARTESIAN_POINT ( 'NONE',  ( 0.5988103564986354543, -28.80261217992950762, 38.53259703935783165 ) ) ;
#54348 = CARTESIAN_POINT ( 'NONE',  ( 3.678748215320119641, -36.44294827805337889, -32.71886818187038415 ) ) ;
#54349 =( LENGTH_UNIT ( ) NAMED_UNIT ( * ) SI_UNIT ( .MILLI., .METRE. ) );
#54351 = ADVANCED_FACE ( 'NONE', ( #34865 ), #48229, .F. ) ;
#54350 = CARTESIAN_POINT ( 'NONE',  ( 0.2230388203127639524, -41.84042374003691833, -10.42432885623869510 ) ) ;
#54352 = CARTESIAN_POINT ( 'NONE',  ( 3.390910168358337362, 35.74601250571907229, -25.61873780018469660 ) ) ;
#54353 = ADVANCED_FACE ( 'NONE', ( #6612 ), #41954, .F. ) ;
#54354 = CARTESIAN_POINT ( 'NONE',  ( 0.6029303876144825880, 0.1308990448395709882, -48.10727438003475953 ) ) ;
#54355 = ADVANCED_FACE ( 'NONE', ( #59257 ), #59503, .T. ) ;
#54357 = ORIENTED_EDGE ( 'NONE', *, *, #36217, .F. ) ;
#54356 = CARTESIAN_POINT ( 'NONE',  ( -2.739355103387248747, -5.801236230415970141, 13.75475282038634361 ) ) ;
#54358 = VERTEX_POINT ( 'NONE', #706 ) ;
#54359 = CARTESIAN_POINT ( 'NONE',  ( 5.901764892641288895, -4.659217859064160194, 48.74713485305014160 ) ) ;
#54360 = CARTESIAN_POINT ( 'NONE',  ( -6.016761891674565099, 0.003433883960047550993, -18.84319130225482297 ) ) ;
#54361 = EDGE_CURVE ( 'NONE', #14724, #54373, #21968, .T. ) ;
#54362 = CARTESIAN_POINT ( 'NONE',  ( 0.1073791018717483448, 16.95003405440257893, 39.65380858626220828 ) ) ;
#54363 = ORIENTED_EDGE ( 'NONE', *, *, #57156, .T. ) ;
#54364 = CARTESIAN_POINT ( 'NONE',  ( 0.1157506346131639274, -22.79424777909198951, 37.78045695843545104 ) ) ;
#54365 = CARTESIAN_POINT ( 'NONE',  ( 5.896782393890504181, 14.91246379622031526, -13.49609241241443947 ) ) ;
#54366 = CARTESIAN_POINT ( 'NONE',  ( 0.1102847568649952675, 41.63105453442837245, -11.25043675627755135 ) ) ;
#54367 = B_SPLINE_CURVE_WITH_KNOTS ( 'NONE', 3,
 ( #46631, #33148, #13419, #61612, #42250, #3982, #61310, #38169, #51296, #57215, #50992, #18734, #8088, #41622, #32527, #51601, #3674, #18425, #37547, #17808, #56924, #22501, #14048, #22809, #37237 ),
 .UNSPECIFIED., .F., .F.,
 ( 4, 3, 3, 3, 3, 3, 3, 3, 4 ),
 ( 6.254634441385500747E-18, 0.0005656085177311399653, 0.001131215744874498755, 0.001696821861372766783, 0.002262427090022496850, 0.002828031679238745925, 0.003393635864401603128, 0.003977030878808131623, 0.004561030005651158133 ),
 .UNSPECIFIED. ) ;
#54368 = ORIENTED_EDGE ( 'NONE', *, *, #31598, .F. ) ;
#54369 = ORIENTED_EDGE ( 'NONE', *, *, #46928, .T. ) ;
#54370 = DIRECTION ( 'NONE',  ( 0.07836865515943411409, 0.9649662368512237354, -0.2503967164834429715 ) ) ;
#54371 = ADVANCED_FACE ( 'NONE', ( #60188 ), #5375, .F. ) ;
#54372 = CARTESIAN_POINT ( 'NONE',  ( 0.1073791018717578927, -39.65380858626204486, -16.95003405440299460 ) ) ;
#54373 = VERTEX_POINT ( 'NONE', #12002 ) ;
#54374 = EDGE_CURVE ( 'NONE', #33554, #46030, #43617, .T. ) ;
#54375 = B_SPLINE_CURVE_WITH_KNOTS ( 'NONE', 3,
 ( #36418, #21999, #41128, #51093, #12611, #3475, #50793, #61107, #31703, #7882, #32321, #46128, #32017, #17299, #3174, #45509, #37336, #22303, #41431, #17604, #8186, #7561, #13217, #51397, #12921 ),
 .UNSPECIFIED., .F., .F.,
 ( 4, 3, 3, 3, 3, 3, 3, 3, 4 ),
 ( 2.602085213965210642E-18, 0.0005656085177311389895, 0.001131215744874498755, 0.001696821861372763965, 0.002262427090022495983, 0.002828031679238745925, 0.003393635864401605296, 0.003977030878808129888, 0.004561030005651158133 ),
 .UNSPECIFIED. ) ;
#54376 = CIRCLE ( 'NONE', #1347, 43.92652462719577500 ) ;
#54377 = EDGE_LOOP ( 'NONE', ( #27224, #56664, #10999, #29888 ) ) ;
#54378 = CARTESIAN_POINT ( 'NONE',  ( 0.5807400328401637335, -0.5448834511093417765, 47.89582301953903709 ) ) ;
#54379 = CARTESIAN_POINT ( 'NONE',  ( 5.981074661064941900, -20.52466374824937034, -0.008585178657544500352 ) ) ;
#54380 = VERTEX_POINT ( 'NONE', #7560 ) ;
#54381 = CARTESIAN_POINT ( 'NONE',  ( -2.000000000000022649, -3.464101615137742396, -5.600000000000000533 ) ) ;
#54382 = CARTESIAN_POINT ( 'NONE',  ( 0.9756354156337465611, 41.47994205070128260, -10.97961179198156678 ) ) ;
#54383 = ORIENTED_EDGE ( 'NONE', *, *, #31930, .T. ) ;
#54384 = DIRECTION ( 'NONE',  ( 0.000000000000000000, 0.7071067811865540120, -0.7071067811865409114 ) ) ;
#54385 = FACE_OUTER_BOUND ( 'NONE', #14600, .T. ) ;
#54386 = ORIENTED_EDGE ( 'NONE', *, *, #24470, .F. ) ;
#54387 = CARTESIAN_POINT ( 'NONE',  ( 7.999999999999996447, 1.469527624586858429E-15, -1.540743955509788245E-31 ) ) ;
#54388 = CARTESIAN_POINT ( 'NONE',  ( 2.624215991343620935, -28.09277600149244947, 38.92973006074502962 ) ) ;
#54389 = CARTESIAN_POINT ( 'NONE',  ( 1.227938101723756947, 30.94118573761312874, 29.74462687941236538 ) ) ;
#54390 = CARTESIAN_POINT ( 'NONE',  ( 4.335381028904201628, -41.60039470203945200, -25.86820458205155759 ) ) ;
#54391 = B_SPLINE_CURVE_WITH_KNOTS ( 'NONE', 3,
 ( #30517, #39976, #35568, #54313 ),
 .UNSPECIFIED., .F., .F.,
 ( 4, 4 ),
 ( 0.000000000000000000, 0.004042984057420973693 ),
 .UNSPECIFIED. ) ;
#54392 = STYLED_ITEM ( 'NONE', ( #12385 ), #52245 ) ;
#54393 = ORIENTED_EDGE ( 'NONE', *, *, #30683, .T. ) ;
#54394 = CARTESIAN_POINT ( 'NONE',  ( 0.6001305935487422083, 44.24520387813827682, -18.89378601236018795 ) ) ;
#54395 = CARTESIAN_POINT ( 'NONE',  ( 2.500000000000000000, 2.357898499370431722, -2.818925648462311528E-15 ) ) ;
#54397 = ORIENTED_EDGE ( 'NONE', *, *, #45845, .F. ) ;
#54396 =( BOUNDED_SURFACE ( )  B_SPLINE_SURFACE ( 3, 1, ( 
 ( #59877, #45816 ),
 ( #60482, #50785 ),
 ( #46424, #2859 ),
 ( #7876, #13211 ) ),
 .UNSPECIFIED., .F., .F., .F. ) 
 B_SPLINE_SURFACE_WITH_KNOTS ( ( 4, 4 ),
 ( 2, 2 ),
 ( 0.000000000000000000, 1.000000000000000000 ),
 ( 0.000000000000000000, 1.000000000000000000 ),
 .UNSPECIFIED. ) 
 GEOMETRIC_REPRESENTATION_ITEM ( )  RATIONAL_B_SPLINE_SURFACE ( (
 ( 1.000000000000000000, 1.000000000000000000),
 ( 0.7282232189291693025, 0.9929344683865674037),
 ( 0.7282232189291693025, 0.9929344683865674037),
 ( 1.000000000000000000, 1.000000000000000000) ) ) 
 REPRESENTATION_ITEM ( '' )  SURFACE ( )  );
#54398 = LINE ( 'NONE', #26216, #21191 ) ;
#54399 = EDGE_CURVE ( 'NONE', #52564, #37381, #9986, .T. ) ;
#54400 = EDGE_LOOP ( 'NONE', ( #10486, #51005, #39878, #38014 ) ) ;
#54401 = CARTESIAN_POINT ( 'NONE',  ( 0.9762797500689124330, 3.691134646837550104, 41.74566217230983511 ) ) ;
#54402 = ORIENTED_EDGE ( 'NONE', *, *, #18596, .T. ) ;
#54403 = CARTESIAN_POINT ( 'NONE',  ( 5.860006189529234355, -40.11385274514663735, -26.78264244998140597 ) ) ;
#54404 = CARTESIAN_POINT ( 'NONE',  ( 5.910764540655178756, 19.71228184310533038, 3.990887496177151217 ) ) ;
#54405 = EDGE_LOOP ( 'NONE', ( #11534, #180, #39586, #41712 ) ) ;
#54406 = CARTESIAN_POINT ( 'NONE',  ( 0.1154773475650539977, 43.34451959701775792, 8.258102139708901390 ) ) ;
#54407 = CARTESIAN_POINT ( 'NONE',  ( 0.1129192098497447394, -38.20615368646970467, 22.07354996983974260 ) ) ;
#54408 = CARTESIAN_POINT ( 'NONE',  ( 9.999999999999991118, 80.00000000000001421, -1.319262011905257654E-31 ) ) ;
#54409 = ORIENTED_EDGE ( 'NONE', *, *, #40870, .T. ) ;
#54410 = ORIENTED_EDGE ( 'NONE', *, *, #55143, .F. ) ;
#54411 =( BOUNDED_SURFACE ( )  B_SPLINE_SURFACE ( 3, 1, ( 
 ( #26625, #22858 ),
 ( #41991, #3723 ),
 ( #3120, #61057 ),
 ( #2502, #51346 ) ),
 .UNSPECIFIED., .F., .F., .F. ) 
 B_SPLINE_SURFACE_WITH_KNOTS ( ( 4, 4 ),
 ( 2, 2 ),
 ( 0.000000000000000000, 1.000000000000000000 ),
 ( 0.000000000000000000, 1.000000000000000000 ),
 .UNSPECIFIED. ) 
 GEOMETRIC_REPRESENTATION_ITEM ( )  RATIONAL_B_SPLINE_SURFACE ( (
 ( 1.000000000000000000, 1.000000000000000000),
 ( 0.9751682680413298332, 0.9999560080971552356),
 ( 0.9751682680413298332, 0.9999560080971552356),
 ( 1.000000000000000000, 1.000000000000000000) ) ) 
 REPRESENTATION_ITEM ( '' )  SURFACE ( )  );
#54412 = CARTESIAN_POINT ( 'NONE',  ( 0.5837374860065628335, 18.49670552082956121, 44.18034382476631805 ) ) ;
#54413 = CARTESIAN_POINT ( 'NONE',  ( 0.8744876279028263033, 46.30617036199606673, 16.31222353896886545 ) ) ;
#54414 = CARTESIAN_POINT ( 'NONE',  ( 4.694002226626920127, -34.93533603653836650, -29.28834354244495941 ) ) ;
#54415 = CARTESIAN_POINT ( 'NONE',  ( 0.1103310638050662151, -5.547176740493243052, -42.76619676553134042 ) ) ;
#54416 = CARTESIAN_POINT ( 'NONE',  ( 0.5997462898726536595, -47.63132954987539591, 11.95023328037892441 ) ) ;
#54417 = B_SPLINE_CURVE_WITH_KNOTS ( 'NONE', 3,
 ( #8375, #46943, #51292, #56303, #60372, #12811, #46627, #32522, #36931, #57752, #29262, #3670, #31904, #14886, #55677, #27194 ),
 .UNSPECIFIED., .F., .F.,
 ( 4, 3, 3, 3, 3, 4 ),
 ( 2.081781105835003463E-17, 0.0002612764279487749517, 0.0003919131003184794077, 0.0005225497727000653642, 0.0007837925190632465469, 0.001045051706266716084 ),
 .UNSPECIFIED. ) ;
#54418 = CARTESIAN_POINT ( 'NONE',  ( 0.6001305935487422083, -37.84751346122875759, 29.70149728382373056 ) ) ;
#54419 = ORIENTED_EDGE ( 'NONE', *, *, #50907, .T. ) ;
#54420 = DIRECTION ( 'NONE',  ( 0.9848077530122080203, 0.1736481776669315247, -2.220446049250313081E-16 ) ) ;
#54421 = CARTESIAN_POINT ( 'NONE',  ( 4.956653778116970166, -27.17045123668450657, -39.67974989265067620 ) ) ;
#54422 = ORIENTED_EDGE ( 'NONE', *, *, #46559, .F. ) ;
#54423 = LINE ( 'NONE', #11875, #23376 ) ;
#54424 = CARTESIAN_POINT ( 'NONE',  ( 0.6016117650947689910, -20.19595095677608398, -44.76242418810664248 ) ) ;
#54425 = CARTESIAN_POINT ( 'NONE',  ( 0.5830082357119567016, 45.15677922592038129, 12.65295715948731825 ) ) ;
#54426 = AXIS2_PLACEMENT_3D ( 'NONE', #50223, #25183, #44622 ) ;
#54427 = CARTESIAN_POINT ( 'NONE',  ( 0.5807400328401574052, 44.04145271122592220, -18.83234461715134955 ) ) ;
#54428 = CARTESIAN_POINT ( 'NONE',  ( -6.077587904424778920, 9.987489566522819828, -16.46347695818013435 ) ) ;
#54429 = CARTESIAN_POINT ( 'NONE',  ( 4.956653778116991482, 9.917440902361805755, -47.05699031914939212 ) ) ;
#54430 = DIRECTION ( 'NONE',  ( 1.000000000000000000, 0.000000000000000000, 0.000000000000000000 ) ) ;
#54431 = CARTESIAN_POINT ( 'NONE',  ( 0.6001305935487315502, -46.33281397023073112, 12.95698906763729852 ) ) ;
#54432 = AXIS2_PLACEMENT_3D ( 'NONE', #8262, #4173, #27383 ) ;
#54433 = ADVANCED_FACE ( 'NONE', ( #41430 ), #11957, .F. ) ;
#54434 = FACE_OUTER_BOUND ( 'NONE', #9599, .T. ) ;
#54435 = CARTESIAN_POINT ( 'NONE',  ( 2.500000000000000000, -2.357898499370432166, 3.035766082959412415E-15 ) ) ;
#54436 = CARTESIAN_POINT ( 'NONE',  ( 4.962356264823599261, -28.94323483023637777, 30.55363735178087126 ) ) ;
#54437 = EDGE_CURVE ( 'NONE', #995, #15923, #6937, .T. ) ;
#54438 = CARTESIAN_POINT ( 'NONE',  ( 1.296416391601052043, -21.88885550073866781, 38.25160622698007273 ) ) ;
#54439 = VECTOR ( 'NONE', #20980, 999.9999999999998863 ) ;
#54440 = CARTESIAN_POINT ( 'NONE',  ( 0.5988103622719985752, 11.86435782853368970, 46.62176011478425863 ) ) ;
#54441 = CARTESIAN_POINT ( 'NONE',  ( 4.975610109902397937, -10.32228546579698403, -47.81108480154335183 ) ) ;
#54442 = VERTEX_POINT ( 'NONE', #59884 ) ;
#54443 = CARTESIAN_POINT ( 'NONE',  ( 4.956445790443988031, 0.000000000000000000, 0.000000000000000000 ) ) ;
#54444 = EDGE_CURVE ( 'NONE', #33056, #13688, #55483, .T. ) ;
#54445 = CARTESIAN_POINT ( 'NONE',  ( 0.5837799406558239479, -19.82278343636528817, -42.50059771829290867 ) ) ;
#54446 = CARTESIAN_POINT ( 'NONE',  ( 0.1147471544378676767, -38.59772625589639006, -21.38148068652244760 ) ) ;
#54447 = CARTESIAN_POINT ( 'NONE',  ( 0.5997462898726536595, -45.31995669577334240, -18.91172004968183984 ) ) ;
#54448 = CARTESIAN_POINT ( 'NONE',  ( 0.1102144999581333301, -41.68747259405357397, 11.03964818279701632 ) ) ;
#54449 = ORIENTED_EDGE ( 'NONE', *, *, #28873, .F. ) ;
#54450 = ADVANCED_FACE ( 'NONE', ( #2864 ), #59476, .F. ) ;
#54451 = DIRECTION ( 'NONE',  ( 0.07439287786467665975, 0.6957517427943022970, 0.7144194931003088334 ) ) ;
#54452 = CARTESIAN_POINT ( 'NONE',  ( 0.5997462898726536595, 27.66511329191646951, -40.57330571557777432 ) ) ;
#54453 = B_SPLINE_CURVE_WITH_KNOTS ( 'NONE', 3,
 ( #10625, #48830, #2118, #31267, #17479, #21254 ),
 .UNSPECIFIED., .F., .F.,
 ( 4, 2, 4 ),
 ( 1.764953265579307567E-18, 0.0002450742804987340677, 0.0004901485609974662924 ),
 .UNSPECIFIED. ) ;
#54454 = CARTESIAN_POINT ( 'NONE',  ( 0.3676999524040323597, 43.96170928169360081, 3.649479463525401535 ) ) ;
#54455 = ORIENTED_EDGE ( 'NONE', *, *, #38177, .F. ) ;
#54456 = CIRCLE ( 'NONE', #39484, 47.09074272231896430 ) ;
#54457 = CARTESIAN_POINT ( 'NONE',  ( 4.549368137175248350, 42.84816078363926550, 2.596185425822091553 ) ) ;
#54458 = ORIENTED_EDGE ( 'NONE', *, *, #34382, .F. ) ;
#54459 = CARTESIAN_POINT ( 'NONE',  ( -6.218809015666120210, -1.096543817334992621, 4.142297321093258830E-16 ) ) ;
#54460 = VERTEX_POINT ( 'NONE', #41737 ) ;
#54461 = CARTESIAN_POINT ( 'NONE',  ( 0.9730545539215883499, -39.83279466599027785, -15.95224156741871546 ) ) ;
#54462 = ORIENTED_EDGE ( 'NONE', *, *, #5425, .F. ) ;
#54463 = CARTESIAN_POINT ( 'NONE',  ( 5.860006189529234355, -36.25227510158484989, 31.81514841426745477 ) ) ;
#54464 = ORIENTED_EDGE ( 'NONE', *, *, #19048, .T. ) ;
#54465 = ORIENTED_EDGE ( 'NONE', *, *, #33601, .F. ) ;
#54466 = DIRECTION ( 'NONE',  ( 0.000000000000000000, 0.000000000000000000, 1.000000000000000000 ) ) ;
#54467 = CARTESIAN_POINT ( 'NONE',  ( 0.1157991065609915715, -1.495616162223984746, 44.09881515225770698 ) ) ;
#54468 = EDGE_CURVE ( 'NONE', #13139, #40550, #30154, .T. ) ;
#54469 = AXIS2_PLACEMENT_3D ( 'NONE', #43989, #39274, #15765 ) ;
#54470 = ORIENTED_EDGE ( 'NONE', *, *, #59184, .F. ) ;
#54471 = EDGE_LOOP ( 'NONE', ( #37940, #21214, #56503, #33918 ) ) ;
#54472 = CARTESIAN_POINT ( 'NONE',  ( 4.962356264823608143, 0.000000000000000000, 0.000000000000000000 ) ) ;
#54473 = LINE ( 'NONE', #1866, #56377 ) ;
#54474 = CARTESIAN_POINT ( 'NONE',  ( 0.5834872094924159480, 34.02770606800808650, -33.70665904794255141 ) ) ;
#54475 = AXIS2_PLACEMENT_3D ( 'NONE', #32065, #17341, #21109 ) ;
#54476 = CARTESIAN_POINT ( 'NONE',  ( -2.739355103387247858, 10.22927580983326656, -10.87241846864702843 ) ) ;
#54477 = ORIENTED_EDGE ( 'NONE', *, *, #28036, .F. ) ;
#54478 = CARTESIAN_POINT ( 'NONE',  ( -6.078075953587585900, -11.02105682227026762, 15.79023371478161053 ) ) ;
#54479 = CARTESIAN_POINT ( 'NONE',  ( -6.057079549204054558, 19.09779050476948115, 2.470957088999126139 ) ) ;
#54480 = AXIS2_PLACEMENT_3D ( 'NONE', #6151, #21518, #16514 ) ;
#54481 = EDGE_LOOP ( 'NONE', ( #1047, #56007, #47342 ) ) ;
#54482 = CARTESIAN_POINT ( 'NONE',  ( 0.5806925824938499181, -46.75147433417400578, -3.677228565731735621 ) ) ;
#54483 = B_SPLINE_CURVE_WITH_KNOTS ( 'NONE', 3,
 ( #19304, #4546, #57471, #23076, #14613, #13373, #32474, #51552, #61260, #18380 ),
 .UNSPECIFIED., .F., .F.,
 ( 4, 3, 3, 4 ),
 ( 4.878909776184769953E-18, 0.0002724573126191764060, 0.0004086839781548493446, 0.0005054209210073039738 ),
 .UNSPECIFIED. ) ;
#54484 = VERTEX_POINT ( 'NONE', #35487 ) ;
#54485 = CARTESIAN_POINT ( 'NONE',  ( 3.661921753702006566, -46.77018590444192370, 5.018050846492144501 ) ) ;
#54486 = CARTESIAN_POINT ( 'NONE',  ( 1.231276596079881047, 28.52807286890743654, 30.71523773966879745 ) ) ;
#54487 = CARTESIAN_POINT ( 'NONE',  ( 0.6064515330803568194, 36.36011321167069354, -29.61885384804041976 ) ) ;
#54488 = ORIENTED_EDGE ( 'NONE', *, *, #43194, .F. ) ;
#54489 = CARTESIAN_POINT ( 'NONE',  ( 3.270143674763207553, 9.482922169187961714, 9.870732238228558941 ) ) ;
#54490 = CARTESIAN_POINT ( 'NONE',  ( 4.553261556744873317, -33.30082861731504096, 28.64601855797499042 ) ) ;
#54491 = CARTESIAN_POINT ( 'NONE',  ( 50.84915202508826582, 12.21967388707288471, 2.632638007633139487 ) ) ;
#54492 = CARTESIAN_POINT ( 'NONE',  ( -20.05982656558827060, -12.49764874730863085, -0.2771623350404011643 ) ) ;
#54493 =( BOUNDED_SURFACE ( )  B_SPLINE_SURFACE ( 3, 1, ( 
 ( #6660, #16110 ),
 ( #30802, #54594 ),
 ( #11724, #49923 ),
 ( #21416, #50230 ) ),
 .UNSPECIFIED., .F., .F., .F. ) 
 B_SPLINE_SURFACE_WITH_KNOTS ( ( 4, 4 ),
 ( 2, 2 ),
 ( 0.000000000000000000, 1.000000000000000000 ),
 ( 0.000000000000000000, 1.000000000000000000 ),
 .UNSPECIFIED. ) 
 GEOMETRIC_REPRESENTATION_ITEM ( )  RATIONAL_B_SPLINE_SURFACE ( (
 ( 1.000000000000000000, 1.000000000000000000),
 ( 0.9953040768229005630, 0.8617119497784937465),
 ( 0.9953040768229005630, 0.8617119497784937465),
 ( 1.000000000000000000, 1.000000000000000000) ) ) 
 REPRESENTATION_ITEM ( '' )  SURFACE ( )  );
#54494 = VERTEX_POINT ( 'NONE', #18226 ) ;
#54495 = CARTESIAN_POINT ( 'NONE',  ( 3.783278058412226752, -41.09146792477075394, 12.79810311738840056 ) ) ;
#54496 = ORIENTED_EDGE ( 'NONE', *, *, #29769, .T. ) ;
#54497 = CARTESIAN_POINT ( 'NONE',  ( 4.967162193818130511, 8.839793687085803597, -42.16965968614184135 ) ) ;
#54498 = DIRECTION ( 'NONE',  ( -0.9848077530122080203, -0.1736481776669315524, 2.220446049250313574E-16 ) ) ;
#54499 = CARTESIAN_POINT ( 'NONE',  ( 0.8560838555295158248, 17.70877843982841782, -43.43698884880027578 ) ) ;
#54500 = VECTOR ( 'NONE', #17417, 1000.000000000000227 ) ;
#54501 = CARTESIAN_POINT ( 'NONE',  ( 4.962356264823608143, -10.17958088187436871, 40.83640203215416165 ) ) ;
#54502 = ADVANCED_FACE ( 'NONE', ( #23224 ), #42319, .F. ) ;
#54503 = CARTESIAN_POINT ( 'NONE',  ( 0.9730545539215883499, -42.60426903087357431, 5.099196237954729760 ) ) ;
#54504 =( BOUNDED_SURFACE ( )  B_SPLINE_SURFACE ( 3, 1, ( 
 ( #50029, #45652 ),
 ( #8034, #50627 ),
 ( #36257, #30597 ),
 ( #35644, #2707 ) ),
 .UNSPECIFIED., .F., .F., .F. ) 
 B_SPLINE_SURFACE_WITH_KNOTS ( ( 4, 4 ),
 ( 2, 2 ),
 ( 0.000000000000000000, 1.000000000000000000 ),
 ( 0.000000000000000000, 1.000000000000000000 ),
 .UNSPECIFIED. ) 
 GEOMETRIC_REPRESENTATION_ITEM ( )  RATIONAL_B_SPLINE_SURFACE ( (
 ( 1.000000000000000000, 1.000000000000000000),
 ( 0.7269869731126817891, 0.9931720237060910339),
 ( 0.7269869731126817891, 0.9931720237060910339),
 ( 1.000000000000000000, 1.000000000000000000) ) ) 
 REPRESENTATION_ITEM ( '' )  SURFACE ( )  );
#54505 = CARTESIAN_POINT ( 'NONE',  ( 0.5850706913938533704, 12.57184842332082297, -46.21698775168632523 ) ) ;
#54506 = ADVANCED_FACE ( 'NONE', ( #37335 ), #3852, .F. ) ;
#54507 =( BOUNDED_SURFACE ( )  B_SPLINE_SURFACE ( 3, 1, ( 
 ( #43683, #5412 ),
 ( #35195, #58036 ),
 ( #10452, #20168 ),
 ( #38977, #44602 ) ),
 .UNSPECIFIED., .F., .F., .F. ) 
 B_SPLINE_SURFACE_WITH_KNOTS ( ( 4, 4 ),
 ( 2, 2 ),
 ( 0.000000000000000000, 1.000000000000000000 ),
 ( 0.000000000000000000, 1.000000000000000000 ),
 .UNSPECIFIED. ) 
 GEOMETRIC_REPRESENTATION_ITEM ( )  RATIONAL_B_SPLINE_SURFACE ( (
 ( 1.000000000000000000, 1.000000000000000000),
 ( 0.7269869731126817891, 0.9931720237060910339),
 ( 0.7269869731126817891, 0.9931720237060910339),
 ( 1.000000000000000000, 1.000000000000000000) ) ) 
 REPRESENTATION_ITEM ( '' )  SURFACE ( )  );
#54508 = CARTESIAN_POINT ( 'NONE',  ( 0.7048096507298635682, -23.32077812596911315, 42.08020459959941206 ) ) ;
#54509 = CARTESIAN_POINT ( 'NONE',  ( 5.960721111146673579, -17.77250458025985225, -10.26825948882919626 ) ) ;
#54510 = CARTESIAN_POINT ( 'NONE',  ( 0.1064266418746774995, -0.5615180042403685734, 43.12102053154801951 ) ) ;
#54511 = ADVANCED_FACE ( 'NONE', ( #4084 ), #39953, .F. ) ;
#54512 = PRESENTATION_LAYER_ASSIGNMENT (  '', '', ( #15564 ) ) ;
#54513 = FACE_OUTER_BOUND ( 'NONE', #47597, .T. ) ;
#54514 = CARTESIAN_POINT ( 'NONE',  ( 0.1145239942831223490, 36.80079408639558380, 24.34434298385119888 ) ) ;
#54515 = ORIENTED_EDGE ( 'NONE', *, *, #46271, .T. ) ;
#54516 = CARTESIAN_POINT ( 'NONE',  ( 1.296416391601052487, -2.522796799315330851, -43.99935079504609092 ) ) ;
#54517 = VECTOR ( 'NONE', #17508, 1000.000000000000114 ) ;
#54518 = CARTESIAN_POINT ( 'NONE',  ( 4.967162193818129623, -38.44485641567058565, -19.45289607368863116 ) ) ;
#54519 = CARTESIAN_POINT ( 'NONE',  ( 3.390910168358336474, -41.99763341749859791, 13.04974803829719221 ) ) ;
#54520 = ORIENTED_EDGE ( 'NONE', *, *, #32032, .T. ) ;
#54521 = ADVANCED_FACE ( 'NONE', ( #51715 ), #23097, .F. ) ;
#54522 = CARTESIAN_POINT ( 'NONE',  ( 0.7044674535453004927, 48.35836311421820710, 8.559873814743298226 ) ) ;
#54523 = AXIS2_PLACEMENT_3D ( 'NONE', #8747, #22856, #32264 ) ;
#54524 = CARTESIAN_POINT ( 'NONE',  ( 3.238018933889920792, -13.37994740236394087, 0.6200805412423465723 ) ) ;
#54525 = CARTESIAN_POINT ( 'NONE',  ( 58.00000000000000000, 1.530808498934191127E-15, -12.50000000000000000 ) ) ;
#54526 = ORIENTED_EDGE ( 'NONE', *, *, #35583, .T. ) ;
#54527 = DIRECTION ( 'NONE',  ( 0.000000000000000000, -1.224646799147332007E-16, 1.000000000000000000 ) ) ;
#54528 = CARTESIAN_POINT ( 'NONE',  ( 0.5980894510889457338, 34.51330645350356008, 33.52121017007839043 ) ) ;
#54529 = VERTEX_POINT ( 'NONE', #13216 ) ;
#54530 = B_SPLINE_CURVE_WITH_KNOTS ( 'NONE', 3,
 ( #34989, #14958, #34066, #10239 ),
 .UNSPECIFIED., .F., .F.,
 ( 4, 4 ),
 ( 0.000000000000000000, 0.004442905043737215703 ),
 .UNSPECIFIED. ) ;
#54531 = CARTESIAN_POINT ( 'NONE',  ( -6.078457390727109555, -4.280596808180907153, -18.77421108870621325 ) ) ;
#54532 = VERTEX_POINT ( 'NONE', #5552 ) ;
#54533 = ORIENTED_EDGE ( 'NONE', *, *, #44101, .T. ) ;
#54534 = CARTESIAN_POINT ( 'NONE',  ( 0.1145239942831223490, 44.01141660824960411, 3.152885795547452741 ) ) ;
#54535 = ORIENTED_EDGE ( 'NONE', *, *, #49277, .T. ) ;
#54536 = CARTESIAN_POINT ( 'NONE',  ( 5.959828726073459926, -2.683617577144242095, -20.34941966491238219 ) ) ;
#54537 = CARTESIAN_POINT ( 'NONE',  ( 0.6001305935487422083, -41.40054608060277275, -24.50730504006441635 ) ) ;
#54538 = ORIENTED_EDGE ( 'NONE', *, *, #55538, .F. ) ;
#54539 = LINE ( 'NONE', #40199, #14721 ) ;
#54540 = CARTESIAN_POINT ( 'NONE',  ( 5.896782393890504181, -19.93422257774826889, 2.674482585249640110 ) ) ;
#54541 = ORIENTED_EDGE ( 'NONE', *, *, #31649, .T. ) ;
#54542 = CARTESIAN_POINT ( 'NONE',  ( 0.1152339509894530906, 43.26722510425824453, -8.653896361332732212 ) ) ;
#54543 = CARTESIAN_POINT ( 'NONE',  ( 0.5807400328401637335, 46.12278621143497048, 12.92266817606032170 ) ) ;
#54544 = CARTESIAN_POINT ( 'NONE',  ( 0.7057020205115047684, 24.67553336431243949, -41.05685587925813707 ) ) ;
#54545 = DIRECTION ( 'NONE',  ( 1.000000000000000000, 1.836909530733573776E-16, 0.000000000000000000 ) ) ;
#54546 = VERTEX_POINT ( 'NONE', #37972 ) ;
#54547 = EDGE_CURVE ( 'NONE', #17218, #50038, #52019, .T. ) ;
#54548 = B_SPLINE_CURVE_WITH_KNOTS ( 'NONE', 3,
 ( #57868, #19688, #29379, #29078 ),
 .UNSPECIFIED., .F., .F.,
 ( 4, 4 ),
 ( 6.254634441385501517E-18, 0.004566006591234647236 ),
 .UNSPECIFIED. ) ;
#54549 = ORIENTED_EDGE ( 'NONE', *, *, #49779, .T. ) ;
#54550 = CARTESIAN_POINT ( 'NONE',  ( 5.959547316686252039, 10.26589671991363417, -17.77392908783923531 ) ) ;
#54551 = ADVANCED_FACE ( 'NONE', ( #8485 ), #20712, .F. ) ;
#54552 = CARTESIAN_POINT ( 'NONE',  ( -6.078726893082806448, -6.647148524917739998, 18.07233957617010134 ) ) ;
#54553 = CARTESIAN_POINT ( 'NONE',  ( 3.221118495291109163, 13.40464864085779517, -41.89363692109937887 ) ) ;
#54554 = AXIS2_PLACEMENT_3D ( 'NONE', #48032, #4460, #56791 ) ;
#54555 = ORIENTED_EDGE ( 'NONE', *, *, #45813, .F. ) ;
#54556 = CARTESIAN_POINT ( 'NONE',  ( 0.6846871229502899947, -34.48177377577813019, -33.25969555998779015 ) ) ;
#54557 = CARTESIAN_POINT ( 'NONE',  ( 4.956445790443989807, 46.03642002599014660, 9.908889005849758291 ) ) ;
#54558 = ADVANCED_FACE ( 'NONE', ( #874 ), #55088, .F. ) ;
#54559 = CARTESIAN_POINT ( 'NONE',  ( 5.896278296736517710, -20.11285533178147844, -0.005478796673508855644 ) ) ;
#54560 =( NAMED_UNIT ( * ) PLANE_ANGLE_UNIT ( ) SI_UNIT ( $, .RADIAN. ) );
#54562 = VERTEX_POINT ( 'NONE', #20912 ) ;
#54561 = CONICAL_SURFACE ( 'NONE', #557, 43.08621763946400307, 1.568696531533066763 ) ;
#54563 = ORIENTED_EDGE ( 'NONE', *, *, #59228, .F. ) ;
#54564 = CARTESIAN_POINT ( 'NONE',  ( 0.9789889208857681657, -39.62124817252024656, -13.65619241567479492 ) ) ;
#54565 = CARTESIAN_POINT ( 'NONE',  ( 0.6254087463353922294, 28.73645667569951101, -38.58044986685661826 ) ) ;
#54566 = CARTESIAN_POINT ( 'NONE',  ( 0.1098349054025746646, -39.92296693299719124, 16.30574661324300223 ) ) ;
#54567 = AXIS2_PLACEMENT_3D ( 'NONE', #11080, #49272, #39289 ) ;
#54568 = CARTESIAN_POINT ( 'NONE',  ( 0.6039202388192952409, 32.88598194813054931, 36.47020570487947566 ) ) ;
#54569 = DIRECTION ( 'NONE',  ( -1.000000000000000000, 0.000000000000000000, 0.000000000000000000 ) ) ;
#54570 = CARTESIAN_POINT ( 'NONE',  ( 2.009741617377216460, -41.31583237047342294, -15.24814982737201774 ) ) ;
#54571 = CARTESIAN_POINT ( 'NONE',  ( 0.9730545539215883499, 6.101350888304637010, 42.47233286818619291 ) ) ;
#54572 = CARTESIAN_POINT ( 'NONE',  ( 0.8560838555295158248, -24.46533024579895610, -40.02274915652004239 ) ) ;
#54573 = ADVANCED_FACE ( 'NONE', ( #1786 ), #27112, .F. ) ;
#54574 = DIRECTION ( 'NONE',  ( -0.07836865515943411409, -0.9240274869783758893, -0.3742079063795003546 ) ) ;
#54575 = CARTESIAN_POINT ( 'NONE',  ( 5.959547316686252039, -14.51632612601518879, -14.51128755440536366 ) ) ;
#54576 = CARTESIAN_POINT ( 'NONE',  ( 0.5987334308729318488, -42.48817502201134744, 24.62352310025235269 ) ) ;
#54577 = CARTESIAN_POINT ( 'NONE',  ( 0.5809828226811553087, -41.20389530892325070, 24.41822904836909203 ) ) ;
#54578 = LINE ( 'NONE', #35831, #51054 ) ;
#54579 = B_SPLINE_CURVE_WITH_KNOTS ( 'NONE', 3,
 ( #20105, #5953, #33898, #29176, #24793, #53576, #52976, #10079, #43932, #14481, #20406, #52663, #25096, #9759, #28866, #5040, #5348, #57971, #53889, #39225, #16022, #36073, #30096, #39852, #11313 ),
 .UNSPECIFIED., .F., .F.,
 ( 4, 3, 3, 3, 3, 3, 3, 3, 4 ),
 ( 4.670885906470169154E-18, 0.0005656085177311400737, 0.001131215744874498538, 0.001696821861372766133, 0.002262427090022497717, 0.002828031679238745925, 0.003393635864401603995, 0.003977030878808132490, 0.004561030005651159000 ),
 .UNSPECIFIED. ) ;
#54580 = CARTESIAN_POINT ( 'NONE',  ( 0.6846871229502899947, -47.60345020167346775, -5.395516691087686389 ) ) ;
#54581 = CARTESIAN_POINT ( 'NONE',  ( 0.3676999524040323597, -23.56959980820351674, 37.28839696479283106 ) ) ;
#54582 = CARTESIAN_POINT ( 'NONE',  ( 2.299746137290199943, 46.92539900250360319, 14.22280795560328137 ) ) ;
#54583 = CARTESIAN_POINT ( 'NONE',  ( 4.967162193818130511, 8.839793687085803597, -42.16965968614184135 ) ) ;
#54584 = EDGE_CURVE ( 'NONE', #23687, #9918, #18191, .T. ) ;
#54585 =( BOUNDED_SURFACE ( )  B_SPLINE_SURFACE ( 3, 1, ( 
 ( #43862, #906 ),
 ( #15647, #39462 ),
 ( #10948, #20042 ),
 ( #39157, #58212 ) ),
 .UNSPECIFIED., .F., .F., .F. ) 
 B_SPLINE_SURFACE_WITH_KNOTS ( ( 4, 4 ),
 ( 2, 2 ),
 ( 0.000000000000000000, 1.000000000000000000 ),
 ( 0.000000000000000000, 1.000000000000000000 ),
 .UNSPECIFIED. ) 
 GEOMETRIC_REPRESENTATION_ITEM ( )  RATIONAL_B_SPLINE_SURFACE ( (
 ( 1.000000000000000000, 1.000000000000000000),
 ( 0.7211978278499970862, 0.9934217856018976445),
 ( 0.7211978278499970862, 0.9934217856018976445),
 ( 1.000000000000000000, 1.000000000000000000) ) ) 
 REPRESENTATION_ITEM ( '' )  SURFACE ( )  );
#54586 = B_SPLINE_CURVE_WITH_KNOTS ( 'NONE', 3,
 ( #24271, #49005, #61842, #10180 ),
 .UNSPECIFIED., .F., .F.,
 ( 4, 4 ),
 ( 2.147596245779529078E-17, 0.004559932413162187670 ),
 .UNSPECIFIED. ) ;
#54587 = CARTESIAN_POINT ( 'NONE',  ( 4.553261556744875094, -36.93702150832111641, 23.77385134801386712 ) ) ;
#54588 = CARTESIAN_POINT ( 'NONE',  ( 4.967162193818130511, 28.74031574030012237, 32.10009971360082659 ) ) ;
#54589 = CARTESIAN_POINT ( 'NONE',  ( 0.5998501479064708430, 46.60114184914316837, -11.94461217097420658 ) ) ;
#54590 =( BOUNDED_SURFACE ( )  B_SPLINE_SURFACE ( 3, 1, ( 
 ( #40916, #17090 ),
 ( #36201, #55268 ),
 ( #12391, #31480 ),
 ( #8912, #23325 ) ),
 .UNSPECIFIED., .F., .F., .F. ) 
 B_SPLINE_SURFACE_WITH_KNOTS ( ( 4, 4 ),
 ( 2, 2 ),
 ( 0.000000000000000000, 1.000000000000000000 ),
 ( 0.000000000000000000, 1.000000000000000000 ),
 .UNSPECIFIED. ) 
 GEOMETRIC_REPRESENTATION_ITEM ( )  RATIONAL_B_SPLINE_SURFACE ( (
 ( 1.000000000000000000, 1.000000000000000000),
 ( 0.9953390228620291325, 0.8624445117760984880),
 ( 0.9953390228620291325, 0.8624445117760984880),
 ( 1.000000000000000000, 1.000000000000000000) ) ) 
 REPRESENTATION_ITEM ( '' )  SURFACE ( )  );
#54592 = ORIENTED_EDGE ( 'NONE', *, *, #37744, .F. ) ;
#54591 = CARTESIAN_POINT ( 'NONE',  ( -6.016761891674565099, -18.68243340030204536, 2.456125503350645278 ) ) ;
#54593 = ORIENTED_EDGE ( 'NONE', *, *, #10195, .T. ) ;
#54594 = CARTESIAN_POINT ( 'NONE',  ( 0.7048096507298635682, 46.68221792389225300, 11.63498350884352739 ) ) ;
#54595 = CARTESIAN_POINT ( 'NONE',  ( 3.050102900204245682, 2.419036304482272026, -43.92691102884036525 ) ) ;
#54596 = CARTESIAN_POINT ( 'NONE',  ( 4.691466044806103852, 40.13652286047866369, 19.42108863068394342 ) ) ;
#54597 = ORIENTED_EDGE ( 'NONE', *, *, #31890, .T. ) ;
#54598 = EDGE_CURVE ( 'NONE', #11517, #4600, #35400, .T. ) ;
#54599 = ORIENTED_EDGE ( 'NONE', *, *, #30191, .F. ) ;
#54600 = CARTESIAN_POINT ( 'NONE',  ( 45.00000000000001421, 0.000000000000000000, 13.00000000000000178 ) ) ;
#54601 = DIRECTION ( 'NONE',  ( -1.000000000000000000, -0.000000000000000000, -0.000000000000000000 ) ) ;
#54602 = CARTESIAN_POINT ( 'NONE',  ( 1.227938101723748288, -36.73927144310496828, -22.18841447410757795 ) ) ;
#54603 = B_SPLINE_CURVE_WITH_KNOTS ( 'NONE', 3,
 ( #34194, #5336, #19788, #57040 ),
 .UNSPECIFIED., .F., .F.,
 ( 4, 4 ),
 ( 4.670885906470169154E-18, 0.004566006591234645501 ),
 .UNSPECIFIED. ) ;
#54604 = EDGE_LOOP ( 'NONE', ( #14760, #50722, #20210, #57629 ) ) ;
#54605 = ORIENTED_EDGE ( 'NONE', *, *, #43236, .F. ) ;
#54606 = CARTESIAN_POINT ( 'NONE',  ( 5.895596859100789899, 18.99884588797239005, -6.600911917118875039 ) ) ;
#54607 = CARTESIAN_POINT ( 'NONE',  ( 4.962356264823596597, 1.841560470688234474, 42.04574000888969465 ) ) ;
#54608 = AXIS2_PLACEMENT_3D ( 'NONE', #40209, #30140, #49251 ) ;
#54609 = CARTESIAN_POINT ( 'NONE',  ( 0.5837800304671215690, -38.63726306782081821, -26.57817214948214968 ) ) ;
#54610 = ORIENTED_EDGE ( 'NONE', *, *, #59880, .F. ) ;
#54611 = CYLINDRICAL_SURFACE ( 'NONE', #34093, 1.000000000000000666 ) ;
#54612 = CARTESIAN_POINT ( 'NONE',  ( 5.910764540655178756, 18.99430111539264843, -6.611940986348606941 ) ) ;
#54613 = CARTESIAN_POINT ( 'NONE',  ( 0.6254087463353902310, -24.64672211239934541, -41.31312313681398507 ) ) ;
#54614 = VERTEX_POINT ( 'NONE', #39430 ) ;
#54615 = AXIS2_PLACEMENT_3D ( 'NONE', #44238, #42998, #38300 ) ;
#54616 = EDGE_LOOP ( 'NONE', ( #11662, #56483, #38734, #4955 ) ) ;
#54617 = CARTESIAN_POINT ( 'NONE',  ( 4.549368137175248350, 38.40568845698277300, -19.17571786012283042 ) ) ;
#54618 = CARTESIAN_POINT ( 'NONE',  ( 0.5997462898726536595, -19.39900779840473888, 45.11352487427402025 ) ) ;
#54619 = B_SPLINE_CURVE_WITH_KNOTS ( 'NONE', 3,
 ( #58958, #11065, #1628, #35806 ),
 .UNSPECIFIED., .F., .F.,
 ( 4, 4 ),
 ( 0.000000000000000000, 0.004447772540403802446 ),
 .UNSPECIFIED. ) ;
#54620 = VERTEX_POINT ( 'NONE', #25299 ) ;
#54621 = CARTESIAN_POINT ( 'NONE',  ( 4.956653778116997699, 42.88673967249161478, -21.75875759808661059 ) ) ;
#54622 = CARTESIAN_POINT ( 'NONE',  ( 5.860006189529246790, -31.81514841426783136, 36.25227510158452304 ) ) ;
#54623 = CARTESIAN_POINT ( 'NONE',  ( 0.7044674535453004927, -38.84805681606468397, 30.04382140185760619 ) ) ;
#54624 = CARTESIAN_POINT ( 'NONE',  ( 4.226256110419178924, -43.82248454676872740, -3.227552963996462854 ) ) ;
#54625 = EDGE_CURVE ( 'NONE', #5464, #37539, #58545, .T. ) ;
#54626 = B_SPLINE_CURVE_WITH_KNOTS ( 'NONE', 3,
 ( #56838, #33071, #9234, #28343 ),
 .UNSPECIFIED., .F., .F.,
 ( 4, 4 ),
 ( 0.000000000000000000, 0.004445488388166992516 ),
 .UNSPECIFIED. ) ;
#54627 = ORIENTED_EDGE ( 'NONE', *, *, #10261, .T. ) ;
#54628 = CARTESIAN_POINT ( 'NONE',  ( -6.072942160501519915, 19.09631935424743077, -2.476842629158153564 ) ) ;
#54629 = CARTESIAN_POINT ( 'NONE',  ( 0.6026777506516367566, -35.15493876059303346, 34.28814184781924013 ) ) ;
#54630 = EDGE_CURVE ( 'NONE', #50134, #52459, #33182, .T. ) ;
#54631 = CARTESIAN_POINT ( 'NONE',  ( 0.9756950546413939440, -21.53795086961238425, -37.11135009583549760 ) ) ;
#54632 = ORIENTED_EDGE ( 'NONE', *, *, #2768, .F. ) ;
#54633 = FACE_OUTER_BOUND ( 'NONE', #60353, .T. ) ;
#54634 = CARTESIAN_POINT ( 'NONE',  ( 0.7764146366350256345, 5.581186775678419032, 46.57135200790456508 ) ) ;
#54636 = EDGE_LOOP ( 'NONE', ( #45261, #38338, #33153, #13155 ) ) ;
#54635 = EDGE_CURVE ( 'NONE', #14061, #59068, #4723, .T. ) ;
#54637 = CARTESIAN_POINT ( 'NONE',  ( 0.5987334308729317378, -48.62339718036277958, 6.879546003219879857 ) ) ;
#54638 = CARTESIAN_POINT ( 'NONE',  ( 0.7764139734771243750, -41.45356087563890668, -21.94636101126028649 ) ) ;
#54639 = ADVANCED_FACE ( 'NONE', ( #18384 ), #52708, .F. ) ;
#54640 = ORIENTED_EDGE ( 'NONE', *, *, #57907, .T. ) ;
#54641 = CARTESIAN_POINT ( 'NONE',  ( -2.708315649062916552, 5.356004933109461241, -13.61924161399628730 ) ) ;
#54642 = EDGE_CURVE ( 'NONE', #52094, #38290, #39180, .T. ) ;
#54643 = CARTESIAN_POINT ( 'NONE',  ( 4.967162193818130511, -38.83676580803754064, -18.65818244221298983 ) ) ;
#54644 = CARTESIAN_POINT ( 'NONE',  ( 0.1365634738349413013, -42.51423502781833008, -11.80688102856425203 ) ) ;
#54645 = B_SPLINE_CURVE_WITH_KNOTS ( 'NONE', 3,
 ( #60094, #17202, #59159, #36321, #55386, #30049 ),
 .UNSPECIFIED., .F., .F.,
 ( 4, 2, 4 ),
 ( 2.168404344971008868E-19, 0.0002291459268755698282, 0.0004582918537511394396 ),
 .UNSPECIFIED. ) ;
#54646 = CARTESIAN_POINT ( 'NONE',  ( 0.9968887458511638267, -15.81144734640156635, -39.89008038581160775 ) ) ;
#54647 = DIRECTION ( 'NONE',  ( 0.000000000000000000, 0.000000000000000000, 1.000000000000000000 ) ) ;
#54648 = EDGE_CURVE ( 'NONE', #10608, #1988, #36551, .T. ) ;
#54649 = CARTESIAN_POINT ( 'NONE',  ( 0.5782707292762423457, 16.17912178775543453, -44.02240761117678147 ) ) ;
#54650 = DIRECTION ( 'NONE',  ( -1.000000000000000000, -0.000000000000000000, -0.000000000000000000 ) ) ;
#54651 = CARTESIAN_POINT ( 'NONE',  ( -6.078457390727109555, -19.21674198601423456, 1.229365072086278987 ) ) ;
#54652 = CARTESIAN_POINT ( 'NONE',  ( 0.8744876279028263033, -48.57046782678510510, -7.159588358748426806 ) ) ;
#54653 = VECTOR ( 'NONE', #1032, 1000.000000000000114 ) ;
#54654 = EDGE_CURVE ( 'NONE', #39805, #22852, #38526, .T. ) ;
#54655 = CARTESIAN_POINT ( 'NONE',  ( 0.8557997880470690211, 7.156447707085701104, 47.37054680076709445 ) ) ;
#54656 = CARTESIAN_POINT ( 'NONE',  ( 0.9785694773339239649, 14.85438594643830434, 39.18778666713557612 ) ) ;
#54657 = ORIENTED_EDGE ( 'NONE', *, *, #51843, .F. ) ;
#54658 = MECHANICAL_DESIGN_GEOMETRIC_PRESENTATION_REPRESENTATION (  '', ( #2658 ), #41736 ) ;
#54659 = VECTOR ( 'NONE', #12156, 1000.000000000000227 ) ;
#54660 = CARTESIAN_POINT ( 'NONE',  ( -15.94111418026541038, -12.48882310846358301, -0.5454162216299145438 ) ) ;
#54661 = CARTESIAN_POINT ( 'NONE',  ( 4.694002226626921015, -4.034398983147053031, -45.40934261020431251 ) ) ;
#54662 = CARTESIAN_POINT ( 'NONE',  ( 4.691466044806103852, 2.583163953528483159, -44.51344083442436528 ) ) ;
#54663 = CARTESIAN_POINT ( 'NONE',  ( 0.1156495703730067298, 44.02457461872624833, -2.963069839081658330 ) ) ;
#54664 = CARTESIAN_POINT ( 'NONE',  ( 4.549368137175248350, -32.13400537129945178, 28.46244473166616729 ) ) ;
#54665 = CARTESIAN_POINT ( 'NONE',  ( 2.618530812446115519, -12.57566640959698923, 45.29436392701340708 ) ) ;
#54666 = DIRECTION ( 'NONE',  ( 1.301032001305298307E-16, -0.7042738517259679032, 0.7099284060911139616 ) ) ;
#54667 = CARTESIAN_POINT ( 'NONE',  ( -5.283180000000052168, 15.43999999999999240, 0.000000000000000000 ) ) ;
#54668 = CARTESIAN_POINT ( 'NONE',  ( 0.6023142530420679819, 41.53076277789742932, -24.28014345169125932 ) ) ;
#54669 = AXIS2_PLACEMENT_3D ( 'NONE', #11713, #36146, #2593 ) ;
#54670 = CARTESIAN_POINT ( 'NONE',  ( 0.1073791018717578927, -6.109314776653017809, 42.68962945260943087 ) ) ;
#54672 = ORIENTED_EDGE ( 'NONE', *, *, #20041, .T. ) ;
#54671 = CARTESIAN_POINT ( 'NONE',  ( 4.962356264823602814, 41.15374796524927348, -8.809348799717806600 ) ) ;
#54673 = ORIENTED_EDGE ( 'NONE', *, *, #33324, .T. ) ;
#54674 = CARTESIAN_POINT ( 'NONE',  ( 3.660176727303412036, -10.60619300811838706, -46.85282580473590031 ) ) ;
#54675 = CARTESIAN_POINT ( 'NONE',  ( 4.975801465491695552, -8.787181743660504196, 47.10002938642126935 ) ) ;
#54676 = CARTESIAN_POINT ( 'NONE',  ( 5.000000000000000888, 0.000000000000000000, 0.000000000000000000 ) ) ;
#54677 = EDGE_CURVE ( 'NONE', #45978, #39651, #33556, .T. ) ;
#54678 = CARTESIAN_POINT ( 'NONE',  ( 3.661933894777862797, 42.53630112315261869, 20.08218742348897123 ) ) ;
#54679 = FACE_OUTER_BOUND ( 'NONE', #56840, .T. ) ;
#54680 = CARTESIAN_POINT ( 'NONE',  ( 0.8560838555295158248, 40.81790744942473737, -23.11430867518922128 ) ) ;
#54682 = EDGE_CURVE ( 'NONE', #46849, #12584, #13516, .T. ) ;
#54681 = ORIENTED_EDGE ( 'NONE', *, *, #17896, .F. ) ;
#54683 = VERTEX_POINT ( 'NONE', #13689 ) ;
#54684 = CARTESIAN_POINT ( 'NONE',  ( 3.270143674763207553, -13.28976595685395878, 3.277085381513066942 ) ) ;
#54685 = CARTESIAN_POINT ( 'NONE',  ( 0.1103310638050661735, -39.81020119244070798, -16.57910240621627906 ) ) ;
#54686 = CARTESIAN_POINT ( 'NONE',  ( 0.7057020205115027700, 41.89806668505412546, -23.21851350879774145 ) ) ;
#54687 = ORIENTED_EDGE ( 'NONE', *, *, #48043, .F. ) ;
#54688 = ORIENTED_EDGE ( 'NONE', *, *, #22515, .T. ) ;
#54689 = CARTESIAN_POINT ( 'NONE',  ( 0.1100247026804066219, -0.1696715072120354439, 43.12411436000287779 ) ) ;
#54690 = CARTESIAN_POINT ( 'NONE',  ( -5.283180000000052168, 1.890854657883512518E-15, -15.43999999999999240 ) ) ;
#54691 = ORIENTED_EDGE ( 'NONE', *, *, #44873, .T. ) ;
#54692 = CARTESIAN_POINT ( 'NONE',  ( 4.549368137175248350, -8.582197505784124658, -42.06008734272393212 ) ) ;
#54693 = CARTESIAN_POINT ( 'NONE',  ( 0.9756008150404594792, 41.40938772927948719, -11.24277293639946151 ) ) ;
#54694 = CIRCLE ( 'NONE', #33771, 10.00000000000000000 ) ;
#54695 = ORIENTED_EDGE ( 'NONE', *, *, #7323, .F. ) ;
#54696 = CARTESIAN_POINT ( 'NONE',  ( 0.9754292580325131246, 4.774021070332235439, -41.63575614449710827 ) ) ;
#54697 = DIRECTION ( 'NONE',  ( -1.000000000000000000, -0.000000000000000000, -0.000000000000000000 ) ) ;
#54698 = MECHANICAL_DESIGN_GEOMETRIC_PRESENTATION_REPRESENTATION (  '', ( #11723 ), #43870 ) ;
#54699 = ORIENTED_EDGE ( 'NONE', *, *, #12532, .T. ) ;
#54700 = AXIS2_PLACEMENT_3D ( 'NONE', #19174, #18866, #23540 ) ;
#54701 = CARTESIAN_POINT ( 'NONE',  ( 0.8557997880470697982, -41.93815086860240626, -23.15977007032367041 ) ) ;
#54702 = CARTESIAN_POINT ( 'NONE',  ( 0.8560838555295223751, 44.99141268455589682, -13.27198623905683128 ) ) ;
#54703 = FACE_OUTER_BOUND ( 'NONE', #13446, .T. ) ;
#54704 = ORIENTED_EDGE ( 'NONE', *, *, #9656, .F. ) ;
#54705 = CARTESIAN_POINT ( 'NONE',  ( 0.5800708119828326126, -33.42085299104044793, 34.30831427709740922 ) ) ;
#54706 = LINE ( 'NONE', #54395, #53001 ) ;
#54707 = EDGE_CURVE ( 'NONE', #2564, #46325, #3628, .T. ) ;
#54708 = ORIENTED_EDGE ( 'NONE', *, *, #19225, .T. ) ;
#54709 = DIRECTION ( 'NONE',  ( -1.000000000000000000, -0.000000000000000000, -0.000000000000000000 ) ) ;
#54710 =( BOUNDED_SURFACE ( )  B_SPLINE_SURFACE ( 3, 1, ( 
 ( #6100, #15852 ),
 ( #59045, #24629 ),
 ( #20249, #39364 ),
 ( #58420, #34968 ) ),
 .UNSPECIFIED., .F., .F., .F. ) 
 B_SPLINE_SURFACE_WITH_KNOTS ( ( 4, 4 ),
 ( 2, 2 ),
 ( 0.000000000000000000, 1.000000000000000000 ),
 ( 0.000000000000000000, 1.000000000000000000 ),
 .UNSPECIFIED. ) 
 GEOMETRIC_REPRESENTATION_ITEM ( )  RATIONAL_B_SPLINE_SURFACE ( (
 ( 1.000000000000000000, 1.000000000000000000),
 ( 0.7223157951917476005, 0.9931996967497186413),
 ( 0.7223157951917476005, 0.9931996967497186413),
 ( 1.000000000000000000, 1.000000000000000000) ) ) 
 REPRESENTATION_ITEM ( '' )  SURFACE ( )  );
#54711 = EDGE_LOOP ( 'NONE', ( #23286, #13749, #22765, #41969 ) ) ;
#54712 = CARTESIAN_POINT ( 'NONE',  ( 4.975801465491695552, 40.15204426031497320, 26.14269827151694514 ) ) ;
#54713 = ORIENTED_EDGE ( 'NONE', *, *, #35677, .T. ) ;
#54714 = CARTESIAN_POINT ( 'NONE',  ( 0.8551540677456715978, -0.9122407826472468395, -47.90804413217341562 ) ) ;
#54716 = AXIS2_PLACEMENT_3D ( 'NONE', #7606, #36465, #45870 ) ;
#54715 = CARTESIAN_POINT ( 'NONE',  ( 0.8557997880470599172, 37.44587306708097429, 29.88293891557482951 ) ) ;
#54717 = EDGE_CURVE ( 'NONE', #52878, #48540, #2494, .T. ) ;
#54718 = CARTESIAN_POINT ( 'NONE',  ( 0.1129192098497455998, -43.82135468580280957, 5.161459220629533107 ) ) ;
#54719 = ORIENTED_EDGE ( 'NONE', *, *, #10675, .F. ) ;
#54720 = FACE_OUTER_BOUND ( 'NONE', #11940, .T. ) ;
#54721 = ADVANCED_FACE ( 'NONE', ( #55637 ), #8648, .F. ) ;
#54722 = CARTESIAN_POINT ( 'NONE',  ( 0.5997462898726536595, 46.76781179977606229, 14.97743000668126001 ) ) ;
#54723 = CARTESIAN_POINT ( 'NONE',  ( 4.975610109902397937, -40.67634447773618689, 27.16402781375239073 ) ) ;
#54724 = ORIENTED_EDGE ( 'NONE', *, *, #41067, .T. ) ;
#54725 = AXIS2_PLACEMENT_3D ( 'NONE', #45152, #2182, #50131 ) ;
#54726 = B_SPLINE_CURVE_WITH_KNOTS ( 'NONE', 3,
 ( #45696, #3058, #22185, #8076, #17482, #12802, #31897, #14036, #52212, #61903, #33137, #57508, #14648, #24029, #28111, #23724 ),
 .UNSPECIFIED., .F., .F.,
 ( 4, 3, 3, 3, 3, 4 ),
 ( 1.214354834101861570E-17, 0.0002732102107931896743, 0.0004098135523333821303, 0.0005464168938824984917, 0.0008195847345945436605, 0.001092771384553106566 ),
 .UNSPECIFIED. ) ;
#54727 = ORIENTED_EDGE ( 'NONE', *, *, #23280, .T. ) ;
#54728 = CARTESIAN_POINT ( 'NONE',  ( 0.8751705887134423323, -44.08562551107069538, -19.22545746485646490 ) ) ;
#54729 = CARTESIAN_POINT ( 'NONE',  ( 0.9722240741986378776, -42.90442369863401950, -0.5819399500324929919 ) ) ;
#54730 = CARTESIAN_POINT ( 'NONE',  ( 4.975610109902397937, 0.000000000000000000, 0.000000000000000000 ) ) ;
#54731 = CARTESIAN_POINT ( 'NONE',  ( 4.975610109902397937, -16.35148546628888866, -46.09857188876371481 ) ) ;
#54732 = CARTESIAN_POINT ( 'NONE',  ( 0.5835226383429287234, -30.41628309188208945, -35.69442810048165171 ) ) ;
#54733 = CARTESIAN_POINT ( 'NONE',  ( -6.077587904424778920, -16.14165210942818618, 10.49967087922869702 ) ) ;
#54734 = EDGE_LOOP ( 'NONE', ( #23203, #42723, #38531, #37244 ) ) ;
#54735 = CARTESIAN_POINT ( 'NONE',  ( 0.5804410086790514622, 28.25755288515070518, 37.43034272883842561 ) ) ;
#54736 = DIRECTION ( 'NONE',  ( -2.249565377136137858E-32, 1.224646799147353207E-16, 1.000000000000000000 ) ) ;
#54737 = ORIENTED_EDGE ( 'NONE', *, *, #48095, .T. ) ;
#54738 = CARTESIAN_POINT ( 'NONE',  ( -2.569797478183783568, -5.182550149005390239, 13.68441171582007598 ) ) ;
#54739 = CARTESIAN_POINT ( 'NONE',  ( 0.5830081025819917606, 36.97261815548455388, 28.84887417406409682 ) ) ;
#54740 = CARTESIAN_POINT ( 'NONE',  ( 0.6846871229502932144, 43.92355552798038332, 19.12907057981221115 ) ) ;
#54741 = CARTESIAN_POINT ( 'NONE',  ( 4.967162193818130511, -35.57684288741994294, 24.30453456948097823 ) ) ;
#54742 = CARTESIAN_POINT ( 'NONE',  ( 1.231276596079881935, -37.02495017545860634, -19.65781868679418309 ) ) ;
#54743 = CARTESIAN_POINT ( 'NONE',  ( 6.999999999999990230, 85.00000000000001421, 1.040949779275250495E-14 ) ) ;
#54744 = DIRECTION ( 'NONE',  ( -1.000000000000000000, -0.000000000000000000, -0.000000000000000000 ) ) ;
#54745 = CARTESIAN_POINT ( 'NONE',  ( 0.1157506346131639274, -12.64344793106056031, -42.27391493838008074 ) ) ;
#54746 = CARTESIAN_POINT ( 'NONE',  ( 0.9756354156337448957, -39.69194847698940265, 16.29989858042615225 ) ) ;
#54747 = CARTESIAN_POINT ( 'NONE',  ( 0.2279481005628848644, 30.21908332445557832, -32.14514722477598951 ) ) ;
#54748 = CIRCLE ( 'NONE', #27755, 4.250000000000000000 ) ;
#54749 = CARTESIAN_POINT ( 'NONE',  ( 0.5997462898726536595, 4.195097405482933972, 48.92803682862026449 ) ) ;
#54750 = CARTESIAN_POINT ( 'NONE',  ( 7.000000000000006217, 1.285836671513502826E-15, -1.348150961071066192E-31 ) ) ;
#54751 = AXIS2_PLACEMENT_3D ( 'NONE', #27698, #17683, #27381 ) ;
#54752 = B_SPLINE_CURVE_WITH_KNOTS ( 'NONE', 3,
 ( #34406, #42349, #15607, #53477, #870, #29996, #14149, #43827, #13840, #20302 ),
 .UNSPECIFIED., .F., .F.,
 ( 4, 3, 3, 4 ),
 ( 0.0005236741812375312905, 0.0005236998216949950062, 0.0007855159896329595411, 0.001047349442285928738 ),
 .UNSPECIFIED. ) ;
#54753 = VECTOR ( 'NONE', #14145, 1000.000000000000114 ) ;
#54754 = CARTESIAN_POINT ( 'NONE',  ( 4.291220156522059348, -9.951772474099044530, 46.04727160136049235 ) ) ;
#54755 = CARTESIAN_POINT ( 'NONE',  ( 4.553261556744875094, 0.000000000000000000, 0.000000000000000000 ) ) ;
#54756 = PRODUCT ( 'circlip for shafts normal_din_Circlip DIN 471 - 20 x 1.2', 'circlip for shafts normal_din_Circlip DIN 471 - 20 x 1.2', '', ( #45936 ) ) ;
#54757 = CARTESIAN_POINT ( 'NONE',  ( -6.218809015666120210, -1.096543817334992621, 4.142297321093258830E-16 ) ) ;
#54758 = CARTESIAN_POINT ( 'NONE',  ( 0.7762777257811875886, -47.37038525518530463, -7.133808567472758710 ) ) ;
#54759 = ADVANCED_FACE ( 'NONE', ( #55957 ), #59106, .F. ) ;
#54760 = VERTEX_POINT ( 'NONE', #27459 ) ;
#54761 = CARTESIAN_POINT ( 'NONE',  ( 0.1103878639767399694, 11.11454059769200420, -41.66755962011269077 ) ) ;
#54762 = CARTESIAN_POINT ( 'NONE',  ( 0.5837800304671224572, -19.69888330479335181, -42.55809357482583266 ) ) ;
#54763 = CARTESIAN_POINT ( 'NONE',  ( 0.9752132459055852243, -39.73079175141339192, -16.20487516111995774 ) ) ;
#54764 = B_SPLINE_CURVE_WITH_KNOTS ( 'NONE', 3,
 ( #32589, #48226, #47007, #57581 ),
 .UNSPECIFIED., .F., .F.,
 ( 4, 4 ),
 ( 0.000000000000000000, 0.004446090762761376394 ),
 .UNSPECIFIED. ) ;
#54765 = DIRECTION ( 'NONE',  ( 0.09722883295013594329, -0.8634569929835251845, -0.4949632060173795312 ) ) ;
#54766 = CARTESIAN_POINT ( 'NONE',  ( 0.9730545539215883499, 39.44597740938085195, -16.88610103448514721 ) ) ;
#54767 = EDGE_LOOP ( 'NONE', ( #50008, #27789, #51340, #38268 ) ) ;
#54768 = FACE_OUTER_BOUND ( 'NONE', #41101, .T. ) ;
#54769 = CARTESIAN_POINT ( 'NONE',  ( 4.975610109902397937, 34.73360008816180056, -34.43873447229760387 ) ) ;
#54770 = AXIS2_PLACEMENT_3D ( 'NONE', #52428, #23942, #9218 ) ;
#54771 =( BOUNDED_SURFACE ( )  B_SPLINE_SURFACE ( 3, 1, ( 
 ( #26221, #25926 ),
 ( #7407, #26536 ),
 ( #45363, #17452 ),
 ( #11853, #45061 ) ),
 .UNSPECIFIED., .F., .F., .F. ) 
 B_SPLINE_SURFACE_WITH_KNOTS ( ( 4, 4 ),
 ( 2, 2 ),
 ( 0.000000000000000000, 1.000000000000000000 ),
 ( 0.000000000000000000, 1.000000000000000000 ),
 .UNSPECIFIED. ) 
 GEOMETRIC_REPRESENTATION_ITEM ( )  RATIONAL_B_SPLINE_SURFACE ( (
 ( 1.000000000000000000, 1.000000000000000000),
 ( 0.9751682680413298332, 0.9999560080971552356),
 ( 0.9751682680413298332, 0.9999560080971552356),
 ( 1.000000000000000000, 1.000000000000000000) ) ) 
 REPRESENTATION_ITEM ( '' )  SURFACE ( )  );
#54772 = FACE_OUTER_BOUND ( 'NONE', #61967, .T. ) ;
#54773 = EDGE_LOOP ( 'NONE', ( #14194, #43927, #3835, #40294 ) ) ;
#54774 = B_SPLINE_CURVE_WITH_KNOTS ( 'NONE', 3,
 ( #26210, #12441, #26837, #45351, #39732, #58781, #54084, #20904, #11205, #30292, #49402, #6455, #25599, #44736, #40050, #59100 ),
 .UNSPECIFIED., .F., .F.,
 ( 4, 3, 3, 3, 3, 4 ),
 ( 9.813676791237319219E-18, 0.0002724568934985644917, 0.0004086836638483901216, 0.0005449104342063723671, 0.0008173270854453691669, 0.001089761613562680986 ),
 .UNSPECIFIED. ) ;
#54775 = CARTESIAN_POINT ( 'NONE',  ( 0.1119899015040014406, -0.8531642396357116409, -44.11613558521091250 ) ) ;
#54776 = VECTOR ( 'NONE', #54987, 999.9999999999998863 ) ;
#54777 = ORIENTED_EDGE ( 'NONE', *, *, #17457, .T. ) ;
#54778 = CARTESIAN_POINT ( 'NONE',  ( 4.956445790443998689, -27.49627641100115838, 38.22947597952995835 ) ) ;
#54779 = CARTESIAN_POINT ( 'NONE',  ( 4.909518593419350374, 0.8656805903097125610, 8.896908036367455278E-17 ) ) ;
#54780 = ORIENTED_EDGE ( 'NONE', *, *, #13980, .T. ) ;
#54781 = CARTESIAN_POINT ( 'NONE',  ( 0.8551540677456739292, 28.44084013485118589, 38.56334384152441430 ) ) ;
#54782 = ORIENTED_EDGE ( 'NONE', *, *, #61708, .T. ) ;
#54783 = DIRECTION ( 'NONE',  ( -1.000000000000000000, -1.836909530733554547E-16, -1.836909530733573529E-16 ) ) ;
#54784 = CARTESIAN_POINT ( 'NONE',  ( 0.1101816497532063094, -26.36013219694247667, -34.13008584880283536 ) ) ;
#54785 = ORIENTED_EDGE ( 'NONE', *, *, #3737, .F. ) ;
#54786 = ORIENTED_EDGE ( 'NONE', *, *, #1861, .T. ) ;
#54787 = CARTESIAN_POINT ( 'NONE',  ( 4.335381028904216727, -33.67825942593300681, 35.57431221687780010 ) ) ;
#54788 = EDGE_CURVE ( 'NONE', #331, #40436, #57771, .T. ) ;
#54789 = VERTEX_POINT ( 'NONE', #17152 ) ;
#54790 = CARTESIAN_POINT ( 'NONE',  ( 0.1097557419366048670, 11.37678103520278583, 41.59672960874316061 ) ) ;
#54791 =( BOUNDED_SURFACE ( )  B_SPLINE_SURFACE ( 3, 1, ( 
 ( #60499, #32335 ),
 ( #37350, #32028 ),
 ( #51730, #8197 ),
 ( #51411, #42366 ) ),
 .UNSPECIFIED., .F., .F., .F. ) 
 B_SPLINE_SURFACE_WITH_KNOTS ( ( 4, 4 ),
 ( 2, 2 ),
 ( 0.000000000000000000, 1.000000000000000000 ),
 ( 0.000000000000000000, 1.000000000000000000 ),
 .UNSPECIFIED. ) 
 GEOMETRIC_REPRESENTATION_ITEM ( )  RATIONAL_B_SPLINE_SURFACE ( (
 ( 1.000000000000000000, 1.000000000000000000),
 ( 0.7211978278499968642, 0.9934217856018975334),
 ( 0.7211978278499968642, 0.9934217856018975334),
 ( 1.000000000000000000, 1.000000000000000000) ) ) 
 REPRESENTATION_ITEM ( '' )  SURFACE ( )  );
#54793 = ADVANCED_FACE ( 'NONE', ( #36888 ), #5854, .F. ) ;
#54792 = EDGE_LOOP ( 'NONE', ( #17079, #53314, #22967, #10794 ) ) ;
#54794 = VERTEX_POINT ( 'NONE', #19622 ) ;
#54795 = CARTESIAN_POINT ( 'NONE',  ( -6.078075953587585900, -16.13536320617233244, 10.50929248103962443 ) ) ;
#54796 = LINE ( 'NONE', #40433, #37481 ) ;
#54797 = AXIS2_PLACEMENT_3D ( 'NONE', #530, #19667, #17134 ) ;
#54798 = CARTESIAN_POINT ( 'NONE',  ( 0.1103878639767399417, -16.45816205842789515, 39.86034920885558108 ) ) ;
#54799 = CARTESIAN_POINT ( 'NONE',  ( 0.5998501479064699549, 44.64337787626223530, 17.92509395669123862 ) ) ;
#54800 = EDGE_LOOP ( 'NONE', ( #40047, #29601, #7894, #38943 ) ) ;
#54801 = EDGE_CURVE ( 'NONE', #46201, #41166, #32396, .T. ) ;
#54802 = CARTESIAN_POINT ( 'NONE',  ( 0.9785694773339257413, -17.84245254737231434, 37.92073697608524441 ) ) ;
#54803 = FACE_OUTER_BOUND ( 'NONE', #31208, .T. ) ;
#54804 = ORIENTED_EDGE ( 'NONE', *, *, #32544, .T. ) ;
#54805 = ORIENTED_EDGE ( 'NONE', *, *, #46906, .F. ) ;
#54806 = B_SPLINE_CURVE_WITH_KNOTS ( 'NONE', 3,
 ( #5772, #15218, #5163, #153, #23987, #5471 ),
 .UNSPECIFIED., .F., .F.,
 ( 4, 2, 4 ),
 ( 1.222218565161306604E-16, 0.0002448718616795921748, 0.0004897437233590620515 ),
 .UNSPECIFIED. ) ;
#54807 = CARTESIAN_POINT ( 'NONE',  ( 0.5998501479064699549, -23.59887241503383493, 41.92175333043579144 ) ) ;
#54808 = CARTESIAN_POINT ( 'NONE',  ( 0.5997462898726536595, -48.76843890605309184, 5.761162800240605897 ) ) ;
#54809 = CARTESIAN_POINT ( 'NONE',  ( 0.9780106845699476636, 40.50128780264890338, -10.76925869233542699 ) ) ;
#54810 = VERTEX_POINT ( 'NONE', #53107 ) ;
#54811 = LINE ( 'NONE', #8135, #8522 ) ;
#54812 = DIRECTION ( 'NONE',  ( 0.000000000000000000, 0.000000000000000000, -1.000000000000000000 ) ) ;
#54813 = CARTESIAN_POINT ( 'NONE',  ( -19.79535493905475008, -12.45603257510279249, -1.053715328945894036 ) ) ;
#54814 = EDGE_CURVE ( 'NONE', #39487, #18847, #45180, .T. ) ;
#54815 = CONICAL_SURFACE ( 'NONE', #8809, 43.08621763946400307, 1.568696531533066763 ) ;
#54816 = ORIENTED_EDGE ( 'NONE', *, *, #48886, .F. ) ;
#54817 = CARTESIAN_POINT ( 'NONE',  ( 4.553261556744873317, 27.21079963941887314, -34.48350256002191117 ) ) ;
#54818 = ORIENTED_EDGE ( 'NONE', *, *, #46312, .T. ) ;
#54819 = EDGE_CURVE ( 'NONE', #20457, #49238, #42820, .T. ) ;
#54820 = CARTESIAN_POINT ( 'NONE',  ( 0.8753041380234530822, -47.26389509135299249, 13.31399822241830577 ) ) ;
#54821 = CARTESIAN_POINT ( 'NONE',  ( 0.7242003506640024568, -26.15097733078639308, -41.55885054679355761 ) ) ;
#54822 = CARTESIAN_POINT ( 'NONE',  ( 2.618530812446111078, -42.57172246446608455, 19.93427288883829718 ) ) ;
#54823 = VERTEX_POINT ( 'NONE', #10213 ) ;
#54824 = CARTESIAN_POINT ( 'NONE',  ( 0.9762797500689124330, 41.59901070109194876, 5.084003725032276932 ) ) ;
#54825 = CARTESIAN_POINT ( 'NONE',  ( 0.000000000000000000, 0.000000000000000000, -5.599999999999999645 ) ) ;
#54826 = AXIS2_PLACEMENT_3D ( 'NONE', #18251, #56436, #35592 ) ;
#54827 = FACE_OUTER_BOUND ( 'NONE', #10572, .T. ) ;
#54828 = FACE_OUTER_BOUND ( 'NONE', #20681, .T. ) ;
#54829 = B_SPLINE_CURVE_WITH_KNOTS ( 'NONE', 3,
 ( #45424, #30674, #17518, #40736, #59805, #2473 ),
 .UNSPECIFIED., .F., .F.,
 ( 4, 2, 4 ),
 ( 3.471140604459641645E-18, 0.0002291459268755729724, 0.0004582918537511424754 ),
 .UNSPECIFIED. ) ;
#54830 = CARTESIAN_POINT ( 'NONE',  ( 5.959547316686252039, 20.35048796920736791, -2.675599016784323769 ) ) ;
#54831 = CARTESIAN_POINT ( 'NONE',  ( 5.894904586330512508, 19.70964338679892691, -4.007414331817491515 ) ) ;
#54832 = CARTESIAN_POINT ( 'NONE',  ( 1.227938101723748288, -37.58536632582793402, 20.72293514920737323 ) ) ;
#54833 = CARTESIAN_POINT ( 'NONE',  ( -6.072942160501519027, -1.834587804586597759, -19.16868409349693891 ) ) ;
#54834 = CARTESIAN_POINT ( 'NONE',  ( 3.660176727303412036, 8.130955556895155922, -47.34518114598549943 ) ) ;
#54835 = EDGE_CURVE ( 'NONE', #41630, #12616, #3960, .T. ) ;
#54836 = AXIS2_PLACEMENT_3D ( 'NONE', #28419, #18113, #4590 ) ;
#54837 = ORIENTED_EDGE ( 'NONE', *, *, #58271, .F. ) ;
#54838 = VECTOR ( 'NONE', #12492, 1000.000000000000000 ) ;
#54839 = CARTESIAN_POINT ( 'NONE',  ( 0.5997462898726536595, -19.39900779840410294, -45.11352487427429736 ) ) ;
#54840 = CARTESIAN_POINT ( 'NONE',  ( -6.015611763856276717, 18.68284711750061788, -2.453375430803879986 ) ) ;
#54841 = CARTESIAN_POINT ( 'NONE',  ( 1.231276596079881047, -30.51591784428347154, -28.74118176309054107 ) ) ;
#54842 = ORIENTED_EDGE ( 'NONE', *, *, #5639, .F. ) ;
#54843 = CARTESIAN_POINT ( 'NONE',  ( -6.078457390727109555, -18.90008989325092870, -3.685256173530143897 ) ) ;
#54844 = CARTESIAN_POINT ( 'NONE',  ( 0.8744876279028263033, 27.35388303025786882, 40.76904626731490566 ) ) ;
#54845 = B_SPLINE_CURVE_WITH_KNOTS ( 'NONE', 3,
 ( #29689, #20014, #48488, #49113 ),
 .UNSPECIFIED., .F., .F.,
 ( 4, 4 ),
 ( 0.000000000000000000, 0.004444103432399265294 ),
 .UNSPECIFIED. ) ;
#54846 = CARTESIAN_POINT ( 'NONE',  ( 0.9762797500689124330, 41.90547441298052433, -0.5059638413352701702 ) ) ;
#54847 = ORIENTED_EDGE ( 'NONE', *, *, #28467, .T. ) ;
#54848 = CARTESIAN_POINT ( 'NONE',  ( 0.5806925824938499181, 11.40214825760356376, -45.48860711711441240 ) ) ;
#54849 = CARTESIAN_POINT ( 'NONE',  ( -6.016489644550736315, 13.32727118274438105, 13.32104266208103738 ) ) ;
#54850 = VERTEX_POINT ( 'NONE', #38426 ) ;
#54851 = CARTESIAN_POINT ( 'NONE',  ( -6.077587904424778920, -4.278847002849007097, -18.77465018902190863 ) ) ;
#54852 = VECTOR ( 'NONE', #14882, 1000.000000000000000 ) ;
#54853 = ORIENTED_EDGE ( 'NONE', *, *, #10402, .F. ) ;
#54854 = VERTEX_POINT ( 'NONE', #37827 ) ;
#54855 = CARTESIAN_POINT ( 'NONE',  ( 0.5806925824938499181, 22.05663578530122493, 41.38510819338441138 ) ) ;
#54856 = ORIENTED_EDGE ( 'NONE', *, *, #387, .F. ) ;
#54857 = CARTESIAN_POINT ( 'NONE',  ( 4.549368137175248350, 0.000000000000000000, 0.000000000000000000 ) ) ;
#54858 = ORIENTED_EDGE ( 'NONE', *, *, #13335, .T. ) ;
#54859 = CARTESIAN_POINT ( 'NONE',  ( 1.227938101723756947, -39.96870412324324917, -15.63977281655884077 ) ) ;
#54860 = DIRECTION ( 'NONE',  ( 0.09722883295013594329, -0.6146093961964115282, 0.7828166095262905078 ) ) ;
#54861 = EDGE_CURVE ( 'NONE', #9797, #46207, #5513, .T. ) ;
#54862 =( BOUNDED_SURFACE ( )  B_SPLINE_SURFACE ( 3, 1, ( 
 ( #20945, #24718 ),
 ( #43857, #900 ),
 ( #20038, #15332 ),
 ( #5883, #25030 ) ),
 .UNSPECIFIED., .F., .F., .F. ) 
 B_SPLINE_SURFACE_WITH_KNOTS ( ( 4, 4 ),
 ( 2, 2 ),
 ( 0.000000000000000000, 1.000000000000000000 ),
 ( 0.000000000000000000, 1.000000000000000000 ),
 .UNSPECIFIED. ) 
 GEOMETRIC_REPRESENTATION_ITEM ( )  RATIONAL_B_SPLINE_SURFACE ( (
 ( 1.000000000000000000, 1.000000000000000000),
 ( 0.9953485035131437453, 0.8621029689291523912),
 ( 0.9953485035131437453, 0.8621029689291523912),
 ( 1.000000000000000000, 1.000000000000000000) ) ) 
 REPRESENTATION_ITEM ( '' )  SURFACE ( )  );
#54863 = ORIENTED_EDGE ( 'NONE', *, *, #50693, .F. ) ;
#54864 = CARTESIAN_POINT ( 'NONE',  ( 4.962356264823601038, -35.98698831890646943, 21.82137185415336589 ) ) ;
#54865 = CARTESIAN_POINT ( 'NONE',  ( 48.50340449756345151, 12.37737586902969333, -1.750926327775586211 ) ) ;
#54866 = CARTESIAN_POINT ( 'NONE',  ( 0.1100247026804066219, -30.61332956994603194, 30.37337782329838376 ) ) ;
#54867 = AXIS2_PLACEMENT_3D ( 'NONE', #59922, #41464, #17033 ) ;
#54868 = CARTESIAN_POINT ( 'NONE',  ( 0.8751705887134423323, -41.19904111682490822, -24.81530984069193480 ) ) ;
#54869 = ORIENTED_EDGE ( 'NONE', *, *, #40779, .T. ) ;
#54870 = ADVANCED_FACE ( 'NONE', ( #28692 ), #43863, .F. ) ;
#54871 = EDGE_LOOP ( 'NONE', ( #17275, #17654, #48874, #36902 ) ) ;
#54872 = CARTESIAN_POINT ( 'NONE',  ( 0.5807400328401574052, -24.41979442053198568, 41.20655774452961850 ) ) ;
#54873 = DIRECTION ( 'NONE',  ( 0.1011922191286468292, -0.9269080304894992128, -0.3613884859841242636 ) ) ;
#54874 = B_SPLINE_CURVE_WITH_KNOTS ( 'NONE', 3,
 ( #61081, #14123, #33225, #18194 ),
 .UNSPECIFIED., .F., .F.,
 ( 4, 4 ),
 ( 0.000000000000000000, 0.005013413432710146778 ),
 .UNSPECIFIED. ) ;
#54875 = CARTESIAN_POINT ( 'NONE',  ( 2.359973842542475886, 13.77930139075350269, -41.81227986866154822 ) ) ;
#54876 = ORIENTED_EDGE ( 'NONE', *, *, #3443, .T. ) ;
#54877 = DIRECTION ( 'NONE',  ( 0.000000000000000000, -0.7071067811865449082, -0.7071067811865500152 ) ) ;
#54878 = CARTESIAN_POINT ( 'NONE',  ( 0.5987334363312689645, 48.08272125986815837, 9.980722554900580690 ) ) ;
#54879 = CARTESIAN_POINT ( 'NONE',  ( 2.879087469061463178, 8.095492153095989352, -43.25002524372141721 ) ) ;
#54880 = CARTESIAN_POINT ( 'NONE',  ( 0.8760168074886960365, 28.57146030081928245, 38.69913431881832366 ) ) ;
#54881 = VECTOR ( 'NONE', #12344, 1000.000000000000227 ) ;
#54882 = AXIS2_PLACEMENT_3D ( 'NONE', #35885, #54955, #12089 ) ;
#54883 = ORIENTED_EDGE ( 'NONE', *, *, #25236, .F. ) ;
#54884 = B_SPLINE_CURVE_WITH_KNOTS ( 'NONE', 3,
 ( #13949, #3573, #38371, #22704, #13319, #3886 ),
 .UNSPECIFIED., .F., .F.,
 ( 4, 2, 4 ),
 ( 3.471140604459641645E-18, 0.0002291966416970813011, 0.0004583932833941591328 ),
 .UNSPECIFIED. ) ;
#54885 = VERTEX_POINT ( 'NONE', #42510 ) ;
#54886 = CARTESIAN_POINT ( 'NONE',  ( 0.6064515330803575965, 21.91205122295670904, -41.46319268025084881 ) ) ;
#54887 = CARTESIAN_POINT ( 'NONE',  ( 0.1073791018717483448, 34.50606437925512182, 25.86618856530722610 ) ) ;
#54888 =( BOUNDED_SURFACE ( )  B_SPLINE_SURFACE ( 3, 1, ( 
 ( #44918, #31098 ),
 ( #36132, #59274 ),
 ( #35505, #45228 ),
 ( #26393, #55195 ) ),
 .UNSPECIFIED., .F., .F., .F. ) 
 B_SPLINE_SURFACE_WITH_KNOTS ( ( 4, 4 ),
 ( 2, 2 ),
 ( 0.000000000000000000, 1.000000000000000000 ),
 ( 0.000000000000000000, 1.000000000000000000 ),
 .UNSPECIFIED. ) 
 GEOMETRIC_REPRESENTATION_ITEM ( )  RATIONAL_B_SPLINE_SURFACE ( (
 ( 1.000000000000000000, 1.000000000000000000),
 ( 0.7269869731126817891, 0.9931720237060910339),
 ( 0.7269869731126817891, 0.9931720237060910339),
 ( 1.000000000000000000, 1.000000000000000000) ) ) 
 REPRESENTATION_ITEM ( '' )  SURFACE ( )  );
#54889 = DIRECTION ( 'NONE',  ( -0.07439287786467650709, 0.1170659376278977565, -0.9903339163990660943 ) ) ;
#54890 = ADVANCED_FACE ( 'NONE', ( #56878 ), #61874, .F. ) ;
#54891 = CARTESIAN_POINT ( 'NONE',  ( 5.896278296736517710, -19.39967646272030422, 5.308439766650788094 ) ) ;
#54892 = DIRECTION ( 'NONE',  ( 1.000000000000000000, 1.836909530733573776E-16, -1.925929944387235853E-32 ) ) ;
#54893 = B_SPLINE_CURVE_WITH_KNOTS ( 'NONE', 3,
 ( #48447, #6424, #19971, #29961 ),
 .UNSPECIFIED., .F., .F.,
 ( 4, 4 ),
 ( 0.000000000000000000, 0.005014147105413703856 ),
 .UNSPECIFIED. ) ;
#54894 = CARTESIAN_POINT ( 'NONE',  ( 0.2285344041767079226, 25.86074962531460386, 35.74524862289040072 ) ) ;
#54895 = CARTESIAN_POINT ( 'NONE',  ( -6.010958268070873523, -18.19761767765826477, -4.891065400978576783 ) ) ;
#54896 = CARTESIAN_POINT ( 'NONE',  ( 0.3676999524040366896, -38.02468164711607557, 22.36233818182511257 ) ) ;
#54897 = AXIS2_PLACEMENT_3D ( 'NONE', #42162, #61215, #47152 ) ;
#54898 = CARTESIAN_POINT ( 'NONE',  ( 0.9730545539215883499, 5.099196237954877198, 42.60426903087355299 ) ) ;
#54899 = CARTESIAN_POINT ( 'NONE',  ( 0.7762777257811899201, -41.92424087089327855, 23.17763256463755894 ) ) ;
#54900 = DIRECTION ( 'NONE',  ( 0.07500201931887538753, 0.7485533666540395981, -0.6588190604171937359 ) ) ;
#54901 = CARTESIAN_POINT ( 'NONE',  ( 4.226256110419179812, 40.88307703899232592, -16.10593871250618392 ) ) ;
#54902 = CARTESIAN_POINT ( 'NONE',  ( 0.5824935313925944103, -14.24163328556457309, -44.68124951714464999 ) ) ;
#54903 = CARTESIAN_POINT ( 'NONE',  ( 1.088908134280557993, 42.64123480278975364, 4.826714665689003425 ) ) ;
#54904 = CARTESIAN_POINT ( 'NONE',  ( -6.063463321072278589, -17.34291445406321230, -8.369215657307158551 ) ) ;
#54905 = CARTESIAN_POINT ( 'NONE',  ( 0.7948878604505663636, -38.82350069238938062, 30.05718618378071127 ) ) ;
#54906 = CARTESIAN_POINT ( 'NONE',  ( -6.016761891674565099, 18.68153697670641833, 2.462934516563870080 ) ) ;
#54907 = CARTESIAN_POINT ( 'NONE',  ( 0.6846871229502899947, -24.69859318104460399, -41.05093867799210727 ) ) ;
#54909 = VERTEX_POINT ( 'NONE', #38128 ) ;
#54908 = CARTESIAN_POINT ( 'NONE',  ( 5.880360259849752858, 47.05949693022707692, -9.312491912827638885 ) ) ;
#54910 = ORIENTED_EDGE ( 'NONE', *, *, #59619, .F. ) ;
#54911 = CARTESIAN_POINT ( 'NONE',  ( 0.6016118706126976079, 17.28650708908693900, -45.96441805835117123 ) ) ;
#54912 = CARTESIAN_POINT ( 'NONE',  ( 7.999999999999996447, 2.649999999999714806, 80.00000000000002842 ) ) ;
#54913 = ORIENTED_EDGE ( 'NONE', *, *, #24775, .F. ) ;
#54914 = VERTEX_POINT ( 'NONE', #19309 ) ;
#54915 = CARTESIAN_POINT ( 'NONE',  ( 4.834790513006555379, -16.75039937818070612, -44.18159641293900108 ) ) ;
#54917 = FACE_OUTER_BOUND ( 'NONE', #3458, .T. ) ;
#54916 = B_SPLINE_CURVE_WITH_KNOTS ( 'NONE', 3,
 ( #7193, #40452, #35437, #26322 ),
 .UNSPECIFIED., .F., .F.,
 ( 4, 4 ),
 ( 0.000000000000000000, 0.005013413432710153717 ),
 .UNSPECIFIED. ) ;
#54918 = EDGE_CURVE ( 'NONE', #9573, #16048, #33961, .T. ) ;
#54919 = B_SPLINE_CURVE_WITH_KNOTS ( 'NONE', 3,
 ( #37804, #38721, #29288, #10191 ),
 .UNSPECIFIED., .F., .F.,
 ( 4, 4 ),
 ( 0.000000000000000000, 0.004444103432399269631 ),
 .UNSPECIFIED. ) ;
#54920 = ORIENTED_EDGE ( 'NONE', *, *, #4768, .T. ) ;
#54921 = ORIENTED_EDGE ( 'NONE', *, *, #17771, .F. ) ;
#54922 = CARTESIAN_POINT ( 'NONE',  ( 0.5834872094924179464, 47.89542889285419136, 0.2270145249674854482 ) ) ;
#54923 = EDGE_CURVE ( 'NONE', #7236, #17964, #51124, .T. ) ;
#54924 = VECTOR ( 'NONE', #47178, 1000.000000000000000 ) ;
#54925 = CARTESIAN_POINT ( 'NONE',  ( -15.25000000000000711, -2.688986455804108555, -9.952330921218299798E-16 ) ) ;
#54926 = CARTESIAN_POINT ( 'NONE',  ( 0.5817216825391119395, -38.91887341143593915, -26.16402577188925349 ) ) ;
#54927 = ORIENTED_EDGE ( 'NONE', *, *, #44839, .T. ) ;
#54928 = CARTESIAN_POINT ( 'NONE',  ( 0.2940133293163010308, -17.11870290862044897, -40.65944613868263247 ) ) ;
#54929 = B_SPLINE_CURVE_WITH_KNOTS ( 'NONE', 3,
 ( #15396, #34500, #27557, #8136 ),
 .UNSPECIFIED., .F., .F.,
 ( 4, 4 ),
 ( 0.000000000000000000, 0.005004948556313808770 ),
 .UNSPECIFIED. ) ;
#54930 = CARTESIAN_POINT ( 'NONE',  ( 0.7246131072078524360, -19.16331062551114428, 44.12003537001145048 ) ) ;
#54931 = CARTESIAN_POINT ( 'NONE',  ( 0.8751705887134553219, -24.81530984069179269, -41.19904111682499348 ) ) ;
#54932 = ORIENTED_EDGE ( 'NONE', *, *, #55861, .F. ) ;
#54933 = ADVANCED_FACE ( 'NONE', ( #58715 ), #18707, .F. ) ;
#54934 = ORIENTED_EDGE ( 'NONE', *, *, #20277, .T. ) ;
#54935 = CARTESIAN_POINT ( 'NONE',  ( 0.9722240741986374335, 0.5819399500326425390, -42.90442369863401950 ) ) ;
#54936 = DIRECTION ( 'NONE',  ( -0.1024043820194934645, 0.5087173657443641028, -0.8548216096550907972 ) ) ;
#54937 = VECTOR ( 'NONE', #52580, 1000.000000000000000 ) ;
#54938 = VERTEX_POINT ( 'NONE', #34955 ) ;
#54939 = CARTESIAN_POINT ( 'NONE',  ( 0.6026112563231247332, -8.009419346916665461, 48.44987303006526247 ) ) ;
#54940 = CARTESIAN_POINT ( 'NONE',  ( 3.661921753702025217, 15.13536876490557681, -44.53708270850657414 ) ) ;
#54941 = DIRECTION ( 'NONE',  ( -1.685288351013738149E-16, 1.000000000000000000, 0.000000000000000000 ) ) ;
#54942 = EDGE_CURVE ( 'NONE', #23289, #19565, #22740, .T. ) ;
#54943 = ORIENTED_EDGE ( 'NONE', *, *, #44725, .F. ) ;
#54944 = CARTESIAN_POINT ( 'NONE',  ( 4.956445790444026223, 13.43466403631445338, -45.13366650706537797 ) ) ;
#54945 = CARTESIAN_POINT ( 'NONE',  ( 0.6025881611877910160, 18.20817581200352819, 44.52856035602914631 ) ) ;
#54946 = EDGE_CURVE ( 'NONE', #7385, #60067, #16447, .T. ) ;
#54947 = DIRECTION ( 'NONE',  ( 1.000000000000000000, 0.000000000000000000, -0.000000000000000000 ) ) ;
#54948 = CARTESIAN_POINT ( 'NONE',  ( 4.553261556744875094, 0.000000000000000000, 0.000000000000000000 ) ) ;
#54949 = DIRECTION ( 'NONE',  ( 0.000000000000000000, 0.000000000000000000, 1.000000000000000000 ) ) ;
#54950 = ORIENTED_EDGE ( 'NONE', *, *, #44418, .F. ) ;
#54951 = CARTESIAN_POINT ( 'NONE',  ( 0.1092565886968784872, 42.71401356099878655, -5.936467125236589482 ) ) ;
#54952 = CARTESIAN_POINT ( 'NONE',  ( 4.335381028904201628, -46.80143676542513731, -14.47005059964403628 ) ) ;
#54953 = CARTESIAN_POINT ( 'NONE',  ( 0.7245667037590751702, 42.06183421678296241, 23.33692989609125945 ) ) ;
#54954 = ORIENTED_EDGE ( 'NONE', *, *, #23420, .F. ) ;
#54955 = DIRECTION ( 'NONE',  ( 0.9848077530122079093, 0.1736481776669314137, -2.220446049250313081E-16 ) ) ;
#54956 = DIRECTION ( 'NONE',  ( -0.07906939808003035641, -0.5295738273858142664, 0.8445706552060647798 ) ) ;
#54957 = CARTESIAN_POINT ( 'NONE',  ( 4.967162193818130511, 38.44485641567072776, 19.45289607368836116 ) ) ;
#54958 = ADVANCED_FACE ( 'NONE', ( #54633 ), #25095, .F. ) ;
#54959 = B_SPLINE_CURVE_WITH_KNOTS ( 'NONE', 3,
 ( #10250, #32911, #6127, #58443, #24344, #15267, #48450, #20570, #34371, #57836, #5819, #49074, #29652, #48761, #5517, #39703 ),
 .UNSPECIFIED., .F., .F.,
 ( 4, 3, 3, 3, 3, 4 ),
 ( 1.398620802506300720E-17, 0.0002724568934985550049, 0.0004086836638483777075, 0.0005449104342063626092, 0.0008173270854453675406, 0.001089761613562686624 ),
 .UNSPECIFIED. ) ;
#54960 = DIRECTION ( 'NONE',  ( -0.07500201931887527651, -0.9744221909196664200, 0.2118397765798677723 ) ) ;
#54961 =( BOUNDED_SURFACE ( )  B_SPLINE_SURFACE ( 3, 1, ( 
 ( #35888, #13313 ),
 ( #32416, #41211 ),
 ( #51492, #60272 ),
 ( #18324, #28620 ) ),
 .UNSPECIFIED., .F., .F., .F. ) 
 B_SPLINE_SURFACE_WITH_KNOTS ( ( 4, 4 ),
 ( 2, 2 ),
 ( 0.000000000000000000, 1.000000000000000000 ),
 ( 0.000000000000000000, 1.000000000000000000 ),
 .UNSPECIFIED. ) 
 GEOMETRIC_REPRESENTATION_ITEM ( )  RATIONAL_B_SPLINE_SURFACE ( (
 ( 1.000000000000000000, 1.000000000000000000),
 ( 0.9732289882329797637, 0.9999525324661233672),
 ( 0.9732289882329797637, 0.9999525324661233672),
 ( 1.000000000000000000, 1.000000000000000000) ) ) 
 REPRESENTATION_ITEM ( '' )  SURFACE ( )  );
#54962 = CARTESIAN_POINT ( 'NONE',  ( 0.1073791018717483448, -34.50606437925530656, -25.86618856530698451 ) ) ;
#54963 = CARTESIAN_POINT ( 'NONE',  ( 0.9749527285493305717, -5.317382389862895131, -42.57770849153631332 ) ) ;
#54964 = CARTESIAN_POINT ( 'NONE',  ( 0.8551540677456715978, 11.51835730326479457, 46.51172240253124812 ) ) ;
#54965 = CARTESIAN_POINT ( 'NONE',  ( 5.999999999999997335, 15.72000000000000064, 0.000000000000000000 ) ) ;
#54966 = CARTESIAN_POINT ( 'NONE',  ( 0.5997462898726536595, 40.86908001809362645, -27.22627276398607421 ) ) ;
#54967 = CARTESIAN_POINT ( 'NONE',  ( 2.500000000000000000, -1.178949249685214307, 2.042000000000001592 ) ) ;
#54968 = ORIENTED_EDGE ( 'NONE', *, *, #36675, .F. ) ;
#54969 = AXIS2_PLACEMENT_3D ( 'NONE', #54075, #21826, #55314 ) ;
#54970 = CARTESIAN_POINT ( 'NONE',  ( 5.960721111146673579, 17.77250458025977764, 10.26825948882932060 ) ) ;
#54971 = CARTESIAN_POINT ( 'NONE',  ( 4.322998006666179727, -10.36018990813345653, 46.85697641700690497 ) ) ;
#54972 = CARTESIAN_POINT ( 'NONE',  ( -4.000000000000000000, 1.935983797701083420, -5.350530693383767300 ) ) ;
#54973 = CARTESIAN_POINT ( 'NONE',  ( 3.783278058412227640, -38.10568111914489720, -20.00643011788494263 ) ) ;
#54974 = CARTESIAN_POINT ( 'NONE',  ( 4.553261556744875094, 0.000000000000000000, 0.000000000000000000 ) ) ;
#54975 = CARTESIAN_POINT ( 'NONE',  ( 0.9785694773339244090, -31.23050093752737411, 27.94622008261178792 ) ) ;
#54976 = SHAPE_DEFINITION_REPRESENTATION ( #50783, #13 ) ;
#54977 = CARTESIAN_POINT ( 'NONE',  ( 5.895881250540457863, 17.94906520686009088, -9.075171613153402816 ) ) ;
#54978 = CARTESIAN_POINT ( 'NONE',  ( 0.9790724872846775506, -7.010505575501338349, 41.31813187400074838 ) ) ;
#54979 = CARTESIAN_POINT ( 'NONE',  ( 0.9762797500689124330, 29.49606728235556830, -29.77090526101713763 ) ) ;
#54980 = EDGE_CURVE ( 'NONE', #49420, #24289, #10518, .T. ) ;
#54982 = ORIENTED_EDGE ( 'NONE', *, *, #196, .T. ) ;
#54981 = CARTESIAN_POINT ( 'NONE',  ( 0.7948878604505671408, -45.17791583987795434, 19.22640287894023103 ) ) ;
#54983 = VERTEX_POINT ( 'NONE', #11763 ) ;
#54985 = AXIS2_PLACEMENT_3D ( 'NONE', #31893, #60672, #8071 ) ;
#54984 = CARTESIAN_POINT ( 'NONE',  ( 2.624215991343620935, -40.85210347989548296, 25.21574086439692053 ) ) ;
#54986 = DIRECTION ( 'NONE',  ( 0.1024043820194936449, 0.9878630899050855341, 0.1167898032637372935 ) ) ;
#54987 = DIRECTION ( 'NONE',  ( 0.07500201931887538753, 0.7304373162253416929, 0.6788490437229849350 ) ) ;
#54988 = ADVANCED_FACE ( 'NONE', ( #7020 ), #26151, .T. ) ;
#54989 = ORIENTED_EDGE ( 'NONE', *, *, #4482, .F. ) ;
#54990 = CARTESIAN_POINT ( 'NONE',  ( 0.5850706913938534814, -12.57184842331985131, -46.21698775168658813 ) ) ;
#54991 = CARTESIAN_POINT ( 'NONE',  ( 5.917102823773431552, 3.353685953999505642, 19.83034312798667642 ) ) ;
#54992 = CARTESIAN_POINT ( 'NONE',  ( 0.8751705887134553219, -46.21789262997766201, 13.30665218149281870 ) ) ;
#54993 = EDGE_CURVE ( 'NONE', #2725, #47783, #30845, .T. ) ;
#54994 = EDGE_LOOP ( 'NONE', ( #42639, #1792, #37558, #50779 ) ) ;
#54995 = ORIENTED_EDGE ( 'NONE', *, *, #20252, .T. ) ;
#54996 = CARTESIAN_POINT ( 'NONE',  ( 0.5800708119828336118, -44.00606550371072956, 18.90714262039457694 ) ) ;
#54997 = ADVANCED_FACE ( 'NONE', ( #59033 ), #61010, .F. ) ;
#54998 = EDGE_CURVE ( 'NONE', #5168, #33426, #1099, .T. ) ;
#54999 = CARTESIAN_POINT ( 'NONE',  ( 2.281448460670306932, -22.83953674062048478, 42.18752512472231331 ) ) ;
#55000 = CARTESIAN_POINT ( 'NONE',  ( 0.3622758884714600280, -4.808133778521581192, -42.84426538328729350 ) ) ;
#55001 = VERTEX_POINT ( 'NONE', #59341 ) ;
#55002 = ORIENTED_EDGE ( 'NONE', *, *, #38299, .T. ) ;
#55003 = CARTESIAN_POINT ( 'NONE',  ( 0.6000166863083090663, -25.90381862410917435, 41.72308308835420121 ) ) ;
#55004 = DIRECTION ( 'NONE',  ( 0.000000000000000000, 0.000000000000000000, 1.000000000000000000 ) ) ;
#55005 = ORIENTED_EDGE ( 'NONE', *, *, #10862, .T. ) ;
#55006 = B_SPLINE_CURVE_WITH_KNOTS ( 'NONE', 3,
 ( #26334, #61069, #3433, #41388 ),
 .UNSPECIFIED., .F., .F.,
 ( 4, 4 ),
 ( 5.818439421673297140E-18, 0.004566006591234645501 ),
 .UNSPECIFIED. ) ;
#55007 = CARTESIAN_POINT ( 'NONE',  ( 3.783198216974393180, -29.18723368117341366, -31.62918462580868706 ) ) ;
#55008 = CARTESIAN_POINT ( 'NONE',  ( 3.270143674763207553, -8.548517033725330450, 10.69018354892884659 ) ) ;
#55009 = ORIENTED_EDGE ( 'NONE', *, *, #25209, .T. ) ;
#55010 = EDGE_CURVE ( 'NONE', #6447, #16220, #46519, .T. ) ;
#55011 = CARTESIAN_POINT ( 'NONE',  ( 0.5997462898726536595, 22.24958391914565681, -43.77793560195825506 ) ) ;
#55012 = CARTESIAN_POINT ( 'NONE',  ( 0.8551540677456834771, -46.03951182599436720, 13.28067116677185844 ) ) ;
#55013 = EDGE_LOOP ( 'NONE', ( #3442, #15863 ) ) ;
#55014 = LINE ( 'NONE', #40969, #18520 ) ;
#55015 = ADVANCED_FACE ( 'NONE', ( #31469 ), #36498, .F. ) ;
#55016 = CARTESIAN_POINT ( 'NONE',  ( 0.5837800005270550319, -19.74012976957846632, 42.53895315263395815 ) ) ;
#55017 = CARTESIAN_POINT ( 'NONE',  ( 3.678748215320120529, 48.39168598034271440, 7.540394040060985681 ) ) ;
#55018 = CARTESIAN_POINT ( 'NONE',  ( 0.8744876279028306332, -42.33402326122651971, 24.86323641237049387 ) ) ;
#55019 = EDGE_LOOP ( 'NONE', ( #24810, #22934, #59835, #21321 ) ) ;
#55020 = CARTESIAN_POINT ( 'NONE',  ( 5.965394784446458765, -7.841344330025064480, 18.96850062921621571 ) ) ;
#55021 = CARTESIAN_POINT ( 'NONE',  ( 0.8560838555295223751, -18.91252766612315739, 42.92655508376904550 ) ) ;
#55022 = ORIENTED_EDGE ( 'NONE', *, *, #169, .F. ) ;
#55023 = EDGE_CURVE ( 'NONE', #38495, #49884, #42548, .T. ) ;
#55024 = CIRCLE ( 'NONE', #34049, 47.91270532121795611 ) ;
#55025 = EDGE_LOOP ( 'NONE', ( #50896, #31668, #55967, #16918, #4247, #55152, #32002, #2602, #48351, #31325, #37084, #12376, #54323, #12153, #59621, #34162, #51444, #37082, #20431, #18149, #6216, #45476, #20450, #37696, #43511, #19711, #24068, #38746, #49342, #20389, #6159, #7286, #41679, #6055, #13928, #15082, #44721, #9323, #54305, #13324, #33397, #26546, #48158, #4159, #14022, #6125, #20013, #3797, #12438, #31135, #60722, #15502, #47921, #2611, #44388, #61162, #29506, #44824, #28075, #50297, #5921, #12054, #25120, #48107, #10107, #33227, #32384, #16620, #58001, #21331, #36047, #34611, #22608, #58334, #920, #46988, #47804, #23348, #14521, #28527, #5617, #23974, #14844, #38777, #52710, #50499, #11920, #53866, #27174, #20925, #40892, #35326, #3236, #54847, #57251, #17606, #22872, #50092, #8236, #33928, #32, #25753, #16114, #15108, #11917, #11520, #35959, #35258, #33175, #59304, #9544, #19435, #60847, #40644, #24073, #7055, #53706, #17287, #21222, #8974, #7263, #55478, #56844, #48617, #23516, #26946, #26917, #2285, #16490, #30126, #50045, #48201, #19932, #7648, #40726, #9329, #36770, #47825, #5133, #943, #48122, #36550, #9589, #5447, #36710, #15358, #4393, #21606 ) ) ;
#55026 = CARTESIAN_POINT ( 'NONE',  ( 0.5837374860065669413, -18.16107481025629156, 44.31936661703463898 ) ) ;
#55027 = ORIENTED_EDGE ( 'NONE', *, *, #6258, .T. ) ;
#55028 = CARTESIAN_POINT ( 'NONE',  ( 0.3622758884714600280, 41.42293301073608802, 11.95365414648511582 ) ) ;
#55029 = CARTESIAN_POINT ( 'NONE',  ( 0.6008123274975391004, -25.82835474539317389, 41.76662115020298671 ) ) ;
#55030 = AXIS2_PLACEMENT_3D ( 'NONE', #7519, #26646, #26964 ) ;
#55031 = CARTESIAN_POINT ( 'NONE',  ( 0.3622758884714600280, -20.83792692158946025, -37.74294673546579304 ) ) ;
#55032 = EDGE_LOOP ( 'NONE', ( #21603, #28686, #38870, #40957 ) ) ;
#55033 = DIRECTION ( 'NONE',  ( 0.000000000000000000, 0.000000000000000000, -1.000000000000000000 ) ) ;
#55034 = DIRECTION ( 'NONE',  ( 0.000000000000000000, 0.000000000000000000, 1.000000000000000000 ) ) ;
#55035 = LINE ( 'NONE', #6171, #29904 ) ;
#55037 = ORIENTED_EDGE ( 'NONE', *, *, #6193, .T. ) ;
#55036 = EDGE_CURVE ( 'NONE', #7202, #4827, #13646, .T. ) ;
#55038 = B_SPLINE_CURVE_WITH_KNOTS ( 'NONE', 3,
 ( #33042, #42441, #56197, #13311 ),
 .UNSPECIFIED., .F., .F.,
 ( 4, 4 ),
 ( 0.000000000000000000, 0.004442905043737215703 ),
 .UNSPECIFIED. ) ;
#55039 = VERTEX_POINT ( 'NONE', #40905 ) ;
#55040 = DIRECTION ( 'NONE',  ( 0.000000000000000000, 0.000000000000000000, 1.000000000000000000 ) ) ;
#55041 = CARTESIAN_POINT ( 'NONE',  ( 5.960721111146673579, 19.82454228767745974, -5.318514366754729217 ) ) ;
#55043 = EDGE_CURVE ( 'NONE', #10045, #21039, #51787, .T. ) ;
#55042 = CARTESIAN_POINT ( 'NONE',  ( 0.6029443199889047422, 33.01497303511078485, 36.35311812410746057 ) ) ;
#55044 = CARTESIAN_POINT ( 'NONE',  ( 0.3622758884714730732, -41.85013935980095567, -10.35929834645908265 ) ) ;
#55045 = CARTESIAN_POINT ( 'NONE',  ( 0.5837800304671205698, -30.24261836534340731, -35.84161501087377388 ) ) ;
#55046 = CARTESIAN_POINT ( 'NONE',  ( 0.2230388203127606772, 41.84042374003679043, 10.42432885623897043 ) ) ;
#55047 = VERTEX_POINT ( 'NONE', #46510 ) ;
#55048 = FACE_OUTER_BOUND ( 'NONE', #11049, .T. ) ;
#55049 = CARTESIAN_POINT ( 'NONE',  ( 3.680974057930773036, -46.78530430706945253, 10.62112035260160603 ) ) ;
#55050 = ORIENTED_EDGE ( 'NONE', *, *, #6926, .F. ) ;
#55051 = CARTESIAN_POINT ( 'NONE',  ( 0.6846871229502932144, 19.12907057981263748, -43.92355552798018437 ) ) ;
#55052 = CARTESIAN_POINT ( 'NONE',  ( 0.5837800304671219020, 36.77575525172623827, 29.09950442610023558 ) ) ;
#55053 = CARTESIAN_POINT ( 'NONE',  ( 0.8557997880470697982, 44.60232077416686991, 17.48760788519232889 ) ) ;
#55054 = CARTESIAN_POINT ( 'NONE',  ( 0.7048096507298579061, -47.80151517212789969, 5.442192462018654808 ) ) ;
#55055 = CARTESIAN_POINT ( 'NONE',  ( 21.00000000000000000, 2.055000000000000160, 0.000000000000000000 ) ) ;
#55056 = CARTESIAN_POINT ( 'NONE',  ( 0.6016117650947689910, 5.062075601541858205, 48.84594604313416966 ) ) ;
#55057 = FILL_AREA_STYLE_COLOUR ( '', #11893 ) ;
#55058 = CARTESIAN_POINT ( 'NONE',  ( 0.6031357023905875581, 38.13964912630292758, 29.32055886552335977 ) ) ;
#55059 = CARTESIAN_POINT ( 'NONE',  ( 4.962356264823602814, -33.29728444345256122, -25.73958909062380229 ) ) ;
#55060 = CARTESIAN_POINT ( 'NONE',  ( 5.959547316686252039, -2.682663672454773440, -20.34955788964375856 ) ) ;
#55061 = VECTOR ( 'NONE', #26499, 1000.000000000000000 ) ;
#55062 = CARTESIAN_POINT ( 'NONE',  ( 5.958863334805807099, 7.855954700275622038, -18.96276366205785635 ) ) ;
#55063 = CARTESIAN_POINT ( 'NONE',  ( -6.057079549204054558, -18.27862279149365676, -6.059965341982332276 ) ) ;
#55064 = B_SPLINE_CURVE_WITH_KNOTS ( 'NONE', 3,
 ( #34985, #1421, #20558, #48748, #54045, #25554 ),
 .UNSPECIFIED., .F., .F.,
 ( 4, 2, 4 ),
 ( 0.000000000000000000, 0.0002447195606305752882, 0.0004894391212611505764 ),
 .UNSPECIFIED. ) ;
#55065 = CARTESIAN_POINT ( 'NONE',  ( 2.526464513654342880, -34.82216969498448833, -25.19161096467265182 ) ) ;
#55066 = CARTESIAN_POINT ( 'NONE',  ( 5.896782393890504181, 3.339090646272911300, -19.83372281075806853 ) ) ;
#55067 = CARTESIAN_POINT ( 'NONE',  ( 4.390527457369402420, 17.48986963896179603, 40.30247879027717062 ) ) ;
#55068 = EDGE_CURVE ( 'NONE', #39264, #32330, #42070, .T. ) ;
#55069 = CARTESIAN_POINT ( 'NONE',  ( 4.553261556744873317, 40.80044851610476542, 16.27461110774448372 ) ) ;
#55070 = CARTESIAN_POINT ( 'NONE',  ( 0.8551540677456715978, -24.74404575822804730, 41.03346287276420412 ) ) ;
#55071 = EDGE_CURVE ( 'NONE', #50920, #2500, #15525, .T. ) ;
#55072 = VECTOR ( 'NONE', #45088, 1000.000000000000000 ) ;
#55073 = ORIENTED_EDGE ( 'NONE', *, *, #486, .T. ) ;
#55074 = FACE_OUTER_BOUND ( 'NONE', #52705, .T. ) ;
#55075 = EDGE_CURVE ( 'NONE', #478, #44297, #45063, .T. ) ;
#55076 = ADVANCED_FACE ( 'NONE', ( #26457 ), #31498, .F. ) ;
#55077 = CARTESIAN_POINT ( 'NONE',  ( 0.5806925824938502512, -20.23436166722406426, -42.30594485723652554 ) ) ;
#55078 = CARTESIAN_POINT ( 'NONE',  ( 0.9752570700956811889, -25.93764562640081195, -34.18150842933902567 ) ) ;
#55079 = DIRECTION ( 'NONE',  ( -1.000000000000000000, -0.000000000000000000, -0.000000000000000000 ) ) ;
#55080 = CARTESIAN_POINT ( 'NONE',  ( 0.9754402186311966760, 39.57010335554349467, -16.59348191374094128 ) ) ;
#55081 = EDGE_CURVE ( 'NONE', #19905, #29740, #51008, .T. ) ;
#55082 = ORIENTED_EDGE ( 'NONE', *, *, #56626, .F. ) ;
#55083 = LINE ( 'NONE', #11260, #32302 ) ;
#55084 = FACE_OUTER_BOUND ( 'NONE', #2623, .T. ) ;
#55085 = DIRECTION ( 'NONE',  ( 0.000000000000000000, 0.000000000000000000, 1.000000000000000000 ) ) ;
#55086 = EDGE_LOOP ( 'NONE', ( #51574, #31531, #11416, #46752 ) ) ;
#55087 = EDGE_CURVE ( 'NONE', #35404, #49963, #47252, .T. ) ;
#55088 =( BOUNDED_SURFACE ( )  B_SPLINE_SURFACE ( 3, 1, ( 
 ( #39123, #18851 ),
 ( #34410, #53481 ),
 ( #30000, #49412 ),
 ( #7093, #44745 ) ),
 .UNSPECIFIED., .F., .F., .F. ) 
 B_SPLINE_SURFACE_WITH_KNOTS ( ( 4, 4 ),
 ( 2, 2 ),
 ( 0.000000000000000000, 1.000000000000000000 ),
 ( 0.000000000000000000, 1.000000000000000000 ),
 .UNSPECIFIED. ) 
 GEOMETRIC_REPRESENTATION_ITEM ( )  RATIONAL_B_SPLINE_SURFACE ( (
 ( 1.000000000000000000, 1.000000000000000000),
 ( 0.9953390228620291325, 0.8624445117761032620),
 ( 0.9953390228620291325, 0.8624445117761032620),
 ( 1.000000000000000000, 1.000000000000000000) ) ) 
 REPRESENTATION_ITEM ( '' )  SURFACE ( )  );
#55089 = CARTESIAN_POINT ( 'NONE',  ( 0.3622758884714730732, 41.85013935980087751, 10.35929834645937397 ) ) ;
#55090 = ORIENTED_EDGE ( 'NONE', *, *, #11187, .F. ) ;
#55091 = FACE_OUTER_BOUND ( 'NONE', #60657, .T. ) ;
#55092 = CARTESIAN_POINT ( 'NONE',  ( 0.6029303876144825880, -29.38970229176932136, 38.08638053211486607 ) ) ;
#55093 = ORIENTED_EDGE ( 'NONE', *, *, #33871, .T. ) ;
#55094 = FACE_OUTER_BOUND ( 'NONE', #35652, .T. ) ;
#55095 = VERTEX_POINT ( 'NONE', #33955 ) ;
#55096 = CARTESIAN_POINT ( 'NONE',  ( 4.291220156522059348, 42.48586100259134923, 20.35535831603521117 ) ) ;
#55097 = CARTESIAN_POINT ( 'NONE',  ( 0.9762797500689124330, 36.31338395866797697, 20.92039508843128814 ) ) ;
#55098 = ORIENTED_EDGE ( 'NONE', *, *, #24589, .T. ) ;
#55099 = CARTESIAN_POINT ( 'NONE',  ( -6.063463321072278589, 13.84388120595888161, -13.38534294049907736 ) ) ;
#55100 = ORIENTED_EDGE ( 'NONE', *, *, #6587, .T. ) ;
#55101 = CARTESIAN_POINT ( 'NONE',  ( 1.091591847532204618, 28.57213991056969959, 30.66580851513083417 ) ) ;
#55102 = VERTEX_POINT ( 'NONE', #9508 ) ;
#55103 = ORIENTED_EDGE ( 'NONE', *, *, #11503, .F. ) ;
#55104 = CARTESIAN_POINT ( 'NONE',  ( 0.6001305935487422083, -34.38748867424691014, -33.64689939321930012 ) ) ;
#55105 = DIRECTION ( 'NONE',  ( -1.000000000000000000, -0.000000000000000000, -0.000000000000000000 ) ) ;
#55106 = DIRECTION ( 'NONE',  ( -0.07500201931887529039, 0.3709639164044522541, 0.9256135639801102988 ) ) ;
#55107 = DIRECTION ( 'NONE',  ( 0.000000000000000000, 0.000000000000000000, 1.000000000000000000 ) ) ;
#55108 = CARTESIAN_POINT ( 'NONE',  ( 0.5807400328401637335, 33.48217046439111755, 34.25275203086248155 ) ) ;
#55109 = ORIENTED_EDGE ( 'NONE', *, *, #37925, .F. ) ;
#55110 = CARTESIAN_POINT ( 'NONE',  ( 1.000433927950260982, -39.36980744151690459, 14.36791354618788041 ) ) ;
#55111 = CARTESIAN_POINT ( 'NONE',  ( 0.9790724872846782167, -17.67747698414031277, 37.99792122546497097 ) ) ;
#55112 = LINE ( 'NONE', #10995, #38934 ) ;
#55113 = B_SPLINE_CURVE_WITH_KNOTS ( 'NONE', 3,
 ( #50886, #41210, #60271, #17087, #31164, #12090 ),
 .UNSPECIFIED., .F., .F.,
 ( 4, 2, 4 ),
 ( 3.476216610979977084E-18, 0.0002291459268755724032, 0.0004582918537511413370 ),
 .UNSPECIFIED. ) ;
#55114 = ORIENTED_EDGE ( 'NONE', *, *, #11767, .F. ) ;
#55115 = ORIENTED_EDGE ( 'NONE', *, *, #35598, .F. ) ;
#55116 = CIRCLE ( 'NONE', #29147, 43.92652462719577500 ) ;
#55117 = CARTESIAN_POINT ( 'NONE',  ( 0.1310142868023736751, -33.82067078731331122, -26.75450212504311764 ) ) ;
#55119 = EDGE_CURVE ( 'NONE', #10982, #26672, #26390, .T. ) ;
#55118 = CARTESIAN_POINT ( 'NONE',  ( 2.643462169533600914, -7.637863311827957524, 47.42536612906414462 ) ) ;
#55120 = CARTESIAN_POINT ( 'NONE',  ( 4.967162193818131399, -35.57684288741960899, -24.30453456948146851 ) ) ;
#55121 = ORIENTED_EDGE ( 'NONE', *, *, #2471, .F. ) ;
#55122 = CARTESIAN_POINT ( 'NONE',  ( -2.569797478183790229, -13.68441171582019855, 5.182550149005058948 ) ) ;
#55123 = CARTESIAN_POINT ( 'NONE',  ( 1.657374760986086271, -34.55241765484513650, 27.33168274104962592 ) ) ;
#55124 = ORIENTED_EDGE ( 'NONE', *, *, #18905, .F. ) ;
#55125 = CARTESIAN_POINT ( 'NONE',  ( -6.016761891674565099, -14.94721834528406923, -11.47373234755518823 ) ) ;
#55126 = ORIENTED_EDGE ( 'NONE', *, *, #20670, .T. ) ;
#55127 = CARTESIAN_POINT ( 'NONE',  ( 0.6000166863083090663, -47.36892948402883263, 12.96179004788911726 ) ) ;
#55128 = DIRECTION ( 'NONE',  ( -0.07836865515943410021, 0.9240274869783785539, 0.3742079063794939153 ) ) ;
#55129 = CARTESIAN_POINT ( 'NONE',  ( 4.975610109902397937, -17.43163075979710541, 45.70106843599904778 ) ) ;
#55130 = VERTEX_POINT ( 'NONE', #33036 ) ;
#55131 = CARTESIAN_POINT ( 'NONE',  ( 0.3676999524040323597, 21.13209774130321250, -38.72189339862975288 ) ) ;
#55132 = CARTESIAN_POINT ( 'NONE',  ( 1.231276596079887264, -39.31472542100218703, 14.54747868495677743 ) ) ;
#55133 = DIRECTION ( 'NONE',  ( 0.000000000000000000, 0.000000000000000000, 1.000000000000000000 ) ) ;
#55134 = CARTESIAN_POINT ( 'NONE',  ( 0.1101816497532063371, -16.62841624476650182, -39.78963561881059263 ) ) ;
#55135 = DIRECTION ( 'NONE',  ( 1.000000000000000000, 1.836970198721027715E-16, -2.218671295934095703E-31 ) ) ;
#55136 = CARTESIAN_POINT ( 'NONE',  ( 0.7954190325252783467, -44.09776758977486111, 19.20649988843040745 ) ) ;
#55137 = CARTESIAN_POINT ( 'NONE',  ( 0.1368894036331284314, 43.18319334776396090, -9.059422620287191918 ) ) ;
#55138 = CARTESIAN_POINT ( 'NONE',  ( 4.975610109902397937, -44.31543648230415755, 20.70245146161774841 ) ) ;
#55139 = CARTESIAN_POINT ( 'NONE',  ( 0.8560838555295223751, -6.899551485032601406, 46.39794201672221163 ) ) ;
#55140 = EDGE_CURVE ( 'NONE', #2711, #21079, #61496, .T. ) ;
#55141 =( BOUNDED_SURFACE ( )  B_SPLINE_SURFACE ( 3, 1, ( 
 ( #3324, #42508 ),
 ( #32169, #46584 ),
 ( #51251, #33105 ),
 ( #14002, #33411 ) ),
 .UNSPECIFIED., .F., .F., .F. ) 
 B_SPLINE_SURFACE_WITH_KNOTS ( ( 4, 4 ),
 ( 2, 2 ),
 ( 0.000000000000000000, 1.000000000000000000 ),
 ( 0.000000000000000000, 1.000000000000000000 ),
 .UNSPECIFIED. ) 
 GEOMETRIC_REPRESENTATION_ITEM ( )  RATIONAL_B_SPLINE_SURFACE ( (
 ( 1.000000000000000000, 1.000000000000000000),
 ( 0.9751682680413298332, 0.9999560080971552356),
 ( 0.9751682680413298332, 0.9999560080971552356),
 ( 1.000000000000000000, 1.000000000000000000) ) ) 
 REPRESENTATION_ITEM ( '' )  SURFACE ( )  );
#55142 = B_SPLINE_CURVE_WITH_KNOTS ( 'NONE', 3,
 ( #20806, #10796, #39015, #1065, #57440, #6352 ),
 .UNSPECIFIED., .F., .F.,
 ( 4, 2, 4 ),
 ( 0.000000000000000000, 0.0002291459268755708853, 0.0004582918537511417706 ),
 .UNSPECIFIED. ) ;
#55143 = EDGE_CURVE ( 'NONE', #23235, #57605, #43055, .T. ) ;
#55144 = CARTESIAN_POINT ( 'NONE',  ( 0.2224561200757615431, 33.74134531362598466, 26.84793396060992876 ) ) ;
#55145 = CARTESIAN_POINT ( 'NONE',  ( -6.079354080745853928, -11.01571246550386540, 15.79389230447975478 ) ) ;
#55146 = ORIENTED_EDGE ( 'NONE', *, *, #23406, .T. ) ;
#55147 = ADVANCED_FACE ( 'NONE', ( #43361 ), #3484, .F. ) ;
#55148 = CARTESIAN_POINT ( 'NONE',  ( 0.9268187852002115479, -2.403807104641838333, -44.02244932204816763 ) ) ;
#55149 = DIRECTION ( 'NONE',  ( -1.000000000000000000, -0.000000000000000000, -0.000000000000000000 ) ) ;
#55150 = CARTESIAN_POINT ( 'NONE',  ( 4.390527457369401532, -41.79567579338402794, 13.53908496180415888 ) ) ;
#55151 = EDGE_CURVE ( 'NONE', #59796, #36643, #14236, .T. ) ;
#55152 = ORIENTED_EDGE ( 'NONE', *, *, #14631, .T. ) ;
#55153 = FACE_OUTER_BOUND ( 'NONE', #42778, .T. ) ;
#55154 = CARTESIAN_POINT ( 'NONE',  ( 4.303969348037246512, -25.89994482339398374, 40.54345935592770189 ) ) ;
#55155 = AXIS2_PLACEMENT_3D ( 'NONE', #33799, #43509, #229 ) ;
#55156 = B_SPLINE_CURVE_WITH_KNOTS ( 'NONE', 3,
 ( #8103, #36630, #27214, #55701 ),
 .UNSPECIFIED., .F., .F.,
 ( 4, 4 ),
 ( 1.734723475976807094E-17, 0.005004741218457440556 ),
 .UNSPECIFIED. ) ;
#55157 = CARTESIAN_POINT ( 'NONE',  ( 0.3622758884714600280, -42.84426538328734324, 4.808133778521152202 ) ) ;
#55158 =( BOUNDED_SURFACE ( )  B_SPLINE_SURFACE ( 3, 1, ( 
 ( #6279, #25414 ),
 ( #354, #38619 ),
 ( #44561, #10096 ),
 ( #57672, #1592 ) ),
 .UNSPECIFIED., .F., .F., .F. ) 
 B_SPLINE_SURFACE_WITH_KNOTS ( ( 4, 4 ),
 ( 2, 2 ),
 ( 0.000000000000000000, 1.000000000000000000 ),
 ( 0.000000000000000000, 1.000000000000000000 ),
 .UNSPECIFIED. ) 
 GEOMETRIC_REPRESENTATION_ITEM ( )  RATIONAL_B_SPLINE_SURFACE ( (
 ( 1.000000000000000000, 1.000000000000000000),
 ( 0.9729067724841187204, 0.9999501103223794596),
 ( 0.9729067724841187204, 0.9999501103223794596),
 ( 1.000000000000000000, 1.000000000000000000) ) ) 
 REPRESENTATION_ITEM ( '' )  SURFACE ( )  );
#55159 = EDGE_LOOP ( 'NONE', ( #21153, #25745, #37345, #33683 ) ) ;
#55161 = CARTESIAN_POINT ( 'NONE',  ( 0.3676999524040323597, 40.09552319080426486, -18.39292264373764851 ) ) ;
#55160 = B_SPLINE_CURVE_WITH_KNOTS ( 'NONE', 3,
 ( #452, #51927, #51301, #8703 ),
 .UNSPECIFIED., .F., .F.,
 ( 4, 4 ),
 ( 0.000000000000000000, 0.004442905043737215703 ),
 .UNSPECIFIED. ) ;
#55162 = VERTEX_POINT ( 'NONE', #9205 ) ;
#55163 = EDGE_CURVE ( 'NONE', #722, #57761, #11419, .T. ) ;
#55164 = CARTESIAN_POINT ( 'NONE',  ( 0.5786265663353153954, -29.72999788434269064, -37.55861529268584320 ) ) ;
#55165 = VERTEX_POINT ( 'NONE', #9823 ) ;
#55166 = VERTEX_POINT ( 'NONE', #28926 ) ;
#55167 = CARTESIAN_POINT ( 'NONE',  ( 3.782542959838389951, -16.11620932553572771, -38.82661008087216459 ) ) ;
#55169 = ORIENTED_EDGE ( 'NONE', *, *, #10057, .T. ) ;
#55168 = EDGE_CURVE ( 'NONE', #20677, #51214, #30818, .T. ) ;
#55170 = CARTESIAN_POINT ( 'NONE',  ( 5.959547316686252039, 0.003562808152905788499, -20.52562247508876681 ) ) ;
#55171 = ORIENTED_EDGE ( 'NONE', *, *, #26324, .F. ) ;
#55172 = CARTESIAN_POINT ( 'NONE',  ( 0.8557997880470690211, -28.43566216844996930, 38.55640757422429488 ) ) ;
#55173 = CARTESIAN_POINT ( 'NONE',  ( 0.5997462898726536595, 40.86908001809362645, -27.22627276398607421 ) ) ;
#55174 = ORIENTED_EDGE ( 'NONE', *, *, #18335, .F. ) ;
#55175 = CARTESIAN_POINT ( 'NONE',  ( 4.000000000000004441, 0.7862748000878170274, -5.565527722372433317 ) ) ;
#55176 = B_SPLINE_CURVE_WITH_KNOTS ( 'NONE', 3,
 ( #49206, #44851, #21021, #40162, #16313, #49826 ),
 .UNSPECIFIED., .F., .F.,
 ( 4, 2, 4 ),
 ( 0.002336974151641576809, 0.003500975885716453226, 0.004664977619791330077 ),
 .UNSPECIFIED. ) ;
#55177 = CARTESIAN_POINT ( 'NONE',  ( 5.901764892641307547, 35.20706988846512075, -34.03606465660227798 ) ) ;
#55178 = CARTESIAN_POINT ( 'NONE',  ( 0.7954196712028469562, 5.415566793624693176, 47.79303691884135219 ) ) ;
#55179 = DIRECTION ( 'NONE',  ( 0.000000000000000000, 0.000000000000000000, -1.000000000000000000 ) ) ;
#55180 = VERTEX_POINT ( 'NONE', #14845 ) ;
#55181 = B_SPLINE_CURVE_WITH_KNOTS ( 'NONE', 3,
 ( #7803, #12535, #45436, #7170, #26930, #2484 ),
 .UNSPECIFIED., .F., .F.,
 ( 4, 2, 4 ),
 ( 1.497895441209388135E-16, 0.0002445252820015227134, 0.0004890505640028956985 ),
 .UNSPECIFIED. ) ;
#55182 = CARTESIAN_POINT ( 'NONE',  ( 0.8557997880470599172, -47.89938907511592703, -0.9121262075951160897 ) ) ;
#55183 = VERTEX_POINT ( 'NONE', #37425 ) ;
#55184 = CARTESIAN_POINT ( 'NONE',  ( 0.9756950546413931669, -42.90834738653779823, 0.09673755062781558278 ) ) ;
#55185 = CARTESIAN_POINT ( 'NONE',  ( 0.9757892942422821125, 26.16173342773539900, 34.01031843153901946 ) ) ;
#55186 = ADVANCED_FACE ( 'NONE', ( #10134 ), #11832, .F. ) ;
#55187 = CARTESIAN_POINT ( 'NONE',  ( 0.1073791018717578927, -41.77800844988522755, 10.69234304549982895 ) ) ;
#55188 = ORIENTED_EDGE ( 'NONE', *, *, #26800, .T. ) ;
#55189 = CARTESIAN_POINT ( 'NONE',  ( 4.956653778116966613, 0.000000000000000000, 0.000000000000000000 ) ) ;
#55190 = CARTESIAN_POINT ( 'NONE',  ( -6.016489644550736315, -18.19999694163067616, 4.881234076340310146 ) ) ;
#55191 = CARTESIAN_POINT ( 'NONE',  ( 0.5782707292762423457, 46.89575936232450459, -0.7239527184646502578 ) ) ;
#55192 = CARTESIAN_POINT ( 'NONE',  ( 0.3676999524040366896, -6.224421213753956295, 43.67158302462379282 ) ) ;
#55193 = ORIENTED_EDGE ( 'NONE', *, *, #37410, .T. ) ;
#55194 = ORIENTED_EDGE ( 'NONE', *, *, #15808, .F. ) ;
#55195 = CARTESIAN_POINT ( 'NONE',  ( 0.8551540677456834771, 46.51172240253119838, 11.51835730326496510 ) ) ;
#55196 = CARTESIAN_POINT ( 'NONE',  ( 0.1098349054025746369, 34.08267426123924082, 26.42143025180000748 ) ) ;
#55197 = CARTESIAN_POINT ( 'NONE',  ( 0.8744876279028306332, -42.33402326122651971, 24.86323641237049387 ) ) ;
#55198 = CARTESIAN_POINT ( 'NONE',  ( 0.6031356219577718170, 6.192730535896147970, -47.70727206974379442 ) ) ;
#55199 = VECTOR ( 'NONE', #44025, 1000.000000000000114 ) ;
#55200 = CARTESIAN_POINT ( 'NONE',  ( 0.5807400328401574052, -44.04145271122551009, -18.83234461715229102 ) ) ;
#55201 = B_SPLINE_CURVE_WITH_KNOTS ( 'NONE', 3,
 ( #26107, #46165, #45545, #49918, #36456, #50526 ),
 .UNSPECIFIED., .F., .F.,
 ( 4, 2, 4 ),
 ( 1.520334456564901176E-16, 0.0002445252820015209787, 0.0004890505640028898439 ),
 .UNSPECIFIED. ) ;
#55202 = CARTESIAN_POINT ( 'NONE',  ( 1.231276596079881047, -2.246340108600348717, 41.85965512441018888 ) ) ;
#55203 = CARTESIAN_POINT ( 'NONE',  ( 4.549368137175248350, 32.13400537129925283, -28.46244473166639111 ) ) ;
#55204 = B_SPLINE_CURVE_WITH_KNOTS ( 'NONE', 3,
 ( #59920, #31423, #16713, #7920, #2901, #45243, #22032, #59295, #46160, #11712, #44932, #54270, #36451, #41462, #55519, #41155 ),
 .UNSPECIFIED., .F., .F.,
 ( 4, 3, 3, 3, 3, 4 ),
 ( 1.962735358247463844E-17, 0.0002618515315864471810, 0.0003927756766342011354, 0.0005236998216950600584, 0.0007855159896329930429, 0.001047349442285932641 ),
 .UNSPECIFIED. ) ;
#55205 = FACE_OUTER_BOUND ( 'NONE', #42497, .T. ) ;
#55206 = CARTESIAN_POINT ( 'NONE',  ( 3.376099380956838925, -13.39845304004337123, 0.4357060543757622639 ) ) ;
#55207 = CARTESIAN_POINT ( 'NONE',  ( 0.8557997880470599172, -47.60865952217002928, 5.347802024197076065 ) ) ;
#55208 = LINE ( 'NONE', #50825, #24062 ) ;
#55209 = CARTESIAN_POINT ( 'NONE',  ( 0.9268187852002115479, 41.51895754277288120, -14.83005385931043918 ) ) ;
#55210 = CARTESIAN_POINT ( 'NONE',  ( 2.299652685299201416, 9.651193673476788248, 48.07427779525340839 ) ) ;
#55211 = DIRECTION ( 'NONE',  ( -1.000000000000000000, -0.000000000000000000, -0.000000000000000000 ) ) ;
#55212 = CARTESIAN_POINT ( 'NONE',  ( 0.6028618097248862329, -6.452328974163289210, -47.67286800277441472 ) ) ;
#55213 = CARTESIAN_POINT ( 'NONE',  ( 0.1101816497532063094, -0.1358190954552562779, -43.12424935764384060 ) ) ;
#55214 = EDGE_CURVE ( 'NONE', #26819, #51265, #5393, .T. ) ;
#55215 = CARTESIAN_POINT ( 'NONE',  ( 0.6021448801613057400, 16.71458247052639123, 46.17536000360927062 ) ) ;
#55216 = CARTESIAN_POINT ( 'NONE',  ( 0.6031356755773454870, 46.46821530722340299, -12.45114731045982026 ) ) ;
#55218 = EDGE_LOOP ( 'NONE', ( #5842, #35111, #39497, #8718 ) ) ;
#55217 = CARTESIAN_POINT ( 'NONE',  ( 0.7764139734771229318, 23.31927515082854541, -40.69707455514238603 ) ) ;
#55219 = ORIENTED_EDGE ( 'NONE', *, *, #30534, .F. ) ;
#55220 = FACE_BOUND ( 'NONE', #52312, .T. ) ;
#55221 = CARTESIAN_POINT ( 'NONE',  ( 2.359973842542475886, 2.722770999149179527, -43.93998648974180554 ) ) ;
#55222 = CARTESIAN_POINT ( 'NONE',  ( 0.7246131072078578761, 34.58859703353080306, -33.42811616637882821 ) ) ;
#55223 = ADVANCED_FACE ( 'NONE', ( #40219 ), #18224, .F. ) ;
#55224 = VERTEX_POINT ( 'NONE', #35189 ) ;
#55225 = ORIENTED_EDGE ( 'NONE', *, *, #34032, .T. ) ;
#55226 = LINE ( 'NONE', #54600, #24286 ) ;
#55227 = CARTESIAN_POINT ( 'NONE',  ( 0.3676999524040323597, 21.13209774130321250, -38.72189339862975288 ) ) ;
#55228 = ORIENTED_EDGE ( 'NONE', *, *, #40548, .T. ) ;
#55229 = ORIENTED_EDGE ( 'NONE', *, *, #44717, .T. ) ;
#55230 = CARTESIAN_POINT ( 'NONE',  ( 1.157643937452369487, 19.41637196408613875, -37.14844242154714493 ) ) ;
#55231 = CARTESIAN_POINT ( 'NONE',  ( -6.016104459813374383, 13.32794178585016098, -13.32039631884670250 ) ) ;
#55232 = CARTESIAN_POINT ( 'NONE',  ( 0.5797568665920714848, 17.44034444229498604, 43.53228335771030544 ) ) ;
#55233 = ORIENTED_EDGE ( 'NONE', *, *, #770, .T. ) ;
#55234 = ADVANCED_FACE ( 'NONE', ( #20161 ), #16316, .F. ) ;
#55235 = CARTESIAN_POINT ( 'NONE',  ( 5.860006189529246790, 48.12869875779309581, 3.171667470662679733 ) ) ;
#55236 = B_SPLINE_CURVE_WITH_KNOTS ( 'NONE', 3,
 ( #16247, #44474, #39771, #19716 ),
 .UNSPECIFIED., .F., .F.,
 ( 4, 4 ),
 ( 0.000000000000000000, 0.004445488388166989914 ),
 .UNSPECIFIED. ) ;
#55237 = CIRCLE ( 'NONE', #10281, 5.000000000000000888 ) ;
#55238 = AXIS2_PLACEMENT_3D ( 'NONE', #47340, #52949, #33259 ) ;
#55239 = CARTESIAN_POINT ( 'NONE',  ( 0.1081432562775997974, 21.19449538864506266, 37.55692207416033312 ) ) ;
#55240 = ORIENTED_EDGE ( 'NONE', *, *, #7224, .F. ) ;
#55241 = ORIENTED_EDGE ( 'NONE', *, *, #4969, .T. ) ;
#55242 = CARTESIAN_POINT ( 'NONE',  ( 0.8560838555295158248, 9.983184696770717181, 45.83349056521764453 ) ) ;
#55243 = VERTEX_POINT ( 'NONE', #6623 ) ;
#55244 = DIRECTION ( 'NONE',  ( 0.000000000000000000, 0.000000000000000000, -1.000000000000000000 ) ) ;
#55245 = CARTESIAN_POINT ( 'NONE',  ( 0.6000166863083090663, -25.01014854877412219, -42.26483113981062445 ) ) ;
#55246 = CARTESIAN_POINT ( 'NONE',  ( 4.549368137175248350, 28.14399996863497577, -32.41327393324110773 ) ) ;
#55247 = CARTESIAN_POINT ( 'NONE',  ( -6.078726893082806448, 12.00325722817128771, 15.05708661006749338 ) ) ;
#55248 = CARTESIAN_POINT ( 'NONE',  ( 0.8744876279028263033, -8.712669995482247742, 48.31603700562906312 ) ) ;
#55249 = EDGE_LOOP ( 'NONE', ( #3322, #43843, #37619, #46528 ) ) ;
#55250 = CARTESIAN_POINT ( 'NONE',  ( 0.000000000000000000, -1.178949249685214307, 2.042000000000001592 ) ) ;
#55251 = DIRECTION ( 'NONE',  ( 0.09722883295013592941, 0.9936727386027172093, 0.05622315004453748433 ) ) ;
#55252 = B_SPLINE_CURVE_WITH_KNOTS ( 'NONE', 3,
 ( #14128, #52614, #9711, #34155 ),
 .UNSPECIFIED., .F., .F.,
 ( 4, 4 ),
 ( 0.000000000000000000, 0.004445488388166995118 ),
 .UNSPECIFIED. ) ;
#55253 = CARTESIAN_POINT ( 'NONE',  ( 0.6254311100348652896, 29.82834996731695298, -37.74260849418467956 ) ) ;
#55254 =( BOUNDED_SURFACE ( )  B_SPLINE_SURFACE ( 3, 1, ( 
 ( #6603, #43651 ),
 ( #24832, #1007 ),
 ( #16355, #35481 ),
 ( #20141, #54537 ) ),
 .UNSPECIFIED., .F., .F., .F. ) 
 B_SPLINE_SURFACE_WITH_KNOTS ( ( 4, 4 ),
 ( 2, 2 ),
 ( 0.000000000000000000, 1.000000000000000000 ),
 ( 0.000000000000000000, 1.000000000000000000 ),
 .UNSPECIFIED. ) 
 GEOMETRIC_REPRESENTATION_ITEM ( )  RATIONAL_B_SPLINE_SURFACE ( (
 ( 1.000000000000000000, 1.000000000000000000),
 ( 0.9751682680413298332, 0.9999560080971552356),
 ( 0.9751682680413298332, 0.9999560080971552356),
 ( 1.000000000000000000, 1.000000000000000000) ) ) 
 REPRESENTATION_ITEM ( '' )  SURFACE ( )  );
#55255 = CARTESIAN_POINT ( 'NONE',  ( 0.6001305935487315502, 47.62765676940944104, -6.798494447611730607 ) ) ;
#55256 = EDGE_CURVE ( 'NONE', #31776, #36339, #42839, .T. ) ;
#55257 = ORIENTED_EDGE ( 'NONE', *, *, #35034, .F. ) ;
#55258 = CARTESIAN_POINT ( 'NONE',  ( 0.1103310638050662290, 42.76619676553136173, -5.547176740493094727 ) ) ;
#55259 = CARTESIAN_POINT ( 'NONE',  ( 0.3622758884714730732, -4.808133778522197588, 42.84426538328723666 ) ) ;
#55260 = CARTESIAN_POINT ( 'NONE',  ( 4.956653778116992370, 31.29546495791903027, -36.51451553856384180 ) ) ;
#55261 = SURFACE_SIDE_STYLE ('',( #11448 ) ) ;
#55262 = ORIENTED_EDGE ( 'NONE', *, *, #58313, .T. ) ;
#55263 = CARTESIAN_POINT ( 'NONE',  ( 4.303969348037258058, -25.89994482339341531, -40.54345935592806427 ) ) ;
#55264 = CARTESIAN_POINT ( 'NONE',  ( 4.956445790443988031, 0.000000000000000000, 0.000000000000000000 ) ) ;
#55265 = FACE_OUTER_BOUND ( 'NONE', #46689, .T. ) ;
#55266 = PRODUCT_DEFINITION_SHAPE ( 'NONE', 'NONE',  #61981 ) ;
#55267 = B_SPLINE_CURVE_WITH_KNOTS ( 'NONE', 3,
 ( #10358, #58556, #48558, #5924, #30679, #1545, #21296, #40132, #44209, #10983, #45128, #49797, #6855, #30368, #20682, #6228, #53550, #40426, #58872 ),
 .UNSPECIFIED., .F., .F.,
 ( 4, 3, 3, 3, 3, 3, 4 ),
 ( 1.250973872328959318E-17, 0.0002732106629380557099, 0.0004098138914053751068, 0.0005464171197651450634, 0.0006830203481512486102, 0.0008196235766963579951, 0.001011968216111138342 ),
 .UNSPECIFIED. ) ;
#55268 = CARTESIAN_POINT ( 'NONE',  ( 0.6846871229502899947, 46.04462816497506594, -13.23224427737781284 ) ) ;
#55269 = DIRECTION ( 'NONE',  ( 0.1011922191286468153, -0.2953728085273201187, -0.9500079151093968610 ) ) ;
#55270 = CARTESIAN_POINT ( 'NONE',  ( 0.8744876279028306332, 21.91587810745098963, -43.93226988397984911 ) ) ;
#55271 = CARTESIAN_POINT ( 'NONE',  ( 0.9757787079277434605, -5.561523338226871616, -42.54650880470570939 ) ) ;
#55272 = DIRECTION ( 'NONE',  ( -1.000000000000000000, -1.836909530733554547E-16, -1.836909530733573529E-16 ) ) ;
#55273 = CARTESIAN_POINT ( 'NONE',  ( 0.5832367798473383491, 37.83194459509911667, 29.37285281143854831 ) ) ;
#55274 = CARTESIAN_POINT ( 'NONE',  ( 2.299746137290200831, -12.71146744108550131, 47.35715292519559227 ) ) ;
#55275 = EDGE_LOOP ( 'NONE', ( #19286, #9235, #57458, #16076 ) ) ;
#55276 = CARTESIAN_POINT ( 'NONE',  ( -16.91961043310876889, -12.36682299961459108, -1.821422909846774907 ) ) ;
#55277 = CARTESIAN_POINT ( 'NONE',  ( 4.962356264823603702, 37.36413190407388640, -19.36897635181878030 ) ) ;
#55278 = DIRECTION ( 'NONE',  ( -0.000000000000000000, -1.000000000000000000, -0.000000000000000000 ) ) ;
#55279 = CARTESIAN_POINT ( 'NONE',  ( 0.1139756605157203478, 44.00639638324004466, -3.223708587354096267 ) ) ;
#55280 = B_SPLINE_CURVE_WITH_KNOTS ( 'NONE', 3,
 ( #18046, #22733, #41865, #60935, #57144, #37163, #33692, #32446, #52768, #9872, #18660, #9550, #14277, #28660, #46552, #18357 ),
 .UNSPECIFIED., .F., .F.,
 ( 4, 3, 3, 3, 3, 4 ),
 ( 9.813676791237319219E-18, 0.0002732102107931875601, 0.0004098135523333767635, 0.0005464168938824943717, 0.0008195847345945264217, 0.001092771384553102012 ),
 .UNSPECIFIED. ) ;
#55281 = CARTESIAN_POINT ( 'NONE',  ( 0.5807400328401637335, -46.40483864045136642, -11.87003418057291704 ) ) ;
#55282 = CARTESIAN_POINT ( 'NONE',  ( 0.9783242366443549720, -31.26083830869256275, 27.91226394336910488 ) ) ;
#55283 = CONTEXT_DEPENDENT_SHAPE_REPRESENTATION ( #44429, #7238 ) ;
#55284 = CARTESIAN_POINT ( 'NONE',  ( 0.6031357023905875581, -44.46217339385183465, 18.36962560204140615 ) ) ;
#55285 = CARTESIAN_POINT ( 'NONE',  ( 4.962356264823608143, 0.000000000000000000, 0.000000000000000000 ) ) ;
#55286 = ADVANCED_FACE ( 'NONE', ( #49259 ), #29115, .F. ) ;
#55287 = CARTESIAN_POINT ( 'NONE',  ( -6.078726893082806448, 16.77644806189623239, -9.452239506869167585 ) ) ;
#55289 = VERTEX_POINT ( 'NONE', #10446 ) ;
#55288 = CARTESIAN_POINT ( 'NONE',  ( 2.099999999999999645, 0.000000000000000000, -5.599999999999999645 ) ) ;
#55290 = ORIENTED_EDGE ( 'NONE', *, *, #11399, .F. ) ;
#55291 = CARTESIAN_POINT ( 'NONE',  ( 0.3622758884714730732, 6.444611261694017657, 42.62881903538212924 ) ) ;
#55292 = CARTESIAN_POINT ( 'NONE',  ( 1.834102595619085729, -19.01334881635286678, -39.73273602013052397 ) ) ;
#55293 = CARTESIAN_POINT ( 'NONE',  ( 3.238018933889920792, -12.07617426668434568, 5.794265048159582321 ) ) ;
#55294 = CARTESIAN_POINT ( 'NONE',  ( 3.678834586032788234, 38.46440325416317307, -30.31669592698840532 ) ) ;
#55295 = EDGE_CURVE ( 'NONE', #19678, #53979, #9188, .T. ) ;
#55296 = B_SPLINE_CURVE_WITH_KNOTS ( 'NONE', 3,
 ( #56254, #27449, #51866, #32470, #8640, #42201 ),
 .UNSPECIFIED., .F., .F.,
 ( 4, 2, 4 ),
 ( 1.553784678811103104E-17, 0.0002293755540694291772, 0.0004587511081388428503 ),
 .UNSPECIFIED. ) ;
#55297 = EDGE_LOOP ( 'NONE', ( #56465, #19472, #22751, #42420 ) ) ;
#55298 = DIRECTION ( 'NONE',  ( -1.000000000000000000, -0.000000000000000000, -0.000000000000000000 ) ) ;
#55299 = FACE_OUTER_BOUND ( 'NONE', #33731, .T. ) ;
#55300 = CARTESIAN_POINT ( 'NONE',  ( 0.1103878639767399555, 41.64243544356628490, -11.20830530106149325 ) ) ;
#55301 = EDGE_CURVE ( 'NONE', #49888, #45339, #27832, .T. ) ;
#55302 = VERTEX_POINT ( 'NONE', #59895 ) ;
#55303 = VERTEX_POINT ( 'NONE', #41137 ) ;
#55304 = AXIS2_PLACEMENT_3D ( 'NONE', #22347, #50536, #26738 ) ;
#55305 = PLANE ( 'NONE',  #58307 ) ;
#55306 = CARTESIAN_POINT ( 'NONE',  ( 0.1102144999581333162, -39.79340763430497674, -16.61938362665535962 ) ) ;
#55307 = CARTESIAN_POINT ( 'NONE',  ( 2.788021980277358036, 6.069845295522647588E-12, -46.99417130740492610 ) ) ;
#55308 = ORIENTED_EDGE ( 'NONE', *, *, #35446, .F. ) ;
#55309 = ADVANCED_FACE ( 'NONE', ( #50194 ), #12933, .F. ) ;
#55310 = CARTESIAN_POINT ( 'NONE',  ( 0.8744876279028306332, 27.35388303025845147, -40.76904626731451486 ) ) ;
#55311 = DIRECTION ( 'NONE',  ( -1.000000000000000000, -0.000000000000000000, -0.000000000000000000 ) ) ;
#55312 = ORIENTED_EDGE ( 'NONE', *, *, #54635, .T. ) ;
#55313 = CARTESIAN_POINT ( 'NONE',  ( 0.3676999524040366896, 33.04872056100262512, -29.21870381457057775 ) ) ;
#55314 = DIRECTION ( 'NONE',  ( 0.000000000000000000, -0.7071067811865449082, -0.7071067811865500152 ) ) ;
#55315 = VERTEX_POINT ( 'NONE', #8196 ) ;
#55316 = B_SPLINE_CURVE_WITH_KNOTS ( 'NONE', 3,
 ( #26878, #36602, #8074, #22793 ),
 .UNSPECIFIED., .F., .F.,
 ( 4, 4 ),
 ( 1.084202172485504434E-19, 0.004446298630425056346 ),
 .UNSPECIFIED. ) ;
#55317 = CARTESIAN_POINT ( 'NONE',  ( 4.322998006666179727, -47.80838462754062590, -4.155494336618541062 ) ) ;
#55318 = FACE_OUTER_BOUND ( 'NONE', #29398, .T. ) ;
#55319 = ORIENTED_EDGE ( 'NONE', *, *, #9987, .F. ) ;
#55320 = CARTESIAN_POINT ( 'NONE',  ( 0.7242486021783859362, -20.62188805686228577, 44.56174587405900667 ) ) ;
#55321 = CARTESIAN_POINT ( 'NONE',  ( 2.618530812446115519, 21.34567399517413477, -41.88184560033076309 ) ) ;
#55322 = CARTESIAN_POINT ( 'NONE',  ( 2.528190830796658517, 5.404281357458566859, -41.62989165446426654 ) ) ;
#55323 = CIRCLE ( 'NONE', #42403, 43.08621763946400307 ) ;
#55324 = ORIENTED_EDGE ( 'NONE', *, *, #14589, .F. ) ;
#55325 = LINE ( 'NONE', #8037, #36776 ) ;
#55326 = CARTESIAN_POINT ( 'NONE',  ( 0.1157506346131639274, 39.71414577812362268, -19.22829386390743878 ) ) ;
#55327 = ORIENTED_EDGE ( 'NONE', *, *, #38018, .F. ) ;
#55328 = DIRECTION ( 'NONE',  ( 0.000000000000000000, 0.000000000000000000, 1.000000000000000000 ) ) ;
#55329 =( BOUNDED_SURFACE ( )  B_SPLINE_SURFACE ( 3, 1, ( 
 ( #55437, #20470 ),
 ( #45463, #55744 ),
 ( #53959, #2814 ),
 ( #26633, #45768 ) ),
 .UNSPECIFIED., .F., .F., .F. ) 
 B_SPLINE_SURFACE_WITH_KNOTS ( ( 4, 4 ),
 ( 2, 2 ),
 ( 0.000000000000000000, 1.000000000000000000 ),
 ( 0.000000000000000000, 1.000000000000000000 ),
 .UNSPECIFIED. ) 
 GEOMETRIC_REPRESENTATION_ITEM ( )  RATIONAL_B_SPLINE_SURFACE ( (
 ( 1.000000000000000000, 1.000000000000000000),
 ( 0.9953390228620291325, 0.8624445117761032620),
 ( 0.9953390228620291325, 0.8624445117761032620),
 ( 1.000000000000000000, 1.000000000000000000) ) ) 
 REPRESENTATION_ITEM ( '' )  SURFACE ( )  );
#55330 = ORIENTED_EDGE ( 'NONE', *, *, #47183, .F. ) ;
#55331 = DIRECTION ( 'NONE',  ( -1.000000000000000000, -0.000000000000000000, -0.000000000000000000 ) ) ;
#55332 = VERTEX_POINT ( 'NONE', #17009 ) ;
#55333 = CARTESIAN_POINT ( 'NONE',  ( 2.526552050251863246, -41.18423939305557013, -12.29062829844021110 ) ) ;
#55334 = CARTESIAN_POINT ( 'NONE',  ( 0.000000000000000000, 0.000000000000000000, -1.199999999999999956 ) ) ;
#55335 = LINE ( 'NONE', #2094, #10243 ) ;
#55336 = ORIENTED_EDGE ( 'NONE', *, *, #49877, .F. ) ;
#55337 = FACE_OUTER_BOUND ( 'NONE', #70, .T. ) ;
#55338 = EDGE_CURVE ( 'NONE', #55726, #33072, #20575, .T. ) ;
#55339 = CARTESIAN_POINT ( 'NONE',  ( 3.407937589446174087, 13.10584870154466586, 3.987184287467832711 ) ) ;
#55340 = CARTESIAN_POINT ( 'NONE',  ( -6.077587904424778920, 0.6233693561571294062, -19.24597183931574662 ) ) ;
#55341 = ORIENTED_EDGE ( 'NONE', *, *, #21428, .F. ) ;
#55342 = AXIS2_PLACEMENT_3D ( 'NONE', #54156, #5607, #20679 ) ;
#55343 = EDGE_CURVE ( 'NONE', #33072, #27868, #41444, .T. ) ;
#55344 = ORIENTED_EDGE ( 'NONE', *, *, #41820, .F. ) ;
#55345 = CARTESIAN_POINT ( 'NONE',  ( 0.5988103564986357874, -37.79415694022880245, 29.76496605343782420 ) ) ;
#55346 = CARTESIAN_POINT ( 'NONE',  ( 0.8751705887134423323, -24.81530984069236823, 41.19904111682465242 ) ) ;
#55347 = CARTESIAN_POINT ( 'NONE',  ( 0.5997462898726536595, 33.39998138387845472, 35.99990102348730403 ) ) ;
#55348 = CARTESIAN_POINT ( 'NONE',  ( 0.1098349054025746646, 30.34240357440793190, 30.64407294528958658 ) ) ;
#55349 = CARTESIAN_POINT ( 'NONE',  ( 0.1073791018717483448, 16.95003405440257893, 39.65380858626220828 ) ) ;
#55350 = VERTEX_POINT ( 'NONE', #41750 ) ;
#55351 = EDGE_CURVE ( 'NONE', #17692, #10204, #7895, .T. ) ;
#55352 = CARTESIAN_POINT ( 'NONE',  ( 0.1097557419366048670, 37.23482781437645173, -21.75515245866085934 ) ) ;
#55353 = DIRECTION ( 'NONE',  ( 1.000000000000000000, -0.000000000000000000, -0.000000000000000000 ) ) ;
#55354 = ORIENTED_EDGE ( 'NONE', *, *, #2465, .F. ) ;
#55355 = CARTESIAN_POINT ( 'NONE',  ( -6.077587904424778920, 16.77513308702627981, 9.454677747363296803 ) ) ;
#55356 = CARTESIAN_POINT ( 'NONE',  ( 0.9787464366903561030, -27.19233698969872037, 31.88903889942633896 ) ) ;
#55357 = CARTESIAN_POINT ( 'NONE',  ( 0.3622758884714600280, 40.13994584881781691, -15.73321244754812298 ) ) ;
#55358 = LINE ( 'NONE', #21872, #40065 ) ;
#55359 = B_SPLINE_CURVE_WITH_KNOTS ( 'NONE', 3,
 ( #34897, #26397, #44923, #6638, #30166, #2266, #49276, #54261, #21704, #58657, #30466, #45234, #6329, #11383, #53961, #49582, #44610, #59911, #21396, #36137, #11086, #16089, #2582, #25785, #35824 ),
 .UNSPECIFIED., .F., .F.,
 ( 4, 3, 3, 3, 3, 3, 3, 3, 4 ),
 ( 4.670885906470169154E-18, 0.0005656085177311403990, 0.001131215744874500707, 0.001696821861372765266, 0.002262427090022498151, 0.002828031679238745492, 0.003393635864401603995, 0.003977030878808131623, 0.004561030005651158133 ),
 .UNSPECIFIED. ) ;
#55360 = CARTESIAN_POINT ( 'NONE',  ( 0.5807400328401574052, -5.711437504335652449, -47.55718917606849061 ) ) ;
#55361 = CARTESIAN_POINT ( 'NONE',  ( 4.967162193818131399, -19.45289607368795259, -38.44485641567092671 ) ) ;
#55362 = DIRECTION ( 'NONE',  ( -0.07500201931887527651, -0.9798016564749993940, -0.1853737065145389662 ) ) ;
#55363 =( NAMED_UNIT ( * ) SI_UNIT ( $, .STERADIAN. ) SOLID_ANGLE_UNIT ( ) );
#55364 = CARTESIAN_POINT ( 'NONE',  ( 0.6030672727741701600, 38.11303703924428277, 29.35514790473164126 ) ) ;
#55365 = CARTESIAN_POINT ( 'NONE',  ( 5.958863334805807099, 14.51296551801783075, 14.51469124124484900 ) ) ;
#55366 = CARTESIAN_POINT ( 'NONE',  ( 0.6039202388192952409, -35.15506827346133889, -34.28826165814277260 ) ) ;
#55367 = EDGE_CURVE ( 'NONE', #52228, #17050, #17615, .T. ) ;
#55368 = CARTESIAN_POINT ( 'NONE',  ( 3.270143674763207553, -5.490410281242870560, 12.53844339339232938 ) ) ;
#55369 = CARTESIAN_POINT ( 'NONE',  ( 0.8557997880470606944, -33.22501220301877112, -34.51495345639583689 ) ) ;
#55370 = B_SPLINE_CURVE_WITH_KNOTS ( 'NONE', 3,
 ( #30640, #41020, #41313, #7439, #45699, #54749 ),
 .UNSPECIFIED., .F., .F.,
 ( 4, 2, 4 ),
 ( 2.335442953235084577E-18, 0.0002447193893791698707, 0.0004894387787583364888 ),
 .UNSPECIFIED. ) ;
#55371 = CARTESIAN_POINT ( 'NONE',  ( 1.227938101723756947, -34.55893248994489397, -25.45152231597092651 ) ) ;
#55372 = EDGE_CURVE ( 'NONE', #9955, #10882, #22621, .T. ) ;
#55373 = CARTESIAN_POINT ( 'NONE',  ( 4.956445790444004018, -43.56224489968113289, 17.88487823385560205 ) ) ;
#55374 = CARTESIAN_POINT ( 'NONE',  ( 3.221118495291109163, 16.94972950403165157, 40.58901439308313286 ) ) ;
#55375 = CIRCLE ( 'NONE', #6296, 43.08621763946400307 ) ;
#55376 = DIRECTION ( 'NONE',  ( 0.000000000000000000, 0.000000000000000000, 1.000000000000000000 ) ) ;
#55377 = CARTESIAN_POINT ( 'NONE',  ( 5.960721111146673579, 10.25731071096582880, -17.77882586010657207 ) ) ;
#55378 = EDGE_CURVE ( 'NONE', #28691, #31261, #15861, .T. ) ;
#55379 = B_SPLINE_CURVE_WITH_KNOTS ( 'NONE', 3,
 ( #38544, #10331, #38240, #19737 ),
 .UNSPECIFIED., .F., .F.,
 ( 4, 4 ),
 ( 3.469446951953614189E-18, 0.004050076154993001616 ),
 .UNSPECIFIED. ) ;
#55380 = ORIENTED_EDGE ( 'NONE', *, *, #38478, .F. ) ;
#55381 = CARTESIAN_POINT ( 'NONE',  ( 1.227938101723756947, -29.74462687941247552, 30.94118573761302926 ) ) ;
#55382 = CARTESIAN_POINT ( 'NONE',  ( 3.894904216938898323, -33.08280459236107163, -28.94222473791284500 ) ) ;
#55383 = CARTESIAN_POINT ( 'NONE',  ( 0.9757787079277439046, -26.08967489699740838, -34.06559579809994176 ) ) ;
#55384 = CARTESIAN_POINT ( 'NONE',  ( -6.072942160501519027, -12.95676005301717382, 14.24522836663417280 ) ) ;
#55385 = EDGE_LOOP ( 'NONE', ( #1226, #60544, #484, #30603 ) ) ;
#55386 = CARTESIAN_POINT ( 'NONE',  ( 1.157644175074336479, -0.5751541904189192422, -41.91266482981518493 ) ) ;
#55387 = CARTESIAN_POINT ( 'NONE',  ( 5.960221823109900008, 14.50993159119810905, -14.51763960716763258 ) ) ;
#55388 = EDGE_CURVE ( 'NONE', #54854, #52998, #25573, .T. ) ;
#55389 = B_SPLINE_CURVE_WITH_KNOTS ( 'NONE', 3,
 ( #9793, #57999, #53305, #18908, #5674, #57077 ),
 .UNSPECIFIED., .F., .F.,
 ( 4, 2, 4 ),
 ( 0.000000000000000000, 0.0002291459268755698824, 0.0004582918537511397649 ),
 .UNSPECIFIED. ) ;
#55390 = FACE_OUTER_BOUND ( 'NONE', #39952, .T. ) ;
#55391 = ORIENTED_EDGE ( 'NONE', *, *, #16014, .F. ) ;
#55392 = B_SPLINE_CURVE_WITH_KNOTS ( 'NONE', 3,
 ( #54670, #1431, #12114, #49994, #10870, #7052 ),
 .UNSPECIFIED., .F., .F.,
 ( 4, 2, 4 ),
 ( 1.823789517034659149E-17, 0.0002293319059085093578, 0.0004586638118170004467 ),
 .UNSPECIFIED. ) ;
#55393 = CARTESIAN_POINT ( 'NONE',  ( 1.827119703190780653, 41.88501940447980587, 9.946884032291251287 ) ) ;
#55394 = ORIENTED_EDGE ( 'NONE', *, *, #38228, .F. ) ;
#55395 = CARTESIAN_POINT ( 'NONE',  ( 2.643462169533613793, 48.01657676222237114, -1.382267876917960381 ) ) ;
#55396 = CARTESIAN_POINT ( 'NONE',  ( 5.910764540655177868, 3.329973395294289151, 19.83462920388972961 ) ) ;
#55397 = EDGE_LOOP ( 'NONE', ( #45965, #27369, #52113, #29962 ) ) ;
#55398 = CARTESIAN_POINT ( 'NONE',  ( 0.6001305935487422083, 18.89378601236001742, 44.24520387813834787 ) ) ;
#55399 = EDGE_LOOP ( 'NONE', ( #39390, #29586, #1599, #6940 ) ) ;
#55400 = CARTESIAN_POINT ( 'NONE',  ( 10.00000000000002132, -80.00000000000001421, 2.649999999999992806 ) ) ;
#55401 = CARTESIAN_POINT ( 'NONE',  ( 0.1095718737110178420, -26.04820588677170079, -34.36877422440991126 ) ) ;
#55402 = VERTEX_POINT ( 'NONE', #32334 ) ;
#55403 = CARTESIAN_POINT ( 'NONE',  ( 0.8760168074886960365, -24.81951362746106682, 41.20610493656867135 ) ) ;
#55404 = ORIENTED_EDGE ( 'NONE', *, *, #57022, .F. ) ;
#55405 = CARTESIAN_POINT ( 'NONE',  ( 0.9754292580325132356, 28.71299566771950751, 30.52689546432007717 ) ) ;
#55406 = ORIENTED_EDGE ( 'NONE', *, *, #4601, .T. ) ;
#55407 = VERTEX_POINT ( 'NONE', #26386 ) ;
#55408 = CARTESIAN_POINT ( 'NONE',  ( 4.291220156522060236, 38.26855966511092078, 27.47555892904714625 ) ) ;
#55409 = CARTESIAN_POINT ( 'NONE',  ( 0.8753041380234465318, 41.63161868429074985, -26.03740873433439162 ) ) ;
#55410 = CARTESIAN_POINT ( 'NONE',  ( 0.8751705887134553219, -5.393078191593054349, 47.79200036674269825 ) ) ;
#55411 = DIRECTION ( 'NONE',  ( -1.000000000000000000, -0.000000000000000000, -0.000000000000000000 ) ) ;
#55412 = CARTESIAN_POINT ( 'NONE',  ( 0.6028618097248863439, 44.51207924874651667, 18.24855319618761840 ) ) ;
#55413 = VERTEX_POINT ( 'NONE', #36126 ) ;
#55414 = CARTESIAN_POINT ( 'NONE',  ( 0.9736507210033074067, 10.66979144439368454, 41.56063510425031637 ) ) ;
#55415 = EDGE_CURVE ( 'NONE', #9472, #19529, #60567, .T. ) ;
#55416 = DIRECTION ( 'NONE',  ( 0.09722883295013597105, -0.9253344465965372967, 0.3664733496245457522 ) ) ;
#55417 = CARTESIAN_POINT ( 'NONE',  ( 0.5806925824938494740, -1.020860314013172454, 46.88475452172951918 ) ) ;
#55418 = VERTEX_POINT ( 'NONE', #8501 ) ;
#55419 = CIRCLE ( 'NONE', #5369, 2.055000000000000160 ) ;
#55420 = ADVANCED_FACE ( 'NONE', ( #31714 ), #45580, .T. ) ;
#55421 = ORIENTED_EDGE ( 'NONE', *, *, #11831, .F. ) ;
#55422 = CARTESIAN_POINT ( 'NONE',  ( 0.9757787079277437936, 34.06559579810004834, -26.08967489699726983 ) ) ;
#55423 = CARTESIAN_POINT ( 'NONE',  ( 3.407937589446174087, 3.987184287467969934, -13.10584870154462500 ) ) ;
#55424 = CARTESIAN_POINT ( 'NONE',  ( 1.092182651088184908, 40.21120180690577683, -11.82456906980473654 ) ) ;
#55425 = ORIENTED_EDGE ( 'NONE', *, *, #61318, .F. ) ;
#55426 = CARTESIAN_POINT ( 'NONE',  ( 0.7044674535452954967, 40.69315356317272148, 27.49308960257011947 ) ) ;
#55427 = CARTESIAN_POINT ( 'NONE',  ( 3.376099380956838925, 2.658192826266143616, 13.13934528545674318 ) ) ;
#55428 = ADVANCED_FACE ( 'NONE', ( #26696 ), #35546, .F. ) ;
#55429 = EDGE_CURVE ( 'NONE', #36314, #53833, #27, .T. ) ;
#55430 = ORIENTED_EDGE ( 'NONE', *, *, #15293, .T. ) ;
#55431 = CARTESIAN_POINT ( 'NONE',  ( -6.016104459813371719, -18.68271063303493307, -2.454244026261287015 ) ) ;
#55432 = ORIENTED_EDGE ( 'NONE', *, *, #44960, .F. ) ;
#55433 = EDGE_CURVE ( 'NONE', #37278, #40338, #25612, .T. ) ;
#55434 = CARTESIAN_POINT ( 'NONE',  ( 0.5807400328401574052, -33.48217046439135913, 34.25275203086223286 ) ) ;
#55435 = CARTESIAN_POINT ( 'NONE',  ( 0.9752570700956780803, -34.18150842933900435, 25.93764562640092564 ) ) ;
#55436 = AXIS2_PLACEMENT_3D ( 'NONE', #22317, #32337, #51413 ) ;
#55437 = CARTESIAN_POINT ( 'NONE',  ( 5.959547316686252039, 17.77392908783934189, -10.26589671991344588 ) ) ;
#55438 = FACE_OUTER_BOUND ( 'NONE', #48498, .T. ) ;
#55439 = EDGE_CURVE ( 'NONE', #29740, #40143, #52446, .T. ) ;
#55440 = ORIENTED_EDGE ( 'NONE', *, *, #16816, .F. ) ;
#55441 = CARTESIAN_POINT ( 'NONE',  ( 0.9754292589017217185, 10.28092790612040908, 40.62794590284416074 ) ) ;
#55442 = CARTESIAN_POINT ( 'NONE',  ( 3.782542959838393504, 16.70562020489267141, -38.57667827802765714 ) ) ;
#55443 = ADVANCED_FACE ( 'NONE', ( #57038 ), #61117, .F. ) ;
#55444 = CARTESIAN_POINT ( 'NONE',  ( 0.2224561200757602386, -39.54039348282969257, -17.20021002050910042 ) ) ;
#55445 = CARTESIAN_POINT ( 'NONE',  ( -2.601141883200662974, 14.30071512379477028, 4.276093359300773500 ) ) ;
#55446 = CARTESIAN_POINT ( 'NONE',  ( 0.9740398440564310700, 36.95080095316304636, -21.81228698783102971 ) ) ;
#55447 = CARTESIAN_POINT ( 'NONE',  ( 0.5806925824938511393, 32.99217760300656010, 33.32774488853447536 ) ) ;
#55448 = DIRECTION ( 'NONE',  ( 1.000000000000000000, 1.836970198721027962E-16, -2.033782021272921061E-31 ) ) ;
#55449 = CARTESIAN_POINT ( 'NONE',  ( -6.001507490154110336, -7.225628667346451373, -17.40350523682702999 ) ) ;
#55450 = CARTESIAN_POINT ( 'NONE',  ( 2.281351352603294913, -43.80196780981706439, -19.56575819747271083 ) ) ;
#55451 = CIRCLE ( 'NONE', #20455, 5.100000000000000533 ) ;
#55452 = CARTESIAN_POINT ( 'NONE',  ( 0.6000166863083090663, 10.41802958826926506, 47.99258423138307705 ) ) ;
#55453 = CARTESIAN_POINT ( 'NONE',  ( 0.5839879882012694035, -29.15724166963622821, -37.99840755997075092 ) ) ;
#55454 = VERTEX_POINT ( 'NONE', #52344 ) ;
#55455 = CARTESIAN_POINT ( 'NONE',  ( 3.559346040607745287, -3.460731807603660837, -43.83438851972076833 ) ) ;
#55456 = DIRECTION ( 'NONE',  ( -1.000000000000000000, -0.000000000000000000, -0.000000000000000000 ) ) ;
#55457 = ORIENTED_EDGE ( 'NONE', *, *, #18346, .F. ) ;
#55458 = CARTESIAN_POINT ( 'NONE',  ( 0.6000166863083090663, 48.30184070260993678, 8.874438937090557644 ) ) ;
#55459 = CARTESIAN_POINT ( 'NONE',  ( 3.660176727303408484, -48.00143922595155743, -1.881607889988255344 ) ) ;
#55460 = EDGE_CURVE ( 'NONE', #31073, #31157, #46614, .T. ) ;
#55461 = CARTESIAN_POINT ( 'NONE',  ( 0.8560838555295223751, -14.76796170096679894, -44.52280473286144513 ) ) ;
#55462 = B_SPLINE_CURVE_WITH_KNOTS ( 'NONE', 3,
 ( #20525, #30217, #59643, #20225, #59025, #39341 ),
 .UNSPECIFIED., .F., .F.,
 ( 4, 2, 4 ),
 ( 0.000000000000000000, 0.0002450742804987318451, 0.0004901485609974636903 ),
 .UNSPECIFIED. ) ;
#55463 = ORIENTED_EDGE ( 'NONE', *, *, #17116, .F. ) ;
#55464 = CARTESIAN_POINT ( 'NONE',  ( 0.3676999524040323597, 3.413584541508654091, 43.98065510995502336 ) ) ;
#55465 = EDGE_CURVE ( 'NONE', #58167, #28193, #33844, .T. ) ;
#55466 = CARTESIAN_POINT ( 'NONE',  ( 0.8760168074887076939, 34.63873394077442214, 33.37827814204136700 ) ) ;
#55467 = CIRCLE ( 'NONE', #9459, 1.000000000000000666 ) ;
#55468 = CARTESIAN_POINT ( 'NONE',  ( 4.962356264823596597, 1.841560470688234474, 42.04574000888969465 ) ) ;
#55469 = ORIENTED_EDGE ( 'NONE', *, *, #13784, .T. ) ;
#55470 = CARTESIAN_POINT ( 'NONE',  ( 0.6845945791218034371, 5.556290360845241416, -46.57825842751017120 ) ) ;
#55471 = AXIS2_PLACEMENT_3D ( 'NONE', #12036, #31111, #50217 ) ;
#55472 = ORIENTED_EDGE ( 'NONE', *, *, #18044, .T. ) ;
#55473 = ORIENTED_EDGE ( 'NONE', *, *, #45938, .T. ) ;
#55474 = CARTESIAN_POINT ( 'NONE',  ( 0.1158403557922069033, 44.03104648574668545, 2.864830283600325878 ) ) ;
#55475 = VERTEX_POINT ( 'NONE', #19473 ) ;
#55476 = CARTESIAN_POINT ( 'NONE',  ( -6.077587904424778920, -8.912150607695380700, 17.06955163264944630 ) ) ;
#55477 = AXIS2_PLACEMENT_3D ( 'NONE', #47439, #19251, #46521 ) ;
#55478 = ORIENTED_EDGE ( 'NONE', *, *, #35086, .F. ) ;
#55479 = CARTESIAN_POINT ( 'NONE',  ( 4.975610109902397937, -37.61482235126175766, 31.26618855282478648 ) ) ;
#55480 = CARTESIAN_POINT ( 'NONE',  ( 0.9730545539215883499, 15.95224156741828914, 39.83279466599044838 ) ) ;
#55481 = ORIENTED_EDGE ( 'NONE', *, *, #21394, .T. ) ;
#55482 = CARTESIAN_POINT ( 'NONE',  ( 5.917102823773431552, -19.39506196288392559, 5.321775033542383682 ) ) ;
#55483 = LINE ( 'NONE', #22610, #5474 ) ;
#55484 = CARTESIAN_POINT ( 'NONE',  ( 0.5998501479064708430, 17.92509395669044636, 44.64337787626254794 ) ) ;
#55485 = CARTESIAN_POINT ( 'NONE',  ( 0.5832655196449139101, -30.45084774278391393, 35.66484339961580474 ) ) ;
#55486 = ORIENTED_EDGE ( 'NONE', *, *, #24038, .F. ) ;
#55487 = CARTESIAN_POINT ( 'NONE',  ( 0.5809828226811617480, 44.03860873105695362, 18.83114015454715684 ) ) ;
#55488 = ORIENTED_EDGE ( 'NONE', *, *, #44796, .T. ) ;
#55489 = CARTESIAN_POINT ( 'NONE',  ( 0.9741495583595167762, -42.90659993968957053, -0.3955098476636077498 ) ) ;
#55490 = EDGE_CURVE ( 'NONE', #31937, #10199, #8396, .T. ) ;
#55491 = CARTESIAN_POINT ( 'NONE',  ( 0.1157506346131639274, -12.46557269385145439, 42.32670737509757686 ) ) ;
#55492 = VECTOR ( 'NONE', #26497, 1000.000000000000114 ) ;
#55493 = CARTESIAN_POINT ( 'NONE',  ( 4.956653778116893783, -15.97476558431863758, -45.35992544608534160 ) ) ;
#55494 = EDGE_LOOP ( 'NONE', ( #53718, #7706 ) ) ;
#55495 = CARTESIAN_POINT ( 'NONE',  ( 5.959828726073459926, 2.674641840416173810, -20.35060134307031987 ) ) ;
#55496 = CARTESIAN_POINT ( 'NONE',  ( -6.015611763856276717, -4.882992715191171840, -18.19956619163663447 ) ) ;
#55497 = EDGE_CURVE ( 'NONE', #55302, #36560, #34811, .T. ) ;
#55498 = CARTESIAN_POINT ( 'NONE',  ( 0.6008123274975391004, 27.73703781927353518, 40.52420615102345636 ) ) ;
#55499 = CARTESIAN_POINT ( 'NONE',  ( 0.6025881611877910160, -41.55278713510066524, -24.24244696985793723 ) ) ;
#55500 = ADVANCED_FACE ( 'NONE', ( #11003 ), #5493, .F. ) ;
#55501 = VERTEX_POINT ( 'NONE', #15702 ) ;
#55502 = ORIENTED_EDGE ( 'NONE', *, *, #9381, .T. ) ;
#55503 = FACE_OUTER_BOUND ( 'NONE', #23747, .T. ) ;
#55504 = EDGE_CURVE ( 'NONE', #10852, #40429, #33070, .T. ) ;
#55505 = CARTESIAN_POINT ( 'NONE',  ( 2.282816707992310956, -20.95674216433703663, -42.03940918073735844 ) ) ;
#55506 = CARTESIAN_POINT ( 'NONE',  ( 0.3676999524040366896, 3.413584541509296688, -43.98065510995495941 ) ) ;
#55507 = CARTESIAN_POINT ( 'NONE',  ( 4.962356264823608143, 41.96072444189411499, 3.245489512196318316 ) ) ;
#55508 = B_SPLINE_CURVE_WITH_KNOTS ( 'NONE', 3,
 ( #11146, #30230, #35266, #54953, #6392, #54324 ),
 .UNSPECIFIED., .F., .F.,
 ( 4, 2, 4 ),
 ( 0.000000000000000000, 0.0002450742804987325499, 0.0004901485609974650997 ),
 .UNSPECIFIED. ) ;
#55509 =( BOUNDED_SURFACE ( )  B_SPLINE_SURFACE ( 3, 1, ( 
 ( #41983, #18459 ),
 ( #4952, #24081 ),
 ( #56963, #37906 ),
 ( #9993, #33187 ) ),
 .UNSPECIFIED., .F., .F., .F. ) 
 B_SPLINE_SURFACE_WITH_KNOTS ( ( 4, 4 ),
 ( 2, 2 ),
 ( 0.000000000000000000, 1.000000000000000000 ),
 ( 0.000000000000000000, 1.000000000000000000 ),
 .UNSPECIFIED. ) 
 GEOMETRIC_REPRESENTATION_ITEM ( )  RATIONAL_B_SPLINE_SURFACE ( (
 ( 1.000000000000000000, 1.000000000000000000),
 ( 0.7282232189291694135, 0.9929344683865672927),
 ( 0.7282232189291694135, 0.9929344683865672927),
 ( 1.000000000000000000, 1.000000000000000000) ) ) 
 REPRESENTATION_ITEM ( '' )  SURFACE ( )  );
#55510 = DIRECTION ( 'NONE',  ( -1.000000000000000000, -0.000000000000000000, -0.000000000000000000 ) ) ;
#55511 = VECTOR ( 'NONE', #53564, 1000.000000000000000 ) ;
#55512 = CARTESIAN_POINT ( 'NONE',  ( 4.962356264823608143, 22.27740539909265394, 35.70648129607319277 ) ) ;
#55513 = LINE ( 'NONE', #21709, #10887 ) ;
#55514 = VECTOR ( 'NONE', #50000, 1000.000000000000000 ) ;
#55515 = CARTESIAN_POINT ( 'NONE',  ( 4.956445790443988031, 0.000000000000000000, 0.000000000000000000 ) ) ;
#55516 = CARTESIAN_POINT ( 'NONE',  ( 0.9788927965476027504, 32.97753259754014010, 25.86153430115767193 ) ) ;
#55517 = VECTOR ( 'NONE', #23614, 1000.000000000000000 ) ;
#55518 = CARTESIAN_POINT ( 'NONE',  ( 0.5806925824938499181, 32.99217760300705748, -33.32774488853398509 ) ) ;
#55519 = CARTESIAN_POINT ( 'NONE',  ( 0.6009452777970412107, -34.32439724343015541, -33.70725232128880577 ) ) ;
#55520 = CARTESIAN_POINT ( 'NONE',  ( -6.016104459813374383, 14.94608397322084414, 11.47525878590921344 ) ) ;
#55521 = CARTESIAN_POINT ( 'NONE',  ( 0.5850706913938533704, 6.431767090163499567, -47.46255051844946848 ) ) ;
#55522 =( BOUNDED_SURFACE ( )  B_SPLINE_SURFACE ( 3, 1, ( 
 ( #61484, #28300 ),
 ( #56794, #48036 ),
 ( #19535, #83 ),
 ( #14225, #24214 ) ),
 .UNSPECIFIED., .F., .F., .F. ) 
 B_SPLINE_SURFACE_WITH_KNOTS ( ( 4, 4 ),
 ( 2, 2 ),
 ( 0.000000000000000000, 1.000000000000000000 ),
 ( 0.000000000000000000, 1.000000000000000000 ),
 .UNSPECIFIED. ) 
 GEOMETRIC_REPRESENTATION_ITEM ( )  RATIONAL_B_SPLINE_SURFACE ( (
 ( 1.000000000000000000, 1.000000000000000000),
 ( 0.9953485035131437453, 0.8621029689291523912),
 ( 0.9953485035131437453, 0.8621029689291523912),
 ( 1.000000000000000000, 1.000000000000000000) ) ) 
 REPRESENTATION_ITEM ( '' )  SURFACE ( )  );
#55523 = DIRECTION ( 'NONE',  ( 0.000000000000000000, 0.000000000000000000, 1.000000000000000000 ) ) ;
#55524 = CARTESIAN_POINT ( 'NONE',  ( 0.6016118706126977189, 16.63270000191639397, 46.20502511015637737 ) ) ;
#55525 = DIRECTION ( 'NONE',  ( -1.000000000000000000, -0.000000000000000000, -0.000000000000000000 ) ) ;
#55527 = VERTEX_POINT ( 'NONE', #11298 ) ;
#55526 = DIRECTION ( 'NONE',  ( 0.000000000000000000, 0.000000000000000000, 1.000000000000000000 ) ) ;
#55528 = VERTEX_POINT ( 'NONE', #24465 ) ;
#55529 = CARTESIAN_POINT ( 'NONE',  ( 2.500000000000000000, 0.000000000000000000, 0.000000000000000000 ) ) ;
#55530 = CARTESIAN_POINT ( 'NONE',  ( 1.154321713695927842, 6.418927679456245095, -42.43366804783609325 ) ) ;
#55531 = ORIENTED_EDGE ( 'NONE', *, *, #9615, .F. ) ;
#55532 = VERTEX_POINT ( 'NONE', #30387 ) ;
#55533 = CARTESIAN_POINT ( 'NONE',  ( 1.827119703190778877, 42.50321986945169073, -6.838980420687535755 ) ) ;
#55534 = CARTESIAN_POINT ( 'NONE',  ( 0.8744876279028306332, 5.599149760997630842, 48.77498920895230583 ) ) ;
#55535 = UNCERTAINTY_MEASURE_WITH_UNIT (LENGTH_MEASURE( 1.000000000000000082E-05 ), #45164, 'distance_accuracy_value', 'NONE');
#55536 = ORIENTED_EDGE ( 'NONE', *, *, #21279, .F. ) ;
#55537 = ORIENTED_EDGE ( 'NONE', *, *, #9809, .T. ) ;
#55538 = EDGE_CURVE ( 'NONE', #22241, #13203, #20095, .T. ) ;
#55539 = CARTESIAN_POINT ( 'NONE',  ( 0.5827357941260203900, 47.89462047563813485, -0.3632531319016042981 ) ) ;
#55540 = FACE_OUTER_BOUND ( 'NONE', #48709, .T. ) ;
#55541 = CARTESIAN_POINT ( 'NONE',  ( 0.9756354156337452288, -41.47994205070121154, 10.97961179198184745 ) ) ;
#55542 = B_SPLINE_CURVE_WITH_KNOTS ( 'NONE', 3,
 ( #27566, #31036, #45466, #35758, #21636, #3132, #13177, #26955, #7203, #50144, #26331, #8442, #2512, #11960, #40777, #59843, #46384, #16959, #22873 ),
 .UNSPECIFIED., .F., .F.,
 ( 4, 3, 3, 3, 3, 3, 4 ),
 ( 3.469446951953614189E-18, 0.0002724573126191812307, 0.0004086839781548551992, 0.0005449106435902030619, 0.0006811373090491647936, 0.0008459866663933863964, 0.001010840725717218136 ),
 .UNSPECIFIED. ) ;
#55543 = ORIENTED_EDGE ( 'NONE', *, *, #5612, .F. ) ;
#55544 = CARTESIAN_POINT ( 'NONE',  ( 4.549368137175248350, -28.46244473166695954, 32.13400537129875545 ) ) ;
#55545 = DIRECTION ( 'NONE',  ( -1.000000000000000000, -1.836909530733573776E-16, 1.925929944387235853E-32 ) ) ;
#55546 = VECTOR ( 'NONE', #18757, 1000.000000000000227 ) ;
#55547 = DIRECTION ( 'NONE',  ( 1.000000000000000000, 0.000000000000000000, 0.000000000000000000 ) ) ;
#55548 = VERTEX_POINT ( 'NONE', #59201 ) ;
#55549 = VERTEX_POINT ( 'NONE', #39213 ) ;
#55550 = CARTESIAN_POINT ( 'NONE',  ( 5.959547316686252039, 17.77749189599203206, 10.25972575517536178 ) ) ;
#55551 = AXIS2_PLACEMENT_3D ( 'NONE', #13741, #61315, #9017 ) ;
#55552 = ORIENTED_EDGE ( 'NONE', *, *, #23085, .F. ) ;
#55553 = CARTESIAN_POINT ( 'NONE',  ( 0.5782707292762442330, -35.26595510591691607, 30.92003823049173405 ) ) ;
#55554 = CARTESIAN_POINT ( 'NONE',  ( 1.227938101723748288, 39.96870412324358313, -15.63977281655798812 ) ) ;
#55555 = LINE ( 'NONE', #12685, #1620 ) ;
#55556 = CARTESIAN_POINT ( 'NONE',  ( 4.962356264823609031, -20.60668162140307658, 36.69605251817252878 ) ) ;
#55557 = CARTESIAN_POINT ( 'NONE',  ( 0.5836750258453360374, 12.57171936981227489, -46.21662382526641721 ) ) ;
#55558 = AXIS2_PLACEMENT_3D ( 'NONE', #43290, #8824, #61120 ) ;
#55559 = ORIENTED_EDGE ( 'NONE', *, *, #49471, .F. ) ;
#55560 = CARTESIAN_POINT ( 'NONE',  ( 0.5824935313925969638, -13.54582896752205201, 44.89709004642145374 ) ) ;
#55561 = CYLINDRICAL_SURFACE ( 'NONE', #54751, 2.649999999999992806 ) ;
#55562 = EDGE_CURVE ( 'NONE', #39239, #36997, #6557, .T. ) ;
#55563 = CARTESIAN_POINT ( 'NONE',  ( -6.072942160501519915, 3.058960253794702489, -19.01175753197806273 ) ) ;
#55564 = ORIENTED_EDGE ( 'NONE', *, *, #9870, .F. ) ;
#55565 = DIRECTION ( 'NONE',  ( -1.000000000000000000, -0.000000000000000000, -0.000000000000000000 ) ) ;
#55566 = EDGE_CURVE ( 'NONE', #51862, #27417, #16305, .T. ) ;
#55567 = CARTESIAN_POINT ( 'NONE',  ( 0.8744876279028263033, -45.83369275826233036, 17.59609782084381280 ) ) ;
#55568 = CARTESIAN_POINT ( 'NONE',  ( 0.9730545539215883499, 30.69604515769650632, 29.98130006528872826 ) ) ;
#55569 = DIRECTION ( 'NONE',  ( 0.000000000000000000, -1.000000000000000000, 0.000000000000000000 ) ) ;
#55570 = ORIENTED_EDGE ( 'NONE', *, *, #57510, .T. ) ;
#55571 = CARTESIAN_POINT ( 'NONE',  ( 0.2940135542859018680, -11.77874396291204384, 42.51472379479353947 ) ) ;
#55572 = EDGE_CURVE ( 'NONE', #45423, #1146, #58554, .T. ) ;
#55573 = CARTESIAN_POINT ( 'NONE',  ( 0.5809828226811617480, -33.48000389720591841, -34.25055090842189287 ) ) ;
#55574 = CARTESIAN_POINT ( 'NONE',  ( 0.5800708057587397048, -0.6275304576133720058, 47.89175345272233386 ) ) ;
#55575 = B_SPLINE_CURVE_WITH_KNOTS ( 'NONE', 3,
 ( #39325, #35239, #58386, #48703 ),
 .UNSPECIFIED., .F., .F.,
 ( 4, 4 ),
 ( 8.673617379884035472E-19, 0.004050076154993000749 ),
 .UNSPECIFIED. ) ;
#55576 = DIRECTION ( 'NONE',  ( 0.9848077530122079093, 0.1736481776669316079, -5.551115123125783935E-17 ) ) ;
#55577 = DIRECTION ( 'NONE',  ( 1.836766033387207149E-16, -1.000000000000000000, 0.000000000000000000 ) ) ;
#55578 = CARTESIAN_POINT ( 'NONE',  ( 0.5797568665920721509, 40.66629937448812626, 23.35545768736671945 ) ) ;
#55579 = DIRECTION ( 'NONE',  ( -1.000000000000000000, 0.000000000000000000, 0.000000000000000000 ) ) ;
#55580 = CARTESIAN_POINT ( 'NONE',  ( 2.282803330402964015, -41.31566501690780768, -22.34978146800645149 ) ) ;
#55581 = CARTESIAN_POINT ( 'NONE',  ( 4.291220156522060236, 42.48586100259165477, -20.35535831603462853 ) ) ;
#55582 = FACE_OUTER_BOUND ( 'NONE', #31745, .T. ) ;
#55584 = ORIENTED_EDGE ( 'NONE', *, *, #3872, .F. ) ;
#55583 = EDGE_CURVE ( 'NONE', #15737, #61648, #41280, .T. ) ;
#55585 = CARTESIAN_POINT ( 'NONE',  ( -6.017396004339686577, 2.458362590803059078, -18.68211039806561047 ) ) ;
#55586 = CARTESIAN_POINT ( 'NONE',  ( 2.281351352603294469, -40.87339198768977155, -25.11567449372752137 ) ) ;
#55588 = EDGE_CURVE ( 'NONE', #43576, #31789, #30085, .T. ) ;
#55587 = CARTESIAN_POINT ( 'NONE',  ( 0.8557997880470690211, -0.9121262075942833114, -47.89938907511595545 ) ) ;
#55589 = CARTESIAN_POINT ( 'NONE',  ( 3.240649175237396484, 11.56283248366031913, -42.44485625317231126 ) ) ;
#55590 = CARTESIAN_POINT ( 'NONE',  ( 5.917102823773431552, -11.92306321980351846, 16.19661327278979357 ) ) ;
#55591 = CARTESIAN_POINT ( 'NONE',  ( 0.5786265663353196143, -47.58023467411541674, 5.535668456753771949 ) ) ;
#55592 = APPLICATION_PROTOCOL_DEFINITION ( 'draft international standard', 'automotive_design', 1998, #18800 ) ;
#55593 = CARTESIAN_POINT ( 'NONE',  ( 0.6017666602106489515, -44.31084100715266061, 18.73203020817283004 ) ) ;
#55594 = CARTESIAN_POINT ( 'NONE',  ( 0.9783242366443549720, -7.234864208425438648, 41.27942865510820525 ) ) ;
#55595 = CARTESIAN_POINT ( 'NONE',  ( 4.549368137175248350, 32.41327393324100825, 28.14399996863509301 ) ) ;
#55597 = ORIENTED_EDGE ( 'NONE', *, *, #4139, .F. ) ;
#55596 = LINE ( 'NONE', #55288, #32344 ) ;
#55598 = VERTEX_POINT ( 'NONE', #48281 ) ;
#55599 = CIRCLE ( 'NONE', #52568, 85.00000000000001421 ) ;
#55600 = B_SPLINE_CURVE_WITH_KNOTS ( 'NONE', 3,
 ( #11512, #55322, #20601, #21520 ),
 .UNSPECIFIED., .F., .F.,
 ( 4, 4 ),
 ( 4.336808689942017736E-19, 0.004041751736740997747 ),
 .UNSPECIFIED. ) ;
#55601 = CARTESIAN_POINT ( 'NONE',  ( 0.5997462898726536595, 27.66511329191589397, 40.57330571557817223 ) ) ;
#55602 = CARTESIAN_POINT ( 'NONE',  ( -2.739355103387248747, -14.92576340101414800, 0.2629711922692996584 ) ) ;
#55603 = CARTESIAN_POINT ( 'NONE',  ( 5.895596859100789899, -9.662743138698489886, 17.63971593444811603 ) ) ;
#55604 = AXIS2_PLACEMENT_3D ( 'NONE', #28875, #57661, #33908 ) ;
#55605 = EDGE_LOOP ( 'NONE', ( #30893, #11975, #5095, #55915 ) ) ;
#55606 = CARTESIAN_POINT ( 'NONE',  ( 0.5987334363312692975, -47.34446306252520742, -13.04088661837312380 ) ) ;
#55607 = CARTESIAN_POINT ( 'NONE',  ( -6.078726893082806448, 3.069885851706299462, 19.00973019603943825 ) ) ;
#55608 = CARTESIAN_POINT ( 'NONE',  ( 0.6027935024548037868, -44.37842839362961911, -18.57106801640284033 ) ) ;
#55609 = B_SPLINE_CURVE_WITH_KNOTS ( 'NONE', 3,
 ( #29644, #48754, #54350, #14960, #43469, #24961 ),
 .UNSPECIFIED., .F., .F.,
 ( 4, 2, 4 ),
 ( 8.571645052368668133E-17, 0.0002293366620881447950, 0.0004586733241762038838 ),
 .UNSPECIFIED. ) ;
#55610 = ORIENTED_EDGE ( 'NONE', *, *, #34815, .T. ) ;
#55611 = ORIENTED_EDGE ( 'NONE', *, *, #47815, .F. ) ;
#55612 = EDGE_CURVE ( 'NONE', #8944, #18653, #37620, .T. ) ;
#55613 = DIRECTION ( 'NONE',  ( -0.9997530559290660479, -0.02222222222222222307, 0.000000000000000000 ) ) ;
#55614 = CIRCLE ( 'NONE', #54615, 48.91267123290010943 ) ;
#55615 = CARTESIAN_POINT ( 'NONE',  ( 3.727782113643637096, 37.96789553646228654, 22.16340868274241771 ) ) ;
#55616 = CARTESIAN_POINT ( 'NONE',  ( -13.51351822333069030, -12.53706398592619387, 7.845252193381024343E-16 ) ) ;
#55617 = ORIENTED_EDGE ( 'NONE', *, *, #38507, .F. ) ;
#55618 = CARTESIAN_POINT ( 'NONE',  ( 3.390910168358336918, -43.93422347332083433, 1.970062011699514448 ) ) ;
#55619 = CARTESIAN_POINT ( 'NONE',  ( 0.1156867017252034557, -42.64922063473789393, -11.31312452528629109 ) ) ;
#55620 = B_SPLINE_CURVE_WITH_KNOTS ( 'NONE', 3,
 ( #45931, #2976, #22097, #56214, #17397, #13326 ),
 .UNSPECIFIED., .F., .F.,
 ( 4, 2, 4 ),
 ( 0.000000000000000000, 0.0002291459268755710480, 0.0004582918537511420959 ),
 .UNSPECIFIED. ) ;
#55621 = DIRECTION ( 'NONE',  ( 0.1011922191286467876, -0.8604626000150176202, 0.4993638440688468183 ) ) ;
#55622 = CARTESIAN_POINT ( 'NONE',  ( -6.078726893082806448, -6.647148524917739998, 18.07233957617010134 ) ) ;
#55623 = VERTEX_POINT ( 'NONE', #29164 ) ;
#55624 = DIRECTION ( 'NONE',  ( 0.07439287786467665975, -0.5965490341031266519, -0.7991213610169847215 ) ) ;
#55625 = VERTEX_POINT ( 'NONE', #7821 ) ;
#55626 = CARTESIAN_POINT ( 'NONE',  ( 2.528100132419515589, -31.93277260506748760, -27.24980389626917443 ) ) ;
#55627 = CARTESIAN_POINT ( 'NONE',  ( 0.2230388203127593727, 34.66629317821133327, 25.64246103889307449 ) ) ;
#55628 = CARTESIAN_POINT ( 'NONE',  ( 4.956653778116994147, 39.67974989265076857, -27.17045123668430406 ) ) ;
#55629 =( LENGTH_UNIT ( ) NAMED_UNIT ( * ) SI_UNIT ( .MILLI., .METRE. ) );
#55630 = ORIENTED_EDGE ( 'NONE', *, *, #11624, .T. ) ;
#55631 = ORIENTED_EDGE ( 'NONE', *, *, #56123, .T. ) ;
#55632 = CARTESIAN_POINT ( 'NONE',  ( 4.967162193818131399, -23.56777426397203357, 36.06913038482792189 ) ) ;
#55633 = LINE ( 'NONE', #17757, #40045 ) ;
#55634 = VERTEX_POINT ( 'NONE', #50130 ) ;
#55635 = DIRECTION ( 'NONE',  ( 0.000000000000000000, 0.000000000000000000, 1.000000000000000000 ) ) ;
#55636 = VERTEX_POINT ( 'NONE', #30701 ) ;
#55637 = FACE_OUTER_BOUND ( 'NONE', #58568, .T. ) ;
#55638 = EDGE_CURVE ( 'NONE', #28532, #4, #26944, .T. ) ;
#55639 = CIRCLE ( 'NONE', #53616, 42.92674063221959813 ) ;
#55640 = ORIENTED_EDGE ( 'NONE', *, *, #55378, .T. ) ;
#55641 = CARTESIAN_POINT ( 'NONE',  ( 5.960721111146673579, -0.006321279846963646747, 20.52557019979492026 ) ) ;
#55642 = CARTESIAN_POINT ( 'NONE',  ( 0.9780303403264775097, 25.11936797697908119, 33.54634057288815541 ) ) ;
#55643 = VECTOR ( 'NONE', #43116, 1000.000000000000114 ) ;
#55644 = CARTESIAN_POINT ( 'NONE',  ( 0.1147471544378677599, -43.72123235070954905, 5.950296648782622100 ) ) ;
#55645 = ORIENTED_EDGE ( 'NONE', *, *, #16319, .T. ) ;
#55646 = CARTESIAN_POINT ( 'NONE',  ( 0.1152339509894530906, -27.68528683457054740, -34.35793333922745774 ) ) ;
#55647 = AXIS2_PLACEMENT_3D ( 'NONE', #49339, #59344, #20846 ) ;
#55648 = ADVANCED_FACE ( 'NONE', ( #49817 ), #50224, .F. ) ;
#55649 = DIRECTION ( 'NONE',  ( 0.07439287786467665975, -0.9597484305373191749, -0.2708295585865100885 ) ) ;
#55650 = CARTESIAN_POINT ( 'NONE',  ( 0.5848930533535030563, 43.10374212188040133, 18.47540249840287530 ) ) ;
#55651 = B_SPLINE_CURVE_WITH_KNOTS ( 'NONE', 3,
 ( #54020, #49337, #49643, #40290, #11765, #59342 ),
 .UNSPECIFIED., .F., .F.,
 ( 4, 2, 4 ),
 ( 1.764953265579307567E-18, 0.0002450742804987336341, 0.0004901485609974654250 ),
 .UNSPECIFIED. ) ;
#55652 = EDGE_CURVE ( 'NONE', #17422, #38487, #7534, .T. ) ;
#55653 = ORIENTED_EDGE ( 'NONE', *, *, #37422, .T. ) ;
#55654 = DIRECTION ( 'NONE',  ( 0.07906939808003035641, 0.1737655548591788279, -0.9816076416938406268 ) ) ;
#55655 = CARTESIAN_POINT ( 'NONE',  ( 5.917102823773431552, 10.81462311420869327, 16.95681706421830270 ) ) ;
#55656 = DIRECTION ( 'NONE',  ( 1.000000000000000000, 0.000000000000000000, 0.000000000000000000 ) ) ;
#55657 = CARTESIAN_POINT ( 'NONE',  ( 0.1103744047535531458, 26.28322091066875998, -34.18931094755013333 ) ) ;
#55658 = B_SPLINE_CURVE_WITH_KNOTS ( 'NONE', 3,
 ( #14584, #38398, #29273, #24270 ),
 .UNSPECIFIED., .F., .F.,
 ( 4, 4 ),
 ( 0.000000000000000000, 0.002290414566844504660 ),
 .UNSPECIFIED. ) ;
#55659 = CARTESIAN_POINT ( 'NONE',  ( 4.833616638992208614, -9.466882727841817058, -45.27110352095245815 ) ) ;
#55660 = ORIENTED_EDGE ( 'NONE', *, *, #56171, .F. ) ;
#55661 = CIRCLE ( 'NONE', #13666, 42.08604991992415023 ) ;
#55662 = CARTESIAN_POINT ( 'NONE',  ( 0.1101816497532062678, 37.27878591512674689, -21.67974746580510725 ) ) ;
#55663 = CARTESIAN_POINT ( 'NONE',  ( 0.5806925824938499181, 40.06810415365472977, 24.36738377166168235 ) ) ;
#55664 = ORIENTED_EDGE ( 'NONE', *, *, #16028, .T. ) ;
#55665 = CARTESIAN_POINT ( 'NONE',  ( 0.9757402383260940226, -30.40085236181972306, 30.28078671294513668 ) ) ;
#55667 = EDGE_CURVE ( 'NONE', #11266, #33185, #48682, .T. ) ;
#55666 = CARTESIAN_POINT ( 'NONE',  ( 5.959547316686252039, -18.96456592444095435, -7.851524054666348285 ) ) ;
#55668 = CARTESIAN_POINT ( 'NONE',  ( 0.3676999524040366896, 19.66859742988788184, -39.48540057367844724 ) ) ;
#55669 = CARTESIAN_POINT ( 'NONE',  ( 2.618530812446111078, -41.30116959783728703, -22.44861196263326164 ) ) ;
#55670 = CARTESIAN_POINT ( 'NONE',  ( 0.6008123274975393224, 4.281860609577630150, 48.92055008765341029 ) ) ;
#55671 = CARTESIAN_POINT ( 'NONE',  ( 0.5998501479064699549, 38.48283596221989455, 28.86886762351138103 ) ) ;
#55672 = CARTESIAN_POINT ( 'NONE',  ( -6.079354080745853928, -11.01571246550363803, -15.79389230447991110 ) ) ;
#55673 = CARTESIAN_POINT ( 'NONE',  ( -6.078726893082806448, 13.83016815118519638, 13.39852567182907350 ) ) ;
#55674 = CARTESIAN_POINT ( 'NONE',  ( 1.091591847532196846, 10.47380871615908582, -40.58396631593750215 ) ) ;
#55675 = CARTESIAN_POINT ( 'NONE',  ( 4.553261556744873317, 43.59419396814051595, 5.393126930805304475 ) ) ;
#55676 = CARTESIAN_POINT ( 'NONE',  ( 0.5804410086790514622, -41.60900809504508402, -21.63816760268459660 ) ) ;
#55677 = CARTESIAN_POINT ( 'NONE',  ( 0.6008122571543325074, -2.009120241389370509, -49.06646498700467873 ) ) ;
#55678 = CARTESIAN_POINT ( 'NONE',  ( 1.657374760986085827, 16.37088960564075180, 40.90090977927223292 ) ) ;
#55679 = LINE ( 'NONE', #36933, #28451 ) ;
#55680 = CARTESIAN_POINT ( 'NONE',  ( 0.5830081025819934260, 46.51316544950417864, 5.979755367010718636 ) ) ;
#55681 = ORIENTED_EDGE ( 'NONE', *, *, #42455, .T. ) ;
#55682 = CARTESIAN_POINT ( 'NONE',  ( 4.956445790443991584, 34.56007374686787159, 31.98654955994301829 ) ) ;
#55683 = CARTESIAN_POINT ( 'NONE',  ( 4.060580049360325461, -33.13615358156597779, -28.86975961413743974 ) ) ;
#55684 = CIRCLE ( 'NONE', #28697, 2.649999999999999467 ) ;
#55685 = FACE_OUTER_BOUND ( 'NONE', #46477, .T. ) ;
#55686 = CARTESIAN_POINT ( 'NONE',  ( 4.553261556744873317, -20.11719049292697648, 39.04917684785332455 ) ) ;
#55687 = CIRCLE ( 'NONE', #31704, 48.91267123290010943 ) ;
#55688 = VERTEX_POINT ( 'NONE', #22248 ) ;
#55689 = EDGE_CURVE ( 'NONE', #51034, #6891, #54811, .T. ) ;
#55690 = CARTESIAN_POINT ( 'NONE',  ( 0.5809828226811553087, -6.791453954330003207, -47.41188724015886180 ) ) ;
#55691 = B_SPLINE_CURVE_WITH_KNOTS ( 'NONE', 3,
 ( #45337, #6141, #2378, #26506, #1149, #1760, #25278, #39401, #45034, #59084, #2064, #30583, #6754, #16196, #44422, #1446 ),
 .UNSPECIFIED., .F., .F.,
 ( 4, 3, 3, 3, 3, 4 ),
 ( 1.962735358247463844E-17, 0.0002612764279487778249, 0.0003919131003184803835, 0.0005225497727000590759, 0.0007837925190632501248, 0.001045051706266716517 ),
 .UNSPECIFIED. ) ;
#55692 = EDGE_CURVE ( 'NONE', #14390, #6519, #1543, .T. ) ;
#55693 = CARTESIAN_POINT ( 'NONE',  ( 0.6017667736363749853, 24.35549005323416694, -41.48674115080378755 ) ) ;
#55694 =( BOUNDED_SURFACE ( )  B_SPLINE_SURFACE ( 3, 1, ( 
 ( #53446, #34997 ),
 ( #44107, #15570 ),
 ( #47013, #54058 ),
 ( #56680, #15880 ) ),
 .UNSPECIFIED., .F., .F., .F. ) 
 B_SPLINE_SURFACE_WITH_KNOTS ( ( 4, 4 ),
 ( 2, 2 ),
 ( 0.000000000000000000, 1.000000000000000000 ),
 ( 0.000000000000000000, 1.000000000000000000 ),
 .UNSPECIFIED. ) 
 GEOMETRIC_REPRESENTATION_ITEM ( )  RATIONAL_B_SPLINE_SURFACE ( (
 ( 1.000000000000000000, 1.000000000000000000),
 ( 0.9953390228620291325, 0.8624445117760984880),
 ( 0.9953390228620291325, 0.8624445117760984880),
 ( 1.000000000000000000, 1.000000000000000000) ) ) 
 REPRESENTATION_ITEM ( '' )  SURFACE ( )  );
#55695 = VERTEX_POINT ( 'NONE', #60134 ) ;
#55696 = B_SPLINE_CURVE_WITH_KNOTS ( 'NONE', 3,
 ( #12673, #17665, #32083, #7308 ),
 .UNSPECIFIED., .F., .F.,
 ( 4, 4 ),
 ( 7.589415207398531038E-19, 0.004446298630425064152 ),
 .UNSPECIFIED. ) ;
#55697 = EDGE_CURVE ( 'NONE', #14464, #53183, #6829, .T. ) ;
#55698 = CARTESIAN_POINT ( 'NONE',  ( 0.7056759521545038494, 37.32480390860856545, -28.40084228153992285 ) ) ;
#55699 = ORIENTED_EDGE ( 'NONE', *, *, #43894, .T. ) ;
#55700 = CARTESIAN_POINT ( 'NONE',  ( 0.5827357941260198348, -0.3632531319011024773, -47.89462047563813485 ) ) ;
#55701 = CARTESIAN_POINT ( 'NONE',  ( 4.967162193818130511, 36.06913038482831979, -23.56777426397140118 ) ) ;
#55702 = VERTEX_POINT ( 'NONE', #60426 ) ;
#55703 = FACE_OUTER_BOUND ( 'NONE', #48013, .T. ) ;
#55704 = CARTESIAN_POINT ( 'NONE',  ( 0.8753041380234524160, 37.96023374381034898, 31.14737520222631417 ) ) ;
#55705 = ORIENTED_EDGE ( 'NONE', *, *, #40202, .F. ) ;
#55706 = CARTESIAN_POINT ( 'NONE',  ( 0.7948878604505668077, -43.19977686076578038, -23.33405079446049868 ) ) ;
#55707 = CARTESIAN_POINT ( 'NONE',  ( 0.9762797500689124330, 41.59901070109202692, -5.084003725031680077 ) ) ;
#55708 = AXIS2_PLACEMENT_3D ( 'NONE', #48153, #39084, #34366 ) ;
#55709 = ORIENTED_EDGE ( 'NONE', *, *, #1048, .F. ) ;
#55710 = CARTESIAN_POINT ( 'NONE',  ( -6.001507490154110336, 9.408444979392550422, -16.32705935667497243 ) ) ;
#55711 = ORIENTED_EDGE ( 'NONE', *, *, #53854, .T. ) ;
#55712 = CARTESIAN_POINT ( 'NONE',  ( -6.001507490154111224, -0.01557731607566560997, 18.84387066167321478 ) ) ;
#55713 = ORIENTED_EDGE ( 'NONE', *, *, #15986, .F. ) ;
#55714 = EDGE_CURVE ( 'NONE', #36411, #4970, #24060, .T. ) ;
#55715 = ORIENTED_EDGE ( 'NONE', *, *, #3803, .F. ) ;
#55716 = CARTESIAN_POINT ( 'NONE',  ( 0.5988103564986357874, 34.44345003622203905, 33.58571500783070718 ) ) ;
#55717 = DIRECTION ( 'NONE',  ( 0.09722883295013594329, -0.9253344465965321897, -0.3664733496245589084 ) ) ;
#55718 = CARTESIAN_POINT ( 'NONE',  ( 0.6027444965799114707, -25.34513801577104530, -42.06141337198453556 ) ) ;
#55719 = LINE ( 'NONE', #12852, #38298 ) ;
#55720 = CARTESIAN_POINT ( 'NONE',  ( 0.6001305935487315502, 41.40054608060258801, 24.50730504006472543 ) ) ;
#55721 = ORIENTED_EDGE ( 'NONE', *, *, #35391, .T. ) ;
#55722 = CARTESIAN_POINT ( 'NONE',  ( 2.009741617377216460, 5.591155404095686343, 43.68344147237367991 ) ) ;
#55723 = EDGE_CURVE ( 'NONE', #4004, #55102, #45711, .T. ) ;
#55724 = LINE ( 'NONE', #60730, #29766 ) ;
#55725 = CARTESIAN_POINT ( 'NONE',  ( 0.8744876279028263033, 16.11801507201566253, 46.37412684372363714 ) ) ;
#55726 = VERTEX_POINT ( 'NONE', #41674 ) ;
#55727 = EDGE_CURVE ( 'NONE', #49695, #24433, #37506, .T. ) ;
#55728 = ORIENTED_EDGE ( 'NONE', *, *, #49242, .F. ) ;
#55729 = CARTESIAN_POINT ( 'NONE',  ( 0.6252788684277224007, 11.59566469080381523, 47.71776285150123442 ) ) ;
#55730 = CARTESIAN_POINT ( 'NONE',  ( 0.7044674535452954967, -35.85885898216653800, 33.55510326772964191 ) ) ;
#55731 = CARTESIAN_POINT ( 'NONE',  ( 0.5830081025819926488, -44.21080646010828019, 15.64086399560760832 ) ) ;
#55732 = VERTEX_POINT ( 'NONE', #9364 ) ;
#55733 = CARTESIAN_POINT ( 'NONE',  ( 4.553261556744873317, 17.57396821678933563, -40.25785894628420181 ) ) ;
#55734 = CARTESIAN_POINT ( 'NONE',  ( 3.559346040607745287, -33.97180693775380433, 27.91678016759760084 ) ) ;
#55735 = VECTOR ( 'NONE', #10278, 1000.000000000000000 ) ;
#55736 = ORIENTED_EDGE ( 'NONE', *, *, #400, .F. ) ;
#55738 = CARTESIAN_POINT ( 'NONE',  ( 0.5832367798473389042, 47.44985149964050208, 6.521664418777336714 ) ) ;
#55737 = CIRCLE ( 'NONE', #21725, 42.92674063221959813 ) ;
#55739 = AXIS2_PLACEMENT_3D ( 'NONE', #46276, #45354, #59414 ) ;
#55740 = CARTESIAN_POINT ( 'NONE',  ( 4.553261556744873317, -36.93702150832076825, -23.77385134801438937 ) ) ;
#55742 = EDGE_CURVE ( 'NONE', #22861, #56714, #33505, .T. ) ;
#55741 = CARTESIAN_POINT ( 'NONE',  ( 3.270143674763207553, 12.74832469035452576, 4.983712007628279927 ) ) ;
#55744 = CARTESIAN_POINT ( 'NONE',  ( 0.5786265663353196143, -41.83999636203335371, 23.32245830379013185 ) ) ;
#55743 = B_SPLINE_CURVE_WITH_KNOTS ( 'NONE', 3,
 ( #6737, #40322, #59377, #16485, #7056, #45325 ),
 .UNSPECIFIED., .F., .F.,
 ( 4, 2, 4 ),
 ( 1.964907063297894324E-17, 0.0002293319059085105775, 0.0004586638118170014767 ),
 .UNSPECIFIED. ) ;
#55745 = CARTESIAN_POINT ( 'NONE',  ( 2.359973842542475886, -43.44419283542142551, 7.123061386174991405 ) ) ;
#55746 = CARTESIAN_POINT ( 'NONE',  ( 3.270143674763207553, 13.60381564321234293, 1.514386915940642897 ) ) ;
#55747 = B_SPLINE_CURVE_WITH_KNOTS ( 'NONE', 3,
 ( #37797, #18666, #36861, #12743, #37168, #47175, #41871, #46558, #56546, #27130, #61547, #8946, #31837, #28057, #55930, #3298, #60617, #4222, #41556 ),
 .UNSPECIFIED., .F., .F.,
 ( 4, 3, 3, 3, 3, 3, 4 ),
 ( 1.250973872328959318E-17, 0.0002732106629380557099, 0.0004098138914053684389, 0.0005464171197651389918, 0.0006830203481512434061, 0.0008196235766963545256, 0.001011968216111132270 ),
 .UNSPECIFIED. ) ;
#55748 = ORIENTED_EDGE ( 'NONE', *, *, #14871, .T. ) ;
#55749 = CARTESIAN_POINT ( 'NONE',  ( 4.975801465491695552, 5.867614121011992532E-15, -47.91270532121795611 ) ) ;
#55750 = CARTESIAN_POINT ( 'NONE',  ( 5.896782393890504181, 8.471952691971306848, -18.24149403045190354 ) ) ;
#55751 = CARTESIAN_POINT ( 'NONE',  ( 0.1073791018717578927, -39.65380858626204486, -16.95003405440299460 ) ) ;
#55752 = FACE_OUTER_BOUND ( 'NONE', #18758, .T. ) ;
#55753 = CARTESIAN_POINT ( 'NONE',  ( 0.9730545539215883499, 36.90443313492362165, -21.89037132892396897 ) ) ;
#55754 = FACE_OUTER_BOUND ( 'NONE', #25457, .T. ) ;
#55755 = CARTESIAN_POINT ( 'NONE',  ( 0.5809828226811617480, 6.791453954331010401, -47.41188724015871969 ) ) ;
#55756 = DIRECTION ( 'NONE',  ( 0.07500201931887538753, -0.6023261099427925647, 0.7947187894968092969 ) ) ;
#55757 = VECTOR ( 'NONE', #40154, 1000.000000000000114 ) ;
#55758 = CARTESIAN_POINT ( 'NONE',  ( 0.5830082357119570347, 22.77652504489005025, -40.99343778969789298 ) ) ;
#55759 = CARTESIAN_POINT ( 'NONE',  ( 4.958415959904820092, 44.40884735405898454, 9.542443633919221568 ) ) ;
#55760 = CARTESIAN_POINT ( 'NONE',  ( 0.5839880159502353063, -29.12121614504435740, -38.02605095487705000 ) ) ;
#55761 = VERTEX_POINT ( 'NONE', #52269 ) ;
#55762 = EDGE_CURVE ( 'NONE', #20260, #38326, #57563, .T. ) ;
#55763 = CARTESIAN_POINT ( 'NONE',  ( 0.8744876279028306332, -38.80702141274064587, 30.07266432244707843 ) ) ;
#55764 = CARTESIAN_POINT ( 'NONE',  ( 0.9772918015221165877, 20.50340863875699426, 36.55060998044800158 ) ) ;
#55765 = FACE_OUTER_BOUND ( 'NONE', #45570, .T. ) ;
#55766 = CARTESIAN_POINT ( 'NONE',  ( -6.016489644550737204, 16.32089497094074559, -9.417787539062077329 ) ) ;
#55767 = ORIENTED_EDGE ( 'NONE', *, *, #22412, .T. ) ;
#55768 = ADVANCED_FACE ( 'NONE', ( #61659 ), #37935, .F. ) ;
#55769 = DIRECTION ( 'NONE',  ( 1.000000000000000000, 1.836909530733573776E-16, -1.925929944387235853E-32 ) ) ;
#55770 = CARTESIAN_POINT ( 'NONE',  ( 0.9785694773339246311, -41.79961263450124420, -3.021223149705917432 ) ) ;
#55771 = EDGE_CURVE ( 'NONE', #38633, #5563, #60650, .T. ) ;
#55772 = FILL_AREA_STYLE_COLOUR ( '', #46697 ) ;
#55773 = ORIENTED_EDGE ( 'NONE', *, *, #35173, .F. ) ;
#55774 = CARTESIAN_POINT ( 'NONE',  ( -6.079354080745853928, 19.25598488485689330, 0.001167186744194736829 ) ) ;
#55775 = CARTESIAN_POINT ( 'NONE',  ( 0.9741495583595148888, -41.34222751889821978, -11.48707840139629610 ) ) ;
#55776 = ADVANCED_FACE ( 'NONE', ( #37915 ), #27556, .T. ) ;
#55777 = CARTESIAN_POINT ( 'NONE',  ( 4.691466044806102076, -8.371234562541538082, -43.79545162262305524 ) ) ;
#55779 = ORIENTED_EDGE ( 'NONE', *, *, #11348, .T. ) ;
#55778 =( BOUNDED_SURFACE ( )  B_SPLINE_SURFACE ( 3, 1, ( 
 ( #23499, #603 ),
 ( #29127, #23817 ),
 ( #48537, #13946 ),
 ( #5595, #285 ) ),
 .UNSPECIFIED., .F., .F., .F. ) 
 B_SPLINE_SURFACE_WITH_KNOTS ( ( 4, 4 ),
 ( 2, 2 ),
 ( 0.000000000000000000, 1.000000000000000000 ),
 ( 0.000000000000000000, 1.000000000000000000 ),
 .UNSPECIFIED. ) 
 GEOMETRIC_REPRESENTATION_ITEM ( )  RATIONAL_B_SPLINE_SURFACE ( (
 ( 1.000000000000000000, 1.000000000000000000),
 ( 0.7282232189291694135, 0.9929344683865672927),
 ( 0.7282232189291694135, 0.9929344683865672927),
 ( 1.000000000000000000, 1.000000000000000000) ) ) 
 REPRESENTATION_ITEM ( '' )  SURFACE ( )  );
#55780 = EDGE_CURVE ( 'NONE', #50250, #58000, #22508, .T. ) ;
#55781 = CARTESIAN_POINT ( 'NONE',  ( 4.975801465491695552, 31.15993731089124097, -36.39623109580435312 ) ) ;
#55782 = AXIS2_PLACEMENT_3D ( 'NONE', #45752, #11613, #35429 ) ;
#55783 = CONICAL_SURFACE ( 'NONE', #32785, 42.92674063221959813, 1.485477209440487556 ) ;
#55784 = ORIENTED_EDGE ( 'NONE', *, *, #17358, .F. ) ;
#55785 = ORIENTED_EDGE ( 'NONE', *, *, #18590, .T. ) ;
#55786 = CARTESIAN_POINT ( 'NONE',  ( 0.1152339509894530906, 44.04726506203218150, 2.604060485150331505 ) ) ;
#55787 = ORIENTED_EDGE ( 'NONE', *, *, #27621, .T. ) ;
#55788 = CARTESIAN_POINT ( 'NONE',  ( 2.648799415243708655, 21.44335952302255777, -44.09875049994042229 ) ) ;
#55789 = ORIENTED_EDGE ( 'NONE', *, *, #57090, .T. ) ;
#55790 = CARTESIAN_POINT ( 'NONE',  ( -2.569797478183783568, 13.68441171582009019, 5.182550149005350271 ) ) ;
#55791 = EDGE_CURVE ( 'NONE', #57258, #6072, #43496, .T. ) ;
#55792 = CARTESIAN_POINT ( 'NONE',  ( 2.114184763582917181, 7.651710973661706259E-12, 44.03514965515166324 ) ) ;
#55793 = EDGE_CURVE ( 'NONE', #52998, #48557, #2283, .T. ) ;
#55794 = EDGE_LOOP ( 'NONE', ( #58997, #9428, #23469, #40735 ) ) ;
#55795 = CARTESIAN_POINT ( 'NONE',  ( 0.1145239942831223490, 14.93204977986375503, 41.52083055619605290 ) ) ;
#55796 = VECTOR ( 'NONE', #9929, 1000.000000000000000 ) ;
#55797 = DIRECTION ( 'NONE',  ( -1.000000000000000000, -0.000000000000000000, -0.000000000000000000 ) ) ;
#55798 = CARTESIAN_POINT ( 'NONE',  ( 50.00005079999999680, 12.80000000000000071, -3.000000000000000000 ) ) ;
#55799 = CARTESIAN_POINT ( 'NONE',  ( 0.7057020205115025480, 19.10543569325853142, -43.92641219669812358 ) ) ;
#55800 = ORIENTED_EDGE ( 'NONE', *, *, #45139, .F. ) ;
#55801 = DIRECTION ( 'NONE',  ( -1.000000000000000000, -0.000000000000000000, -0.000000000000000000 ) ) ;
#55802 = ORIENTED_EDGE ( 'NONE', *, *, #19064, .F. ) ;
#55803 = VECTOR ( 'NONE', #53497, 1000.000000000000114 ) ;
#55804 = CARTESIAN_POINT ( 'NONE',  ( 4.975610109902397937, -36.86873347511098586, -32.14258700041121131 ) ) ;
#55805 = EDGE_CURVE ( 'NONE', #33185, #44510, #41944, .T. ) ;
#55806 = VERTEX_POINT ( 'NONE', #23780 ) ;
#55807 = CARTESIAN_POINT ( 'NONE',  ( 0.1140933569871964842, -12.91770938709908734, 42.19102670325003146 ) ) ;
#55808 = CARTESIAN_POINT ( 'NONE',  ( 4.553261556744875094, 6.787618719203488915, 43.39893775135925580 ) ) ;
#55809 = ORIENTED_EDGE ( 'NONE', *, *, #8066, .F. ) ;
#55810 = CARTESIAN_POINT ( 'NONE',  ( 1.227938101723756947, -29.74462687941247552, 30.94118573761302926 ) ) ;
#55811 = CARTESIAN_POINT ( 'NONE',  ( 4.956653778116991482, 8.845409907521601056, -47.27023054223744225 ) ) ;
#55812 = CARTESIAN_POINT ( 'NONE',  ( 0.6029443449137434907, 28.05947194175915271, 40.30143387440406144 ) ) ;
#55813 = CARTESIAN_POINT ( 'NONE',  ( 0.5824936645240084143, -1.202945444167589750, -46.88060474544526102 ) ) ;
#55814 = VECTOR ( 'NONE', #14941, 1000.000000000000000 ) ;
#55815 = ORIENTED_EDGE ( 'NONE', *, *, #24619, .F. ) ;
#55816 = ORIENTED_EDGE ( 'NONE', *, *, #13547, .F. ) ;
#55817 = CARTESIAN_POINT ( 'NONE',  ( 4.958415959904820092, 34.02476434053166088, 30.09184881980370108 ) ) ;
#55818 = CARTESIAN_POINT ( 'NONE',  ( 0.9791128995231611620, -41.81475145202444565, 2.804281592776174836 ) ) ;
#55819 = CARTESIAN_POINT ( 'NONE',  ( 4.975801465491694664, -9.906103548668557579, 46.87746200127438101 ) ) ;
#55821 = EDGE_CURVE ( 'NONE', #18602, #8650, #6533, .T. ) ;
#55820 = CARTESIAN_POINT ( 'NONE',  ( 4.549368137175248350, 38.59302160394752690, -18.79584381673492288 ) ) ;
#55822 = CARTESIAN_POINT ( 'NONE',  ( 0.8557997880470599172, -29.88293891557496096, 37.44587306708088192 ) ) ;
#55823 = ADVANCED_FACE ( 'NONE', ( #58814 ), #44341, .F. ) ;
#55824 = CARTESIAN_POINT ( 'NONE',  ( 1.000110580585051423, 41.90446991591855408, 0.6579390836365230921 ) ) ;
#55825 = CARTESIAN_POINT ( 'NONE',  ( 4.967162193818130511, 0.000000000000000000, 0.000000000000000000 ) ) ;
#55826 = CIRCLE ( 'NONE', #13870, 48.91267123290010943 ) ;
#55827 = CARTESIAN_POINT ( 'NONE',  ( 0.8753041380234465318, 48.93739466471249955, 4.033575498629935474 ) ) ;
#55828 = CIRCLE ( 'NONE', #51848, 2.041999999999999815 ) ;
#55829 = CARTESIAN_POINT ( 'NONE',  ( 0.7242486021783801631, 43.87788672623142361, 22.03956711947809310 ) ) ;
#55830 = CARTESIAN_POINT ( 'NONE',  ( 0.9780106845699465534, 32.69455122756870935, 26.21826780096896314 ) ) ;
#55831 = CARTESIAN_POINT ( 'NONE',  ( 4.975610109902397937, 38.85236532789244279, 29.71435874397685595 ) ) ;
#55832 = B_SPLINE_CURVE_WITH_KNOTS ( 'NONE', 3,
 ( #43910, #16610, #25689, #48878, #39508, #1868 ),
 .UNSPECIFIED., .F., .F.,
 ( 4, 2, 4 ),
 ( 1.159750240187440271E-16, 0.0002448718616795903858, 0.0004897437233590648704 ),
 .UNSPECIFIED. ) ;
#55833 = CARTESIAN_POINT ( 'NONE',  ( 0.7948884756798502149, 16.14026985310537654, 46.37014485279392062 ) ) ;
#55834 = CARTESIAN_POINT ( 'NONE',  ( 5.894904586330512508, -19.93329511855189295, 2.682006297225661751 ) ) ;
#55835 = CARTESIAN_POINT ( 'NONE',  ( 0.8551540677456739292, -47.61725548905994287, 5.348818140990737824 ) ) ;
#55836 = CARTESIAN_POINT ( 'NONE',  ( 5.895596859100789899, -7.225383168025214076, 18.77024297359267990 ) ) ;
#55837 = CARTESIAN_POINT ( 'NONE',  ( 5.959828726073459926, 10.26672511661755927, -17.77343634131831607 ) ) ;
#55838 = CARTESIAN_POINT ( 'NONE',  ( 0.8560838555295158248, -13.02223058219810881, -45.06433561859972059 ) ) ;
#55839 = CARTESIAN_POINT ( 'NONE',  ( 0.5998501479064699549, 46.33007877220738635, -12.95623334615453892 ) ) ;
#55841 = VERTEX_POINT ( 'NONE', #25317 ) ;
#55840 = LINE ( 'NONE', #47088, #13347 ) ;
#55842 = ORIENTED_EDGE ( 'NONE', *, *, #30133, .T. ) ;
#55843 = VECTOR ( 'NONE', #57654, 1000.000000000000114 ) ;
#55844 = DIRECTION ( 'NONE',  ( 0.000000000000000000, 0.000000000000000000, 1.000000000000000000 ) ) ;
#55845 = CARTESIAN_POINT ( 'NONE',  ( 0.8557997880470697982, -19.17299735371977221, -43.90420959842202109 ) ) ;
#55846 = CARTESIAN_POINT ( 'NONE',  ( 0.8751705887134423323, -46.67919521768896374, 11.58504748649118810 ) ) ;
#55847 = ORIENTED_EDGE ( 'NONE', *, *, #27446, .F. ) ;
#55848 = B_SPLINE_CURVE_WITH_KNOTS ( 'NONE', 3,
 ( #40595, #7331, #56807, #51186, #61802, #56195 ),
 .UNSPECIFIED., .F., .F.,
 ( 4, 2, 4 ),
 ( 1.274743298368305687E-16, 0.0002450741128632353779, 0.0004901482257263433621 ),
 .UNSPECIFIED. ) ;
#55849 = EDGE_CURVE ( 'NONE', #58618, #5670, #3072, .T. ) ;
#55850 = ORIENTED_EDGE ( 'NONE', *, *, #22208, .F. ) ;
#55851 = CARTESIAN_POINT ( 'NONE',  ( 0.5839879882012687373, -33.86754218494321123, 33.86758487442388343 ) ) ;
#55852 = CARTESIAN_POINT ( 'NONE',  ( 0.9722240750034557566, 5.023189755349555696, -42.61332880321398164 ) ) ;
#55853 = EDGE_CURVE ( 'NONE', #41784, #32640, #27719, .T. ) ;
#55854 = ORIENTED_EDGE ( 'NONE', *, *, #56222, .F. ) ;
#55855 = VERTEX_POINT ( 'NONE', #30320 ) ;
#55856 = CARTESIAN_POINT ( 'NONE',  ( 1.000110580585049647, -37.69726589122901572, 18.31211694747177177 ) ) ;
#55857 = EDGE_CURVE ( 'NONE', #18232, #2143, #40504, .T. ) ;
#55858 = EDGE_CURVE ( 'NONE', #58483, #7638, #59882, .T. ) ;
#55859 = CARTESIAN_POINT ( 'NONE',  ( 5.958863334805807099, -18.96276366205788122, -7.855954700275556313 ) ) ;
#55860 = CARTESIAN_POINT ( 'NONE',  ( 0.8744876279028306332, 49.04340454744548339, 2.257104511336577968 ) ) ;
#55861 = EDGE_CURVE ( 'NONE', #17733, #34547, #10000, .T. ) ;
#55862 = ORIENTED_EDGE ( 'NONE', *, *, #44810, .T. ) ;
#55863 = CARTESIAN_POINT ( 'NONE',  ( 0.9762797500689124330, 14.58899758184639595, 39.28722355604407568 ) ) ;
#55864 = CARTESIAN_POINT ( 'NONE',  ( 4.975610109902397937, -48.77192499014914517, 3.707929326866768349 ) ) ;
#55865 = EDGE_CURVE ( 'NONE', #8159, #42198, #22589, .T. ) ;
#55866 = B_SPLINE_CURVE_WITH_KNOTS ( 'NONE', 3,
 ( #60693, #847, #6138, #49085, #53454, #52537 ),
 .UNSPECIFIED., .F., .F.,
 ( 4, 2, 4 ),
 ( 9.898949898072313973E-18, 0.0002448709889506559098, 0.0004897419779013018450 ),
 .UNSPECIFIED. ) ;
#55867 = CARTESIAN_POINT ( 'NONE',  ( 0.1100247026804066219, 21.41511734445746740, 37.43141430507378686 ) ) ;
#55868 = ORIENTED_EDGE ( 'NONE', *, *, #7352, .T. ) ;
#55869 = CIRCLE ( 'NONE', #12887, 48.09070567114147110 ) ;
#55870 = ORIENTED_EDGE ( 'NONE', *, *, #2108, .F. ) ;
#55871 = CARTESIAN_POINT ( 'NONE',  ( 0.8551540677456739292, -19.17641535420883869, 43.91216198251533598 ) ) ;
#55872 = CIRCLE ( 'NONE', #37942, 48.91267123290010943 ) ;
#55873 = EDGE_LOOP ( 'NONE', ( #38376, #32937, #55103, #38804 ) ) ;
#55874 = CARTESIAN_POINT ( 'NONE',  ( 0.5997462898726536595, -48.63480578518805686, 6.797594896825438049 ) ) ;
#55875 = CARTESIAN_POINT ( 'NONE',  ( 1.154321485836933725, 17.18284940416451079, 39.32643515542041257 ) ) ;
#55876 = CARTESIAN_POINT ( 'NONE',  ( 0.5806925824938499181, -20.23436166722466467, 42.30594485723624132 ) ) ;
#55877 = CARTESIAN_POINT ( 'NONE',  ( 0.6252788684277210685, 16.31351639750482718, -46.31752922946136408 ) ) ;
#55878 = CARTESIAN_POINT ( 'NONE',  ( 0.8560838555295223751, -20.57050347530454104, -42.15717282805163535 ) ) ;
#55879 = ORIENTED_EDGE ( 'NONE', *, *, #35007, .T. ) ;
#55880 = FACE_OUTER_BOUND ( 'NONE', #33261, .T. ) ;
#55881 = CARTESIAN_POINT ( 'NONE',  ( 1.000110580585054532, 32.47884455641464285, 26.48664076571725445 ) ) ;
#55882 =( BOUNDED_SURFACE ( )  B_SPLINE_SURFACE ( 3, 1, ( 
 ( #38150, #57196 ),
 ( #52830, #14955 ),
 ( #14330, #14640 ),
 ( #33437, #52514 ) ),
 .UNSPECIFIED., .F., .F., .F. ) 
 B_SPLINE_SURFACE_WITH_KNOTS ( ( 4, 4 ),
 ( 2, 2 ),
 ( 0.000000000000000000, 1.000000000000000000 ),
 ( 0.000000000000000000, 1.000000000000000000 ),
 .UNSPECIFIED. ) 
 GEOMETRIC_REPRESENTATION_ITEM ( )  RATIONAL_B_SPLINE_SURFACE ( (
 ( 1.000000000000000000, 1.000000000000000000),
 ( 0.7282232189291693025, 0.9929344683865674037),
 ( 0.7282232189291693025, 0.9929344683865674037),
 ( 1.000000000000000000, 1.000000000000000000) ) ) 
 REPRESENTATION_ITEM ( '' )  SURFACE ( )  );
#55883 = CARTESIAN_POINT ( 'NONE',  ( 5.895596859100789899, -18.51832497669317945, -7.848555489392246010 ) ) ;
#55884 = ORIENTED_EDGE ( 'NONE', *, *, #32868, .T. ) ;
#55885 = DIRECTION ( 'NONE',  ( -1.000000000000000000, -1.836909530733573776E-16, 1.361838123766442686E-32 ) ) ;
#55886 = CYLINDRICAL_SURFACE ( 'NONE', #25706, 2.698940690764988215 ) ;
#55887 = CARTESIAN_POINT ( 'NONE',  ( 0.5998501479064699549, 34.38546660123250120, 33.64490850298857083 ) ) ;
#55888 = CARTESIAN_POINT ( 'NONE',  ( 4.967162193818129623, 32.68434214048168940, 28.07411493385305334 ) ) ;
#55889 = AXIS2_PLACEMENT_3D ( 'NONE', #1873, #45141, #11291 ) ;
#55890 = ORIENTED_EDGE ( 'NONE', *, *, #25179, .T. ) ;
#55891 = CARTESIAN_POINT ( 'NONE',  ( 4.694002226626920127, 36.74006825548320876, 26.98985283451114014 ) ) ;
#55892 = CARTESIAN_POINT ( 'NONE',  ( -6.016104459813371719, 18.84322058118302579, -0.005335450885131768489 ) ) ;
#55893 = CARTESIAN_POINT ( 'NONE',  ( 1.231276596079887264, -13.22565419921979313, -39.77887431816952102 ) ) ;
#55894 = DIRECTION ( 'NONE',  ( 0.07906939808003037029, 0.5295738273858020539, 0.8445706552060724404 ) ) ;
#55896 = CARTESIAN_POINT ( 'NONE',  ( 0.1119898979215351170, 10.36499891643169846, 42.88972028020465643 ) ) ;
#55895 = PRODUCT_DEFINITION_FORMATION_WITH_SPECIFIED_SOURCE ( 'ANY', '', #13314, .NOT_KNOWN. ) ;
#55897 =( BOUNDED_SURFACE ( )  B_SPLINE_SURFACE ( 3, 1, ( 
 ( #26770, #41202 ),
 ( #55563, #50877 ),
 ( #3251, #17685 ),
 ( #13007, #10442 ) ),
 .UNSPECIFIED., .F., .F., .F. ) 
 B_SPLINE_SURFACE_WITH_KNOTS ( ( 4, 4 ),
 ( 2, 2 ),
 ( 0.000000000000000000, 1.000000000000000000 ),
 ( 0.000000000000000000, 1.000000000000000000 ),
 .UNSPECIFIED. ) 
 GEOMETRIC_REPRESENTATION_ITEM ( )  RATIONAL_B_SPLINE_SURFACE ( (
 ( 1.000000000000000000, 1.000000000000000000),
 ( 0.7211978278499970862, 0.9934217856018976445),
 ( 0.7211978278499970862, 0.9934217856018976445),
 ( 1.000000000000000000, 1.000000000000000000) ) ) 
 REPRESENTATION_ITEM ( '' )  SURFACE ( )  );
#55898 = CARTESIAN_POINT ( 'NONE',  ( 1.231276596079887264, -23.26513148155214594, -34.87134107206314582 ) ) ;
#55899 = ADVANCED_FACE ( 'NONE', ( #43527 ), #27546, .T. ) ;
#55900 = CARTESIAN_POINT ( 'NONE',  ( 4.834790513006553603, -27.40943972694875441, 38.48781566650860242 ) ) ;
#55901 = CARTESIAN_POINT ( 'NONE',  ( 0.5806925824938499181, -45.84420715090598009, -9.875780123533834498 ) ) ;
#55902 = CARTESIAN_POINT ( 'NONE',  ( 5.917102823773431552, -18.51940219202235838, 7.843561722958504845 ) ) ;
#55903 = CARTESIAN_POINT ( 'NONE',  ( 0.8557997880470599172, -47.37054680076701629, -7.156447707086194043 ) ) ;
#55904 = VERTEX_POINT ( 'NONE', #5264 ) ;
#55905 = CARTESIAN_POINT ( 'NONE',  ( -6.057079549204054558, 15.42772006041527355, 11.52461213391576678 ) ) ;
#55906 = DIRECTION ( 'NONE',  ( 0.000000000000000000, 0.000000000000000000, -1.000000000000000000 ) ) ;
#55907 = CARTESIAN_POINT ( 'NONE',  ( 5.960721111146673579, 5.306302591836580262, -19.82781442290492890 ) ) ;
#55908 = CARTESIAN_POINT ( 'NONE',  ( 0.6008123274975392114, -39.09350553450490651, -29.71956218018853590 ) ) ;
#55909 = CARTESIAN_POINT ( 'NONE',  ( 1.657374760986086715, -23.88755842655104900, -37.01722571547405494 ) ) ;
#55910 = CARTESIAN_POINT ( 'NONE',  ( 0.9730545539215892381, 26.52009130076819687, -33.73144377768529978 ) ) ;
#55911 = CARTESIAN_POINT ( 'NONE',  ( 0.8744876279028306332, 10.05549467470575209, -48.05452192277493850 ) ) ;
#55912 = FACE_OUTER_BOUND ( 'NONE', #42880, .T. ) ;
#55913 = CARTESIAN_POINT ( 'NONE',  ( 0.6024113833632039894, -1.791547436567632490, 49.07476160801390108 ) ) ;
#55915 = ORIENTED_EDGE ( 'NONE', *, *, #28397, .F. ) ;
#55914 = CARTESIAN_POINT ( 'NONE',  ( 4.962356264823602814, 42.01891079680549979, 2.376285612557970772 ) ) ;
#55916 = EDGE_LOOP ( 'NONE', ( #620, #18956 ) ) ;
#55917 = AXIS2_PLACEMENT_3D ( 'NONE', #1077, #15819, #2848 ) ;
#55918 = CARTESIAN_POINT ( 'NONE',  ( 4.226256110419178924, -19.95723175456961229, -39.14761998744732097 ) ) ;
#55919 = DIRECTION ( 'NONE',  ( 0.000000000000000000, 0.000000000000000000, 1.000000000000000000 ) ) ;
#55920 = CARTESIAN_POINT ( 'NONE',  ( 4.691466044806102076, -2.583163953528165635, -44.51344083442437949 ) ) ;
#55921 = B_SPLINE_CURVE_WITH_KNOTS ( 'NONE', 3,
 ( #55989, #37227, #13109, #46622 ),
 .UNSPECIFIED., .F., .F.,
 ( 4, 4 ),
 ( 0.000000000000000000, 0.005013413432710150247 ),
 .UNSPECIFIED. ) ;
#55922 = ORIENTED_EDGE ( 'NONE', *, *, #37789, .T. ) ;
#55923 = CARTESIAN_POINT ( 'NONE',  ( 0.7245667037590732829, -38.65590879674368807, -28.62745028382802914 ) ) ;
#55924 = CARTESIAN_POINT ( 'NONE',  ( 0.5824936645240094135, -46.02748468922020919, 8.983809449443411310 ) ) ;
#55925 = CARTESIAN_POINT ( 'NONE',  ( -6.001507490154110336, -13.33564355450099015, -13.31361390284173929 ) ) ;
#55926 = EDGE_CURVE ( 'NONE', #33035, #41260, #32279, .T. ) ;
#55927 = ORIENTED_EDGE ( 'NONE', *, *, #61934, .T. ) ;
#55928 = VERTEX_POINT ( 'NONE', #54416 ) ;
#55929 = EDGE_CURVE ( 'NONE', #29392, #6786, #9076, .T. ) ;
#55930 = CARTESIAN_POINT ( 'NONE',  ( 0.9783242366443551941, 25.07469261982136288, -33.57967063906372829 ) ) ;
#55931 = ADVANCED_FACE ( 'NONE', ( #56200 ), #18347, .F. ) ;
#55932 = VECTOR ( 'NONE', #2928, 1000.000000000000114 ) ;
#55933 = CARTESIAN_POINT ( 'NONE',  ( 0.6001305935487315502, 46.33281397023046111, 12.95698906763826841 ) ) ;
#55934 = CARTESIAN_POINT ( 'NONE',  ( 0.6009452777970412107, 41.87890062806003755, 23.67489783211108900 ) ) ;
#55935 = EDGE_CURVE ( 'NONE', #41374, #37381, #46564, .T. ) ;
#55936 = CARTESIAN_POINT ( 'NONE',  ( 2.185380717157383135, -44.00852750110943390, 1.438509732776827477 ) ) ;
#55937 = CARTESIAN_POINT ( 'NONE',  ( 0.6026777506516367566, 49.01745359636671395, 2.972479363301738342 ) ) ;
#55938 = CARTESIAN_POINT ( 'NONE',  ( 0.6252788684277218456, -24.86667677503463736, 42.34492552053455228 ) ) ;
#55939 = VERTEX_POINT ( 'NONE', #26236 ) ;
#55940 = CARTESIAN_POINT ( 'NONE',  ( 2.281351352603288696, -34.83869092251583766, 32.98025003937404875 ) ) ;
#55941 = EDGE_CURVE ( 'NONE', #30590, #41729, #40077, .T. ) ;
#55942 =( NAMED_UNIT ( * ) PLANE_ANGLE_UNIT ( ) SI_UNIT ( $, .RADIAN. ) );
#55943 = VERTEX_POINT ( 'NONE', #40684 ) ;
#55944 = CARTESIAN_POINT ( 'NONE',  ( 4.956445790443994248, 24.88142650099509723, 39.98065363916922621 ) ) ;
#55945 = CARTESIAN_POINT ( 'NONE',  ( 0.8551540677456739292, -47.90804413217340141, -0.9122407826480745108 ) ) ;
#55946 = CARTESIAN_POINT ( 'NONE',  ( 0.9780303403264766215, 3.872540855671210647, -41.72940259237177685 ) ) ;
#55947 = CARTESIAN_POINT ( 'NONE',  ( 4.967162193818130511, -13.42934394584192148, 40.93989340068605998 ) ) ;
#55948 = EDGE_CURVE ( 'NONE', #52878, #7613, #16237, .T. ) ;
#55949 = ORIENTED_EDGE ( 'NONE', *, *, #19763, .F. ) ;
#55950 = ORIENTED_EDGE ( 'NONE', *, *, #58901, .T. ) ;
#55951 = CARTESIAN_POINT ( 'NONE',  ( 0.5809828226811553087, -33.48000389720640868, 34.25055090842140970 ) ) ;
#55952 = CARTESIAN_POINT ( 'NONE',  ( 0.5832367798473397924, 41.34221369670682122, 24.18350431151176139 ) ) ;
#55953 = ORIENTED_EDGE ( 'NONE', *, *, #41997, .T. ) ;
#55954 = CARTESIAN_POINT ( 'NONE',  ( 0.8560838555295158248, 17.70877843982841782, -43.43698884880027578 ) ) ;
#55955 = VECTOR ( 'NONE', #61464, 999.9999999999998863 ) ;
#55956 = ORIENTED_EDGE ( 'NONE', *, *, #57332, .T. ) ;
#55957 = FACE_OUTER_BOUND ( 'NONE', #35570, .T. ) ;
#55958 = VERTEX_POINT ( 'NONE', #18326 ) ;
#55959 = CARTESIAN_POINT ( 'NONE',  ( -6.015611763856276717, -18.20278301740933102, -4.870987357968367348 ) ) ;
#55960 = CARTESIAN_POINT ( 'NONE',  ( 0.6021447746440204973, -48.73699394290184017, -6.020511647529366073 ) ) ;
#55961 = VECTOR ( 'NONE', #54304, 1000.000000000000000 ) ;
#55962 = CARTESIAN_POINT ( 'NONE',  ( 0.1155031312995260795, -43.78313126285997470, 5.475312717186315403 ) ) ;
#55963 = ORIENTED_EDGE ( 'NONE', *, *, #38363, .F. ) ;
#55964 = CARTESIAN_POINT ( 'NONE',  ( 0.1145239942831223490, -27.25490258565300650, -34.70037126244096726 ) ) ;
#55965 = CARTESIAN_POINT ( 'NONE',  ( 0.6039202388192952409, 11.09723268158311171, -47.83738224087722557 ) ) ;
#55966 = CARTESIAN_POINT ( 'NONE',  ( 0.5817217712918330008, -42.05893918154934141, 20.74320584989474980 ) ) ;
#55967 = ORIENTED_EDGE ( 'NONE', *, *, #16129, .T. ) ;
#55968 = CARTESIAN_POINT ( 'NONE',  ( 0.5997462898726536595, 49.03735788587803768, -2.624721264558313560 ) ) ;
#55969 = CARTESIAN_POINT ( 'NONE',  ( 1.231276596079881935, -39.31472542100197387, -14.54747868495734053 ) ) ;
#55970 = CARTESIAN_POINT ( 'NONE',  ( 3.376099380956838925, -8.298464850405457227, -10.52824129466323910 ) ) ;
#55971 = FACE_OUTER_BOUND ( 'NONE', #28898, .T. ) ;
#55972 = EDGE_CURVE ( 'NONE', #14312, #23007, #18078, .T. ) ;
#55973 = CARTESIAN_POINT ( 'NONE',  ( 0.8751705887134423323, -11.58504748649167837, -46.67919521768883584 ) ) ;
#55974 = ORIENTED_EDGE ( 'NONE', *, *, #11207, .T. ) ;
#55975 = CARTESIAN_POINT ( 'NONE',  ( 0.1104177457020373010, 37.34442418285502896, -21.56646482560092792 ) ) ;
#55976 = DIRECTION ( 'NONE',  ( -0.9848077530122077983, -0.1736481776669315802, 5.551115123125782702E-17 ) ) ;
#55977 = CIRCLE ( 'NONE', #51010, 48.91267123290010943 ) ;
#55978 = ORIENTED_EDGE ( 'NONE', *, *, #33698, .F. ) ;
#55979 = DIRECTION ( 'NONE',  ( 0.000000000000000000, -1.000000000000000000, 0.000000000000000000 ) ) ;
#55980 = CARTESIAN_POINT ( 'NONE',  ( 0.9762797500689124330, -27.44172181261435739, 31.67454323498272117 ) ) ;
#55981 = DIRECTION ( 'NONE',  ( -0.07500201931887526263, 0.9127009170568879393, -0.4016861126571428797 ) ) ;
#55982 = CARTESIAN_POINT ( 'NONE',  ( 0.9758171775293917882, 5.594812732687712398, -42.54217005300505861 ) ) ;
#55983 = B_SPLINE_CURVE_WITH_KNOTS ( 'NONE', 3,
 ( #32497, #22169, #51271, #60980 ),
 .UNSPECIFIED., .F., .F.,
 ( 4, 4 ),
 ( 8.673617379884035472E-19, 0.004050076154993000749 ),
 .UNSPECIFIED. ) ;
#55984 = CARTESIAN_POINT ( 'NONE',  ( 4.303969348037258058, 27.54579249306266675, -39.44373910178582321 ) ) ;
#55985 = CARTESIAN_POINT ( 'NONE',  ( 4.322998006666165516, 47.94177812210861589, 2.120302895116446873 ) ) ;
#55986 = CARTESIAN_POINT ( 'NONE',  ( 0.6028777368367060907, 4.628771803277713204, 48.88879524905737384 ) ) ;
#55987 = CARTESIAN_POINT ( 'NONE',  ( 1.088908134280555107, -42.64123480278973943, -4.826714665689302741 ) ) ;
#55988 = CARTESIAN_POINT ( 'NONE',  ( 0.9756950546413932779, -39.60512406639357863, 16.50968749804426849 ) ) ;
#55989 = CARTESIAN_POINT ( 'NONE',  ( 4.553261556744873317, -4.442710778081946366, -43.70128015019640344 ) ) ;
#55990 = B_SPLINE_CURVE_WITH_KNOTS ( 'NONE', 3,
 ( #54588, #24884, #1060, #49596 ),
 .UNSPECIFIED., .F., .F.,
 ( 4, 4 ),
 ( 0.000000000000000000, 0.005004741218457314789 ),
 .UNSPECIFIED. ) ;
#55991 = CARTESIAN_POINT ( 'NONE',  ( 0.5997462898726536595, 44.46857747280011353, 20.83500054451363326 ) ) ;
#55992 = CARTESIAN_POINT ( 'NONE',  ( 1.091591847532195958, 8.955707924048176949, 40.94574808859866977 ) ) ;
#55993 = CARTESIAN_POINT ( 'NONE',  ( 5.981074661064941900, -10.26976685693810865, -17.77058762078874565 ) ) ;
#55994 = CARTESIAN_POINT ( 'NONE',  ( 5.838029081930957709, -10.93035914537738584, 45.95206531926487514 ) ) ;
#55995 = DIRECTION ( 'NONE',  ( 1.000000000000000000, 1.836970198721027962E-16, -2.033782021272921061E-31 ) ) ;
#55996 = CARTESIAN_POINT ( 'NONE',  ( 0.8744876279028263033, 28.81338721758142896, -39.75095932715596092 ) ) ;
#55997 = CARTESIAN_POINT ( 'NONE',  ( 3.661921753702011451, -26.87747736193279025, -38.60352748768983844 ) ) ;
#55998 = FACE_OUTER_BOUND ( 'NONE', #2225, .T. ) ;
#55999 =( BOUNDED_SURFACE ( )  B_SPLINE_SURFACE ( 3, 1, ( 
 ( #12183, #8367 ),
 ( #31268, #26250 ),
 ( #17180, #2743 ),
 ( #46310, #50367 ) ),
 .UNSPECIFIED., .F., .F., .F. ) 
 B_SPLINE_SURFACE_WITH_KNOTS ( ( 4, 4 ),
 ( 2, 2 ),
 ( 0.000000000000000000, 1.000000000000000000 ),
 ( 0.000000000000000000, 1.000000000000000000 ),
 .UNSPECIFIED. ) 
 GEOMETRIC_REPRESENTATION_ITEM ( )  RATIONAL_B_SPLINE_SURFACE ( (
 ( 1.000000000000000000, 1.000000000000000000),
 ( 0.7282232189291693025, 0.9929344683865674037),
 ( 0.7282232189291693025, 0.9929344683865674037),
 ( 1.000000000000000000, 1.000000000000000000) ) ) 
 REPRESENTATION_ITEM ( '' )  SURFACE ( )  );
#56000 = ORIENTED_EDGE ( 'NONE', *, *, #30649, .T. ) ;
#56001 = EDGE_CURVE ( 'NONE', #516, #27868, #51536, .T. ) ;
#56002 = DIRECTION ( 'NONE',  ( 0.07836865515943411409, 0.9179910502197331512, 0.3887811538706230086 ) ) ;
#56003 = CIRCLE ( 'NONE', #4974, 12.49999999999999822 ) ;
#56004 = CARTESIAN_POINT ( 'NONE',  ( 3.050102900204245682, -32.83519750374883728, -29.27925979371518750 ) ) ;
#56005 = CARTESIAN_POINT ( 'NONE',  ( 3.559346040607745287, 28.00880476468896774, -33.89597523594098050 ) ) ;
#56006 = CARTESIAN_POINT ( 'NONE',  ( 3.240649175237396928, -19.46330462187410504, 39.45180212099042905 ) ) ;
#56007 = ORIENTED_EDGE ( 'NONE', *, *, #37617, .F. ) ;
#56008 = ADVANCED_FACE ( 'NONE', ( #50353 ), #11196, .F. ) ;
#56009 = DIRECTION ( 'NONE',  ( 0.000000000000000000, 0.000000000000000000, 1.000000000000000000 ) ) ;
#56010 = B_SPLINE_CURVE_WITH_KNOTS ( 'NONE', 3,
 ( #38896, #29459, #53559, #10676 ),
 .UNSPECIFIED., .F., .F.,
 ( 4, 4 ),
 ( 0.000000000000000000, 0.005014147105413699519 ),
 .UNSPECIFIED. ) ;
#56011 = CARTESIAN_POINT ( 'NONE',  ( 4.291220156522059348, -37.58001468972560843, -28.41005971879863168 ) ) ;
#56012 = ORIENTED_EDGE ( 'NONE', *, *, #17487, .F. ) ;
#56013 = CARTESIAN_POINT ( 'NONE',  ( 1.834102595619085729, -26.43261434248111286, 35.23513365774772410 ) ) ;
#56014 = ORIENTED_EDGE ( 'NONE', *, *, #9346, .F. ) ;
#56015 = DIRECTION ( 'NONE',  ( -1.000000000000000000, -1.836909530733554547E-16, -1.836909530733573529E-16 ) ) ;
#56016 = AXIS2_PLACEMENT_3D ( 'NONE', #12880, #7842, #2520 ) ;
#56017 = CARTESIAN_POINT ( 'NONE',  ( 0.7048096507298635682, -46.68221792389232405, -11.63498350884320232 ) ) ;
#56018 = EDGE_LOOP ( 'NONE', ( #20615, #59646, #29511, #27227 ) ) ;
#56019 = CARTESIAN_POINT ( 'NONE',  ( -6.072942160501519027, -1.863502906426436789, 19.16589468839794463 ) ) ;
#56020 = CARTESIAN_POINT ( 'NONE',  ( 0.5819845079324652559, -28.79567599618788520, 38.27312975753802959 ) ) ;
#56021 = EDGE_LOOP ( 'NONE', ( #51949, #55391, #7935, #48463 ) ) ;
#56022 = LINE ( 'NONE', #19372, #55735 ) ;
#56023 = CARTESIAN_POINT ( 'NONE',  ( 0.1103878639767399555, -26.29099398937423615, -34.18336104662730435 ) ) ;
#56024 = EDGE_CURVE ( 'NONE', #8960, #3302, #26268, .T. ) ;
#56025 = ORIENTED_EDGE ( 'NONE', *, *, #16371, .T. ) ;
#56026 = CARTESIAN_POINT ( 'NONE',  ( 0.8751705887134553219, -42.09020928323357680, -23.27176129838411001 ) ) ;
#56027 = ORIENTED_EDGE ( 'NONE', *, *, #48464, .T. ) ;
#56028 = CARTESIAN_POINT ( 'NONE',  ( 5.959547316686252039, -20.35048796920738923, 2.675599016784190098 ) ) ;
#56029 = ORIENTED_EDGE ( 'NONE', *, *, #26720, .T. ) ;
#56030 = EDGE_LOOP ( 'NONE', ( #5175, #12525, #18039, #45959 ) ) ;
#56031 = CARTESIAN_POINT ( 'NONE',  ( 0.6024113833632039894, -42.68099031389036213, -24.28734104274209926 ) ) ;
#56032 = CARTESIAN_POINT ( 'NONE',  ( 1.000110580585049869, -7.618717594574525798, 41.21131671017104026 ) ) ;
#56033 = CARTESIAN_POINT ( 'NONE',  ( 3.680882792899938138, -4.423598386734752808, 47.77138407787914787 ) ) ;
#56034 = CARTESIAN_POINT ( 'NONE',  ( 4.553261556744873317, 42.43205150231990075, -11.36048287389704292 ) ) ;
#56035 = CARTESIAN_POINT ( 'NONE',  ( -6.015611763856276717, -16.32183393015590056, -9.416239407363475422 ) ) ;
#56036 = ORIENTED_EDGE ( 'NONE', *, *, #31758, .T. ) ;
#56037 = CARTESIAN_POINT ( 'NONE',  ( 1.112077966505211402, 5.276550529686780067, 43.76286484722197656 ) ) ;
#56038 = CARTESIAN_POINT ( 'NONE',  ( 0.9762797500689124330, -18.09842611962814019, 37.79909730639167265 ) ) ;
#56039 = CARTESIAN_POINT ( 'NONE',  ( 0.5848930533535030563, -46.80349522319539091, 2.950579143131832005 ) ) ;
#56040 = ORIENTED_EDGE ( 'NONE', *, *, #13183, .F. ) ;
#56041 = VERTEX_POINT ( 'NONE', #5417 ) ;
#56042 = CARTESIAN_POINT ( 'NONE',  ( 0.6041374136657475802, -48.10739871142803992, -0.1745662470642904973 ) ) ;
#56043 = CARTESIAN_POINT ( 'NONE',  ( -6.057079549204054558, -6.658663215491944065, -18.06912934489077216 ) ) ;
#56044 = FACE_OUTER_BOUND ( 'NONE', #37248, .T. ) ;
#56045 = EDGE_CURVE ( 'NONE', #34317, #17061, #52423, .T. ) ;
#56046 = CARTESIAN_POINT ( 'NONE',  ( 0.1095718737110178836, -34.36877422441016705, 26.04820588677135618 ) ) ;
#56047 = CARTESIAN_POINT ( 'NONE',  ( 4.226256110419179812, -33.72520557204028790, 28.16802724918466083 ) ) ;
#56048 = CONICAL_SURFACE ( 'NONE', #2021, 2.060000000000000941, 0.9599310885968777018 ) ;
#56049 = EDGE_LOOP ( 'NONE', ( #54488, #27416, #6299, #54563 ) ) ;
#56050 = CARTESIAN_POINT ( 'NONE',  ( 0.5838002273316443835, 47.46823345111868520, 6.386683873060672312 ) ) ;
#56051 = CARTESIAN_POINT ( 'NONE',  ( 1.000433927950262758, -17.04159546744087450, 38.28841471746964942 ) ) ;
#56052 = CARTESIAN_POINT ( 'NONE',  ( 0.6001305935487315502, 37.84751346122814653, 29.70149728382449794 ) ) ;
#56053 = CARTESIAN_POINT ( 'NONE',  ( -1.600000000000000089, -11.64055411052240352, -1.199999999999999956 ) ) ;
#56054 = CARTESIAN_POINT ( 'NONE',  ( 2.879087469061463178, -41.40359735493927928, -14.89442187039979260 ) ) ;
#56055 = EDGE_CURVE ( 'NONE', #32395, #39423, #39725, .T. ) ;
#56056 = B_SPLINE_CURVE_WITH_KNOTS ( 'NONE', 3,
 ( #34470, #42636, #28507, #53539, #614, #43568 ),
 .UNSPECIFIED., .F., .F.,
 ( 4, 2, 4 ),
 ( 2.197015137584158753E-17, 0.0002293755540694321316, 0.0004587511081388422540 ),
 .UNSPECIFIED. ) ;
#56057 = CARTESIAN_POINT ( 'NONE',  ( 1.139999999999998570, 0.000000000000000000, 0.000000000000000000 ) ) ;
#56058 = CONICAL_SURFACE ( 'NONE', #24100, 43.92652462719577500, 1.486293639869522343 ) ;
#56059 = ORIENTED_EDGE ( 'NONE', *, *, #2958, .F. ) ;
#56060 = LINE ( 'NONE', #46086, #7689 ) ;
#56061 = CARTESIAN_POINT ( 'NONE',  ( 0.09136607875274982415, 12.80000000000000071, -3.000000000000000000 ) ) ;
#56062 = EDGE_CURVE ( 'NONE', #15046, #51445, #59094, .T. ) ;
#56063 = CARTESIAN_POINT ( 'NONE',  ( 0.5998501479064699549, 46.33007877220738635, -12.95623334615453892 ) ) ;
#56064 = CARTESIAN_POINT ( 'NONE',  ( 0.7044674535452954967, 3.876803250505699072, 48.95684956538539012 ) ) ;
#56065 = CARTESIAN_POINT ( 'NONE',  ( 5.960221823109900008, 18.96108896995714943, -7.859839668735016716 ) ) ;
#56066 = CARTESIAN_POINT ( 'NONE',  ( 0.6026112563231248442, -49.10713455106970571, -0.1741582250239009644 ) ) ;
#56067 = B_SPLINE_CURVE_WITH_KNOTS ( 'NONE', 3,
 ( #41550, #46246, #2993, #11807, #55606, #2371 ),
 .UNSPECIFIED., .F., .F.,
 ( 4, 2, 4 ),
 ( 2.611104600503255956E-18, 0.0002447193893791690575, 0.0004894387787583355130 ),
 .UNSPECIFIED. ) ;
#56068 = CARTESIAN_POINT ( 'NONE',  ( 0.7056313189692711152, 37.32477945609016956, 28.40087115762097625 ) ) ;
#56069 =( BOUNDED_SURFACE ( )  B_SPLINE_SURFACE ( 3, 1, ( 
 ( #60775, #46715 ),
 ( #32294, #27898 ),
 ( #52300, #47315 ),
 ( #27281, #22279 ) ),
 .UNSPECIFIED., .F., .F., .F. ) 
 B_SPLINE_SURFACE_WITH_KNOTS ( ( 4, 4 ),
 ( 2, 2 ),
 ( 0.000000000000000000, 1.000000000000000000 ),
 ( 0.000000000000000000, 1.000000000000000000 ),
 .UNSPECIFIED. ) 
 GEOMETRIC_REPRESENTATION_ITEM ( )  RATIONAL_B_SPLINE_SURFACE ( (
 ( 1.000000000000000000, 1.000000000000000000),
 ( 0.9953485035131437453, 0.8621029689291515030),
 ( 0.9953485035131437453, 0.8621029689291515030),
 ( 1.000000000000000000, 1.000000000000000000) ) ) 
 REPRESENTATION_ITEM ( '' )  SURFACE ( )  );
#56070 = EDGE_CURVE ( 'NONE', #45566, #20883, #12586, .T. ) ;
#56071 = DIRECTION ( 'NONE',  ( 1.000000000000000000, 0.000000000000000000, 0.000000000000000000 ) ) ;
#56072 = CARTESIAN_POINT ( 'NONE',  ( -6.077587904424778920, -16.14165210942818618, 10.49967087922869702 ) ) ;
#56073 = ORIENTED_EDGE ( 'NONE', *, *, #19206, .F. ) ;
#56074 = DIRECTION ( 'NONE',  ( 0.07439287786467664587, 0.5100024374914937653, -0.8569499480574966910 ) ) ;
#56075 = B_SPLINE_CURVE_WITH_KNOTS ( 'NONE', 3,
 ( #12008, #50190, #36423, #32022, #3791, #22310, #55184, #41437, #23232, #42059, #13224, #31396, #12617, #46437, #22933, #7566, #55489, #26692, #8191 ),
 .UNSPECIFIED., .F., .F.,
 ( 4, 3, 3, 3, 3, 3, 4 ),
 ( 4.878909776184769953E-18, 0.0002724573126191762976, 0.0004086839781548491277, 0.0005449106435901837631, 0.0006811373090491486390, 0.0008459866663933688323, 0.001010840725717212282 ),
 .UNSPECIFIED. ) ;
#56076 = CARTESIAN_POINT ( 'NONE',  ( 0.9780106845699474416, 19.86490431973512472, 36.90144743534066407 ) ) ;
#56077 = FACE_OUTER_BOUND ( 'NONE', #9084, .T. ) ;
#56078 = CARTESIAN_POINT ( 'NONE',  ( 0.7048096507298635682, -41.23648859290943847, 24.78213711671527619 ) ) ;
#56079 = EDGE_LOOP ( 'NONE', ( #10501, #4954, #16596, #4883 ) ) ;
#56080 = EDGE_CURVE ( 'NONE', #45127, #43289, #8280, .T. ) ;
#56081 = B_SPLINE_CURVE_WITH_KNOTS ( 'NONE', 3,
 ( #6852, #22222, #40737, #25990 ),
 .UNSPECIFIED., .F., .F.,
 ( 4, 4 ),
 ( 0.000000000000000000, 0.005013413432710145910 ),
 .UNSPECIFIED. ) ;
#56082 = CARTESIAN_POINT ( 'NONE',  ( 0.6067099128993228563, 46.07641759122984126, -13.08009036336154196 ) ) ;
#56083 = CARTESIAN_POINT ( 'NONE',  ( 2.281351352603294913, -47.95523304704243372, -1.314116150903955615 ) ) ;
#56084 = EDGE_CURVE ( 'NONE', #33948, #53671, #33355, .T. ) ;
#56085 = ORIENTED_EDGE ( 'NONE', *, *, #30924, .T. ) ;
#56086 = DIRECTION ( 'NONE',  ( -0.07836865515943411409, 0.3887811538706132941, 0.9179910502197372590 ) ) ;
#56087 = CARTESIAN_POINT ( 'NONE',  ( 4.967162193818130511, 2.375726030843182457, -43.02067033766016380 ) ) ;
#56088 = DIRECTION ( 'NONE',  ( -1.000000000000000000, -0.000000000000000000, -0.000000000000000000 ) ) ;
#56089 = ORIENTED_EDGE ( 'NONE', *, *, #47277, .F. ) ;
#56090 = CARTESIAN_POINT ( 'NONE',  ( 0.6031356219577718170, 29.35521383643406779, 38.11305734842073178 ) ) ;
#56091 = ORIENTED_EDGE ( 'NONE', *, *, #10057, .F. ) ;
#56092 = ORIENTED_EDGE ( 'NONE', *, *, #5129, .F. ) ;
#56093 = CARTESIAN_POINT ( 'NONE',  ( -1.400000000000000799, 9.062386313690440012E-16, 7.400000000000021672 ) ) ;
#56094 = ORIENTED_EDGE ( 'NONE', *, *, #22916, .F. ) ;
#56095 = CARTESIAN_POINT ( 'NONE',  ( 5.959547316686252039, 20.52562247508876681, 0.003562808152977453395 ) ) ;
#56096 = EDGE_CURVE ( 'NONE', #52648, #17303, #53044, .T. ) ;
#56097 = VERTEX_POINT ( 'NONE', #61508 ) ;
#56098 = CARTESIAN_POINT ( 'NONE',  ( -6.079354080745853928, 16.77867255551491255, 9.448232772480407604 ) ) ;
#56099 = AXIS2_PLACEMENT_3D ( 'NONE', #43969, #53008, #20140 ) ;
#56100 = CARTESIAN_POINT ( 'NONE',  ( 5.896278296736517710, 8.461230214157993146, 18.24649453668850541 ) ) ;
#56101 = CARTESIAN_POINT ( 'NONE',  ( 0.9752570700956777472, 16.20701641182919417, 39.72995844664864507 ) ) ;
#56102 = B_SPLINE_CURVE_WITH_KNOTS ( 'NONE', 3,
 ( #25552, #16171, #15865, #29328, #34983, #30246, #49361, #43781, #6412, #49665, #5502, #39076, #25864, #15250, #16468, #54660, #58129, #26791, #18025, #41224, #46530, #2660, #37143, #55276, #41528, #11786, #30867, #36211, #31812, #40611 ),
 .UNSPECIFIED., .F., .F.,
 ( 4, 2, 2, 2, 2, 2, 2, 2, 2, 2, 2, 2, 2, 2, 4 ),
 ( 0.000000000000000000, 0.0004110759757379565276, 0.0008221519514759130553, 0.001233227927213869637, 0.001644303902951826111, 0.002466455854427739708, 0.003288607805903653956, 0.003699683781641610429, 0.004110759757379567336, 0.004521835733117523376, 0.004932911708855479416, 0.005343987684593436323, 0.005755063660331393230, 0.006166139636069349270, 0.006577215611807306177 ),
 .UNSPECIFIED. ) ;
#56103 = ORIENTED_EDGE ( 'NONE', *, *, #13395, .T. ) ;
#56104 = CARTESIAN_POINT ( 'NONE',  ( -0.2999999999999999889, -13.49666625504239015, -1.199999999999999956 ) ) ;
#56105 = CARTESIAN_POINT ( 'NONE',  ( -6.063463321072276813, -11.00428472829056759, 15.80272666656551372 ) ) ;
#56106 = CARTESIAN_POINT ( 'NONE',  ( 0.5835871038041877679, -44.25621114391295663, -15.51200271038183764 ) ) ;
#56107 = CARTESIAN_POINT ( 'NONE',  ( 0.7762777257811910303, 19.15108781300990159, -43.90991299786880830 ) ) ;
#56108 = EDGE_LOOP ( 'NONE', ( #37591, #41133, #39255, #1637 ) ) ;
#56109 = CARTESIAN_POINT ( 'NONE',  ( 0.7764146366350271888, 43.52296033649982121, 17.48692074713635591 ) ) ;
#56110 = ORIENTED_EDGE ( 'NONE', *, *, #9876, .T. ) ;
#56111 = DIRECTION ( 'NONE',  ( 0.09722883295013590166, -0.1513788123411506925, 0.9836823721188344694 ) ) ;
#56112 = ORIENTED_EDGE ( 'NONE', *, *, #36302, .T. ) ;
#56113 = CARTESIAN_POINT ( 'NONE',  ( 4.962356264823608143, 0.9708976703217077064, 42.07484944210865052 ) ) ;
#56114 = LINE ( 'NONE', #57333, #54040 ) ;
#56115 = ORIENTED_EDGE ( 'NONE', *, *, #50146, .T. ) ;
#56116 = DIRECTION ( 'NONE',  ( 0.09835009131224552170, 0.9592125346408720832, -0.2650256080583662799 ) ) ;
#56117 = CARTESIAN_POINT ( 'NONE',  ( -6.016761891674564211, -18.20023637398602290, 4.880293656734900232 ) ) ;
#56118 = CARTESIAN_POINT ( 'NONE',  ( 4.975610109902397937, 47.16372689271652519, 12.96272628450595832 ) ) ;
#56119 = CARTESIAN_POINT ( 'NONE',  ( 0.5998501479064708430, -46.33007877220729398, -12.95623334615486222 ) ) ;
#56120 = ORIENTED_EDGE ( 'NONE', *, *, #28645, .F. ) ;
#56121 = CARTESIAN_POINT ( 'NONE',  ( 4.956653778116975495, 3.690426056929986043, 47.94889704119053420 ) ) ;
#56122 = CARTESIAN_POINT ( 'NONE',  ( 0.9762797500689124330, -41.84568905980458453, 2.294143041716202092 ) ) ;
#56123 = EDGE_CURVE ( 'NONE', #47245, #15844, #11303, .T. ) ;
#56124 = CARTESIAN_POINT ( 'NONE',  ( 0.6001305935487422083, 41.40054608060260222, 24.50730504006470767 ) ) ;
#56125 = CARTESIAN_POINT ( 'NONE',  ( 0.6001305935487422083, -47.62765676940948367, 6.798494447611420632 ) ) ;
#56126 = B_SPLINE_CURVE_WITH_KNOTS ( 'NONE', 3,
 ( #17165, #8985, #52818, #29319, #493, #28095 ),
 .UNSPECIFIED., .F., .F.,
 ( 4, 2, 4 ),
 ( 6.106282077343214115E-18, 0.0002291472222819941282, 0.0004582944445639821848 ),
 .UNSPECIFIED. ) ;
#56127 = EDGE_CURVE ( 'NONE', #15021, #24192, #24549, .T. ) ;
#56128 = CARTESIAN_POINT ( 'NONE',  ( -1.114299999999999624, 0.000000000000000000, 0.000000000000000000 ) ) ;
#56129 = CARTESIAN_POINT ( 'NONE',  ( 3.270143674763207553, -11.02405647745164430, -8.113405361969626028 ) ) ;
#56130 = CARTESIAN_POINT ( 'NONE',  ( 0.1129192098497455998, -22.45785791439690371, -37.98152716363461678 ) ) ;
#56131 = CARTESIAN_POINT ( 'NONE',  ( 0.5827359174754819238, -46.35666395585283084, 12.04517879102121292 ) ) ;
#56132 = ADVANCED_FACE ( 'NONE', ( #61812 ), #4747, .F. ) ;
#56133 = FACE_OUTER_BOUND ( 'NONE', #22385, .T. ) ;
#56134 = CARTESIAN_POINT ( 'NONE',  ( 0.9780106845699487739, -12.71570332633824840, 39.93297053027720978 ) ) ;
#56135 = CYLINDRICAL_SURFACE ( 'NONE', #19409, 2.649999999999992806 ) ;
#56136 = CARTESIAN_POINT ( 'NONE',  ( 1.088908134280559770, 33.56490895818201636, -26.73890361625880630 ) ) ;
#56137 = CARTESIAN_POINT ( 'NONE',  ( 0.1102847568649952675, -21.48234084756722240, 37.39286109091540311 ) ) ;
#56138 = CARTESIAN_POINT ( 'NONE',  ( 4.967162193818130511, 0.000000000000000000, 0.000000000000000000 ) ) ;
#56139 = CARTESIAN_POINT ( 'NONE',  ( 4.967162193818130511, 0.000000000000000000, 0.000000000000000000 ) ) ;
#56140 = DIRECTION ( 'NONE',  ( 0.000000000000000000, 0.000000000000000000, -1.000000000000000000 ) ) ;
#56141 = AXIS2_PLACEMENT_3D ( 'NONE', #42022, #3752, #4357 ) ;
#56142 = AXIS2_PLACEMENT_3D ( 'NONE', #18029, #60915, #56525 ) ;
#56143 = CARTESIAN_POINT ( 'NONE',  ( 0.9758171775293911221, -37.16279804060120995, -21.44911662810690345 ) ) ;
#56144 = ADVANCED_FACE ( 'NONE', ( #102 ), #24729, .F. ) ;
#56146 =( BOUNDED_SURFACE ( )  B_SPLINE_SURFACE ( 3, 1, ( 
 ( #12831, #41958 ),
 ( #31607, #18439 ),
 ( #61023, #55395 ),
 ( #46044, #3689 ) ),
 .UNSPECIFIED., .F., .F., .F. ) 
 B_SPLINE_SURFACE_WITH_KNOTS ( ( 4, 4 ),
 ( 2, 2 ),
 ( 0.000000000000000000, 1.000000000000000000 ),
 ( 0.000000000000000000, 1.000000000000000000 ),
 .UNSPECIFIED. ) 
 GEOMETRIC_REPRESENTATION_ITEM ( )  RATIONAL_B_SPLINE_SURFACE ( (
 ( 1.000000000000000000, 1.000000000000000000),
 ( 0.7223157951917476005, 0.9931996967497186413),
 ( 0.7223157951917476005, 0.9931996967497186413),
 ( 1.000000000000000000, 1.000000000000000000) ) ) 
 REPRESENTATION_ITEM ( '' )  SURFACE ( )  );
#56145 = CARTESIAN_POINT ( 'NONE',  ( 4.000000000000003553, -1.933795701539621659, -5.351162342337697275 ) ) ;
#56147 = CARTESIAN_POINT ( 'NONE',  ( 0.9972139404380315764, 11.74016833743920252, 41.27214627875013520 ) ) ;
#56149 = ORIENTED_EDGE ( 'NONE', *, *, #16498, .F. ) ;
#56148 = DIRECTION ( 'NONE',  ( -0.000000000000000000, -1.000000000000000000, -0.000000000000000000 ) ) ;
#56150 = EDGE_LOOP ( 'NONE', ( #17888, #59657, #5249, #45494 ) ) ;
#56151 = B_SPLINE_CURVE_WITH_KNOTS ( 'NONE', 3,
 ( #48570, #23846, #52642, #5936, #10371, #38897, #29460, #47652, #15075, #24144, #33263, #14767, #43283, #5626, #28846, #58256, #52334, #39513, #15387 ),
 .UNSPECIFIED., .F., .F.,
 ( 4, 3, 3, 3, 3, 3, 4 ),
 ( 3.469552829456483146E-18, 0.0002612768053151668301, 0.0003919133833142874560, 0.0005225499612322542483, 0.0006531865391693342238, 0.0008112755173415162795, 0.0009693688056799698626 ),
 .UNSPECIFIED. ) ;
#56152 = CARTESIAN_POINT ( 'NONE',  ( 4.549368137175248350, 0.000000000000000000, 0.000000000000000000 ) ) ;
#56153 = CARTESIAN_POINT ( 'NONE',  ( -6.063463321072276813, -17.34291445406333310, 8.369215657306909861 ) ) ;
#56155 = ADVANCED_FACE ( 'NONE', ( #9837 ), #40583, .F. ) ;
#56154 = CARTESIAN_POINT ( 'NONE',  ( 4.549368137175248350, -35.57418903283098643, -24.02461520945259466 ) ) ;
#56156 = VERTEX_POINT ( 'NONE', #33969 ) ;
#56157 = VERTEX_POINT ( 'NONE', #57727 ) ;
#56158 = CARTESIAN_POINT ( 'NONE',  ( 0.5809828226811553087, -33.48000389720640868, 34.25055090842140970 ) ) ;
#56159 = CARTESIAN_POINT ( 'NONE',  ( 1.091591847532198623, -39.33176300527454572, -14.48348748930166252 ) ) ;
#56160 = EDGE_CURVE ( 'NONE', #41822, #28421, #29241, .T. ) ;
#56161 = B_SPLINE_CURVE_WITH_KNOTS ( 'NONE', 3,
 ( #51766, #8234, #18278, #12661, #22662, #61458 ),
 .UNSPECIFIED., .F., .F.,
 ( 4, 2, 4 ),
 ( 1.870366591887036261E-17, 0.0002293755540694321316, 0.0004587511081388455608 ),
 .UNSPECIFIED. ) ;
#56162 = PRODUCT_DEFINITION_CONTEXT ( 'detailed design', #48782, 'design' ) ;
#56163 = ORIENTED_EDGE ( 'NONE', *, *, #23767, .F. ) ;
#56164 = ORIENTED_EDGE ( 'NONE', *, *, #20282, .F. ) ;
#56165 = CARTESIAN_POINT ( 'NONE',  ( 0.9745511491811748028, -10.77620558745907786, -41.53317535253985682 ) ) ;
#56166 = DIRECTION ( 'NONE',  ( 1.000000000000000000, 0.000000000000000000, 0.000000000000000000 ) ) ;
#56167 = CARTESIAN_POINT ( 'NONE',  ( 1.092182651088184242, -2.180685162625981555, -41.85696831668280282 ) ) ;
#56168 = VERTEX_POINT ( 'NONE', #29859 ) ;
#56169 = VERTEX_POINT ( 'NONE', #48660 ) ;
#56170 = CARTESIAN_POINT ( 'NONE',  ( 0.8557997880470599172, 44.60232077416710439, -17.48760788519168941 ) ) ;
#56171 = EDGE_CURVE ( 'NONE', #23427, #61046, #48555, .T. ) ;
#56172 = CARTESIAN_POINT ( 'NONE',  ( 2.528100132419517365, 2.996127168110702677, -41.87215065678599757 ) ) ;
#56173 = B_SPLINE_CURVE_WITH_KNOTS ( 'NONE', 3,
 ( #25818, #7303, #49311, #40263, #59013, #11121, #35549, #40567, #54609, #41180, #59629, #30203, #6366, #59945, #54926, #12059 ),
 .UNSPECIFIED., .F., .F.,
 ( 4, 3, 3, 3, 3, 4 ),
 ( 1.551621725782133898E-17, 0.0002732102107931876685, 0.0004098135523333712340, 0.0005464168938824954559, 0.0008195847345945416005, 0.001092771384553108084 ),
 .UNSPECIFIED. ) ;
#56174 = EDGE_CURVE ( 'NONE', #32390, #26300, #49459, .T. ) ;
#56175 = B_SPLINE_CURVE_WITH_KNOTS ( 'NONE', 3,
 ( #2672, #40014, #45321, #29960 ),
 .UNSPECIFIED., .F., .F.,
 ( 4, 4 ),
 ( 0.000000000000000000, 0.005014147105413695182 ),
 .UNSPECIFIED. ) ;
#56176 = CARTESIAN_POINT ( 'NONE',  ( 0.1103878639767399555, 21.60424693647505023, 37.32258098927775336 ) ) ;
#56177 = ORIENTED_EDGE ( 'NONE', *, *, #1408, .F. ) ;
#56178 = ORIENTED_EDGE ( 'NONE', *, *, #48950, .F. ) ;
#56179 = CARTESIAN_POINT ( 'NONE',  ( 4.303969348037246512, -20.38638383586150127, 43.57722561725952204 ) ) ;
#56180 = EDGE_LOOP ( 'NONE', ( #31236, #25487, #15992, #35793 ) ) ;
#56181 = CARTESIAN_POINT ( 'NONE',  ( -6.017396004339686577, 4.875835690939434919, -18.20140164570664254 ) ) ;
#56182 = CARTESIAN_POINT ( 'NONE',  ( 1.231276596079887264, 24.17959027891153667, -34.24360064248551083 ) ) ;
#56183 = CARTESIAN_POINT ( 'NONE',  ( 0.8744876279028263033, 3.827863332834932297, 48.94586308039354350 ) ) ;
#56184 = CARTESIAN_POINT ( 'NONE',  ( 0.5804410086790514622, 5.237717535875737518, -46.60564522533483967 ) ) ;
#56185 = DIRECTION ( 'NONE',  ( -1.000000000000000000, -0.000000000000000000, -0.000000000000000000 ) ) ;
#56186 = ORIENTED_EDGE ( 'NONE', *, *, #24479, .F. ) ;
#56187 = CARTESIAN_POINT ( 'NONE',  ( -6.016761891674565099, 9.424569481870481269, -16.31696541414262214 ) ) ;
#56188 = VECTOR ( 'NONE', #18892, 1000.000000000000000 ) ;
#56189 = CARTESIAN_POINT ( 'NONE',  ( 4.833616638992208614, 26.07076047129084273, 38.20222678111946379 ) ) ;
#56190 = CARTESIAN_POINT ( 'NONE',  ( -6.016104459813374383, -18.68271063303496504, 2.454244026261025446 ) ) ;
#56191 = EDGE_LOOP ( 'NONE', ( #60231, #55705, #50530, #61724 ) ) ;
#56192 = CARTESIAN_POINT ( 'NONE',  ( 5.960221823109900008, 7.849768660536287967, 18.96526051813983571 ) ) ;
#56193 = CARTESIAN_POINT ( 'NONE',  ( 0.6845945791218023269, -29.61886432666044300, 36.37484565895540811 ) ) ;
#56194 = CARTESIAN_POINT ( 'NONE',  ( 5.901764892641307547, -28.05153439370029389, 40.13854613210009603 ) ) ;
#56195 = CARTESIAN_POINT ( 'NONE',  ( 0.5998501479064708430, 6.798102206414135651, -47.62484632993681544 ) ) ;
#56196 = ORIENTED_EDGE ( 'NONE', *, *, #34196, .F. ) ;
#56197 = CARTESIAN_POINT ( 'NONE',  ( 3.678748215320120529, -46.87105689412023679, 14.20270537354160822 ) ) ;
#56198 = CARTESIAN_POINT ( 'NONE',  ( -6.016104459813374383, 14.95258000663147691, -11.46679299034565247 ) ) ;
#56199 = EDGE_CURVE ( 'NONE', #46408, #28202, #23945, .T. ) ;
#56200 = FACE_OUTER_BOUND ( 'NONE', #1454, .T. ) ;
#56201 = EDGE_CURVE ( 'NONE', #16043, #24805, #30464, .T. ) ;
#56202 = CARTESIAN_POINT ( 'NONE',  ( 0.1152809850208375564, -17.65825178363827774, -40.43675835716051381 ) ) ;
#56203 = CARTESIAN_POINT ( 'NONE',  ( 0.3676999524040366896, 10.61898383218289155, 42.81574203134493928 ) ) ;
#56204 = CARTESIAN_POINT ( 'NONE',  ( 0.9756354156337461170, 42.90827993934335893, 0.1303083999668459281 ) ) ;
#56205 = LINE ( 'NONE', #18331, #5750 ) ;
#56206 = CARTESIAN_POINT ( 'NONE',  ( 0.9722240741986377666, -21.95618662952211508, 36.86535088273198113 ) ) ;
#56207 = EDGE_CURVE ( 'NONE', #41822, #27686, #25375, .T. ) ;
#56208 = FACE_OUTER_BOUND ( 'NONE', #1461, .T. ) ;
#56209 = EDGE_CURVE ( 'NONE', #37177, #4442, #6575, .T. ) ;
#56210 = CARTESIAN_POINT ( 'NONE',  ( 4.975610109902397937, -11.44439439467595143, 47.55497076097179843 ) ) ;
#56211 = VERTEX_POINT ( 'NONE', #58341 ) ;
#56212 = EDGE_CURVE ( 'NONE', #59068, #53799, #6327, .T. ) ;
#56213 = CARTESIAN_POINT ( 'NONE',  ( 0.5807400328401637335, 23.47602859900772998, -41.75144119563861267 ) ) ;
#56214 = CARTESIAN_POINT ( 'NONE',  ( 1.091591847532191073, -18.34768875777499275, 37.68449692119637717 ) ) ;
#56215 = CARTESIAN_POINT ( 'NONE',  ( 0.5988103622719990193, -33.58571533649136143, -34.44344971428014901 ) ) ;
#56216 = DIRECTION ( 'NONE',  ( 0.000000000000000000, 0.7071067811865527908, -0.7071067811865421326 ) ) ;
#56217 = CARTESIAN_POINT ( 'NONE',  ( 4.390527457369402420, -24.87150827751877813, -36.21592760968486857 ) ) ;
#56219 = B_SPLINE_CURVE_WITH_KNOTS ( 'NONE', 3,
 ( #7988, #59987, #27101, #46226, #7661, #56518 ),
 .UNSPECIFIED., .F., .F.,
 ( 4, 2, 4 ),
 ( 1.524244818460479926E-16, 0.0002445252820015232013, 0.0004890505640028939638 ),
 .UNSPECIFIED. ) ;
#56218 = DIRECTION ( 'NONE',  ( 0.000000000000000000, 0.000000000000000000, 1.000000000000000000 ) ) ;
#56220 = PRODUCT_CONTEXT ( 'NONE', #33157, 'mechanical' ) ;
#56221 = DIRECTION ( 'NONE',  ( -1.000000000000000000, -0.000000000000000000, -0.000000000000000000 ) ) ;
#56222 = EDGE_CURVE ( 'NONE', #49600, #42216, #52326, .T. ) ;
#56223 = CARTESIAN_POINT ( 'NONE',  ( 0.5836750258453360374, 12.22088356912726681, 46.31062999473589059 ) ) ;
#56224 = LINE ( 'NONE', #28042, #27435 ) ;
#56226 = ORIENTED_EDGE ( 'NONE', *, *, #18681, .F. ) ;
#56225 = DIRECTION ( 'NONE',  ( 0.07439287786467665975, 0.8569499480574949146, 0.5100024374914968739 ) ) ;
#56227 = ORIENTED_EDGE ( 'NONE', *, *, #49273, .T. ) ;
#56228 = CARTESIAN_POINT ( 'NONE',  ( 0.1101816497532062955, -43.12424935764384060, 0.1358190954554068519 ) ) ;
#56229 = CARTESIAN_POINT ( 'NONE',  ( 0.5806925824938502512, -7.260877859417425029, 46.33035738103242096 ) ) ;
#56230 = CARTESIAN_POINT ( 'NONE',  ( 5.974727161628367256, -14.52429704002354072, -14.50236057684839963 ) ) ;
#56231 = ORIENTED_EDGE ( 'NONE', *, *, #45112, .T. ) ;
#56232 = CARTESIAN_POINT ( 'NONE',  ( 4.956653778116989706, -40.28700667097662347, -26.26162724282415084 ) ) ;
#56233 = CARTESIAN_POINT ( 'NONE',  ( 2.648799415243708655, 15.62808678998979239, -46.47881632070836844 ) ) ;
#56234 = CARTESIAN_POINT ( 'NONE',  ( -5.995132425357893702, -13.33084941932897927, -13.31880955509740971 ) ) ;
#56235 = AXIS2_PLACEMENT_3D ( 'NONE', #26398, #49904, #41148 ) ;
#56236 = ORIENTED_EDGE ( 'NONE', *, *, #18952, .F. ) ;
#56237 = ORIENTED_EDGE ( 'NONE', *, *, #14631, .F. ) ;
#56238 = CARTESIAN_POINT ( 'NONE',  ( 0.9730545539215883499, 41.31259007387230753, 11.59290486963521971 ) ) ;
#56239 = CARTESIAN_POINT ( 'NONE',  ( 4.962356264823608143, 37.36413190407361640, 19.36897635181929545 ) ) ;
#56240 = CARTESIAN_POINT ( 'NONE',  ( 4.549368137175248350, -13.59764261105721950, -40.71620287708339703 ) ) ;
#56241 = CARTESIAN_POINT ( 'NONE',  ( 0.7948878604505671408, 43.85325310457696446, -22.08145917833165939 ) ) ;
#56242 = EDGE_CURVE ( 'NONE', #2408, #18299, #41163, .T. ) ;
#56243 = CARTESIAN_POINT ( 'NONE',  ( 0.6008122571543327295, 49.03265619930817820, 2.711674114963254389 ) ) ;
#56244 =( BOUNDED_SURFACE ( )  B_SPLINE_SURFACE ( 3, 1, ( 
 ( #19958, #6111 ),
 ( #24954, #59363 ),
 ( #44091, #20261 ),
 ( #24641, #15554 ) ),
 .UNSPECIFIED., .F., .F., .F. ) 
 B_SPLINE_SURFACE_WITH_KNOTS ( ( 4, 4 ),
 ( 2, 2 ),
 ( 0.000000000000000000, 1.000000000000000000 ),
 ( 0.000000000000000000, 1.000000000000000000 ),
 .UNSPECIFIED. ) 
 GEOMETRIC_REPRESENTATION_ITEM ( )  RATIONAL_B_SPLINE_SURFACE ( (
 ( 1.000000000000000000, 1.000000000000000000),
 ( 0.9953390228620291325, 0.8624445117760984880),
 ( 0.9953390228620291325, 0.8624445117760984880),
 ( 1.000000000000000000, 1.000000000000000000) ) ) 
 REPRESENTATION_ITEM ( '' )  SURFACE ( )  );
#56245 = EDGE_CURVE ( 'NONE', #39870, #5752, #47149, .T. ) ;
#56246 = CARTESIAN_POINT ( 'NONE',  ( 0.8554163680231738898, -13.02474486562517519, -45.07284652978098904 ) ) ;
#56247 = ORIENTED_EDGE ( 'NONE', *, *, #21933, .F. ) ;
#56248 = CARTESIAN_POINT ( 'NONE',  ( 4.553261556744875094, 42.54662847375985280, -10.92355122382294752 ) ) ;
#56249 = CARTESIAN_POINT ( 'NONE',  ( 0.5980894510889457338, 48.10766805928369649, -0.7015180095999885568 ) ) ;
#56250 = VERTEX_POINT ( 'NONE', #24750 ) ;
#56251 = CARTESIAN_POINT ( 'NONE',  ( 5.901764892641307547, -44.13851569553294496, 21.20808571358740124 ) ) ;
#56252 = FACE_OUTER_BOUND ( 'NONE', #49957, .T. ) ;
#56253 = CARTESIAN_POINT ( 'NONE',  ( 0.9268187852002115479, 39.28166228011650674, -20.01762576879431066 ) ) ;
#56254 = CARTESIAN_POINT ( 'NONE',  ( 0.1129192098497455998, -35.06977877439224045, -26.77802092202373174 ) ) ;
#56255 = ORIENTED_EDGE ( 'NONE', *, *, #486, .F. ) ;
#56256 = ORIENTED_EDGE ( 'NONE', *, *, #5911, .F. ) ;
#56257 = CARTESIAN_POINT ( 'NONE',  ( -6.015611763856276717, -11.47596948473821321, 14.94556629257421498 ) ) ;
#56258 = DIRECTION ( 'NONE',  ( 1.000000000000000000, 0.000000000000000000, 0.000000000000000000 ) ) ;
#56259 = CARTESIAN_POINT ( 'NONE',  ( 0.1073791018717578927, 25.86618856530665767, 34.50606437925554815 ) ) ;
#56260 =( BOUNDED_SURFACE ( )  B_SPLINE_SURFACE ( 3, 1, ( 
 ( #16890, #8692 ),
 ( #36004, #14044 ),
 ( #52530, #34077 ),
 ( #53145, #61307 ) ),
 .UNSPECIFIED., .F., .F., .F. ) 
 B_SPLINE_SURFACE_WITH_KNOTS ( ( 4, 4 ),
 ( 2, 2 ),
 ( 0.000000000000000000, 1.000000000000000000 ),
 ( 0.000000000000000000, 1.000000000000000000 ),
 .UNSPECIFIED. ) 
 GEOMETRIC_REPRESENTATION_ITEM ( )  RATIONAL_B_SPLINE_SURFACE ( (
 ( 1.000000000000000000, 1.000000000000000000),
 ( 0.9952954269826590483, 0.8620686068821339365),
 ( 0.9952954269826590483, 0.8620686068821339365),
 ( 1.000000000000000000, 1.000000000000000000) ) ) 
 REPRESENTATION_ITEM ( '' )  SURFACE ( )  );
#56261 = ORIENTED_EDGE ( 'NONE', *, *, #23690, .F. ) ;
#56262 = CARTESIAN_POINT ( 'NONE',  ( 4.000000000000003553, 1.935983797701078757, -0.2494693066162350648 ) ) ;
#56263 = ORIENTED_EDGE ( 'NONE', *, *, #39784, .F. ) ;
#56264 = CARTESIAN_POINT ( 'NONE',  ( 0.5832655196449145762, 27.63416530929389836, 37.88915531694979677 ) ) ;
#56265 = B_SPLINE_CURVE_WITH_KNOTS ( 'NONE', 3,
 ( #4972, #43235, #270, #61369 ),
 .UNSPECIFIED., .F., .F.,
 ( 4, 4 ),
 ( 6.505213034913026604E-19, 0.004041751736740995145 ),
 .UNSPECIFIED. ) ;
#56266 = CARTESIAN_POINT ( 'NONE',  ( 0.6021447746440204973, -14.22269149442896463, -47.00272530122892789 ) ) ;
#56267 = VERTEX_POINT ( 'NONE', #42958 ) ;
#56268 = CARTESIAN_POINT ( 'NONE',  ( 0.5838002273316429402, -47.46823345111864256, -6.386683873061000938 ) ) ;
#56269 = CARTESIAN_POINT ( 'NONE',  ( 2.528190830796654520, 13.95207949221547672, 39.59284801572006529 ) ) ;
#56270 = CARTESIAN_POINT ( 'NONE',  ( 0.9754292589017212745, -41.84984047562296894, -2.217728355815624219 ) ) ;
#56271 = AXIS2_PLACEMENT_3D ( 'NONE', #7215, #36693, #40472 ) ;
#56272 = EDGE_CURVE ( 'NONE', #24504, #2547, #59773, .T. ) ;
#56273 = ORIENTED_EDGE ( 'NONE', *, *, #30896, .T. ) ;
#56274 = CARTESIAN_POINT ( 'NONE',  ( 0.5806925824938511393, 10.33919002968708689, -45.74192291403568333 ) ) ;
#56275 = AXIS2_PLACEMENT_3D ( 'NONE', #39747, #30307, #58798 ) ;
#56276 = CARTESIAN_POINT ( 'NONE',  ( 0.3676999524040323597, -34.85286720109652947, -27.04123205746306979 ) ) ;
#56277 = CARTESIAN_POINT ( 'NONE',  ( 5.910764540655177868, 10.80896614705642556, 16.96076322872739084 ) ) ;
#56278 = CARTESIAN_POINT ( 'NONE',  ( 0.1081432562775997697, 26.58728936586516767, -33.95357233988202239 ) ) ;
#56279 = CARTESIAN_POINT ( 'NONE',  ( 0.8560838555295158248, 36.24009790160309308, 29.78301761346479282 ) ) ;
#56280 = ORIENTED_EDGE ( 'NONE', *, *, #50151, .F. ) ;
#56281 = ADVANCED_FACE ( 'NONE', ( #43893, #37960, #10349, #43571, #38563, #42638, #14139, #38259, #9720, #5 ), #58235, .T. ) ;
#56282 = CARTESIAN_POINT ( 'NONE',  ( -6.015611763856276717, -9.427003116184058840, -16.31561949997086103 ) ) ;
#56283 = EDGE_CURVE ( 'NONE', #31513, #46120, #24595, .T. ) ;
#56284 = FACE_OUTER_BOUND ( 'NONE', #7632, .T. ) ;
#56285 = VERTEX_POINT ( 'NONE', #20068 ) ;
#56286 = EDGE_CURVE ( 'NONE', #22147, #59631, #31615, .T. ) ;
#56287 = CARTESIAN_POINT ( 'NONE',  ( 4.956445790444010235, -22.15545010017738647, -41.55326799420456751 ) ) ;
#56288 = CARTESIAN_POINT ( 'NONE',  ( -6.072942160501519027, -17.35560219702265528, 8.341896347217623742 ) ) ;
#56289 = CARTESIAN_POINT ( 'NONE',  ( 0.1368894036331302633, -34.97597666220990220, 26.89874313881377788 ) ) ;
#56290 = CARTESIAN_POINT ( 'NONE',  ( 0.3622758884714600280, -11.95365414648526148, 41.42293301073604539 ) ) ;
#56291 = CARTESIAN_POINT ( 'NONE',  ( 3.407937589446174087, 1.331713209622503058, 13.63405474014708929 ) ) ;
#56292 = CARTESIAN_POINT ( 'NONE',  ( 2.643462169533600914, 48.01657676222235693, 1.382267876918626959 ) ) ;
#56293 = B_SPLINE_CURVE_WITH_KNOTS ( 'NONE', 3,
 ( #26850, #50338, #2718, #31546, #6468, #16221 ),
 .UNSPECIFIED., .F., .F.,
 ( 4, 2, 4 ),
 ( 2.693102327163510278E-18, 0.0002447193893791694912, 0.0004894387787583362719 ),
 .UNSPECIFIED. ) ;
#56294 = CARTESIAN_POINT ( 'NONE',  ( 0.2940135542859016460, 3.434477694418887950, -43.98232499150039132 ) ) ;
#56295 = DIRECTION ( 'NONE',  ( -1.000000000000000000, -1.836909530733580185E-16, 1.836909530733574022E-16 ) ) ;
#56296 = VECTOR ( 'NONE', #54451, 1000.000000000000114 ) ;
#56297 = CARTESIAN_POINT ( 'NONE',  ( 4.549368137175248350, 0.000000000000000000, 0.000000000000000000 ) ) ;
#56298 = CARTESIAN_POINT ( 'NONE',  ( 4.975801465491695552, -46.87746200127462970, 9.906103548667402947 ) ) ;
#56300 = EDGE_CURVE ( 'NONE', #20883, #16844, #737, .T. ) ;
#56299 = CARTESIAN_POINT ( 'NONE',  ( 0.1098349054025746369, -5.840292671757984166, 42.72717686504319801 ) ) ;
#56301 = EDGE_LOOP ( 'NONE', ( #20837, #41653, #50227, #21282 ) ) ;
#56302 = CARTESIAN_POINT ( 'NONE',  ( 4.303969348037246512, 22.16169334783837996, 42.70173985163825137 ) ) ;
#56303 = CARTESIAN_POINT ( 'NONE',  ( 0.6021448801613057400, -1.312835145200685227, -49.08989307900835541 ) ) ;
#56304 = CARTESIAN_POINT ( 'NONE',  ( 4.956445790443988031, 0.000000000000000000, 0.000000000000000000 ) ) ;
#56305 = CARTESIAN_POINT ( 'NONE',  ( 0.3622758884714600280, 26.89560658783384994, -33.69533458712316332 ) ) ;
#56306 = CARTESIAN_POINT ( 'NONE',  ( 0.8560838555295158248, -46.85553835019179303, 2.220666565569249684 ) ) ;
#56307 = ORIENTED_EDGE ( 'NONE', *, *, #4841, .F. ) ;
#56308 = CARTESIAN_POINT ( 'NONE',  ( 1.830465331921977690, 39.13607268272329520, 20.21741503879734481 ) ) ;
#56309 = CARTESIAN_POINT ( 'NONE',  ( 3.270143674763207553, 8.113405361969507013, 11.02405647745173134 ) ) ;
#56310 = CARTESIAN_POINT ( 'NONE',  ( 1.657374760986086271, 28.69055495241272880, -33.43265624766942778 ) ) ;
#56311 = CARTESIAN_POINT ( 'NONE',  ( -19.79470381413520386, -7.930988484581699360, -1.054774614931486720 ) ) ;
#56312 = ORIENTED_EDGE ( 'NONE', *, *, #16413, .F. ) ;
#56313 = CARTESIAN_POINT ( 'NONE',  ( 5.896782393890504181, 0.6657210432555761281, 20.10181341000306077 ) ) ;
#56314 = VECTOR ( 'NONE', #54370, 1000.000000000000114 ) ;
#56315 = CARTESIAN_POINT ( 'NONE',  ( 0.6027935024548037868, 24.20473723001696698, -41.57475399306895980 ) ) ;
#56316 = VERTEX_POINT ( 'NONE', #34163 ) ;
#56317 = EDGE_CURVE ( 'NONE', #3844, #41582, #9733, .T. ) ;
#56318 = CARTESIAN_POINT ( 'NONE',  ( 2.185380717157382691, -26.31419589484018928, 35.30414844568801414 ) ) ;
#56319 = ORIENTED_EDGE ( 'NONE', *, *, #44042, .F. ) ;
#56320 = CARTESIAN_POINT ( 'NONE',  ( 45.00000000000001421, 9.184850993605150311E-15, -75.00000000000001421 ) ) ;
#56321 = FACE_OUTER_BOUND ( 'NONE', #30263, .T. ) ;
#56322 = B_SPLINE_CURVE_WITH_KNOTS ( 'NONE', 3,
 ( #20177, #10461, #58042, #44308, #39602, #43375 ),
 .UNSPECIFIED., .F., .F.,
 ( 4, 2, 4 ),
 ( 6.946513017424995024E-18, 0.0002291966416970823311, 0.0004583932833941577233 ),
 .UNSPECIFIED. ) ;
#56323 = EDGE_LOOP ( 'NONE', ( #41844, #59564, #11337, #760 ) ) ;
#56324 = CARTESIAN_POINT ( 'NONE',  ( 5.981074661064941900, 12.48781255314288963, -16.28853686865586425 ) ) ;
#56325 = CARTESIAN_POINT ( 'NONE',  ( 0.1100053167205931048, 26.39466280306222856, 34.10339839758293579 ) ) ;
#56326 = EDGE_LOOP ( 'NONE', ( #7955, #18094, #7447, #57566 ) ) ;
#56327 = CARTESIAN_POINT ( 'NONE',  ( 0.9754642270333676590, 21.30186789325757246, 37.24735125696664539 ) ) ;
#56328 = CARTESIAN_POINT ( 'NONE',  ( 2.299652685299203636, 18.13764577205347805, -45.55554335869198468 ) ) ;
#56329 = AXIS2_PLACEMENT_3D ( 'NONE', #17962, #56148, #32364 ) ;
#56330 = ORIENTED_EDGE ( 'NONE', *, *, #22929, .F. ) ;
#56331 = B_SPLINE_CURVE_WITH_KNOTS ( 'NONE', 3,
 ( #54957, #7336, #22086, #27091 ),
 .UNSPECIFIED., .F., .F.,
 ( 4, 4 ),
 ( 0.000000000000000000, 0.004050076154993000749 ),
 .UNSPECIFIED. ) ;
#56332 = CARTESIAN_POINT ( 'NONE',  ( 0.9791128995231617171, -6.975674438753351581, -41.32405353266649684 ) ) ;
#56333 = ORIENTED_EDGE ( 'NONE', *, *, #50853, .F. ) ;
#56334 = CARTESIAN_POINT ( 'NONE',  ( 0.6846871229502899947, -28.47437962186153371, 38.52803883689291098 ) ) ;
#56335 = B_SPLINE_CURVE_WITH_KNOTS ( 'NONE', 3,
 ( #35871, #45578, #54940, #12073 ),
 .UNSPECIFIED., .F., .F.,
 ( 4, 4 ),
 ( 8.673617379884035472E-19, 0.004446298630425088438 ),
 .UNSPECIFIED. ) ;
#56336 = VERTEX_POINT ( 'NONE', #34472 ) ;
#56337 = EDGE_LOOP ( 'NONE', ( #46825, #38211 ) ) ;
#56338 = CARTESIAN_POINT ( 'NONE',  ( 1.227938101723748288, -42.43379953535180960, -6.439911493065006987 ) ) ;
#56339 = CARTESIAN_POINT ( 'NONE',  ( 0.9787284016396613495, -37.31945016035690799, 19.06815771535011095 ) ) ;
#56340 = CARTESIAN_POINT ( 'NONE',  ( 0.5782707292762442330, 28.40044722094953400, -37.32493739254866227 ) ) ;
#56341 = CARTESIAN_POINT ( 'NONE',  ( 4.226256110419179812, -29.23450101563807024, -32.80504839737084666 ) ) ;
#56342 = VERTEX_POINT ( 'NONE', #47949 ) ;
#56343 = CARTESIAN_POINT ( 'NONE',  ( 2.185380717157383135, 5.657694518177669885, 43.66703900891589285 ) ) ;
#56344 = CARTESIAN_POINT ( 'NONE',  ( 0.5806925824938506953, -46.06186276235258958, -8.804950948515241294 ) ) ;
#56345 = CARTESIAN_POINT ( 'NONE',  ( 3.727782113643637096, 0.7293963419152633687, 43.95731744411134656 ) ) ;
#56346 = ORIENTED_EDGE ( 'NONE', *, *, #15721, .F. ) ;
#56347 = ORIENTED_EDGE ( 'NONE', *, *, #16394, .F. ) ;
#56348 = CARTESIAN_POINT ( 'NONE',  ( 45.00000000000001421, 0.000000000000000000, 0.000000000000000000 ) ) ;
#56349 = LINE ( 'NONE', #32575, #41828 ) ;
#56350 = DIRECTION ( 'NONE',  ( 0.000000000000000000, 0.000000000000000000, 1.000000000000000000 ) ) ;
#56351 = CARTESIAN_POINT ( 'NONE',  ( 0.7954190325252785687, -34.61997719899462567, -33.39101560460790097 ) ) ;
#56352 = CARTESIAN_POINT ( 'NONE',  ( 3.221118495291108719, -34.08871765526027531, 27.79785510217824651 ) ) ;
#56353 = EDGE_CURVE ( 'NONE', #28471, #34340, #34383, .T. ) ;
#56354 = EDGE_LOOP ( 'NONE', ( #16003, #36192, #53052, #36942 ) ) ;
#56355 = CARTESIAN_POINT ( 'NONE',  ( 0.5836750258453369256, 47.46217286060751661, 6.431686642654920405 ) ) ;
#56356 = ADVANCED_FACE ( 'NONE', ( #5604 ), #31130, .F. ) ;
#56357 = CARTESIAN_POINT ( 'NONE',  ( 5.880360259849752858, 31.59460303415934845, 36.09847387447869238 ) ) ;
#56358 = CARTESIAN_POINT ( 'NONE',  ( 1.479689385636123067, 43.01073730641239479, -9.573939712912206801 ) ) ;
#56359 = CARTESIAN_POINT ( 'NONE',  ( 4.553261556744875094, -39.47791437445886942, -19.26223877088359515 ) ) ;
#56360 = AXIS2_PLACEMENT_3D ( 'NONE', #51043, #27257, #18172 ) ;
#56361 = CARTESIAN_POINT ( 'NONE',  ( 3.050102900204245682, -41.42303492486365002, -14.81747032362766880 ) ) ;
#56362 =( NAMED_UNIT ( * ) SI_UNIT ( $, .STERADIAN. ) SOLID_ANGLE_UNIT ( ) );
#56363 = CARTESIAN_POINT ( 'NONE',  ( 0.5998501479064708430, 48.10473956285918717, 0.5236536531316605680 ) ) ;
#56364 =( REPRESENTATION_RELATIONSHIP ('NONE','NONE', #44881, #19619 ) REPRESENTATION_RELATIONSHIP_WITH_TRANSFORMATION ( #23954 )SHAPE_REPRESENTATION_RELATIONSHIP( ) );
#56365 =( BOUNDED_SURFACE ( )  B_SPLINE_SURFACE ( 3, 1, ( 
 ( #43959, #20131 ),
 ( #39556, #15425 ),
 ( #44882, #49537 ),
 ( #58936, #57678 ) ),
 .UNSPECIFIED., .F., .F., .F. ) 
 B_SPLINE_SURFACE_WITH_KNOTS ( ( 4, 4 ),
 ( 2, 2 ),
 ( 0.000000000000000000, 1.000000000000000000 ),
 ( 0.000000000000000000, 1.000000000000000000 ),
 .UNSPECIFIED. ) 
 GEOMETRIC_REPRESENTATION_ITEM ( )  RATIONAL_B_SPLINE_SURFACE ( (
 ( 1.000000000000000000, 1.000000000000000000),
 ( 0.9953390228620291325, 0.8624445117761032620),
 ( 0.9953390228620291325, 0.8624445117761032620),
 ( 1.000000000000000000, 1.000000000000000000) ) ) 
 REPRESENTATION_ITEM ( '' )  SURFACE ( )  );
#56366 = ORIENTED_EDGE ( 'NONE', *, *, #25159, .T. ) ;
#56367 = CARTESIAN_POINT ( 'NONE',  ( 0.6000166863083106206, 49.04012132094733545, 2.624877622903676766 ) ) ;
#56368 = CARTESIAN_POINT ( 'NONE',  ( -6.077587904424778920, -18.27312872431383894, 6.073614082124997537 ) ) ;
#56369 = CARTESIAN_POINT ( 'NONE',  ( 2.643462169533600914, 25.20536747735779315, -40.89244134039086020 ) ) ;
#56371 = EDGE_CURVE ( 'NONE', #23457, #42423, #10039, .T. ) ;
#56370 = CARTESIAN_POINT ( 'NONE',  ( 0.6000166863083090663, 4.195342255946697740, 48.93079383234981350 ) ) ;
#56372 = CARTESIAN_POINT ( 'NONE',  ( 0.5848930533535030563, -45.92005787004946882, -9.519525597363942993 ) ) ;
#56373 = DIRECTION ( 'NONE',  ( 0.000000000000000000, 0.000000000000000000, -1.000000000000000000 ) ) ;
#56374 = EDGE_CURVE ( 'NONE', #37874, #30066, #55316, .T. ) ;
#56375 = B_SPLINE_CURVE_WITH_KNOTS ( 'NONE', 3,
 ( #50277, #26471, #27097, #45601, #45921, #21467, #21784, #40303, #32114, #55271, #40605, #60586, #2344, #17701, #54963, #46223, #22091, #12395, #31482 ),
 .UNSPECIFIED., .F., .F.,
 ( 4, 3, 3, 3, 3, 3, 4 ),
 ( 5.204170427930421283E-18, 0.0002724573126191779239, 0.0004086839781548503745, 0.0005449106435901876662, 0.0006811373090491533010, 0.0008459866663933717596, 0.001010840725717214016 ),
 .UNSPECIFIED. ) ;
#56376 = CARTESIAN_POINT ( 'NONE',  ( 4.963659409799330291, 43.98510776953407486, 8.262218268420630451 ) ) ;
#56377 = VECTOR ( 'NONE', #39822, 1000.000000000000227 ) ;
#56378 = CARTESIAN_POINT ( 'NONE',  ( 0.5834584762367746036, 22.69689635113398651, -41.03762767313761373 ) ) ;
#56379 = DIRECTION ( 'NONE',  ( 0.000000000000000000, 0.000000000000000000, -1.000000000000000000 ) ) ;
#56380 = VERTEX_POINT ( 'NONE', #59767 ) ;
#56381 = CARTESIAN_POINT ( 'NONE',  ( 0.7242003506640011246, 46.33602329577892931, -16.24760349279418392 ) ) ;
#56382 = CARTESIAN_POINT ( 'NONE',  ( 0.9789233960466703355, 20.02512277535910457, 36.81482289328764068 ) ) ;
#56383 = CARTESIAN_POINT ( 'NONE',  ( 0.5806925824938499181, -41.60618895332673617, -21.63671424046719594 ) ) ;
#56384 = CARTESIAN_POINT ( 'NONE',  ( 0.7764146366350267447, 42.82684524705668139, -19.12855979559951436 ) ) ;
#56385 = ORIENTED_EDGE ( 'NONE', *, *, #18044, .F. ) ;
#56386 = CARTESIAN_POINT ( 'NONE',  ( 4.549368137175248350, 8.582197505783829783, 42.06008734272398897 ) ) ;
#56387 = CARTESIAN_POINT ( 'NONE',  ( 0.9769922540276037015, -41.78318551423056704, -3.239901753065929757 ) ) ;
#56388 = ORIENTED_EDGE ( 'NONE', *, *, #35314, .T. ) ;
#56389 = DIRECTION ( 'NONE',  ( 1.836970198721031906E-16, -1.000000000000000000, 1.110223024625156540E-16 ) ) ;
#56390 = EDGE_CURVE ( 'NONE', #14899, #35341, #8958, .T. ) ;
#56391 = CARTESIAN_POINT ( 'NONE',  ( -2.739355103387248747, -10.90485690860409029, -10.19468796746063433 ) ) ;
#56392 = CARTESIAN_POINT ( 'NONE',  ( 4.975801465491694664, -8.787181743659814970, -47.10002938642139014 ) ) ;
#56393 = VERTEX_POINT ( 'NONE', #27185 ) ;
#56394 = CARTESIAN_POINT ( 'NONE',  ( 4.322998006666165516, -39.32552843303867718, 27.50295597456385366 ) ) ;
#56395 = EDGE_LOOP ( 'NONE', ( #34922, #19685, #26655, #13769, #49499, #49894 ) ) ;
#56396 = ORIENTED_EDGE ( 'NONE', *, *, #39031, .T. ) ;
#56397 = CARTESIAN_POINT ( 'NONE',  ( 2.648799415243696664, 23.90046839033458426, -42.81687837771707450 ) ) ;
#56398 = FACE_OUTER_BOUND ( 'NONE', #12355, .T. ) ;
#56399 = ORIENTED_EDGE ( 'NONE', *, *, #39231, .F. ) ;
#56400 = CARTESIAN_POINT ( 'NONE',  ( 0.6845945791218034371, -14.72268806499663718, 44.53817437720981331 ) ) ;
#56401 = AXIS2_PLACEMENT_3D ( 'NONE', #49666, #6722, #40309 ) ;
#56402 = ORIENTED_EDGE ( 'NONE', *, *, #26805, .T. ) ;
#56403 = CARTESIAN_POINT ( 'NONE',  ( 0.5839879882074159312, 2.012401425053789955E-05, 47.89596766821753704 ) ) ;
#56404 = B_SPLINE_CURVE_WITH_KNOTS ( 'NONE', 3,
 ( #54178, #29777, #35428, #21006 ),
 .UNSPECIFIED., .F., .F.,
 ( 4, 4 ),
 ( 0.000000000000000000, 0.004442905043737213101 ),
 .UNSPECIFIED. ) ;
#56405 = CARTESIAN_POINT ( 'NONE',  ( 0.8560838555295223751, 36.24009790160352651, -29.78301761346427767 ) ) ;
#56406 = B_SPLINE_CURVE_WITH_KNOTS ( 'NONE', 3,
 ( #31337, #35440, #50440, #54497 ),
 .UNSPECIFIED., .F., .F.,
 ( 4, 4 ),
 ( 1.430489624538199204E-17, 0.005004741218457437087 ),
 .UNSPECIFIED. ) ;
#56407 = CARTESIAN_POINT ( 'NONE',  ( -6.078726893082806448, -14.66019907464893635, -12.48489504803234418 ) ) ;
#56408 = VERTEX_POINT ( 'NONE', #17481 ) ;
#56409 = CARTESIAN_POINT ( 'NONE',  ( 0.9741495583595165542, -16.05424148287297470, -39.79188455996737872 ) ) ;
#56410 = CARTESIAN_POINT ( 'NONE',  ( 4.335381028904201628, 29.74326630871473398, -38.92422069808487350 ) ) ;
#56411 = CARTESIAN_POINT ( 'NONE',  ( 0.5837799406558221715, -44.33108515927273174, -15.29700749096085843 ) ) ;
#56412 = CARTESIAN_POINT ( 'NONE',  ( 0.5830082357119579228, 16.59956988142198497, 43.85984854841750291 ) ) ;
#56413 = EDGE_LOOP ( 'NONE', ( #9135, #7552, #12653, #2018, #16271 ) ) ;
#56414 = FACE_OUTER_BOUND ( 'NONE', #61873, .T. ) ;
#56415 = CARTESIAN_POINT ( 'NONE',  ( 0.1158403557922069033, -31.67019805176805747, -30.72358804803900867 ) ) ;
#56416 = STYLED_ITEM ( 'NONE', ( #26699 ), #52453 ) ;
#56417 = ORIENTED_EDGE ( 'NONE', *, *, #10119, .F. ) ;
#56418 = FACE_OUTER_BOUND ( 'NONE', #57677, .T. ) ;
#56419 = VERTEX_POINT ( 'NONE', #2434 ) ;
#56420 = CARTESIAN_POINT ( 'NONE',  ( 0.1139756605157203617, -12.17292277066103701, 42.41196966558549519 ) ) ;
#56421 = CARTESIAN_POINT ( 'NONE',  ( 0.6021448801613057400, 46.68736458834386838, -15.22600165578615083 ) ) ;
#56422 = EDGE_LOOP ( 'NONE', ( #52617, #38815, #3993, #52808 ) ) ;
#56423 = CARTESIAN_POINT ( 'NONE',  ( 4.975801465491695552, 14.85979367497174408, -45.55012473237738391 ) ) ;
#56424 = CARTESIAN_POINT ( 'NONE',  ( -6.015611763856276717, -18.19956619163661671, 4.882992715191235789 ) ) ;
#56425 = CARTESIAN_POINT ( 'NONE',  ( 2.624215991343608501, -32.93378783738824467, -34.92983774303001354 ) ) ;
#56426 = CARTESIAN_POINT ( 'NONE',  ( 0.5837799406558230597, -1.658065787041380634, -46.86677253047242431 ) ) ;
#56427 = EDGE_CURVE ( 'NONE', #52560, #49823, #12755, .T. ) ;
#56428 = ORIENTED_EDGE ( 'NONE', *, *, #36892, .T. ) ;
#56429 = CARTESIAN_POINT ( 'NONE',  ( 50.15577769773999961, 0.000000000000000000, 3.000000000000000000 ) ) ;
#56430 = CARTESIAN_POINT ( 'NONE',  ( 4.549368137175248350, 40.71620287708344677, -13.59764261105707739 ) ) ;
#56431 = EDGE_CURVE ( 'NONE', #56955, #34923, #31896, .T. ) ;
#56432 = CARTESIAN_POINT ( 'NONE',  ( 5.880360259849752858, 43.04573319267444731, -21.17507050419470715 ) ) ;
#56433 = FACE_OUTER_BOUND ( 'NONE', #36406, .T. ) ;
#56434 = EDGE_CURVE ( 'NONE', #59176, #18115, #3056, .T. ) ;
#56435 = FACE_OUTER_BOUND ( 'NONE', #30325, .T. ) ;
#56436 = DIRECTION ( 'NONE',  ( -1.000000000000000000, -0.000000000000000000, -0.000000000000000000 ) ) ;
#56437 =( BOUNDED_SURFACE ( )  B_SPLINE_SURFACE ( 3, 1, ( 
 ( #20635, #39770 ),
 ( #11238, #21562 ),
 ( #59137, #49750 ),
 ( #15331, #58207 ) ),
 .UNSPECIFIED., .F., .F., .F. ) 
 B_SPLINE_SURFACE_WITH_KNOTS ( ( 4, 4 ),
 ( 2, 2 ),
 ( 0.000000000000000000, 1.000000000000000000 ),
 ( 0.000000000000000000, 1.000000000000000000 ),
 .UNSPECIFIED. ) 
 GEOMETRIC_REPRESENTATION_ITEM ( )  RATIONAL_B_SPLINE_SURFACE ( (
 ( 1.000000000000000000, 1.000000000000000000),
 ( 0.9754377213608244057, 0.9999580625633939235),
 ( 0.9754377213608244057, 0.9999580625633939235),
 ( 1.000000000000000000, 1.000000000000000000) ) ) 
 REPRESENTATION_ITEM ( '' )  SURFACE ( )  );
#56438 = CARTESIAN_POINT ( 'NONE',  ( 0.6041374136657475802, -29.14743607025058125, -38.27243465845331372 ) ) ;
#56439 = CARTESIAN_POINT ( 'NONE',  ( -2.569797478183790229, 11.33042594333535646, 9.259773107243104207 ) ) ;
#56440 = CARTESIAN_POINT ( 'NONE',  ( 0.9790850452238877288, -12.36814557455428876, 40.04205670679053952 ) ) ;
#56441 = CARTESIAN_POINT ( 'NONE',  ( 0.1073791018717578927, -21.98088480513690968, 37.10214135362851096 ) ) ;
#56442 = CARTESIAN_POINT ( 'NONE',  ( 1.231276596079881935, -37.02495017545860634, -19.65781868679418309 ) ) ;
#56443 = ADVANCED_FACE ( 'NONE', ( #22183 ), #55999, .F. ) ;
#56444 = CARTESIAN_POINT ( 'NONE',  ( 0.6845945791218023269, 42.84081778543567509, -19.10682737110073859 ) ) ;
#56445 = CARTESIAN_POINT ( 'NONE',  ( 4.834790513006553603, 34.26126461650199673, -32.53851698836949424 ) ) ;
#56446 = CARTESIAN_POINT ( 'NONE',  ( 1.227938101723756947, -41.66816631169184859, -10.28900963485423858 ) ) ;
#56447 = CARTESIAN_POINT ( 'NONE',  ( 2.533389852662419894, -21.44996906063816056, 38.43630261915527768 ) ) ;
#56448 = CARTESIAN_POINT ( 'NONE',  ( 5.960721111146673579, -14.50930005615006912, -14.51823969584094698 ) ) ;
#56449 = CIRCLE ( 'NONE', #2440, 2.649999999999999467 ) ;
#56450 = CARTESIAN_POINT ( 'NONE',  ( 0.5837799406558222826, 45.20568596181698240, -12.47756011000493892 ) ) ;
#56451 = CARTESIAN_POINT ( 'NONE',  ( 0.9730545539215883499, 11.59290486963506517, 41.31259007387235727 ) ) ;
#56453 = ORIENTED_EDGE ( 'NONE', *, *, #51493, .T. ) ;
#56452 = CARTESIAN_POINT ( 'NONE',  ( 4.834790513006553603, -39.34655703395242909, -26.16176199146973147 ) ) ;
#56455 = ORIENTED_EDGE ( 'NONE', *, *, #26602, .T. ) ;
#56454 = B_SPLINE_CURVE_WITH_KNOTS ( 'NONE', 3,
 ( #23024, #33047, #28022, #27712 ),
 .UNSPECIFIED., .F., .F.,
 ( 4, 4 ),
 ( 2.189128766608093472E-17, 0.004559932413162188537 ),
 .UNSPECIFIED. ) ;
#56456 = CARTESIAN_POINT ( 'NONE',  ( 0.6016118706126977189, -39.56281023115544571, 29.09183908585898592 ) ) ;
#56457 = DIRECTION ( 'NONE',  ( 1.000000000000000000, 0.000000000000000000, 0.000000000000000000 ) ) ;
#56458 = CARTESIAN_POINT ( 'NONE',  ( 0.8557997880470606944, -34.51495345639572321, 33.22501220301889191 ) ) ;
#56459 = ORIENTED_EDGE ( 'NONE', *, *, #46970, .F. ) ;
#56460 = ORIENTED_EDGE ( 'NONE', *, *, #8769, .F. ) ;
#56461 = CARTESIAN_POINT ( 'NONE',  ( 0.1119898979215350199, -23.35186511842599089, -37.43863918123450674 ) ) ;
#56462 = VECTOR ( 'NONE', #54960, 1000.000000000000114 ) ;
#56463 = CARTESIAN_POINT ( 'NONE',  ( 0.9754292580325134576, -39.39482823006320444, -14.29597760308189258 ) ) ;
#56464 = ORIENTED_EDGE ( 'NONE', *, *, #5501, .T. ) ;
#56465 = ORIENTED_EDGE ( 'NONE', *, *, #12781, .F. ) ;
#56466 = CARTESIAN_POINT ( 'NONE',  ( 0.6029303876144825880, -38.08638053211517871, -29.38970229176890570 ) ) ;
#56467 = CARTESIAN_POINT ( 'NONE',  ( 0.8560838555295223751, 3.785103201470721768, -46.75516899590834186 ) ) ;
#56468 = CARTESIAN_POINT ( 'NONE',  ( 0.9762797500689124330, -1.905951756780080775, -41.86516610604251554 ) ) ;
#56469 = VERTEX_POINT ( 'NONE', #50067 ) ;
#56470 = EDGE_CURVE ( 'NONE', #18514, #28003, #60364, .T. ) ;
#56471 = ORIENTED_EDGE ( 'NONE', *, *, #20731, .T. ) ;
#56472 = CARTESIAN_POINT ( 'NONE',  ( 0.5832367798473397924, -12.13303976268028350, -46.33367954572893410 ) ) ;
#56473 = VERTEX_POINT ( 'NONE', #35685 ) ;
#56474 = CARTESIAN_POINT ( 'NONE',  ( 0.2279481005628783696, -23.51699569010370894, 37.32900214022007646 ) ) ;
#56475 = CARTESIAN_POINT ( 'NONE',  ( -6.015611763856276717, 11.47596948473810841, 14.94556629257429492 ) ) ;
#56476 = EDGE_CURVE ( 'NONE', #60419, #6142, #32606, .T. ) ;
#56477 = CARTESIAN_POINT ( 'NONE',  ( 0.1092565886968784594, -30.71235995742719993, -30.27341312544103857 ) ) ;
#56478 = ORIENTED_EDGE ( 'NONE', *, *, #33987, .F. ) ;
#56479 = VECTOR ( 'NONE', #22807, 1000.000000000000114 ) ;
#56480 = CARTESIAN_POINT ( 'NONE',  ( 0.6029303876144825880, -48.10727438003475953, -0.1308990448394030115 ) ) ;
#56481 = ORIENTED_EDGE ( 'NONE', *, *, #45193, .T. ) ;
#56482 = ADVANCED_FACE ( 'NONE', ( #36295, #7123 ), #41610, .T. ) ;
#56483 = ORIENTED_EDGE ( 'NONE', *, *, #11958, .F. ) ;
#56484 = CARTESIAN_POINT ( 'NONE',  ( 0.5806925824938511393, 40.62497527030930655, 23.42720099863236882 ) ) ;
#56485 = ORIENTED_EDGE ( 'NONE', *, *, #24150, .F. ) ;
#56486 = CARTESIAN_POINT ( 'NONE',  ( 1.479689385636123067, 34.30196355977874845, 27.65789473570436385 ) ) ;
#56487 = CARTESIAN_POINT ( 'NONE',  ( 0.8760168074886960365, -0.8912768426709578584, 48.09529047980636562 ) ) ;
#56488 = DIRECTION ( 'NONE',  ( 0.07906939808003035641, -0.2232318573464372458, -0.9715531730960079715 ) ) ;
#56489 = CARTESIAN_POINT ( 'NONE',  ( 0.7048096507298635682, -29.95256433478701297, -37.64898672361943710 ) ) ;
#56490 = DIRECTION ( 'NONE',  ( 0.000000000000000000, 0.000000000000000000, 1.000000000000000000 ) ) ;
#56491 = EDGE_LOOP ( 'NONE', ( #41237, #39748, #31525, #37956 ) ) ;
#56492 = DIRECTION ( 'NONE',  ( -1.000000000000000000, -0.000000000000000000, -0.000000000000000000 ) ) ;
#56493 = CARTESIAN_POINT ( 'NONE',  ( 4.975610109902397937, -47.89734868211986907, 9.914302615978730415 ) ) ;
#56494 = CARTESIAN_POINT ( 'NONE',  ( 3.680974057930773036, 36.90739001595131441, 30.65154904503192412 ) ) ;
#56495 = CONICAL_SURFACE ( 'NONE', #49834, 42.08604991992415023, 1.569615340895231137 ) ;
#56496 = ORIENTED_EDGE ( 'NONE', *, *, #19120, .F. ) ;
#56497 = CARTESIAN_POINT ( 'NONE',  ( -6.077587904424778920, 12.01079512011132522, 15.05114022181178335 ) ) ;
#56498 = CARTESIAN_POINT ( 'NONE',  ( 4.999999999999986677, 58.44237546506807490, 54.69470952477956871 ) ) ;
#56499 = CARTESIAN_POINT ( 'NONE',  ( 5.895596859100789899, 3.341829471547073549, -19.83331437242869910 ) ) ;
#56500 = CARTESIAN_POINT ( 'NONE',  ( 0.7044674535452954967, -34.68719619958476130, -34.76494128604877432 ) ) ;
#56501 = ADVANCED_FACE ( 'NONE', ( #17793 ), #35174, .F. ) ;
#56503 = ORIENTED_EDGE ( 'NONE', *, *, #13597, .F. ) ;
#56502 = AXIS2_PLACEMENT_3D ( 'NONE', #21808, #8008, #46243 ) ;
#56504 = ORIENTED_EDGE ( 'NONE', *, *, #25437, .F. ) ;
#56505 = CARTESIAN_POINT ( 'NONE',  ( 5.838029081930957709, 38.93046761018084112, -26.74852799324816743 ) ) ;
#56506 = CARTESIAN_POINT ( 'NONE',  ( 0.1104177457020373010, -42.75487793940128256, 5.633723015004153289 ) ) ;
#56507 = CARTESIAN_POINT ( 'NONE',  ( 4.975610109902397937, 47.45567470742105343, -11.84940273605426242 ) ) ;
#56508 = AXIS2_PLACEMENT_3D ( 'NONE', #21843, #3326, #8338 ) ;
#56509 = CARTESIAN_POINT ( 'NONE',  ( 0.5835871038041848813, -30.17293921915137034, -35.90025336650005272 ) ) ;
#56510 = EDGE_CURVE ( 'NONE', #12923, #60397, #57528, .T. ) ;
#56511 = CARTESIAN_POINT ( 'NONE',  ( 5.880360259849752858, 9.405269135695244032, -47.04104239318758118 ) ) ;
#56512 = CARTESIAN_POINT ( 'NONE',  ( 4.956653778116975495, 8.845409907520915382, 47.27023054223757015 ) ) ;
#56513 = CARTESIAN_POINT ( 'NONE',  ( 4.956653778116961284, 40.28700667097682953, 26.26162724282386662 ) ) ;
#56514 = FACE_OUTER_BOUND ( 'NONE', #438, .T. ) ;
#56515 = FACE_OUTER_BOUND ( 'NONE', #15124, .T. ) ;
#56516 = DIRECTION ( 'NONE',  ( 0.000000000000000000, 0.000000000000000000, -1.000000000000000000 ) ) ;
#56517 =( BOUNDED_SURFACE ( )  B_SPLINE_SURFACE ( 3, 1, ( 
 ( #1216, #48238 ),
 ( #47618, #4981 ),
 ( #10025, #20351 ),
 ( #53222, #19131 ) ),
 .UNSPECIFIED., .F., .F., .F. ) 
 B_SPLINE_SURFACE_WITH_KNOTS ( ( 4, 4 ),
 ( 2, 2 ),
 ( 0.000000000000000000, 1.000000000000000000 ),
 ( 0.000000000000000000, 1.000000000000000000 ),
 .UNSPECIFIED. ) 
 GEOMETRIC_REPRESENTATION_ITEM ( )  RATIONAL_B_SPLINE_SURFACE ( (
 ( 1.000000000000000000, 1.000000000000000000),
 ( 0.9732289882329797637, 0.9999525324661233672),
 ( 0.9732289882329797637, 0.9999525324661233672),
 ( 1.000000000000000000, 1.000000000000000000) ) ) 
 REPRESENTATION_ITEM ( '' )  SURFACE ( )  );
#56518 = CARTESIAN_POINT ( 'NONE',  ( 0.5809828226811626362, -18.83114015454730961, 44.03860873105688967 ) ) ;
#56519 = ORIENTED_EDGE ( 'NONE', *, *, #36666, .F. ) ;
#56520 = CARTESIAN_POINT ( 'NONE',  ( 4.553261556744875094, -43.07273893850278768, -8.618510669438375515 ) ) ;
#56521 = CARTESIAN_POINT ( 'NONE',  ( 4.962356264823608143, -41.76635909427997717, 5.177532797578748180 ) ) ;
#56522 = CARTESIAN_POINT ( 'NONE',  ( 0.7242486021783856032, -13.18373570521661975, -47.29905469699126286 ) ) ;
#56523 = CARTESIAN_POINT ( 'NONE',  ( 0.6028777368367060907, -39.30322683055775457, -29.44140265029500725 ) ) ;
#56524 = EDGE_CURVE ( 'NONE', #26869, #8116, #28366, .T. ) ;
#56525 = DIRECTION ( 'NONE',  ( 0.000000000000000000, 0.000000000000000000, 1.000000000000000000 ) ) ;
#56526 = DIRECTION ( 'NONE',  ( 0.000000000000000000, 0.000000000000000000, 1.000000000000000000 ) ) ;
#56527 = CARTESIAN_POINT ( 'NONE',  ( 4.956653778116966613, 5.889412876890086925E-15, 48.09070567114147110 ) ) ;
#56528 = CARTESIAN_POINT ( 'NONE',  ( 0.5838002273316434954, 12.26477999444068345, 46.29900743592982337 ) ) ;
#56529 = B_SPLINE_CURVE_WITH_KNOTS ( 'NONE', 3,
 ( #50309, #21195, #40331, #40638 ),
 .UNSPECIFIED., .F., .F.,
 ( 4, 4 ),
 ( 2.012794395885733147E-17, 0.004444306975806115029 ),
 .UNSPECIFIED. ) ;
#56530 = CARTESIAN_POINT ( 'NONE',  ( -6.079354080745853928, 16.77752703747136920, -9.450266755763003346 ) ) ;
#56531 =( BOUNDED_SURFACE ( )  B_SPLINE_SURFACE ( 3, 1, ( 
 ( #40138, #25376 ),
 ( #2167, #11285 ),
 ( #16292, #29762 ),
 ( #15689, #48875 ) ),
 .UNSPECIFIED., .F., .F., .F. ) 
 B_SPLINE_SURFACE_WITH_KNOTS ( ( 4, 4 ),
 ( 2, 2 ),
 ( 0.000000000000000000, 1.000000000000000000 ),
 ( 0.000000000000000000, 1.000000000000000000 ),
 .UNSPECIFIED. ) 
 GEOMETRIC_REPRESENTATION_ITEM ( )  RATIONAL_B_SPLINE_SURFACE ( (
 ( 1.000000000000000000, 1.000000000000000000),
 ( 0.9953485035131437453, 0.8621029689291515030),
 ( 0.9953485035131437453, 0.8621029689291515030),
 ( 1.000000000000000000, 1.000000000000000000) ) ) 
 REPRESENTATION_ITEM ( '' )  SURFACE ( )  );
#56533 = ORIENTED_EDGE ( 'NONE', *, *, #26112, .T. ) ;
#56532 = CARTESIAN_POINT ( 'NONE',  ( 0.5806925824938499181, -8.338382001838064994, 46.14860504863594315 ) ) ;
#56534 = ORIENTED_EDGE ( 'NONE', *, *, #59279, .F. ) ;
#56535 = CARTESIAN_POINT ( 'NONE',  ( 0.1158403557922069033, -7.079586543883442218, 43.55249432066416659 ) ) ;
#56536 = CARTESIAN_POINT ( 'NONE',  ( 0.1098349054025746785, 39.75970464594242060, 16.69989664087468739 ) ) ;
#56537 = CARTESIAN_POINT ( 'NONE',  ( 5.838029081930955932, -40.65053383315998303, 24.05408816047773968 ) ) ;
#56538 =( BOUNDED_SURFACE ( )  B_SPLINE_SURFACE ( 3, 1, ( 
 ( #46042, #45723 ),
 ( #16586, #39807 ),
 ( #21589, #1847 ),
 ( #40412, #2773 ) ),
 .UNSPECIFIED., .F., .F., .F. ) 
 B_SPLINE_SURFACE_WITH_KNOTS ( ( 4, 4 ),
 ( 2, 2 ),
 ( 0.000000000000000000, 1.000000000000000000 ),
 ( 0.000000000000000000, 1.000000000000000000 ),
 .UNSPECIFIED. ) 
 GEOMETRIC_REPRESENTATION_ITEM ( )  RATIONAL_B_SPLINE_SURFACE ( (
 ( 1.000000000000000000, 1.000000000000000000),
 ( 0.7211978278499970862, 0.9934217856018976445),
 ( 0.7211978278499970862, 0.9934217856018976445),
 ( 1.000000000000000000, 1.000000000000000000) ) ) 
 REPRESENTATION_ITEM ( '' )  SURFACE ( )  );
#56539 = ORIENTED_EDGE ( 'NONE', *, *, #46286, .T. ) ;
#56540 = CARTESIAN_POINT ( 'NONE',  ( 4.956445790443988031, 0.000000000000000000, 0.000000000000000000 ) ) ;
#56541 = CARTESIAN_POINT ( 'NONE',  ( 4.956653778116488773, 2.599733001513538255, 48.02038484091099235 ) ) ;
#56542 = CARTESIAN_POINT ( 'NONE',  ( 0.6030672727741701600, -44.41203814406394912, -18.49051564326117969 ) ) ;
#56543 = ORIENTED_EDGE ( 'NONE', *, *, #19728, .T. ) ;
#56544 = ORIENTED_EDGE ( 'NONE', *, *, #4069, .F. ) ;
#56545 = AXIS2_PLACEMENT_3D ( 'NONE', #16136, #30214, #44354 ) ;
#56546 = CARTESIAN_POINT ( 'NONE',  ( 0.9791128995231614951, 24.85527234537524777, -33.74244909432907491 ) ) ;
#56547 = DIRECTION ( 'NONE',  ( -0.1024043820194934368, -0.9878630899050870884, 0.1167898032637235545 ) ) ;
#56549 = CARTESIAN_POINT ( 'NONE',  ( 0.3676999524040366896, 37.41430475689384139, 23.36921870497834774 ) ) ;
#56548 = VECTOR ( 'NONE', #29508, 1000.000000000000000 ) ;
#56550 = CARTESIAN_POINT ( 'NONE',  ( 0.9789233960466712237, 32.97123601430887874, -25.86956363221230148 ) ) ;
#56551 = EDGE_CURVE ( 'NONE', #60958, #40436, #19338, .T. ) ;
#56553 = CARTESIAN_POINT ( 'NONE',  ( 0.5997462898726536595, -35.63787911784795170, 33.78599121123970406 ) ) ;
#56552 = VECTOR ( 'NONE', #56116, 1000.000000000000114 ) ;
#56554 = EDGE_CURVE ( 'NONE', #32580, #35399, #11986, .T. ) ;
#56555 = CARTESIAN_POINT ( 'NONE',  ( 0.6016118706126977189, 48.98309811941713576, 3.493873696555625852 ) ) ;
#56556 = FACE_OUTER_BOUND ( 'NONE', #39426, .T. ) ;
#56557 = ORIENTED_EDGE ( 'NONE', *, *, #43119, .T. ) ;
#56558 = EDGE_CURVE ( 'NONE', #18521, #18160, #49341, .T. ) ;
#56559 = ADVANCED_FACE ( 'NONE', ( #23110 ), #60379, .F. ) ;
#56560 = DIRECTION ( 'NONE',  ( -0.1011922191286467460, 0.8049255303601348110, -0.5846836968500794818 ) ) ;
#56561 = DIRECTION ( 'NONE',  ( -1.000000000000000000, -0.000000000000000000, -0.000000000000000000 ) ) ;
#56562 = VERTEX_POINT ( 'NONE', #37221 ) ;
#56563 = CARTESIAN_POINT ( 'NONE',  ( 0.9791128995231621612, -37.40658675588493054, -18.89668493468148824 ) ) ;
#56564 = EDGE_CURVE ( 'NONE', #24212, #5544, #48563, .T. ) ;
#56565 = CARTESIAN_POINT ( 'NONE',  ( 0.5980271706414711508, -43.13192993667259856, 23.48799401353017302 ) ) ;
#56566 = CARTESIAN_POINT ( 'NONE',  ( 3.727782113643637540, 38.63515341906938261, -20.97862474498617757 ) ) ;
#56567 = CARTESIAN_POINT ( 'NONE',  ( 4.833616638992208614, 45.44786513329586342, 8.578242093415909153 ) ) ;
#56568 = ORIENTED_EDGE ( 'NONE', *, *, #11878, .F. ) ;
#56569 = ORIENTED_EDGE ( 'NONE', *, *, #27906, .T. ) ;
#56570 = CARTESIAN_POINT ( 'NONE',  ( 1.157644175074336923, -31.63536299616512437, 27.49920150804474162 ) ) ;
#56571 = CARTESIAN_POINT ( 'NONE',  ( 0.5819845901640493535, 41.25023214430201079, 24.34012668949501901 ) ) ;
#56572 = CARTESIAN_POINT ( 'NONE',  ( -2.739355103387248747, -14.50431811309219832, -3.531617621606664592 ) ) ;
#56573 = ADVANCED_FACE ( 'NONE', ( #40008 ), #49367, .F. ) ;
#56574 = ORIENTED_EDGE ( 'NONE', *, *, #23189, .F. ) ;
#56575 = CARTESIAN_POINT ( 'NONE',  ( 5.860006189529234355, 31.78942168514615219, -36.27483683749403554 ) ) ;
#56576 = VERTEX_POINT ( 'NONE', #49064 ) ;
#56577 = CARTESIAN_POINT ( 'NONE',  ( 0.000000000000000000, 0.000000000000000000, 0.000000000000000000 ) ) ;
#56578 = CARTESIAN_POINT ( 'NONE',  ( 0.5834584762367733823, 27.67094651009132278, 37.86231250529817061 ) ) ;
#56579 = EDGE_CURVE ( 'NONE', #30663, #52112, #32947, .T. ) ;
#56580 = CARTESIAN_POINT ( 'NONE',  ( 0.6008123274975391004, -13.55448476036326610, -47.19989930115886523 ) ) ;
#56581 = ORIENTED_EDGE ( 'NONE', *, *, #13379, .T. ) ;
#56582 = CARTESIAN_POINT ( 'NONE',  ( 1.231276596079881047, 33.41651732065586344, -25.31033664684003170 ) ) ;
#56583 = DIRECTION ( 'NONE',  ( 0.09835009131224552170, 0.9855991218957030897, -0.1375559175655191035 ) ) ;
#56584 = CARTESIAN_POINT ( 'NONE',  ( 2.526464513654345989, -42.96196573359002002, 1.212545078562630607 ) ) ;
#56585 = ORIENTED_EDGE ( 'NONE', *, *, #40745, .T. ) ;
#56586 = CARTESIAN_POINT ( 'NONE',  ( 0.5839880159502339740, -18.28706857028339527, -44.26747004398436758 ) ) ;
#56587 = CARTESIAN_POINT ( 'NONE',  ( 0.1139756605157200980, 33.33919145751784896, -28.90421306062476958 ) ) ;
#56588 = FACE_OUTER_BOUND ( 'NONE', #18300, .T. ) ;
#56589 = CARTESIAN_POINT ( 'NONE',  ( 0.6017666602106488405, 47.64919188470828715, -6.625262199740582503 ) ) ;
#56590 = CARTESIAN_POINT ( 'NONE',  ( 0.1073791018717483448, 41.77800844988500018, 10.69234304550068337 ) ) ;
#56591 = ORIENTED_EDGE ( 'NONE', *, *, #51367, .F. ) ;
#56592 = CARTESIAN_POINT ( 'NONE',  ( -6.001507490154110336, 14.95933060264873937, 11.45906331631436359 ) ) ;
#56593 = CARTESIAN_POINT ( 'NONE',  ( 2.281448460670571166, -46.66132715497955274, -11.14236343022421316 ) ) ;
#56594 = ORIENTED_EDGE ( 'NONE', *, *, #8630, .F. ) ;
#56595 = CONICAL_SURFACE ( 'NONE', #6525, 4.000000000000000000, 1.047197551196595855 ) ;
#56596 = CARTESIAN_POINT ( 'NONE',  ( 2.282816707992308736, -29.31214480238963915, 36.70551911486484897 ) ) ;
#56597 = FACE_OUTER_BOUND ( 'NONE', #40079, .T. ) ;
#56598 = CIRCLE ( 'NONE', #29591, 42.92674063221959813 ) ;
#56599 = CARTESIAN_POINT ( 'NONE',  ( 0.9730545539215883499, 5.099196237955498923, -42.60426903087348194 ) ) ;
#56600 = ADVANCED_FACE ( 'NONE', ( #44096 ), #14642, .T. ) ;
#56601 = CARTESIAN_POINT ( 'NONE',  ( 4.975801465491695552, -39.51822597168514051, 27.09127437476313816 ) ) ;
#56602 = FACE_OUTER_BOUND ( 'NONE', #61783, .T. ) ;
#56603 = CARTESIAN_POINT ( 'NONE',  ( 52.49678397332792201, 15.40128748659475377, 1.750934580577085287 ) ) ;
#56604 = DIRECTION ( 'NONE',  ( 1.000000000000000000, 5.742781273388963137E-17, -1.005019234048045307E-16 ) ) ;
#56605 = CARTESIAN_POINT ( 'NONE',  ( 0.9730545539215883499, -41.57420493492393376, 10.61654491617549034 ) ) ;
#56606 = EDGE_CURVE ( 'NONE', #52461, #40793, #25256, .T. ) ;
#56607 = CARTESIAN_POINT ( 'NONE',  ( 10.00000000000000888, 9.184850993605147156E-15, -75.00000000000001421 ) ) ;
#56608 = CARTESIAN_POINT ( 'NONE',  ( 5.200000000000002842, 3.306546357697854226E-16, 2.700000000000000622 ) ) ;
#56609 = VECTOR ( 'NONE', #54192, 1000.000000000000000 ) ;
#56610 = CARTESIAN_POINT ( 'NONE',  ( 0.1073791018717578927, -6.109314776653017809, 42.68962945260943087 ) ) ;
#56611 = ORIENTED_EDGE ( 'NONE', *, *, #4871, .F. ) ;
#56612 = CARTESIAN_POINT ( 'NONE',  ( 0.8760168074887076939, 0.8912768426699595459, 48.09529047980637984 ) ) ;
#56613 = CARTESIAN_POINT ( 'NONE',  ( 4.967162193818130511, 42.16965968614205451, -8.839793687084773310 ) ) ;
#56614 = CARTESIAN_POINT ( 'NONE',  ( 0.5807400328401637335, 47.89582301953903709, -0.5448834511091659172 ) ) ;
#56615 = DIRECTION ( 'NONE',  ( 0.000000000000000000, 0.000000000000000000, 1.000000000000000000 ) ) ;
#56616 = DIRECTION ( 'NONE',  ( 0.000000000000000000, 0.000000000000000000, 1.000000000000000000 ) ) ;
#56617 = CARTESIAN_POINT ( 'NONE',  ( 0.8560838555295223751, -46.73345513967318965, 4.044379407262076676 ) ) ;
#56618 =( BOUNDED_SURFACE ( )  B_SPLINE_SURFACE ( 3, 1, ( 
 ( #61135, #18257 ),
 ( #32664, #51743 ),
 ( #38002, #57056 ),
 ( #53283, #24797 ) ),
 .UNSPECIFIED., .F., .F., .F. ) 
 B_SPLINE_SURFACE_WITH_KNOTS ( ( 4, 4 ),
 ( 2, 2 ),
 ( 0.000000000000000000, 1.000000000000000000 ),
 ( 0.000000000000000000, 1.000000000000000000 ),
 .UNSPECIFIED. ) 
 GEOMETRIC_REPRESENTATION_ITEM ( )  RATIONAL_B_SPLINE_SURFACE ( (
 ( 1.000000000000000000, 1.000000000000000000),
 ( 0.9953390228620291325, 0.8624445117760984880),
 ( 0.9953390228620291325, 0.8624445117760984880),
 ( 1.000000000000000000, 1.000000000000000000) ) ) 
 REPRESENTATION_ITEM ( '' )  SURFACE ( )  );
#56619 = ORIENTED_EDGE ( 'NONE', *, *, #5204, .F. ) ;
#56620 = CARTESIAN_POINT ( 'NONE',  ( 3.240649175237396484, 38.80770280631830360, 20.71779718730070385 ) ) ;
#56621 =( BOUNDED_SURFACE ( )  B_SPLINE_SURFACE ( 3, 1, ( 
 ( #50699, #4002 ),
 ( #27523, #46048 ),
 ( #27217, #51315 ),
 ( #26594, #51627 ) ),
 .UNSPECIFIED., .F., .F., .F. ) 
 B_SPLINE_SURFACE_WITH_KNOTS ( ( 4, 4 ),
 ( 2, 2 ),
 ( 0.000000000000000000, 1.000000000000000000 ),
 ( 0.000000000000000000, 1.000000000000000000 ),
 .UNSPECIFIED. ) 
 GEOMETRIC_REPRESENTATION_ITEM ( )  RATIONAL_B_SPLINE_SURFACE ( (
 ( 1.000000000000000000, 1.000000000000000000),
 ( 0.7211978278499970862, 0.9934217856018976445),
 ( 0.7211978278499970862, 0.9934217856018976445),
 ( 1.000000000000000000, 1.000000000000000000) ) ) 
 REPRESENTATION_ITEM ( '' )  SURFACE ( )  );
#56622 = CARTESIAN_POINT ( 'NONE',  ( -19.96581960764538266, -7.972194200162546096, -0.6786982475873951648 ) ) ;
#56623 = ORIENTED_EDGE ( 'NONE', *, *, #14244, .F. ) ;
#56624 = EDGE_CURVE ( 'NONE', #46800, #23080, #20181, .T. ) ;
#56625 = CARTESIAN_POINT ( 'NONE',  ( 0.9762797500689124330, 32.57381952463267538, -26.36799322592379369 ) ) ;
#56626 = EDGE_CURVE ( 'NONE', #34842, #46672, #2957, .T. ) ;
#56627 = CARTESIAN_POINT ( 'NONE',  ( 3.660176727303406707, -42.51126973288297251, 22.37119938028475374 ) ) ;
#56628 = VERTEX_POINT ( 'NONE', #11169 ) ;
#56629 = CARTESIAN_POINT ( 'NONE',  ( 4.975610109902397937, -44.31543648230415755, 20.70245146161774841 ) ) ;
#56630 = ORIENTED_EDGE ( 'NONE', *, *, #32057, .T. ) ;
#56631 = ADVANCED_FACE ( 'NONE', ( #53133 ), #1583, .T. ) ;
#56632 = EDGE_CURVE ( 'NONE', #42473, #22519, #508, .T. ) ;
#56633 = CARTESIAN_POINT ( 'NONE',  ( 0.6001305935487422083, -44.24520387813841893, 18.89378601235986110 ) ) ;
#56634 = CARTESIAN_POINT ( 'NONE',  ( 0.3622758884714730732, 22.26738722580116558, 36.91764744403329246 ) ) ;
#56635 = AXIS2_PLACEMENT_3D ( 'NONE', #51472, #7635, #2630 ) ;
#56636 = VERTEX_POINT ( 'NONE', #49671 ) ;
#56637 = AXIS2_PLACEMENT_3D ( 'NONE', #8340, #12774, #41900 ) ;
#56638 = CARTESIAN_POINT ( 'NONE',  ( -6.017396004339686577, -7.212050743684049081, -17.40836349643175041 ) ) ;
#56639 = EDGE_CURVE ( 'NONE', #10029, #1548, #54530, .T. ) ;
#56640 = CARTESIAN_POINT ( 'NONE',  ( 0.5839254288179542840, -29.22920395911540581, 37.94310411505137637 ) ) ;
#56641 = CARTESIAN_POINT ( 'NONE',  ( 0.9736507210033072957, 21.06291100879439071, 37.38294557109041705 ) ) ;
#56642 = CARTESIAN_POINT ( 'NONE',  ( 0.6000166863083090663, -48.77118664543516502, 5.761495891223071375 ) ) ;
#56643 = ORIENTED_EDGE ( 'NONE', *, *, #14014, .F. ) ;
#56644 = CARTESIAN_POINT ( 'NONE',  ( 5.917102823773431552, 16.58597737984221610, -11.37519548874235298 ) ) ;
#56645 = VERTEX_POINT ( 'NONE', #19649 ) ;
#56646 = CARTESIAN_POINT ( 'NONE',  ( 2.114184763561894886, 5.677447754278171364E-15, -44.03514965515262247 ) ) ;
#56647 = B_SPLINE_CURVE_WITH_KNOTS ( 'NONE', 3,
 ( #44185, #20350, #39471, #10956 ),
 .UNSPECIFIED., .F., .F.,
 ( 4, 4 ),
 ( 2.199414408396618760E-17, 0.004559932413162187670 ),
 .UNSPECIFIED. ) ;
#56648 = ORIENTED_EDGE ( 'NONE', *, *, #35672, .F. ) ;
#56649 = ORIENTED_EDGE ( 'NONE', *, *, #13147, .F. ) ;
#56650 = CARTESIAN_POINT ( 'NONE',  ( 0.5997462898726536595, -42.52950339524468859, -24.55184251941555118 ) ) ;
#56651 = CARTESIAN_POINT ( 'NONE',  ( 3.660087539127316880, 46.85281175970452949, 10.60624038924609991 ) ) ;
#56652 = CARTESIAN_POINT ( 'NONE',  ( 0.9754642270333693244, 33.93430397636412721, 26.26019354539047157 ) ) ;
#56653 = ORIENTED_EDGE ( 'NONE', *, *, #33958, .T. ) ;
#56654 = CARTESIAN_POINT ( 'NONE',  ( 6.890143360408123030, -11.60930335864404306, -1.199999999999999956 ) ) ;
#56655 = CARTESIAN_POINT ( 'NONE',  ( 0.5804410086790514622, 45.37396088368723923, -11.86269470150088168 ) ) ;
#56656 = CARTESIAN_POINT ( 'NONE',  ( 3.050102900204245682, 0.4003407177367952485, 43.99164666715468996 ) ) ;
#56657 = ORIENTED_EDGE ( 'NONE', *, *, #57961, .F. ) ;
#56658 = ORIENTED_EDGE ( 'NONE', *, *, #34617, .T. ) ;
#56659 = SURFACE_SIDE_STYLE ('',( #27860 ) ) ;
#56660 = CARTESIAN_POINT ( 'NONE',  ( 0.7954196712028470673, 47.56618050291064748, 7.138712347928350077 ) ) ;
#56661 = CARTESIAN_POINT ( 'NONE',  ( 5.981074661064941900, -5.303881226583815334, 19.82752479807518142 ) ) ;
#56662 = CARTESIAN_POINT ( 'NONE',  ( 4.960156602257180580, -35.23783291257192474, 30.22163187094376724 ) ) ;
#56663 = DIRECTION ( 'NONE',  ( 0.000000000000000000, 0.7071067811865395791, 0.7071067811865553443 ) ) ;
#56664 = ORIENTED_EDGE ( 'NONE', *, *, #43988, .T. ) ;
#56665 = CARTESIAN_POINT ( 'NONE',  ( 4.694002226626921015, -43.37309735483348305, 14.03777750551250136 ) ) ;
#56666 = CARTESIAN_POINT ( 'NONE',  ( 0.9772918015221174759, -40.98423817134506919, 8.753803588448938910 ) ) ;
#56667 = DIRECTION ( 'NONE',  ( 0.09722883295013592941, -0.8708738917980980432, -0.4817937511296604414 ) ) ;
#56668 = CARTESIAN_POINT ( 'NONE',  ( 4.390527457369402420, -43.18387362959315823, 8.083216870278070232 ) ) ;
#56669 =( NAMED_UNIT ( * ) PLANE_ANGLE_UNIT ( ) SI_UNIT ( $, .RADIAN. ) );
#56670 = DIRECTION ( 'NONE',  ( 0.000000000000000000, 0.000000000000000000, 1.000000000000000000 ) ) ;
#56671 = EDGE_CURVE ( 'NONE', #55548, #56965, #39606, .T. ) ;
#56672 = ORIENTED_EDGE ( 'NONE', *, *, #39380, .T. ) ;
#56673 = CARTESIAN_POINT ( 'NONE',  ( -6.079354080745853928, -19.21649618062450671, -1.232570398884354379 ) ) ;
#56674 = DIRECTION ( 'NONE',  ( -0.07836865515943411409, 0.8672783706145159588, 0.4916162952473524528 ) ) ;
#56675 = FACE_OUTER_BOUND ( 'NONE', #7884, .T. ) ;
#56676 = CIRCLE ( 'NONE', #8653, 47.09074272231896430 ) ;
#56677 = AXIS2_PLACEMENT_3D ( 'NONE', #42414, #22987, #27676 ) ;
#56678 = CARTESIAN_POINT ( 'NONE',  ( 0.9780106845699483298, 28.90828061660102577, 30.34209218638833505 ) ) ;
#56679 = EDGE_CURVE ( 'NONE', #37474, #11351, #14193, .T. ) ;
#56680 = CARTESIAN_POINT ( 'NONE',  ( 5.959547316686252039, 16.28624005235099403, -12.49238070347959351 ) ) ;
#56681 = FACE_OUTER_BOUND ( 'NONE', #43382, .T. ) ;
#56682 = CARTESIAN_POINT ( 'NONE',  ( 0.5824935313925965197, 22.21726476033930453, -41.29928962612820698 ) ) ;
#56683 = CARTESIAN_POINT ( 'NONE',  ( 0.8753041380234471980, 32.34805756193355819, 36.94240787824763572 ) ) ;
#56684 = ORIENTED_EDGE ( 'NONE', *, *, #45527, .F. ) ;
#56685 = CARTESIAN_POINT ( 'NONE',  ( 0.6067099128993235224, 47.89177823194874861, -0.7089426894592245620 ) ) ;
#56686 = CARTESIAN_POINT ( 'NONE',  ( 0.5850706913938534814, -41.56998471741211176, -23.79070617305425372 ) ) ;
#56687 = CARTESIAN_POINT ( 'NONE',  ( 4.975801465491694664, 39.51822597168457918, 27.09127437476394817 ) ) ;
#56688 = CARTESIAN_POINT ( 'NONE',  ( 2.301430502907645614, 47.43735983879643214, 7.543848632415379285 ) ) ;
#56689 = ORIENTED_EDGE ( 'NONE', *, *, #15235, .F. ) ;
#56690 = LINE ( 'NONE', #24118, #34315 ) ;
#56691 = CARTESIAN_POINT ( 'NONE',  ( 5.895596859100789899, -4.659086063545737844, -19.56581458219824299 ) ) ;
#56692 = EDGE_CURVE ( 'NONE', #51070, #37795, #14975, .T. ) ;
#56693 = ORIENTED_EDGE ( 'NONE', *, *, #38057, .F. ) ;
#56694 = CARTESIAN_POINT ( 'NONE',  ( 0.1156495703730067715, 4.101228919911528159, -43.93316372147072713 ) ) ;
#56695 = CARTESIAN_POINT ( 'NONE',  ( 0.5834584762367761579, -45.91967682079450697, -9.519415406787116396 ) ) ;
#56696 = ADVANCED_FACE ( 'NONE', ( #2665 ), #41579, .F. ) ;
#56697 = CARTESIAN_POINT ( 'NONE',  ( 0.5988103564986354543, 24.57719524907183839, 41.35593036885941132 ) ) ;
#56698 = ORIENTED_EDGE ( 'NONE', *, *, #48733, .F. ) ;
#56699 = CARTESIAN_POINT ( 'NONE',  ( 3.678748215320121417, 12.69311693770709404, 47.30219441743878406 ) ) ;
#56700 = VERTEX_POINT ( 'NONE', #12721 ) ;
#56701 = EDGE_CURVE ( 'NONE', #25197, #60182, #48597, .T. ) ;
#56702 = ORIENTED_EDGE ( 'NONE', *, *, #60792, .F. ) ;
#56703 = DIRECTION ( 'NONE',  ( 0.000000000000000000, 0.000000000000000000, -1.000000000000000000 ) ) ;
#56704 = CARTESIAN_POINT ( 'NONE',  ( 0.7044674535453004927, -48.59206901384838062, 7.114320189891886415 ) ) ;
#56705 = EDGE_LOOP ( 'NONE', ( #56887, #53157, #40522, #52403 ) ) ;
#56706 = CARTESIAN_POINT ( 'NONE',  ( 3.782625744892853525, 39.34346952798183850, 14.80977749987372150 ) ) ;
#56707 = B_SPLINE_CURVE_WITH_KNOTS ( 'NONE', 3,
 ( #37893, #37261, #56951, #41968, #43196, #57239, #4614, #19378, #38494, #19082, #33482, #227, #61034, #46973, #28764, #57548 ),
 .UNSPECIFIED., .F., .F.,
 ( 4, 3, 3, 3, 3, 4 ),
 ( 1.908319024389645146E-17, 0.0002612764279487757107, 0.0003919131003184790824, 0.0005225497727000649306, 0.0007837925190632454627, 0.001045051706266716951 ),
 .UNSPECIFIED. ) ;
#56708 = EDGE_LOOP ( 'NONE', ( #51728, #8783, #39320, #30070 ) ) ;
#56710 = B_SPLINE_CURVE_WITH_KNOTS ( 'NONE', 3,
 ( #29148, #24136, #43904, #28521, #19765, #29449, #38267, #308, #4690, #946, #57625, #15376, #14758, #23836, #57314, #5615 ),
 .UNSPECIFIED., .F., .F.,
 ( 4, 3, 3, 3, 3, 4 ),
 ( 1.551621725782133898E-17, 0.0002732102107931821933, 0.0004098135523333748661, 0.0005464168938825010938, 0.0008195847345945432268, 0.001092771384553104397 ),
 .UNSPECIFIED. ) ;
#56709 = CARTESIAN_POINT ( 'NONE',  ( 0.6064515330803574855, 11.56175758416135047, 45.44953352458280449 ) ) ;
#56711 = LINE ( 'NONE', #59956, #30828 ) ;
#56712 = CARTESIAN_POINT ( 'NONE',  ( 4.303969348037246512, 45.22910199346996762, -16.39840148505043516 ) ) ;
#56713 = CIRCLE ( 'NONE', #46735, 12.50000000000000000 ) ;
#56714 = VERTEX_POINT ( 'NONE', #45935 ) ;
#56715 = CARTESIAN_POINT ( 'NONE',  ( 4.960386119450146403, 43.62260476509047891, -3.391875319206996142 ) ) ;
#56716 = EDGE_CURVE ( 'NONE', #12754, #32617, #10521, .T. ) ;
#56717 = CIRCLE ( 'NONE', #7711, 42.08604991992415023 ) ;
#56718 = CARTESIAN_POINT ( 'NONE',  ( 2.648799415243696664, 29.17954675436516609, -39.40902833741801459 ) ) ;
#56719 = DIRECTION ( 'NONE',  ( -0.07906939808003035641, 0.5978040102392314648, 0.7977332860230633704 ) ) ;
#56720 = AXIS2_PLACEMENT_3D ( 'NONE', #944, #20987, #54466 ) ;
#56721 = CARTESIAN_POINT ( 'NONE',  ( 0.6000166863083090663, -39.04292238714128160, -29.79049669240369624 ) ) ;
#56722 = ORIENTED_EDGE ( 'NONE', *, *, #53938, .F. ) ;
#56723 = CARTESIAN_POINT ( 'NONE',  ( 0.5819845079324660331, -34.18710788661927324, -33.54497088780116343 ) ) ;
#56724 = ADVANCED_FACE ( 'NONE', ( #26177 ), #17599, .F. ) ;
#56725 = CARTESIAN_POINT ( 'NONE',  ( 5.894904586330512508, 14.91596325940037815, -13.49234790930995764 ) ) ;
#56726 = VERTEX_POINT ( 'NONE', #55910 ) ;
#56727 = CARTESIAN_POINT ( 'NONE',  ( 0.7762783648524403946, 47.60264408896660626, 5.369627767359989257 ) ) ;
#56728 = ORIENTED_EDGE ( 'NONE', *, *, #52381, .T. ) ;
#56729 = DIRECTION ( 'NONE',  ( -1.000000000000000000, -1.836909530733573776E-16, 1.925929944387235853E-32 ) ) ;
#56730 =( BOUNDED_SURFACE ( )  B_SPLINE_SURFACE ( 3, 1, ( 
 ( #54606, #1994 ),
 ( #20211, #35547 ),
 ( #29895, #25499 ),
 ( #21120, #1676 ) ),
 .UNSPECIFIED., .F., .F., .F. ) 
 B_SPLINE_SURFACE_WITH_KNOTS ( ( 4, 4 ),
 ( 2, 2 ),
 ( 0.000000000000000000, 1.000000000000000000 ),
 ( 0.000000000000000000, 1.000000000000000000 ),
 .UNSPECIFIED. ) 
 GEOMETRIC_REPRESENTATION_ITEM ( )  RATIONAL_B_SPLINE_SURFACE ( (
 ( 1.000000000000000000, 1.000000000000000000),
 ( 0.9952954269826590483, 0.8620686068821339365),
 ( 0.9952954269826590483, 0.8620686068821339365),
 ( 1.000000000000000000, 1.000000000000000000) ) ) 
 REPRESENTATION_ITEM ( '' )  SURFACE ( )  );
#56731 = CARTESIAN_POINT ( 'NONE',  ( 0.5824935313925957425, 10.51678459559550838, -45.70159098788227681 ) ) ;
#56732 = EDGE_LOOP ( 'NONE', ( #13897, #36283, #42800, #55319 ) ) ;
#56733 = CARTESIAN_POINT ( 'NONE',  ( 0.5830082357119570347, 4.422203156529602275, 46.68700198321495520 ) ) ;
#56734 = CARTESIAN_POINT ( 'NONE',  ( -6.079354080745853928, -19.21649618062452802, 1.232570398884076823 ) ) ;
#56735 = CARTESIAN_POINT ( 'NONE',  ( -6.078726893082806448, -18.90156862012328887, -3.677600436084754509 ) ) ;
#56736 = CARTESIAN_POINT ( 'NONE',  ( 4.322998006666165516, 27.50295597456399577, 39.32552843303859191 ) ) ;
#56737 = VERTEX_POINT ( 'NONE', #13032 ) ;
#56738 = CARTESIAN_POINT ( 'NONE',  ( 4.834790513006553603, -47.12142688710416394, -3.487186408507438440 ) ) ;
#56739 = FACE_OUTER_BOUND ( 'NONE', #29364, .T. ) ;
#56740 = CARTESIAN_POINT ( 'NONE',  ( 0.8551540677456715978, 29.88829867897814196, 37.45266983663506721 ) ) ;
#56741 = B_SPLINE_CURVE_WITH_KNOTS ( 'NONE', 3,
 ( #39043, #28998, #24926, #38416 ),
 .UNSPECIFIED., .F., .F.,
 ( 4, 4 ),
 ( 8.673617379884034509E-19, 0.004042984057420971090 ),
 .UNSPECIFIED. ) ;
#56742 = CARTESIAN_POINT ( 'NONE',  ( 5.960721111146673579, -10.25731071096595137, 17.77882586010649391 ) ) ;
#56743 = CARTESIAN_POINT ( 'NONE',  ( 0.5782707292762442330, -46.83939014838222903, 2.409955235113546923 ) ) ;
#56744 = ADVANCED_FACE ( 'NONE', ( #32126 ), #33158, .F. ) ;
#56745 = CYLINDRICAL_SURFACE ( 'NONE', #25259, 2.649999999999997691 ) ;
#56746 = CONICAL_SURFACE ( 'NONE', #8731, 43.08621763946400307, 1.568696531533066763 ) ;
#56747 = CARTESIAN_POINT ( 'NONE',  ( 4.956445790443988031, 0.000000000000000000, 0.000000000000000000 ) ) ;
#56748 = CARTESIAN_POINT ( 'NONE',  ( 0.9788927965476035276, -12.28110083706939903, 40.06883046535685367 ) ) ;
#56749 = LINE ( 'NONE', #42084, #53403 ) ;
#56750 = CARTESIAN_POINT ( 'NONE',  ( 0.9756950546413938330, 30.27237962848480635, -30.40918718457309566 ) ) ;
#56751 = CARTESIAN_POINT ( 'NONE',  ( -0.2111111111111110827, -9.497654031326126400, -1.199999999999999956 ) ) ;
#56752 = CARTESIAN_POINT ( 'NONE',  ( 0.6001305935487422083, 28.87057754790887643, 38.48510059944056394 ) ) ;
#56753 = CARTESIAN_POINT ( 'NONE',  ( 1.231276596079887931, -41.87427716283724521, -1.954912557623687652 ) ) ;
#56754 = CARTESIAN_POINT ( 'NONE',  ( 5.894904586330512508, -7.229884331608815273, 18.76854242111518190 ) ) ;
#56755 = CARTESIAN_POINT ( 'NONE',  ( 0.9740398440564319582, -37.36539512268005581, -21.09418882170575671 ) ) ;
#56756 = CIRCLE ( 'NONE', #35783, 5.612499999999999822 ) ;
#56757 = CARTESIAN_POINT ( 'NONE',  ( 0.8554163680231708922, 11.76336166872351008, -45.41837508500965725 ) ) ;
#56758 = CARTESIAN_POINT ( 'NONE',  ( -6.078726893082806448, 19.09835798914753369, -2.459016752095146252 ) ) ;
#56760 = ORIENTED_EDGE ( 'NONE', *, *, #57794, .F. ) ;
#56759 = CARTESIAN_POINT ( 'NONE',  ( 0.9754402186311958989, 39.71365199966012938, 16.24692483025432566 ) ) ;
#56761 = VECTOR ( 'NONE', #36054, 1000.000000000000114 ) ;
#56762 = CARTESIAN_POINT ( 'NONE',  ( 0.6026112563231247332, -39.45929242848867347, 29.23192152334880944 ) ) ;
#56763 = CARTESIAN_POINT ( 'NONE',  ( 0.5827359174754815907, 23.63273677570916220, 41.65957726278045925 ) ) ;
#56764 = FACE_OUTER_BOUND ( 'NONE', #8422, .T. ) ;
#56765 = ORIENTED_EDGE ( 'NONE', *, *, #14084, .T. ) ;
#56766 = CARTESIAN_POINT ( 'NONE',  ( 4.834790513006553603, -39.84947630189473244, 25.38914294317774178 ) ) ;
#56767 = CARTESIAN_POINT ( 'NONE',  ( 1.088908134280555551, 4.826714665689470607, -42.64123480278970391 ) ) ;
#56768 = ORIENTED_EDGE ( 'NONE', *, *, #33526, .T. ) ;
#56769 = ORIENTED_EDGE ( 'NONE', *, *, #57977, .T. ) ;
#56770 = CARTESIAN_POINT ( 'NONE',  ( 0.8560838555295158248, -35.39593983670192756, 30.78149244527153883 ) ) ;
#56771 = ADVANCED_FACE ( 'NONE', ( #8599 ), #13963, .F. ) ;
#56772 = ORIENTED_EDGE ( 'NONE', *, *, #45387, .T. ) ;
#56773 = CARTESIAN_POINT ( 'NONE',  ( 0.5806925824938502512, 4.150136846023314341, -46.71186922509998141 ) ) ;
#56774 = CARTESIAN_POINT ( 'NONE',  ( 0.9757787079277455700, -41.45659305953926577, 11.06737752163081545 ) ) ;
#56775 = ORIENTED_EDGE ( 'NONE', *, *, #32008, .T. ) ;
#56776 = EDGE_CURVE ( 'NONE', #57783, #24396, #47800, .T. ) ;
#56777 = EDGE_LOOP ( 'NONE', ( #15807, #54837, #56809, #39898 ) ) ;
#56778 = CARTESIAN_POINT ( 'NONE',  ( 4.958415959904818315, 29.71032706691277880, 34.35841118852422937 ) ) ;
#56779 = ORIENTED_EDGE ( 'NONE', *, *, #7018, .T. ) ;
#56780 = CARTESIAN_POINT ( 'NONE',  ( 0.1129192098497455998, 15.69290830752535726, -41.23935519181593889 ) ) ;
#56781 = CARTESIAN_POINT ( 'NONE',  ( 4.956445790443991584, 41.78282513192503700, 21.71942849465911252 ) ) ;
#56782 = AXIS2_PLACEMENT_3D ( 'NONE', #10532, #49051, #30544 ) ;
#56783 = CARTESIAN_POINT ( 'NONE',  ( -6.079354080745853928, 17.84825706230192210, 7.227217658694907954 ) ) ;
#56784 = ORIENTED_EDGE ( 'NONE', *, *, #50949, .T. ) ;
#56785 = CARTESIAN_POINT ( 'NONE',  ( 0.000000000000000000, 0.6959691356230525150, -1.199999999999999956 ) ) ;
#56786 =( BOUNDED_SURFACE ( )  B_SPLINE_SURFACE ( 3, 1, ( 
 ( #5251, #48805 ),
 ( #555, #39125 ),
 ( #19692, #57872 ),
 ( #53483, #53185 ) ),
 .UNSPECIFIED., .F., .F., .F. ) 
 B_SPLINE_SURFACE_WITH_KNOTS ( ( 4, 4 ),
 ( 2, 2 ),
 ( 0.000000000000000000, 1.000000000000000000 ),
 ( 0.000000000000000000, 1.000000000000000000 ),
 .UNSPECIFIED. ) 
 GEOMETRIC_REPRESENTATION_ITEM ( )  RATIONAL_B_SPLINE_SURFACE ( (
 ( 1.000000000000000000, 1.000000000000000000),
 ( 0.7282232189291693025, 0.9929344683865674037),
 ( 0.7282232189291693025, 0.9929344683865674037),
 ( 1.000000000000000000, 1.000000000000000000) ) ) 
 REPRESENTATION_ITEM ( '' )  SURFACE ( )  );
#56787 = CARTESIAN_POINT ( 'NONE',  ( 0.9754642270333683252, -33.93430397636394957, -26.26019354539071671 ) ) ;
#56788 = VERTEX_POINT ( 'NONE', #8928 ) ;
#56789 = AXIS2_PLACEMENT_3D ( 'NONE', #60301, #27120, #8009 ) ;
#56790 = ORIENTED_EDGE ( 'NONE', *, *, #40664, .F. ) ;
#56791 = DIRECTION ( 'NONE',  ( 0.000000000000000000, 0.000000000000000000, 1.000000000000000000 ) ) ;
#56792 = ORIENTED_EDGE ( 'NONE', *, *, #30171, .T. ) ;
#56793 = CARTESIAN_POINT ( 'NONE',  ( 4.226256110419178924, 34.96636023808753890, 26.61166852505640534 ) ) ;
#56794 = CARTESIAN_POINT ( 'NONE',  ( -6.078457390727109555, -14.66526260008060234, -12.47896565858665419 ) ) ;
#56795 = CARTESIAN_POINT ( 'NONE',  ( 0.9749527285493316819, -0.2856147164661618776, 42.90750796893246388 ) ) ;
#56796 = CARTESIAN_POINT ( 'NONE',  ( 0.1102847568649952675, 5.720244683738028968, 42.74337176234131164 ) ) ;
#56797 = CARTESIAN_POINT ( 'NONE',  ( 5.894904586330512508, 16.58122937421105192, 11.38385894595691816 ) ) ;
#56798 = EDGE_CURVE ( 'NONE', #32640, #4311, #27587, .T. ) ;
#56799 = ORIENTED_EDGE ( 'NONE', *, *, #9954, .F. ) ;
#56800 = CARTESIAN_POINT ( 'NONE',  ( -6.063463321072276813, 11.99415941893250093, -15.06521132651987394 ) ) ;
#56801 = CARTESIAN_POINT ( 'NONE',  ( 0.8753041380234471980, 5.600023814136011246, -48.78296896616778611 ) ) ;
#56802 =( BOUNDED_SURFACE ( )  B_SPLINE_SURFACE ( 3, 1, ( 
 ( #45544, #54274 ),
 ( #44935, #11715 ),
 ( #59925, #35217 ),
 ( #12337, #21409 ) ),
 .UNSPECIFIED., .F., .F., .F. ) 
 B_SPLINE_SURFACE_WITH_KNOTS ( ( 4, 4 ),
 ( 2, 2 ),
 ( 0.000000000000000000, 1.000000000000000000 ),
 ( 0.000000000000000000, 1.000000000000000000 ),
 .UNSPECIFIED. ) 
 GEOMETRIC_REPRESENTATION_ITEM ( )  RATIONAL_B_SPLINE_SURFACE ( (
 ( 1.000000000000000000, 1.000000000000000000),
 ( 0.7269869731126817891, 0.9931720237060910339),
 ( 0.7269869731126817891, 0.9931720237060910339),
 ( 1.000000000000000000, 1.000000000000000000) ) ) 
 REPRESENTATION_ITEM ( '' )  SURFACE ( )  );
#56803 = CARTESIAN_POINT ( 'NONE',  ( 4.291220156522060236, -45.16379180774710278, -13.40227245105002751 ) ) ;
#56804 = ORIENTED_EDGE ( 'NONE', *, *, #31167, .T. ) ;
#56805 = CARTESIAN_POINT ( 'NONE',  ( 5.917102823773431552, -19.93362549613923207, -2.672132599892811822 ) ) ;
#56806 = CARTESIAN_POINT ( 'NONE',  ( 0.1073791018717483448, -37.58707531572191840, -21.14095454447545919 ) ) ;
#56807 = CARTESIAN_POINT ( 'NONE',  ( 0.7246131072078552116, 7.091231226024794054, -47.57651137777907735 ) ) ;
#56808 = CIRCLE ( 'NONE', #6752, 2.649999999999985700 ) ;
#56809 = ORIENTED_EDGE ( 'NONE', *, *, #61480, .T. ) ;
#56810 = ORIENTED_EDGE ( 'NONE', *, *, #601, .F. ) ;
#56811 = DIRECTION ( 'NONE',  ( -1.000000000000000000, -0.000000000000000000, -0.000000000000000000 ) ) ;
#56812 = CARTESIAN_POINT ( 'NONE',  ( 4.956653778116970166, 45.35992544608529187, 15.97476558431900884 ) ) ;
#56813 = CARTESIAN_POINT ( 'NONE',  ( 0.3676999524040323597, -32.25712563511804376, 30.09033780274075198 ) ) ;
#56814 = DIRECTION ( 'NONE',  ( 0.09835009131224567436, 0.9164135549743729348, 0.3879606369183669079 ) ) ;
#56815 = CARTESIAN_POINT ( 'NONE',  ( 5.894904586330512508, 19.00045333391150848, 6.596376669619000488 ) ) ;
#56816 = CARTESIAN_POINT ( 'NONE',  ( 0.9756354156337457839, -42.55820231551293631, 5.471460801653261541 ) ) ;
#56817 = B_SPLINE_CURVE_WITH_KNOTS ( 'NONE', 3,
 ( #34462, #40408, #58225, #49466, #15354, #53532, #30354, #49777, #1523, #58537, #54143, #6838, #10649, #48851, #5905, #25049, #45111, #21276, #20664 ),
 .UNSPECIFIED., .F., .F.,
 ( 4, 3, 3, 3, 3, 3, 4 ),
 ( 6.938893903907228378E-18, 0.0002724573126191734244, 0.0004086839781548483146, 0.0005449106435901873409, 0.0006811373090491491811, 0.0008459866663933664471, 0.001010840725717215534 ),
 .UNSPECIFIED. ) ;
#56818 = CARTESIAN_POINT ( 'NONE',  ( 0.2885697896453118805, 40.13549262224777436, -15.75356890148114886 ) ) ;
#56819 = CARTESIAN_POINT ( 'NONE',  ( -6.057079549204054558, -14.65763772032107148, 12.48939100034742644 ) ) ;
#56820 = DIRECTION ( 'NONE',  ( 0.000000000000000000, 0.000000000000000000, -1.000000000000000000 ) ) ;
#56821 = CARTESIAN_POINT ( 'NONE',  ( 2.618530812446115519, 39.70953715621357816, -25.15709538157162584 ) ) ;
#56822 = CARTESIAN_POINT ( 'NONE',  ( 0.9783242366443536397, -1.132393795794202296, -41.89334284224371174 ) ) ;
#56823 = CARTESIAN_POINT ( 'NONE',  ( 0.9762797500689124330, 3.691134646838137190, -41.74566217230977117 ) ) ;
#56824 = ORIENTED_EDGE ( 'NONE', *, *, #34684, .F. ) ;
#56825 = AXIS2_PLACEMENT_3D ( 'NONE', #18013, #26466, #22699 ) ;
#56826 = CARTESIAN_POINT ( 'NONE',  ( 0.8760168074886965917, 23.27577685234539118, 42.09738177923962610 ) ) ;
#56827 = CARTESIAN_POINT ( 'NONE',  ( 0.6039202388192952409, -1.399875120785617488, -49.08771804122897464 ) ) ;
#56828 = FACE_OUTER_BOUND ( 'NONE', #44847, .T. ) ;
#56829 = CARTESIAN_POINT ( 'NONE',  ( 0.7048096507298579061, -37.64898672361932341, -29.95256433478712310 ) ) ;
#56830 = DIRECTION ( 'NONE',  ( 0.07836865515943410021, 0.2656332009267382555, -0.9608836331491532601 ) ) ;
#56831 = CARTESIAN_POINT ( 'NONE',  ( 4.963659409799330291, -33.33129552235108406, 29.86601237216398275 ) ) ;
#56832 = ADVANCED_FACE ( 'NONE', ( #46536 ), #4429, .T. ) ;
#56833 = CYLINDRICAL_SURFACE ( 'NONE', #13770, 5.612499999999999822 ) ;
#56834 = CARTESIAN_POINT ( 'NONE',  ( 0.5819845079324660331, 12.83441846783130558, 46.14435090135479811 ) ) ;
#56835 = EDGE_CURVE ( 'NONE', #57176, #5968, #20477, .T. ) ;
#56836 = VECTOR ( 'NONE', #53279, 1000.000000000000000 ) ;
#56837 = CARTESIAN_POINT ( 'NONE',  ( 5.965394784446458765, 0.01447339372424741311, 20.52536205633085231 ) ) ;
#56839 = VERTEX_POINT ( 'NONE', #42466 ) ;
#56838 = CARTESIAN_POINT ( 'NONE',  ( 4.975801465491695552, 3.702618843596801934, 47.76942479135487218 ) ) ;
#56840 = EDGE_LOOP ( 'NONE', ( #19245, #26492, #7958, #30737 ) ) ;
#56841 = CARTESIAN_POINT ( 'NONE',  ( 5.894904586330512508, 10.82137050184767268, 16.95368256525359740 ) ) ;
#56842 = CARTESIAN_POINT ( 'NONE',  ( 0.6000166863083090663, -7.321729200003415983, 48.56146376737702752 ) ) ;
#56843 = CARTESIAN_POINT ( 'NONE',  ( 5.974727161628369032, -5.327229920347563485, 19.82156119440436370 ) ) ;
#56844 = ORIENTED_EDGE ( 'NONE', *, *, #30518, .T. ) ;
#56845 = CARTESIAN_POINT ( 'NONE',  ( 1.227938101723756947, -42.91134962331487657, 0.8460948827223682134 ) ) ;
#56846 = CARTESIAN_POINT ( 'NONE',  ( 4.956653778116973719, 21.75875759808707244, 42.88673967249138741 ) ) ;
#56847 = CARTESIAN_POINT ( 'NONE',  ( 4.322998006666165516, 32.40067585697750729, 35.39923696759023386 ) ) ;
#56848 = ORIENTED_EDGE ( 'NONE', *, *, #48933, .F. ) ;
#56849 = ORIENTED_EDGE ( 'NONE', *, *, #49993, .F. ) ;
#56850 = CARTESIAN_POINT ( 'NONE',  ( 0.9756950546413922787, 41.47131842451904760, 11.01205619898733978 ) ) ;
#56851 = ADVANCED_FACE ( 'NONE', ( #13640 ), #5127, .F. ) ;
#56852 = AXIS2_PLACEMENT_3D ( 'NONE', #35377, #15031, #39780 ) ;
#56853 = CARTESIAN_POINT ( 'NONE',  ( 5.960221823109900008, 7.859839668734944773, 18.96108896995718496 ) ) ;
#56854 = B_SPLINE_CURVE_WITH_KNOTS ( 'NONE', 3,
 ( #52856, #849, #43177, #14053 ),
 .UNSPECIFIED., .F., .F.,
 ( 4, 4 ),
 ( 2.380737581782212780E-07, 0.002336974151641520864 ),
 .UNSPECIFIED. ) ;
#56855 = CARTESIAN_POINT ( 'NONE',  ( 0.5830081025819935370, 46.89517456657120675, -0.2731972786442221079 ) ) ;
#56856 = EDGE_CURVE ( 'NONE', #33892, #33914, #19404, .T. ) ;
#56857 = CARTESIAN_POINT ( 'NONE',  ( 4.967162193818130511, 0.000000000000000000, 0.000000000000000000 ) ) ;
#56858 = CARTESIAN_POINT ( 'NONE',  ( -6.016489644550737204, -7.206912786933163062, -17.41053539857207610 ) ) ;
#56859 = EDGE_CURVE ( 'NONE', #21542, #8227, #44055, .T. ) ;
#56860 = CARTESIAN_POINT ( 'NONE',  ( 0.9754642270333694354, 42.51806607596984833, 5.774842730422176551 ) ) ;
#56861 = ORIENTED_EDGE ( 'NONE', *, *, #55465, .T. ) ;
#56862 = CARTESIAN_POINT ( 'NONE',  ( -6.015611763856276717, -9.427003116184289766, 16.31561949997072958 ) ) ;
#56863 = AXIS2_PLACEMENT_3D ( 'NONE', #9845, #48064, #61516 ) ;
#56864 = ORIENTED_EDGE ( 'NONE', *, *, #41681, .F. ) ;
#56865 = CARTESIAN_POINT ( 'NONE',  ( 3.680974057930773924, 16.63696281867796500, 44.99871514631797709 ) ) ;
#56866 = CARTESIAN_POINT ( 'NONE',  ( -4.467299999999993609, 0.000000000000000000, -12.50000000000000000 ) ) ;
#56867 = CARTESIAN_POINT ( 'NONE',  ( 0.5806925824938490299, 46.40146083665128174, 6.791670970260652140 ) ) ;
#56868 = FACE_OUTER_BOUND ( 'NONE', #38993, .T. ) ;
#56869 = EDGE_CURVE ( 'NONE', #14833, #56169, #7376, .T. ) ;
#56870 = EDGE_LOOP ( 'NONE', ( #16426, #7614, #55354, #25285 ) ) ;
#56871 = B_SPLINE_CURVE_WITH_KNOTS ( 'NONE', 3,
 ( #40407, #26274, #6211, #16579 ),
 .UNSPECIFIED., .F., .F.,
 ( 4, 4 ),
 ( 0.000000000000000000, 0.004446090762761362516 ),
 .UNSPECIFIED. ) ;
#56872 = EDGE_LOOP ( 'NONE', ( #28049, #34411, #17522, #61094 ) ) ;
#56873 = CARTESIAN_POINT ( 'NONE',  ( 0.1158816050234198758, -44.12416581690439443, 0.005680447781237294401 ) ) ;
#56874 = FACE_OUTER_BOUND ( 'NONE', #31229, .T. ) ;
#56875 = DIRECTION ( 'NONE',  ( 0.07439287786467665975, 0.1432402660415289519, -0.9868880006907386759 ) ) ;
#56876 = PRODUCT_DEFINITION_FORMATION_WITH_SPECIFIED_SOURCE ( 'ANY', '', #27294, .NOT_KNOWN. ) ;
#56877 = VERTEX_POINT ( 'NONE', #49284 ) ;
#56878 = FACE_OUTER_BOUND ( 'NONE', #42182, .T. ) ;
#56879 = ORIENTED_EDGE ( 'NONE', *, *, #8861, .F. ) ;
#56880 = CARTESIAN_POINT ( 'NONE',  ( 1.296416391601052487, 43.45757030793557618, 7.331231615969850068 ) ) ;
#56881 = CARTESIAN_POINT ( 'NONE',  ( 0.6016118706126977189, -25.75422445077556333, 41.81233045075345700 ) ) ;
#56882 =( BOUNDED_SURFACE ( )  B_SPLINE_SURFACE ( 3, 1, ( 
 ( #61900, #37851 ),
 ( #38155, #43155 ),
 ( #23409, #56908 ),
 ( #13407, #57200 ) ),
 .UNSPECIFIED., .F., .F., .F. ) 
 B_SPLINE_SURFACE_WITH_KNOTS ( ( 4, 4 ),
 ( 2, 2 ),
 ( 0.000000000000000000, 1.000000000000000000 ),
 ( 0.000000000000000000, 1.000000000000000000 ),
 .UNSPECIFIED. ) 
 GEOMETRIC_REPRESENTATION_ITEM ( )  RATIONAL_B_SPLINE_SURFACE ( (
 ( 1.000000000000000000, 1.000000000000000000),
 ( 0.9754377213608244057, 0.9999580625633939235),
 ( 0.9754377213608244057, 0.9999580625633939235),
 ( 1.000000000000000000, 1.000000000000000000) ) ) 
 REPRESENTATION_ITEM ( '' )  SURFACE ( )  );
#56883 = ORIENTED_EDGE ( 'NONE', *, *, #8921, .T. ) ;
#56884 = CARTESIAN_POINT ( 'NONE',  ( 4.962356264823601926, 34.44911810793277596, -24.17630781256817940 ) ) ;
#56885 = CARTESIAN_POINT ( 'NONE',  ( 5.917102823773431552, 0.6634426252563657700, -20.10098410363868027 ) ) ;
#56886 = DIRECTION ( 'NONE',  ( 0.000000000000000000, -0.000000000000000000, 1.000000000000000000 ) ) ;
#56887 = ORIENTED_EDGE ( 'NONE', *, *, #29679, .F. ) ;
#56888 = CARTESIAN_POINT ( 'NONE',  ( 0.5836750258453361484, -18.16108240858311618, -44.31929073742209368 ) ) ;
#56889 = CARTESIAN_POINT ( 'NONE',  ( 4.549368137175248350, 19.17571786012324608, -38.40568845698256695 ) ) ;
#56890 = CARTESIAN_POINT ( 'NONE',  ( 0.8554163680231738898, 44.99993935735606954, 13.27444654010463410 ) ) ;
#56891 = CARTESIAN_POINT ( 'NONE',  ( 2.301529144917014769, 42.22700141647010952, 22.89307126380001378 ) ) ;
#56892 = CARTESIAN_POINT ( 'NONE',  ( 0.1084644655670283508, 16.13497904887303847, -39.99242539812098585 ) ) ;
#56893 = ORIENTED_EDGE ( 'NONE', *, *, #56679, .T. ) ;
#56894 = VECTOR ( 'NONE', #38860, 999.9999999999998863 ) ;
#56895 = EDGE_CURVE ( 'NONE', #19147, #12519, #41059, .T. ) ;
#56896 =( BOUNDED_SURFACE ( )  B_SPLINE_SURFACE ( 3, 1, ( 
 ( #21923, #31007 ),
 ( #16606, #35731 ),
 ( #54795, #50116 ),
 ( #36349, #55409 ) ),
 .UNSPECIFIED., .F., .F., .F. ) 
 B_SPLINE_SURFACE_WITH_KNOTS ( ( 4, 4 ),
 ( 2, 2 ),
 ( 0.000000000000000000, 1.000000000000000000 ),
 ( 0.000000000000000000, 1.000000000000000000 ),
 .UNSPECIFIED. ) 
 GEOMETRIC_REPRESENTATION_ITEM ( )  RATIONAL_B_SPLINE_SURFACE ( (
 ( 1.000000000000000000, 1.000000000000000000),
 ( 0.9953485035131437453, 0.8621029689291523912),
 ( 0.9953485035131437453, 0.8621029689291523912),
 ( 1.000000000000000000, 1.000000000000000000) ) ) 
 REPRESENTATION_ITEM ( '' )  SURFACE ( )  );
#56897 = DIRECTION ( 'NONE',  ( -1.000000000000000000, -1.836909530733573776E-16, 1.925929944387235579E-32 ) ) ;
#56898 = VERTEX_POINT ( 'NONE', #48070 ) ;
#56899 = CIRCLE ( 'NONE', #15881, 47.91270532121795611 ) ;
#56900 = EDGE_CURVE ( 'NONE', #3984, #56700, #43263, .T. ) ;
#56902 = CARTESIAN_POINT ( 'NONE',  ( 0.9736507210033059634, -30.65767007549935030, 30.02062799605188914 ) ) ;
#56901 =( BOUNDED_SURFACE ( )  B_SPLINE_SURFACE ( 3, 1, ( 
 ( #54540, #2236 ),
 ( #26067, #11668 ),
 ( #48948, #59251 ),
 ( #16359, #45205 ) ),
 .UNSPECIFIED., .F., .F., .F. ) 
 B_SPLINE_SURFACE_WITH_KNOTS ( ( 4, 4 ),
 ( 2, 2 ),
 ( 0.000000000000000000, 1.000000000000000000 ),
 ( 0.000000000000000000, 1.000000000000000000 ),
 .UNSPECIFIED. ) 
 GEOMETRIC_REPRESENTATION_ITEM ( )  RATIONAL_B_SPLINE_SURFACE ( (
 ( 1.000000000000000000, 1.000000000000000000),
 ( 0.9952954269826590483, 0.8620686068821307169),
 ( 0.9952954269826590483, 0.8620686068821307169),
 ( 1.000000000000000000, 1.000000000000000000) ) ) 
 REPRESENTATION_ITEM ( '' )  SURFACE ( )  );
#56903 = CARTESIAN_POINT ( 'NONE',  ( 0.9762797500689124330, 32.57381952463267538, -26.36799322592379369 ) ) ;
#56904 = CARTESIAN_POINT ( 'NONE',  ( 4.956653778116992370, 26.26162724282429650, -40.28700667097652399 ) ) ;
#56905 = CARTESIAN_POINT ( 'NONE',  ( 0.9756008150404611445, 5.459718823766134044, -42.55970871350800167 ) ) ;
#56906 = B_SPLINE_CURVE_WITH_KNOTS ( 'NONE', 3,
 ( #28568, #5359, #43012, #47691, #38013, #4127 ),
 .UNSPECIFIED., .F., .F.,
 ( 4, 2, 4 ),
 ( 8.673617379884035472E-19, 0.0002293801035737091281, 0.0004587602071474173888 ),
 .UNSPECIFIED. ) ;
#56907 = CARTESIAN_POINT ( 'NONE',  ( 1.092182651088184908, -6.200333517503296754, 41.45258796159785675 ) ) ;
#56908 = CARTESIAN_POINT ( 'NONE',  ( 0.6039202388192952409, 10.75760111029171107, 47.91490093072135181 ) ) ;
#56909 = CARTESIAN_POINT ( 'NONE',  ( 0.5832366564991506852, -47.89515933308367579, 0.2724446024275744560 ) ) ;
#56910 = EDGE_CURVE ( 'NONE', #30745, #4178, #24251, .T. ) ;
#56911 = DIRECTION ( 'NONE',  ( -0.9848077530122079093, -0.09698383872753976731, -0.1440410519008964996 ) ) ;
#56912 = CARTESIAN_POINT ( 'NONE',  ( 0.6031357023905874470, 47.69018446756500396, 6.322524267548747190 ) ) ;
#56913 = CARTESIAN_POINT ( 'NONE',  ( -6.072942160501519027, 3.058960253794435591, 19.01175753197810181 ) ) ;
#56914 = AXIS2_PLACEMENT_3D ( 'NONE', #14013, #39058, #19631 ) ;
#56915 = ADVANCED_FACE ( 'NONE', ( #24879 ), #5561, .F. ) ;
#56916 = CARTESIAN_POINT ( 'NONE',  ( 0.5782707292762423457, 43.45719891954316694, 17.64109451748601032 ) ) ;
#56917 = CARTESIAN_POINT ( 'NONE',  ( 0.1102144999581333162, -5.753800096706359390, 42.73889315046709925 ) ) ;
#56918 = VERTEX_POINT ( 'NONE', #1348 ) ;
#56919 = CIRCLE ( 'NONE', #57892, 9.500000000000000000 ) ;
#56920 = CARTESIAN_POINT ( 'NONE',  ( 0.3676999524040323597, 40.09552319080426486, -18.39292264373764851 ) ) ;
#56921 = CARTESIAN_POINT ( 'NONE',  ( 49.80938579167644775, 15.28643915577036339, -2.564367652788756669 ) ) ;
#56922 = CARTESIAN_POINT ( 'NONE',  ( 5.901764892641307547, -4.745137497650260272, 48.73884628884923131 ) ) ;
#56923 = DIRECTION ( 'NONE',  ( -1.000000000000000000, -1.836909530733573776E-16, 1.361838123766442686E-32 ) ) ;
#56924 = CARTESIAN_POINT ( 'NONE',  ( 1.112077966505211846, 32.87428506335748324, -29.36514441819868537 ) ) ;
#56925 = ORIENTED_EDGE ( 'NONE', *, *, #30224, .T. ) ;
#56926 = CARTESIAN_POINT ( 'NONE',  ( 0.9745511491811735816, 11.43411988112660715, -41.35688774886278196 ) ) ;
#56927 = EDGE_CURVE ( 'NONE', #43595, #26311, #18620, .T. ) ;
#56928 = B_SPLINE_CURVE_WITH_KNOTS ( 'NONE', 3,
 ( #37683, #24481, #43616, #37366 ),
 .UNSPECIFIED., .F., .F.,
 ( 4, 4 ),
 ( 0.000000000000000000, 0.004446090762761352976 ),
 .UNSPECIFIED. ) ;
#56929 = CARTESIAN_POINT ( 'NONE',  ( 0.6026777506516368677, -45.58364336417871954, -18.26685107741847958 ) ) ;
#56930 = DIRECTION ( 'NONE',  ( 1.000000000000000000, 0.000000000000000000, 0.000000000000000000 ) ) ;
#56931 = EDGE_CURVE ( 'NONE', #34782, #55528, #27597, .T. ) ;
#56932 = VERTEX_POINT ( 'NONE', #1971 ) ;
#56933 = CARTESIAN_POINT ( 'NONE',  ( 4.963659409799328515, 24.46566636552824292, 37.47512675766701307 ) ) ;
#56934 = CARTESIAN_POINT ( 'NONE',  ( 1.227938101723756947, -30.94118573761292623, -29.74462687941258210 ) ) ;
#56935 = ADVANCED_FACE ( 'NONE', ( #49591 ), #52613, .T. ) ;
#56936 = B_SPLINE_CURVE_WITH_KNOTS ( 'NONE', 3,
 ( #54207, #16974, #12580, #25412 ),
 .UNSPECIFIED., .F., .F.,
 ( 4, 4 ),
 ( 0.000000000000000000, 0.004447772540403788569 ),
 .UNSPECIFIED. ) ;
#56937 = ORIENTED_EDGE ( 'NONE', *, *, #26880, .T. ) ;
#56938 = AXIS2_PLACEMENT_3D ( 'NONE', #60386, #37246, #56009 ) ;
#56939 = CARTESIAN_POINT ( 'NONE',  ( 1.112077966505211624, -26.65465479487276568, 35.10782965229723374 ) ) ;
#56940 = ORIENTED_EDGE ( 'NONE', *, *, #56096, .T. ) ;
#56941 = CARTESIAN_POINT ( 'NONE',  ( 0.2940135542859015905, 42.11535309265164528, 13.13535620273383664 ) ) ;
#56943 = CARTESIAN_POINT ( 'NONE',  ( 0.6031356219577718170, 34.07882816221574274, 33.95537057546196991 ) ) ;
#56942 = VECTOR ( 'NONE', #6883, 1000.000000000000114 ) ;
#56944 = EDGE_LOOP ( 'NONE', ( #6953, #24664, #50637, #59395 ) ) ;
#56945 = CARTESIAN_POINT ( 'NONE',  ( 5.838029081930957709, -43.49392513872139432, -18.42127938499984197 ) ) ;
#56946 = DIRECTION ( 'NONE',  ( 0.000000000000000000, 0.000000000000000000, 1.000000000000000000 ) ) ;
#56947 = CARTESIAN_POINT ( 'NONE',  ( 0.7242003506639985710, -43.17949308384103801, -23.37826022501576873 ) ) ;
#56948 = CARTESIAN_POINT ( 'NONE',  ( 4.549368137175248350, 23.67244292351640667, -35.80950303116076583 ) ) ;
#56949 = EDGE_CURVE ( 'NONE', #42739, #49695, #55204, .T. ) ;
#56950 = ORIENTED_EDGE ( 'NONE', *, *, #60314, .T. ) ;
#56951 = CARTESIAN_POINT ( 'NONE',  ( 0.6016118706126978299, -7.493489753196714176, -48.53244961984368899 ) ) ;
#56952 = VERTEX_POINT ( 'NONE', #11394 ) ;
#56953 = EDGE_CURVE ( 'NONE', #30244, #48102, #21600, .T. ) ;
#56954 = ORIENTED_EDGE ( 'NONE', *, *, #4848, .F. ) ;
#56955 = VERTEX_POINT ( 'NONE', #7595 ) ;
#56956 = CARTESIAN_POINT ( 'NONE',  ( 0.9968887458511642707, -42.45154664631704833, -6.251925120321881302 ) ) ;
#56957 = CARTESIAN_POINT ( 'NONE',  ( 0.9789233960466692253, -37.46340317803434772, 18.78377355997430342 ) ) ;
#56958 = AXIS2_PLACEMENT_3D ( 'NONE', #18166, #28165, #22855 ) ;
#56959 = CARTESIAN_POINT ( 'NONE',  ( 5.896278296736517710, 10.82699056113231251, -16.95002227147609020 ) ) ;
#56960 = CARTESIAN_POINT ( 'NONE',  ( 3.678748215320120529, 42.02540356438220215, 25.14912065163104771 ) ) ;
#56961 = ORIENTED_EDGE ( 'NONE', *, *, #61924, .F. ) ;
#56962 = CARTESIAN_POINT ( 'NONE',  ( 0.8554163680231720024, 11.76336166872288302, 45.41837508500981357 ) ) ;
#56963 = CARTESIAN_POINT ( 'NONE',  ( 5.910764540655178756, 12.97317151014757464, -15.36873642943551310 ) ) ;
#56964 = CARTESIAN_POINT ( 'NONE',  ( 0.1155031312995260795, -38.52861385246892212, 21.50552364252377657 ) ) ;
#56965 = VERTEX_POINT ( 'NONE', #45856 ) ;
#56966 = ORIENTED_EDGE ( 'NONE', *, *, #10526, .F. ) ;
#56967 = CARTESIAN_POINT ( 'NONE',  ( 0.8751705887134553219, -48.08707113907594533, 0.8911681664086766874 ) ) ;
#56968 = CARTESIAN_POINT ( 'NONE',  ( 0.5998501479064708430, 47.62484632993678701, 6.798102206414301740 ) ) ;
#56969 = CARTESIAN_POINT ( 'NONE',  ( 30.00000000000001066, 4.342925291379521108E-15, -1.386669559958810165E-30 ) ) ;
#56970 = CARTESIAN_POINT ( 'NONE',  ( 0.1310142868023688456, -42.66681113736510866, -6.259743112235379492 ) ) ;
#56971 = LINE ( 'NONE', #61353, #8773 ) ;
#56972 = ORIENTED_EDGE ( 'NONE', *, *, #10260, .F. ) ;
#56973 = EDGE_LOOP ( 'NONE', ( #19582, #15423, #41418, #17916 ) ) ;
#56974 = B_SPLINE_CURVE_WITH_KNOTS ( 'NONE', 3,
 ( #29831, #16672, #11997, #48629, #53929, #25133 ),
 .UNSPECIFIED., .F., .F.,
 ( 4, 2, 4 ),
 ( 1.138360651264128102E-17, 0.0002291978881530170003, 0.0004583957763060226166 ),
 .UNSPECIFIED. ) ;
#56975 = EDGE_CURVE ( 'NONE', #8504, #23672, #33603, .T. ) ;
#56976 = CARTESIAN_POINT ( 'NONE',  ( -6.001507490154111224, -11.45906331631421438, -14.95933060264885484 ) ) ;
#56977 = CARTESIAN_POINT ( 'NONE',  ( 2.009741617377216460, 42.94470556311812715, -9.759935538728488069 ) ) ;
#56978 = CARTESIAN_POINT ( 'NONE',  ( 1.112077966505211846, -38.91188999537838100, -20.70978372934219891 ) ) ;
#56979 = LINE ( 'NONE', #61972, #57806 ) ;
#56980 = EDGE_CURVE ( 'NONE', #20981, #55303, #3206, .T. ) ;
#56981 = CARTESIAN_POINT ( 'NONE',  ( 0.6031356219577718170, 0.08729769678243670672, 48.10744328000515679 ) ) ;
#56982 =( BOUNDED_SURFACE ( )  B_SPLINE_SURFACE ( 3, 1, ( 
 ( #10631, #29720 ),
 ( #48834, #5887 ),
 ( #44177, #30032 ),
 ( #58517, #53818 ) ),
 .UNSPECIFIED., .F., .F., .F. ) 
 B_SPLINE_SURFACE_WITH_KNOTS ( ( 4, 4 ),
 ( 2, 2 ),
 ( 0.000000000000000000, 1.000000000000000000 ),
 ( 0.000000000000000000, 1.000000000000000000 ),
 .UNSPECIFIED. ) 
 GEOMETRIC_REPRESENTATION_ITEM ( )  RATIONAL_B_SPLINE_SURFACE ( (
 ( 1.000000000000000000, 1.000000000000000000),
 ( 0.9952954269826590483, 0.8620686068821307169),
 ( 0.9952954269826590483, 0.8620686068821307169),
 ( 1.000000000000000000, 1.000000000000000000) ) ) 
 REPRESENTATION_ITEM ( '' )  SURFACE ( )  );
#56983 = ORIENTED_EDGE ( 'NONE', *, *, #31204, .T. ) ;
#56984 = CARTESIAN_POINT ( 'NONE',  ( 0.8551540677456834771, 0.9122407826475761317, 47.90804413217340851 ) ) ;
#56985 = CARTESIAN_POINT ( 'NONE',  ( 4.694002226626921015, 45.25670317367046636, -5.487767241458218592 ) ) ;
#56986 = EDGE_CURVE ( 'NONE', #52075, #2327, #57407, .T. ) ;
#56987 = LINE ( 'NONE', #51671, #6817 ) ;
#56988 = EDGE_CURVE ( 'NONE', #37964, #55501, #4369, .T. ) ;
#56989 = CARTESIAN_POINT ( 'NONE',  ( 5.896782393890504181, 20.06834277495332941, 1.337050913387667350 ) ) ;
#56990 = AXIS2_PLACEMENT_3D ( 'NONE', #60701, #27211, #46338 ) ;
#56991 = ADVANCED_FACE ( 'NONE', ( #26102 ), #59605, .F. ) ;
#56992 = CARTESIAN_POINT ( 'NONE',  ( 4.956445790443996913, 7.299064093730984304, 46.52162629890795387 ) ) ;
#56993 = CARTESIAN_POINT ( 'NONE',  ( 4.322998006666165516, 16.38761975793144288, 45.10383234877038916 ) ) ;
#56994 = CARTESIAN_POINT ( 'NONE',  ( 3.660087539127330647, -1.881558488211391378, -48.00143792263126841 ) ) ;
#56995 = EDGE_CURVE ( 'NONE', #61378, #57990, #60410, .T. ) ;
#56996 = CARTESIAN_POINT ( 'NONE',  ( 0.8760168074887090262, -37.61398439004553751, 29.98565522133282713 ) ) ;
#56997 = ORIENTED_EDGE ( 'NONE', *, *, #51925, .F. ) ;
#56998 = VECTOR ( 'NONE', #4891, 1000.000000000000227 ) ;
#56999 = CARTESIAN_POINT ( 'NONE',  ( 0.9730545539215883499, -39.83279466599027785, -15.95224156741871546 ) ) ;
#57000 = CARTESIAN_POINT ( 'NONE',  ( 4.226256110419179812, 23.13112329552939528, -37.36011757307789338 ) ) ;
#57001 = CARTESIAN_POINT ( 'NONE',  ( 0.5997462898726536595, -42.52950339524468859, -24.55184251941555118 ) ) ;
#57002 = CARTESIAN_POINT ( 'NONE',  ( 4.962356264823602814, -15.53171314616136200, -39.11523340858015274 ) ) ;
#57003 = ORIENTED_EDGE ( 'NONE', *, *, #3177, .F. ) ;
#57004 = CARTESIAN_POINT ( 'NONE',  ( 4.975801465491695552, 0.000000000000000000, 0.000000000000000000 ) ) ;
#57005 = CARTESIAN_POINT ( 'NONE',  ( 5.895596859100789899, 19.00119700155561020, -6.594141014609973261 ) ) ;
#57006 =( LENGTH_UNIT ( ) NAMED_UNIT ( * ) SI_UNIT ( .MILLI., .METRE. ) );
#57007 = ORIENTED_EDGE ( 'NONE', *, *, #8024, .F. ) ;
#57008 = LINE ( 'NONE', #51697, #40103 ) ;
#57009 = CARTESIAN_POINT ( 'NONE',  ( 0.5830082357119558134, -45.90106299026774650, -9.608561354428239554 ) ) ;
#57010 = CARTESIAN_POINT ( 'NONE',  ( -6.077587904424778920, 17.84644683124306397, 7.231898567703008318 ) ) ;
#57011 = ORIENTED_EDGE ( 'NONE', *, *, #18823, .F. ) ;
#57012 = CARTESIAN_POINT ( 'NONE',  ( 4.962356264823602814, 39.61238188121407688, -14.21600504921160812 ) ) ;
#57013 = ORIENTED_EDGE ( 'NONE', *, *, #16857, .F. ) ;
#57014 = CARTESIAN_POINT ( 'NONE',  ( 4.960386119450145515, 43.68547429165921159, 2.452712903118134946 ) ) ;
#57015 = ORIENTED_EDGE ( 'NONE', *, *, #34378, .T. ) ;
#57016 = CARTESIAN_POINT ( 'NONE',  ( 0.5819845079324663661, -6.701571823032408837, -47.42480735454292784 ) ) ;
#57017 = CARTESIAN_POINT ( 'NONE',  ( -6.010958268070873523, 17.41463273278779056, 7.197664668556505774 ) ) ;
#57018 = EDGE_LOOP ( 'NONE', ( #60425, #26058, #25427, #60494 ) ) ;
#57019 = CARTESIAN_POINT ( 'NONE',  ( 0.3676999524040366896, -43.84864779214676389, -4.821480075983068048 ) ) ;
#57020 = ORIENTED_EDGE ( 'NONE', *, *, #37459, .F. ) ;
#57021 = CARTESIAN_POINT ( 'NONE',  ( -2.739355103387247858, 14.91194544146095069, -0.6938660547317456739 ) ) ;
#57022 = EDGE_CURVE ( 'NONE', #59557, #51084, #5157, .T. ) ;
#57023 = DIRECTION ( 'NONE',  ( 0.07439287786467665975, 0.01320009283086933695, -0.9971416435352942198 ) ) ;
#57024 = CARTESIAN_POINT ( 'NONE',  ( 4.553261556744875094, 0.000000000000000000, 0.000000000000000000 ) ) ;
#57025 = ORIENTED_EDGE ( 'NONE', *, *, #3757, .T. ) ;
#57026 = CARTESIAN_POINT ( 'NONE',  ( 0.5782707292762442330, 46.38083794024484519, 6.968086227104402397 ) ) ;
#57027 = CARTESIAN_POINT ( 'NONE',  ( 5.838029081930955932, -45.56116631979260490, 12.45974244248718144 ) ) ;
#57028 = CARTESIAN_POINT ( 'NONE',  ( 2.624215991343608501, -7.662883702704991862, 47.39206852872455045 ) ) ;
#57029 = CARTESIAN_POINT ( 'NONE',  ( 0.1140933569871964703, -22.54850122134973489, -37.92776084551650229 ) ) ;
#57030 = VERTEX_POINT ( 'NONE', #8524 ) ;
#57031 = CARTESIAN_POINT ( 'NONE',  ( 5.895596859100789899, 0.6756533542676474990, -20.10153416427100836 ) ) ;
#57032 = EDGE_LOOP ( 'NONE', ( #36158, #19140, #34234, #14687 ) ) ;
#57033 = CARTESIAN_POINT ( 'NONE',  ( 0.5832655196449156865, 43.26316045182046111, -18.09790404144539266 ) ) ;
#57034 = ORIENTED_EDGE ( 'NONE', *, *, #21862, .T. ) ;
#57035 = CARTESIAN_POINT ( 'NONE',  ( 5.917102823773431552, 12.99138957749423540, -15.35296436840508427 ) ) ;
#57036 = CARTESIAN_POINT ( 'NONE',  ( 0.2230388203127602886, 11.89247826311217260, 41.44703429209689460 ) ) ;
#57037 = EDGE_LOOP ( 'NONE', ( #23074, #41365, #56417, #47875 ) ) ;
#57038 = FACE_OUTER_BOUND ( 'NONE', #28448, .T. ) ;
#57039 = CARTESIAN_POINT ( 'NONE',  ( 2.528100132419516921, 36.72067332157243413, 20.34320351966313112 ) ) ;
#57040 = CARTESIAN_POINT ( 'NONE',  ( 0.3622758884714730732, 15.73321244754854753, -40.13994584881767480 ) ) ;
#57041 = CARTESIAN_POINT ( 'NONE',  ( 3.376099380956842921, 13.04318434631697521, 3.095759315589459604 ) ) ;
#57042 = CIRCLE ( 'NONE', #6000, 6.728125000000022560 ) ;
#57043 = ORIENTED_EDGE ( 'NONE', *, *, #31890, .F. ) ;
#57044 = CARTESIAN_POINT ( 'NONE',  ( 4.956445790443991584, 35.28522167764473494, 31.18479086508529363 ) ) ;
#57045 = CARTESIAN_POINT ( 'NONE',  ( 0.5848930533535030563, 36.69111421824725028, 29.20676667847867947 ) ) ;
#57046 = CARTESIAN_POINT ( 'NONE',  ( 0.5804410086790514622, -25.69437916690408841, 39.23415261073904503 ) ) ;
#57047 = EDGE_CURVE ( 'NONE', #6564, #2091, #19599, .T. ) ;
#57048 = CARTESIAN_POINT ( 'NONE',  ( 0.8751705887134423323, -29.98056538504989277, 37.60752970653777538 ) ) ;
#57049 = CARTESIAN_POINT ( 'NONE',  ( -2.739355103387248747, 13.56174707817303293, 6.239117176226312012 ) ) ;
#57050 = DIRECTION ( 'NONE',  ( 1.000000000000000000, 0.000000000000000000, 0.000000000000000000 ) ) ;
#57051 = ADVANCED_FACE ( 'NONE', ( #52059 ), #8848, .T. ) ;
#57052 = CARTESIAN_POINT ( 'NONE',  ( 0.5997462898726536595, 48.97040376101519144, -3.667585803694250135 ) ) ;
#57053 = EDGE_CURVE ( 'NONE', #26589, #885, #61596, .T. ) ;
#57054 = ADVANCED_FACE ( 'NONE', ( #27959 ), #49594, .F. ) ;
#57055 = CARTESIAN_POINT ( 'NONE',  ( 5.960721111146673579, -0.006321279846680040275, -20.52557019979492026 ) ) ;
#57056 = CARTESIAN_POINT ( 'NONE',  ( 0.5786265663353153954, -46.07681357296495150, 13.09387673186319212 ) ) ;
#57057 = CARTESIAN_POINT ( 'NONE',  ( 1.318516776095788545, 3.857556137907071747, -5.600000000000003197 ) ) ;
#57058 = CARTESIAN_POINT ( 'NONE',  ( 0.9730545539215883499, -34.34678117142574649, 25.71816799638765971 ) ) ;
#57059 = CARTESIAN_POINT ( 'NONE',  ( 0.9756950546413930558, 37.20808764646341160, 21.37039651692511555 ) ) ;
#57060 = CARTESIAN_POINT ( 'NONE',  ( 0.5809828226811617480, -47.55412398569210808, 5.711058609465143654 ) ) ;
#57061 = CARTESIAN_POINT ( 'NONE',  ( 0.9757787079277436826, -37.14005577278808801, -21.48842038179473590 ) ) ;
#57062 = SURFACE_STYLE_USAGE ( .BOTH. , #19198 ) ;
#57063 = CARTESIAN_POINT ( 'NONE',  ( 5.880360259849739535, 47.86623372148050493, -3.184717612777442142 ) ) ;
#57064 = ORIENTED_EDGE ( 'NONE', *, *, #31156, .F. ) ;
#57065 = EDGE_CURVE ( 'NONE', #57224, #43088, #9616, .T. ) ;
#57066 = CARTESIAN_POINT ( 'NONE',  ( 0.6026777506516367566, -39.25098745825879831, 29.51112288932478478 ) ) ;
#57067 = CARTESIAN_POINT ( 'NONE',  ( 5.958863334805807099, 19.82657410201435511, 5.311251202228921109 ) ) ;
#57068 = VERTEX_POINT ( 'NONE', #23560 ) ;
#57069 = EDGE_CURVE ( 'NONE', #49359, #34393, #56598, .T. ) ;
#57070 = CARTESIAN_POINT ( 'NONE',  ( 2.359973842542475442, -30.55638990495834051, 31.69294764783894180 ) ) ;
#57072 = VERTEX_POINT ( 'NONE', #42386 ) ;
#57071 = AXIS2_PLACEMENT_3D ( 'NONE', #32425, #17702, #32115 ) ;
#57073 = ORIENTED_EDGE ( 'NONE', *, *, #53930, .T. ) ;
#57074 = CARTESIAN_POINT ( 'NONE',  ( 0.9758171775293916772, -11.11125068417964279, -41.44488232057079102 ) ) ;
#57075 = ORIENTED_EDGE ( 'NONE', *, *, #18770, .F. ) ;
#57076 = CARTESIAN_POINT ( 'NONE',  ( 5.958863334805807099, 7.855954700275350255, 18.96276366205797004 ) ) ;
#57077 = CARTESIAN_POINT ( 'NONE',  ( 1.231276596079881047, -41.87427716283725943, 1.954912557623087022 ) ) ;
#57078 = B_SPLINE_CURVE_WITH_KNOTS ( 'NONE', 3,
 ( #25825, #26133, #54613, #30507, #2308, #54931 ),
 .UNSPECIFIED., .F., .F.,
 ( 4, 2, 4 ),
 ( 0.000000000000000000, 0.0002450742804987323330, 0.0004901485609974646660 ),
 .UNSPECIFIED. ) ;
#57079 = VERTEX_POINT ( 'NONE', #18260 ) ;
#57080 = VERTEX_POINT ( 'NONE', #8219 ) ;
#57081 = CARTESIAN_POINT ( 'NONE',  ( 4.549368137175248350, 38.59302160394725689, 18.79584381673547711 ) ) ;
#57082 = VERTEX_POINT ( 'NONE', #51431 ) ;
#57083 = CARTESIAN_POINT ( 'NONE',  ( 5.838029081930957709, 7.876159563729070889, 46.57285871276959455 ) ) ;
#57084 = LINE ( 'NONE', #8877, #21101 ) ;
#57085 = CARTESIAN_POINT ( 'NONE',  ( 0.6000166863083106206, -45.71468846346234471, -17.94410043432203494 ) ) ;
#57086 = ORIENTED_EDGE ( 'NONE', *, *, #28573, .T. ) ;
#57087 = CARTESIAN_POINT ( 'NONE',  ( 0.5988103564986357874, -44.67429521517320978, -17.84821699813467077 ) ) ;
#57088 =( BOUNDED_SURFACE ( )  B_SPLINE_SURFACE ( 3, 1, ( 
 ( #59172, #16279 ),
 ( #35403, #11590 ),
 ( #25987, #2148 ),
 ( #56324, #46965 ) ),
 .UNSPECIFIED., .F., .F., .F. ) 
 B_SPLINE_SURFACE_WITH_KNOTS ( ( 4, 4 ),
 ( 2, 2 ),
 ( 0.000000000000000000, 1.000000000000000000 ),
 ( 0.000000000000000000, 1.000000000000000000 ),
 .UNSPECIFIED. ) 
 GEOMETRIC_REPRESENTATION_ITEM ( )  RATIONAL_B_SPLINE_SURFACE ( (
 ( 1.000000000000000000, 1.000000000000000000),
 ( 0.7269869731126821222, 0.9931720237060910339),
 ( 0.7269869731126821222, 0.9931720237060910339),
 ( 1.000000000000000000, 1.000000000000000000) ) ) 
 REPRESENTATION_ITEM ( '' )  SURFACE ( )  );
#57090 = EDGE_CURVE ( 'NONE', #45131, #8350, #26821, .T. ) ;
#57089 = B_SPLINE_CURVE_WITH_KNOTS ( 'NONE', 3,
 ( #31415, #45235, #54894, #12028, #50512, #31103 ),
 .UNSPECIFIED., .F., .F.,
 ( 4, 2, 4 ),
 ( 1.463672932855430986E-18, 0.0002293801035737111881, 0.0004587602071474209124 ),
 .UNSPECIFIED. ) ;
#57091 = DIRECTION ( 'NONE',  ( -1.000000000000000000, 0.000000000000000000, 0.000000000000000000 ) ) ;
#57092 = EDGE_LOOP ( 'NONE', ( #36111, #54300, #51227, #34176 ) ) ;
#57093 = ORIENTED_EDGE ( 'NONE', *, *, #42674, .T. ) ;
#57094 = CARTESIAN_POINT ( 'NONE',  ( 0.9730545539215883499, 0.5054011016618756846, -42.90536227157002003 ) ) ;
#57095 = ORIENTED_EDGE ( 'NONE', *, *, #33173, .F. ) ;
#57096 = CARTESIAN_POINT ( 'NONE',  ( 3.660087539127321321, 35.27260502801134834, 32.61167949558399215 ) ) ;
#57097 = FACE_OUTER_BOUND ( 'NONE', #32377, .T. ) ;
#57098 = CARTESIAN_POINT ( 'NONE',  ( 0.9756354156337452288, -0.1303083999669958082, 42.90827993934337314 ) ) ;
#57099 = CARTESIAN_POINT ( 'NONE',  ( 3.661933894777898324, 44.00646638618364648, -16.61511604393246699 ) ) ;
#57100 = ORIENTED_EDGE ( 'NONE', *, *, #21356, .T. ) ;
#57101 = CARTESIAN_POINT ( 'NONE',  ( 4.322998006666165516, 14.45630056002939945, -45.75942687572284484 ) ) ;
#57102 = DIRECTION ( 'NONE',  ( -1.000000000000000000, -0.000000000000000000, -0.000000000000000000 ) ) ;
#57103 = CARTESIAN_POINT ( 'NONE',  ( 0.5834584762367761579, 36.91654477532374301, -28.92066235176340427 ) ) ;
#57104 = ORIENTED_EDGE ( 'NONE', *, *, #4727, .T. ) ;
#57105 = CARTESIAN_POINT ( 'NONE',  ( 0.9754292589017237169, -34.87747755813919071, -23.23551217590808449 ) ) ;
#57106 = CARTESIAN_POINT ( 'NONE',  ( 1.231276596079887931, 41.42457922925077440, -6.425029704024191268 ) ) ;
#57107 = CARTESIAN_POINT ( 'NONE',  ( 0.6254087463353906751, 38.58044986685651878, 28.73645667569962825 ) ) ;
#57108 = B_SPLINE_CURVE_WITH_KNOTS ( 'NONE', 3,
 ( #2076, #20902, #11510, #45048, #10583, #50026 ),
 .UNSPECIFIED., .F., .F.,
 ( 4, 2, 4 ),
 ( 1.269856260368691521E-16, 0.0002450741128632377090, 0.0004901482257263484578 ),
 .UNSPECIFIED. ) ;
#57109 = ORIENTED_EDGE ( 'NONE', *, *, #10176, .F. ) ;
#57110 = EDGE_LOOP ( 'NONE', ( #59827, #60040, #5222, #58791 ) ) ;
#57111 = CARTESIAN_POINT ( 'NONE',  ( 5.959828726073459926, 18.96492317065683153, 7.850628836606922789 ) ) ;
#57112 = CARTESIAN_POINT ( 'NONE',  ( 0.1102144999581333440, -42.77179372778547162, 5.503895401229260465 ) ) ;
#57113 = CARTESIAN_POINT ( 'NONE',  ( 0.8557997880470690211, 43.90420959842208504, -19.17299735371961944 ) ) ;
#57114 = CARTESIAN_POINT ( 'NONE',  ( 0.8753041380234471980, -43.21430456406350373, 23.31656511833038081 ) ) ;
#57115 = CARTESIAN_POINT ( 'NONE',  ( -2.708315649062910779, 5.356004933109274724, 13.61924161399635658 ) ) ;
#57116 = CARTESIAN_POINT ( 'NONE',  ( 0.9757402383260945777, -42.55239275983112890, 5.516496958496923675 ) ) ;
#57117 = CIRCLE ( 'NONE', #10100, 10.00000000000000000 ) ;
#57118 = CARTESIAN_POINT ( 'NONE',  ( 0.8751705887134553219, -29.98056538504934210, -37.60752970653818039 ) ) ;
#57119 = CARTESIAN_POINT ( 'NONE',  ( 4.975801465491694664, -14.85979367497141546, -45.55012473237748338 ) ) ;
#57120 = CARTESIAN_POINT ( 'NONE',  ( 5.960721111146673579, 20.35079619394242201, 2.672857320903374578 ) ) ;
#57121 = ADVANCED_FACE ( 'NONE', ( #27645 ), #24364, .F. ) ;
#57122 = CARTESIAN_POINT ( 'NONE',  ( -6.057079549204054558, -4.293366707802237947, -18.77227299535338290 ) ) ;
#57123 = CARTESIAN_POINT ( 'NONE',  ( 3.783278058412225864, -1.726763838445890320, -43.00370293663100085 ) ) ;
#57124 = ORIENTED_EDGE ( 'NONE', *, *, #31765, .T. ) ;
#57125 = EDGE_CURVE ( 'NONE', #61394, #9477, #1380, .T. ) ;
#57126 = CARTESIAN_POINT ( 'NONE',  ( 4.834790513006553603, -46.28862912354740189, -9.484310981144691510 ) ) ;
#57127 = CARTESIAN_POINT ( 'NONE',  ( -2.601141883200665639, 12.25953444924667401, 8.514648704269756507 ) ) ;
#57128 = CARTESIAN_POINT ( 'NONE',  ( 0.3676999524040366896, 10.61898383218289155, 42.81574203134493928 ) ) ;
#57129 = DIRECTION ( 'NONE',  ( 0.07906939808003034253, 0.7338893160900376023, 0.6746513929550271849 ) ) ;
#57130 = B_SPLINE_CURVE_WITH_KNOTS ( 'NONE', 3,
 ( #22252, #12868, #37286, #36668 ),
 .UNSPECIFIED., .F., .F.,
 ( 4, 4 ),
 ( 0.000000000000000000, 0.005004741218457393719 ),
 .UNSPECIFIED. ) ;
#57131 = FACE_OUTER_BOUND ( 'NONE', #29502, .T. ) ;
#57132 = CARTESIAN_POINT ( 'NONE',  ( 0.3622758884714730732, 29.89648521331631414, -31.06363466427696807 ) ) ;
#57133 = CARTESIAN_POINT ( 'NONE',  ( 0.6029442701453591180, 48.18517623212597556, -9.472804053565065274 ) ) ;
#57134 = CARTESIAN_POINT ( 'NONE',  ( 5.901463166500145796, 16.57349776239436068, 11.39460584050830327 ) ) ;
#57135 = CARTESIAN_POINT ( 'NONE',  ( 3.238741278300273141, 42.34697043723801357, 7.419593128524208936 ) ) ;
#57137 = ORIENTED_EDGE ( 'NONE', *, *, #52782, .T. ) ;
#57136 = CARTESIAN_POINT ( 'NONE',  ( -1.114299999999999846, 6.898680348956876061E-16, 5.633200000000004870 ) ) ;
#57138 = ORIENTED_EDGE ( 'NONE', *, *, #16924, .T. ) ;
#57139 = EDGE_CURVE ( 'NONE', #5538, #8036, #22384, .T. ) ;
#57140 = CARTESIAN_POINT ( 'NONE',  ( 4.834790513006553603, -26.65333699373555021, -39.01524020203834908 ) ) ;
#57141 = CARTESIAN_POINT ( 'NONE',  ( 0.1084644655670282676, 39.99242539812092190, 16.13497904887317347 ) ) ;
#57142 = EDGE_CURVE ( 'NONE', #13269, #35477, #12638, .T. ) ;
#57143 = ORIENTED_EDGE ( 'NONE', *, *, #37947, .F. ) ;
#57144 = CARTESIAN_POINT ( 'NONE',  ( 0.5832655196449135770, 22.33746898810849757, 41.23436263820043735 ) ) ;
#57145 = CARTESIAN_POINT ( 'NONE',  ( 0.5800708119828328346, 37.61306658477512599, -29.65250521075907386 ) ) ;
#57146 = CARTESIAN_POINT ( 'NONE',  ( 0.6001305935487315502, -44.64600790884043846, -17.92615948558525218 ) ) ;
#57147 =( BOUNDED_SURFACE ( )  B_SPLINE_SURFACE ( 3, 1, ( 
 ( #8802, #38266 ),
 ( #27919, #32625 ),
 ( #47042, #47956 ),
 ( #37967, #19762 ) ),
 .UNSPECIFIED., .F., .F., .F. ) 
 B_SPLINE_SURFACE_WITH_KNOTS ( ( 4, 4 ),
 ( 2, 2 ),
 ( 0.000000000000000000, 1.000000000000000000 ),
 ( 0.000000000000000000, 1.000000000000000000 ),
 .UNSPECIFIED. ) 
 GEOMETRIC_REPRESENTATION_ITEM ( )  RATIONAL_B_SPLINE_SURFACE ( (
 ( 1.000000000000000000, 1.000000000000000000),
 ( 0.9729067724841187204, 0.9999501103223794596),
 ( 0.9729067724841187204, 0.9999501103223794596),
 ( 1.000000000000000000, 1.000000000000000000) ) ) 
 REPRESENTATION_ITEM ( '' )  SURFACE ( )  );
#57148 = ORIENTED_EDGE ( 'NONE', *, *, #33173, .T. ) ;
#57149 = ORIENTED_EDGE ( 'NONE', *, *, #50593, .F. ) ;
#57150 = CARTESIAN_POINT ( 'NONE',  ( 4.956653778116987041, -47.27023054223747067, -8.845409907521421644 ) ) ;
#57151 = CARTESIAN_POINT ( 'NONE',  ( 0.8551540677456715978, -17.49081417858753795, -44.61036085020969466 ) ) ;
#57152 = CARTESIAN_POINT ( 'NONE',  ( 0.5837800304671213469, 16.89725109513926782, -43.74608825492073549 ) ) ;
#57153 = AXIS2_PLACEMENT_3D ( 'NONE', #22002, #31393, #50492 ) ;
#57154 = DIRECTION ( 'NONE',  ( 1.000000000000000000, 0.000000000000000000, 0.000000000000000000 ) ) ;
#57155 =( BOUNDED_SURFACE ( )  B_SPLINE_SURFACE ( 3, 1, ( 
 ( #31210, #6440 ),
 ( #50012, #16500 ),
 ( #45033, #11495 ),
 ( #30277, #26195 ) ),
 .UNSPECIFIED., .F., .F., .F. ) 
 B_SPLINE_SURFACE_WITH_KNOTS ( ( 4, 4 ),
 ( 2, 2 ),
 ( 0.000000000000000000, 1.000000000000000000 ),
 ( 0.000000000000000000, 1.000000000000000000 ),
 .UNSPECIFIED. ) 
 GEOMETRIC_REPRESENTATION_ITEM ( )  RATIONAL_B_SPLINE_SURFACE ( (
 ( 1.000000000000000000, 1.000000000000000000),
 ( 0.9754377213608244057, 0.9999580625633939235),
 ( 0.9754377213608244057, 0.9999580625633939235),
 ( 1.000000000000000000, 1.000000000000000000) ) ) 
 REPRESENTATION_ITEM ( '' )  SURFACE ( )  );
#57156 = EDGE_CURVE ( 'NONE', #4994, #49420, #2580, .T. ) ;
#57157 = CARTESIAN_POINT ( 'NONE',  ( 0.1149546198390367369, 33.42001444042882241, 28.81057444454637562 ) ) ;
#57158 = ORIENTED_EDGE ( 'NONE', *, *, #35466, .F. ) ;
#57159 = CARTESIAN_POINT ( 'NONE',  ( 4.975610109902397937, 0.000000000000000000, 0.000000000000000000 ) ) ;
#57160 = CARTESIAN_POINT ( 'NONE',  ( -6.072942160501519915, 19.10003410082481778, 2.448031788263668851 ) ) ;
#57161 = ORIENTED_EDGE ( 'NONE', *, *, #50872, .T. ) ;
#57162 = CARTESIAN_POINT ( 'NONE',  ( 0.9783242366443567484, -37.28257179578840663, -19.14012357583945345 ) ) ;
#57163 = CARTESIAN_POINT ( 'NONE',  ( -2.739355103387247858, -0.2155581815327103357, -14.92652342715447134 ) ) ;
#57164 = CARTESIAN_POINT ( 'NONE',  ( 0.5797568665920713737, -13.29195617976572663, 44.97276075044824495 ) ) ;
#57165 = CARTESIAN_POINT ( 'NONE',  ( 0.3676999524040323597, -43.84864779214683495, 4.821480075982420566 ) ) ;
#57166 = B_SPLINE_CURVE_WITH_KNOTS ( 'NONE', 3,
 ( #11482, #54674, #35918, #45019 ),
 .UNSPECIFIED., .F., .F.,
 ( 4, 4 ),
 ( 0.000000000000000000, 0.004446090762761373792 ),
 .UNSPECIFIED. ) ;
#57167 = ORIENTED_EDGE ( 'NONE', *, *, #58114, .F. ) ;
#57168 = ORIENTED_EDGE ( 'NONE', *, *, #36316, .F. ) ;
#57169 = CARTESIAN_POINT ( 'NONE',  ( 0.1154773475650540393, -44.12381759653407443, 0.1798631532872248806 ) ) ;
#57170 = CARTESIAN_POINT ( 'NONE',  ( 0.9730545539215883499, -42.60426903087349615, -5.099196237955331057 ) ) ;
#57171 = CARTESIAN_POINT ( 'NONE',  ( 5.896782393890504181, 8.471952691971054605, 18.24149403045202078 ) ) ;
#57172 =( REPRESENTATION_RELATIONSHIP ('NONE','NONE', #44881, #42491 ) REPRESENTATION_RELATIONSHIP_WITH_TRANSFORMATION ( #28642 )SHAPE_REPRESENTATION_RELATIONSHIP( ) );
#57173 = B_SPLINE_CURVE_WITH_KNOTS ( 'NONE', 3,
 ( #22089, #46221, #12392, #46841, #2965, #8275, #21464, #40603, #45919, #17699, #50275, #40917, #41837, #41215, #7981, #60904 ),
 .UNSPECIFIED., .F., .F.,
 ( 4, 3, 3, 3, 3, 4 ),
 ( 1.170988539753570110E-17, 0.0002732102107931889696, 0.0004098135523333795282, 0.0005464168938824970822, 0.0008195847345945433352, 0.001092771384553107650 ),
 .UNSPECIFIED. ) ;
#57174 = EDGE_LOOP ( 'NONE', ( #49632, #49860, #1173, #57487, #18480, #58182 ) ) ;
#57175 = CARTESIAN_POINT ( 'NONE',  ( 0.6041374136657476912, -33.89363087703070931, 34.14050483116080414 ) ) ;
#57176 = VERTEX_POINT ( 'NONE', #1279 ) ;
#57177 = CARTESIAN_POINT ( 'NONE',  ( 0.1313383488274130484, -26.75504982351785088, -33.82021892231536953 ) ) ;
#57178 = CARTESIAN_POINT ( 'NONE',  ( 0.5837157313716011542, 27.74442730813685998, 37.80851513780375939 ) ) ;
#57179 = ORIENTED_EDGE ( 'NONE', *, *, #46004, .T. ) ;
#57180 = CARTESIAN_POINT ( 'NONE',  ( 0.5834872094924179464, -0.2270145249676526200, 47.89542889285419136 ) ) ;
#57181 = CARTESIAN_POINT ( 'NONE',  ( 1.091591847532197512, -30.55658497080212044, -28.68891956623656370 ) ) ;
#57182 = DIRECTION ( 'NONE',  ( 0.000000000000000000, 0.000000000000000000, 1.000000000000000000 ) ) ;
#57183 = ORIENTED_EDGE ( 'NONE', *, *, #3147, .F. ) ;
#57184 = CARTESIAN_POINT ( 'NONE',  ( 0.5987334363312691865, -0.9689270393919278135, -49.09810675437915251 ) ) ;
#57185 = CARTESIAN_POINT ( 'NONE',  ( 0.1129192098497447394, 33.28205046155626690, -28.96993104685574139 ) ) ;
#57186 = CARTESIAN_POINT ( 'NONE',  ( 0.1073791018717578927, 10.69234304549997105, 41.77800844988518492 ) ) ;
#57187 = DIRECTION ( 'NONE',  ( 0.000000000000000000, 0.000000000000000000, -1.000000000000000000 ) ) ;
#57188 = CARTESIAN_POINT ( 'NONE',  ( 0.1092565886968784317, 16.21587544131324421, -39.95965440403629998 ) ) ;
#57189 = ORIENTED_EDGE ( 'NONE', *, *, #47688, .F. ) ;
#57190 = EDGE_CURVE ( 'NONE', #52200, #33819, #50011, .T. ) ;
#57191 = CARTESIAN_POINT ( 'NONE',  ( 4.975801465491695552, 0.000000000000000000, 0.000000000000000000 ) ) ;
#57192 = CARTESIAN_POINT ( 'NONE',  ( 2.706805983486679779, -16.28756729630821809, 40.88387536533181787 ) ) ;
#57193 = ORIENTED_EDGE ( 'NONE', *, *, #973, .F. ) ;
#57194 = EDGE_CURVE ( 'NONE', #44276, #40973, #42628, .T. ) ;
#57195 = CARTESIAN_POINT ( 'NONE',  ( 5.896278296736517710, 10.82699056113207092, 16.95002227147624652 ) ) ;
#57196 = CARTESIAN_POINT ( 'NONE',  ( 5.838029081930955932, 47.12733084333029865, 3.174861530241645191 ) ) ;
#57197 = CARTESIAN_POINT ( 'NONE',  ( 0.5800708119828331677, 18.90714262039473681, 44.00606550371067982 ) ) ;
#57198 = CARTESIAN_POINT ( 'NONE',  ( 4.967162193818131399, 35.57684288741977241, 24.30453456948122692 ) ) ;
#57199 = CARTESIAN_POINT ( 'NONE',  ( -6.063463321072276813, 5.494009911919050637, 18.45633516078436287 ) ) ;
#57200 = CARTESIAN_POINT ( 'NONE',  ( 0.6000166863083106206, 10.41802958826928638, 47.99258423138307705 ) ) ;
#57201 = VECTOR ( 'NONE', #46459, 999.9999999999998863 ) ;
#57202 = CARTESIAN_POINT ( 'NONE',  ( 0.5809828226811617480, -47.89273459658653564, -0.5448590168537535972 ) ) ;
#57203 = ADVANCED_FACE ( 'NONE', ( #39539 ), #23996, .F. ) ;
#57204 = CARTESIAN_POINT ( 'NONE',  ( 0.7948884756798517692, -29.92962957645406519, -38.92192079042860797 ) ) ;
#57205 = FACE_OUTER_BOUND ( 'NONE', #11202, .T. ) ;
#57206 = CARTESIAN_POINT ( 'NONE',  ( 0.3622758884714600280, -26.89560658783410574, 33.69533458712297147 ) ) ;
#57208 = VERTEX_POINT ( 'NONE', #14794 ) ;
#57207 = CARTESIAN_POINT ( 'NONE',  ( 0.1087620492084206414, -5.987629195158126194, 42.70684898916385208 ) ) ;
#57209 = ORIENTED_EDGE ( 'NONE', *, *, #61189, .F. ) ;
#57210 = CARTESIAN_POINT ( 'NONE',  ( -6.016104459813374383, 0.005335450885330034372, -18.84322058118302223 ) ) ;
#57211 = CARTESIAN_POINT ( 'NONE',  ( 0.8551540677456739292, 7.157691013575036010, -47.37911285756612756 ) ) ;
#57212 = ADVANCED_FACE ( 'NONE', ( #20114 ), #44, .T. ) ;
#57213 = CARTESIAN_POINT ( 'NONE',  ( -2.000000000000022649, -3.464101615137742396, 0.000000000000000000 ) ) ;
#57214 = FACE_OUTER_BOUND ( 'NONE', #23675, .T. ) ;
#57215 = CARTESIAN_POINT ( 'NONE',  ( 3.050102900204245682, 32.29689866186377856, -29.87198664306346174 ) ) ;
#57216 = EDGE_LOOP ( 'NONE', ( #43961, #60928, #53853, #38589 ) ) ;
#57217 = B_SPLINE_CURVE_WITH_KNOTS ( 'NONE', 3,
 ( #35904, #50286, #7351, #26478 ),
 .UNSPECIFIED., .F., .F.,
 ( 4, 4 ),
 ( 2.033478910116247305E-17, 0.004444306975806114161 ),
 .UNSPECIFIED. ) ;
#57218 = CARTESIAN_POINT ( 'NONE',  ( 1.227938101723748288, -29.74462687941204209, -30.94118573761343782 ) ) ;
#57219 = LINE ( 'NONE', #10263, #37224 ) ;
#57220 = DIRECTION ( 'NONE',  ( 0.000000000000000000, 0.000000000000000000, -1.000000000000000000 ) ) ;
#57221 = VERTEX_POINT ( 'NONE', #33595 ) ;
#57222 = DIRECTION ( 'NONE',  ( 0.07500201931887537365, 0.2825166499419793920, 0.9563258020171012674 ) ) ;
#57223 = CARTESIAN_POINT ( 'NONE',  ( 1.231276596079881047, -18.40965318903201364, 37.66113965983544887 ) ) ;
#57224 = VERTEX_POINT ( 'NONE', #25104 ) ;
#57225 = DIRECTION ( 'NONE',  ( -1.000000000000000000, -1.836909530733554547E-16, -1.836909530733573529E-16 ) ) ;
#57226 = ORIENTED_EDGE ( 'NONE', *, *, #26281, .T. ) ;
#57227 =( BOUNDED_SURFACE ( )  B_SPLINE_SURFACE ( 3, 1, ( 
 ( #32301, #61389 ),
 ( #52305, #37952 ),
 ( #33235, #9397 ),
 ( #47630, #4674 ) ),
 .UNSPECIFIED., .F., .F., .F. ) 
 B_SPLINE_SURFACE_WITH_KNOTS ( ( 4, 4 ),
 ( 2, 2 ),
 ( 0.000000000000000000, 1.000000000000000000 ),
 ( 0.000000000000000000, 1.000000000000000000 ),
 .UNSPECIFIED. ) 
 GEOMETRIC_REPRESENTATION_ITEM ( )  RATIONAL_B_SPLINE_SURFACE ( (
 ( 1.000000000000000000, 1.000000000000000000),
 ( 0.7269869731126817891, 0.9931720237060910339),
 ( 0.7269869731126817891, 0.9931720237060910339),
 ( 1.000000000000000000, 1.000000000000000000) ) ) 
 REPRESENTATION_ITEM ( '' )  SURFACE ( )  );
#57228 = CARTESIAN_POINT ( 'NONE',  ( 0.7048096507298579061, 33.41730025321705710, 34.61049487267071356 ) ) ;
#57229 = CARTESIAN_POINT ( 'NONE',  ( -6.057079549204054558, -1.857573237466950022, -19.16717644221978745 ) ) ;
#57230 = VERTEX_POINT ( 'NONE', #38610 ) ;
#57231 = CARTESIAN_POINT ( 'NONE',  ( 4.956445790444031552, 30.81386304088997719, -35.60960396630257208 ) ) ;
#57232 = CARTESIAN_POINT ( 'NONE',  ( -2.569797478183783568, -14.55946937464482893, -1.464172661884112214 ) ) ;
#57233 = CARTESIAN_POINT ( 'NONE',  ( 5.895881250540457863, 12.98195518060007103, 15.36217827318742657 ) ) ;
#57234 = ADVANCED_FACE ( 'NONE', ( #34211 ), #30753, .F. ) ;
#57235 = B_SPLINE_CURVE_WITH_KNOTS ( 'NONE', 3,
 ( #15774, #16083, #58972, #15158 ),
 .UNSPECIFIED., .F., .F.,
 ( 4, 4 ),
 ( 0.000000000000000000, 0.005013413432710150247 ),
 .UNSPECIFIED. ) ;
#57236 = AXIS2_PLACEMENT_3D ( 'NONE', #20049, #44487, #1516 ) ;
#57237 = VERTEX_POINT ( 'NONE', #52671 ) ;
#57238 = EDGE_CURVE ( 'NONE', #9806, #38401, #58588, .T. ) ;
#57239 = CARTESIAN_POINT ( 'NONE',  ( 0.6026112563231247332, -7.665567692565208091, -48.50546429893140044 ) ) ;
#57240 = ORIENTED_EDGE ( 'NONE', *, *, #29725, .T. ) ;
#57241 = CARTESIAN_POINT ( 'NONE',  ( -2.569797478183790229, 9.259773107243065127, -11.33042594333538666 ) ) ;
#57242 = AXIS2_PLACEMENT_3D ( 'NONE', #60254, #17369, #27375 ) ;
#57243 = B_SPLINE_CURVE_WITH_KNOTS ( 'NONE', 3,
 ( #23895, #63, #42108, #9169, #9791, #61766, #61461, #18904, #57074, #32378, #5064, #51453, #46802, #8545, #19513, #56165, #37394, #27668, #8868 ),
 .UNSPECIFIED., .F., .F.,
 ( 4, 3, 3, 3, 3, 3, 4 ),
 ( 1.734723475976807094E-18, 0.0002724573126191768939, 0.0004086839781548526514, 0.0005449106435901883167, 0.0006811373090491506990, 0.0008459866663933706754, 0.001010840725717216185 ),
 .UNSPECIFIED. ) ;
#57244 = ORIENTED_EDGE ( 'NONE', *, *, #50228, .T. ) ;
#57245 = ADVANCED_FACE ( 'NONE', ( #45702 ), #37559, .F. ) ;
#57246 = EDGE_LOOP ( 'NONE', ( #59586, #39136, #56658, #38951 ) ) ;
#57247 = DIRECTION ( 'NONE',  ( 1.000000000000000000, 1.836909530733573776E-16, 0.000000000000000000 ) ) ;
#57248 = CARTESIAN_POINT ( 'NONE',  ( 0.6029303876144825880, -34.10953954078163974, 33.92442033626723941 ) ) ;
#57249 = CARTESIAN_POINT ( 'NONE',  ( 0.9747592971366234593, 34.23774590565637510, 25.86343094887193317 ) ) ;
#57250 = CARTESIAN_POINT ( 'NONE',  ( 1.231276596079887931, 41.42457922925077440, -6.425029704024191268 ) ) ;
#57251 = ORIENTED_EDGE ( 'NONE', *, *, #16280, .T. ) ;
#57252 = CARTESIAN_POINT ( 'NONE',  ( 0.9757954354143122400, -4.033171854401937560E-17, -42.90846090505964128 ) ) ;
#57253 = CARTESIAN_POINT ( 'NONE',  ( 1.129531546211735016, 0.000000000000000000, -5.612499999999999822 ) ) ;
#57254 =( BOUNDED_SURFACE ( )  B_SPLINE_SURFACE ( 3, 1, ( 
 ( #27017, #36429 ),
 ( #8198, #13541 ),
 ( #41752, #22623 ),
 ( #56735, #17936 ) ),
 .UNSPECIFIED., .F., .F., .F. ) 
 B_SPLINE_SURFACE_WITH_KNOTS ( ( 4, 4 ),
 ( 2, 2 ),
 ( 0.000000000000000000, 1.000000000000000000 ),
 ( 0.000000000000000000, 1.000000000000000000 ),
 .UNSPECIFIED. ) 
 GEOMETRIC_REPRESENTATION_ITEM ( )  RATIONAL_B_SPLINE_SURFACE ( (
 ( 1.000000000000000000, 1.000000000000000000),
 ( 0.9754377213608244057, 0.9999580625633939235),
 ( 0.9754377213608244057, 0.9999580625633939235),
 ( 1.000000000000000000, 1.000000000000000000) ) ) 
 REPRESENTATION_ITEM ( '' )  SURFACE ( )  );
#57255 = CARTESIAN_POINT ( 'NONE',  ( 4.975801465491694664, -36.39623109580487892, 31.15993731089061924 ) ) ;
#57256 = B_SPLINE_CURVE_WITH_KNOTS ( 'NONE', 3,
 ( #40362, #27161, #12777, #8343 ),
 .UNSPECIFIED., .F., .F.,
 ( 4, 4 ),
 ( 0.000000000000000000, 0.004446090762761355578 ),
 .UNSPECIFIED. ) ;
#57257 = ORIENTED_EDGE ( 'NONE', *, *, #6119, .F. ) ;
#57258 = VERTEX_POINT ( 'NONE', #50374 ) ;
#57259 = CARTESIAN_POINT ( 'NONE',  ( 0.8753041380234471980, 16.12068986424767303, 46.38169559399184294 ) ) ;
#57260 = CARTESIAN_POINT ( 'NONE',  ( 0.1101816497532062955, 30.58948775778045004, 30.39741055095869982 ) ) ;
#57261 = CARTESIAN_POINT ( 'NONE',  ( 0.1102847568649952675, -34.15672344772105617, 26.32556309315059551 ) ) ;
#57262 = CARTESIAN_POINT ( 'NONE',  ( 0.1129192098497447394, -42.55567333040724520, 11.66046547873710537 ) ) ;
#57263 = EDGE_LOOP ( 'NONE', ( #38418, #53170, #15150, #50967 ) ) ;
#57264 = EDGE_CURVE ( 'NONE', #32172, #33924, #9604, .T. ) ;
#57265 = ORIENTED_EDGE ( 'NONE', *, *, #1037, .F. ) ;
#57266 = B_SPLINE_CURVE_WITH_KNOTS ( 'NONE', 3,
 ( #31566, #21863, #36589, #41004 ),
 .UNSPECIFIED., .F., .F.,
 ( 4, 4 ),
 ( 4.670885906470169924E-18, 0.004566006591234647236 ),
 .UNSPECIFIED. ) ;
#57267 = ADVANCED_FACE ( 'NONE', ( #31903 ), #47974, .F. ) ;
#57268 = CARTESIAN_POINT ( 'NONE',  ( 3.238741278300274029, -42.34697043723806331, -7.419593128523912284 ) ) ;
#57269 = CARTESIAN_POINT ( 'NONE',  ( 0.9788927965476035276, -41.04043099582347054, 8.486438375951868451 ) ) ;
#57270 = CARTESIAN_POINT ( 'NONE',  ( -4.908599999999998964, 1.224646799147353256E-15, -10.00000000000000000 ) ) ;
#57271 = CARTESIAN_POINT ( 'NONE',  ( 0.9757892942422835558, -21.40977514834409945, 37.18547544211205746 ) ) ;
#57272 = DIRECTION ( 'NONE',  ( 0.000000000000000000, 0.000000000000000000, 1.000000000000000000 ) ) ;
#57273 = EDGE_CURVE ( 'NONE', #57258, #33914, #49489, .T. ) ;
#57274 = SURFACE_STYLE_FILL_AREA ( #19717 ) ;
#57275 = CARTESIAN_POINT ( 'NONE',  ( 1.827119703190780653, -42.50321986945174046, 6.838980420687256867 ) ) ;
#57276 = ORIENTED_EDGE ( 'NONE', *, *, #54625, .T. ) ;
#57277 = CARTESIAN_POINT ( 'NONE',  ( -6.078726893082806448, -19.21666810860932983, -1.230328440814576041 ) ) ;
#57278 = CARTESIAN_POINT ( 'NONE',  ( 4.962356264823608143, 0.000000000000000000, 0.000000000000000000 ) ) ;
#57279 = CARTESIAN_POINT ( 'NONE',  ( -6.001507490154110336, -9.408444979392434959, 16.32705935667504349 ) ) ;
#57280 = CARTESIAN_POINT ( 'NONE',  ( 0.5782707292762442330, -46.74268073083581498, -3.854627323460666499 ) ) ;
#57281 = LINE ( 'NONE', #19419, #38248 ) ;
#57282 = EDGE_CURVE ( 'NONE', #11449, #43871, #612, .T. ) ;
#57283 = FACE_OUTER_BOUND ( 'NONE', #19051, .T. ) ;
#57284 = CIRCLE ( 'NONE', #3317, 47.91270532121795611 ) ;
#57285 = CARTESIAN_POINT ( 'NONE',  ( 2.000000000000010658, -3.464101615137748169, 0.000000000000000000 ) ) ;
#57286 = B_SPLINE_CURVE_WITH_KNOTS ( 'NONE', 3,
 ( #25276, #58454, #24044, #15581, #47866, #58154 ),
 .UNSPECIFIED., .F., .F.,
 ( 4, 2, 4 ),
 ( 1.736958732247374613E-17, 0.0002293319059085089783, 0.0004586638118170005551 ),
 .UNSPECIFIED. ) ;
#57287 = CARTESIAN_POINT ( 'NONE',  ( 2.648799415243696664, 31.92790172190984066, 37.21728838759838709 ) ) ;
#57288 = ORIENTED_EDGE ( 'NONE', *, *, #49552, .F. ) ;
#57289 = LINE ( 'NONE', #29424, #56894 ) ;
#57290 = CARTESIAN_POINT ( 'NONE',  ( 0.5839254288179550612, 18.41284501069738155, -44.21529885210810562 ) ) ;
#57291 = CARTESIAN_POINT ( 'NONE',  ( 2.528190830796654964, 40.15110720712335279, 12.25327410103500725 ) ) ;
#57292 = CARTESIAN_POINT ( 'NONE',  ( 0.2279481005628798962, 4.991633957252439302, -43.83591082103482961 ) ) ;
#57293 = ORIENTED_EDGE ( 'NONE', *, *, #14108, .T. ) ;
#57294 = CARTESIAN_POINT ( 'NONE',  ( 0.7242486021783792749, 32.40042614170994284, 36.89476721988594932 ) ) ;
#57295 = DIRECTION ( 'NONE',  ( 0.000000000000000000, 0.000000000000000000, 1.000000000000000000 ) ) ;
#57296 = VECTOR ( 'NONE', #25367, 1000.000000000000114 ) ;
#57297 = ORIENTED_EDGE ( 'NONE', *, *, #34385, .T. ) ;
#57298 = CARTESIAN_POINT ( 'NONE',  ( 0.8554163680231708922, -29.58718577084388102, -36.41159034254603455 ) ) ;
#57299 = CARTESIAN_POINT ( 'NONE',  ( 3.240649175237395596, 7.998380844884640517, 43.25841907950212573 ) ) ;
#57300 = ORIENTED_EDGE ( 'NONE', *, *, #19977, .F. ) ;
#57301 = CARTESIAN_POINT ( 'NONE',  ( 0.7044674535453004927, 16.16814117525605354, -46.37234017976553702 ) ) ;
#57302 = ORIENTED_EDGE ( 'NONE', *, *, #13452, .T. ) ;
#57303 = CARTESIAN_POINT ( 'NONE',  ( 4.553261556744873317, 40.80044851610476542, 16.27461110774448372 ) ) ;
#57304 = ORIENTED_EDGE ( 'NONE', *, *, #37727, .F. ) ;
#57305 = CARTESIAN_POINT ( 'NONE',  ( 0.5848930533535030563, -19.90539571549713926, 42.46231627922605867 ) ) ;
#57306 = CARTESIAN_POINT ( 'NONE',  ( 0.8753041380234465318, -14.82204010568780994, 46.81287702094758174 ) ) ;
#57307 = EDGE_CURVE ( 'NONE', #5305, #38501, #31517, .T. ) ;
#57308 = ORIENTED_EDGE ( 'NONE', *, *, #19519, .T. ) ;
#57309 = CARTESIAN_POINT ( 'NONE',  ( 5.959547316686252039, -0.003562808152765511386, -20.52562247508876681 ) ) ;
#57310 = PRODUCT_DEFINITION_SHAPE ( 'NONE', 'NONE',  #62000 ) ;
#57311 = ORIENTED_EDGE ( 'NONE', *, *, #5811, .F. ) ;
#57312 = EDGE_CURVE ( 'NONE', #41577, #539, #2443, .T. ) ;
#57313 = DIRECTION ( 'NONE',  ( 0.000000000000000000, 0.000000000000000000, 1.000000000000000000 ) ) ;
#57314 = CARTESIAN_POINT ( 'NONE',  ( 0.5817216825391117174, 40.57952703393794991, 23.50610426909058503 ) ) ;
#57315 = EDGE_CURVE ( 'NONE', #6564, #27525, #38835, .T. ) ;
#57316 = EDGE_LOOP ( 'NONE', ( #54883, #33939 ) ) ;
#57317 = EDGE_CURVE ( 'NONE', #13226, #44269, #44826, .T. ) ;
#57318 = DIRECTION ( 'NONE',  ( -1.000000000000000000, -0.000000000000000000, -0.000000000000000000 ) ) ;
#57319 = FACE_OUTER_BOUND ( 'NONE', #23931, .T. ) ;
#57320 = CARTESIAN_POINT ( 'NONE',  ( 0.1147471544378676211, -23.13865296268714289, -37.57066578523163258 ) ) ;
#57322 = EDGE_CURVE ( 'NONE', #26385, #47550, #58505, .T. ) ;
#57321 = ORIENTED_EDGE ( 'NONE', *, *, #18929, .F. ) ;
#57323 = CARTESIAN_POINT ( 'NONE',  ( 0.5827357941260210561, 44.38787053017151152, 17.99287562175603483 ) ) ;
#57324 = CARTESIAN_POINT ( 'NONE',  ( 0.8751705887134423323, -13.30665218149394669, 46.21789262997734227 ) ) ;
#57325 = B_SPLINE_CURVE_WITH_KNOTS ( 'NONE', 3,
 ( #43885, #34773, #930, #14434 ),
 .UNSPECIFIED., .F., .F.,
 ( 4, 4 ),
 ( 0.000000000000000000, 0.005013413432710153717 ),
 .UNSPECIFIED. ) ;
#57326 = EDGE_LOOP ( 'NONE', ( #56453, #57937 ) ) ;
#57327 = VECTOR ( 'NONE', #43151, 1000.000000000000227 ) ;
#57328 = CARTESIAN_POINT ( 'NONE',  ( 5.965394784446458765, -16.27505370423089559, 12.50653125158980039 ) ) ;
#57329 =( BOUNDED_SURFACE ( )  B_SPLINE_SURFACE ( 3, 1, ( 
 ( #2039, #1419 ),
 ( #6721, #53431 ),
 ( #58738, #20864 ),
 ( #11164, #21168 ) ),
 .UNSPECIFIED., .F., .F., .F. ) 
 B_SPLINE_SURFACE_WITH_KNOTS ( ( 4, 4 ),
 ( 2, 2 ),
 ( 0.000000000000000000, 1.000000000000000000 ),
 ( 0.000000000000000000, 1.000000000000000000 ),
 .UNSPECIFIED. ) 
 GEOMETRIC_REPRESENTATION_ITEM ( )  RATIONAL_B_SPLINE_SURFACE ( (
 ( 1.000000000000000000, 1.000000000000000000),
 ( 0.7269869731126821222, 0.9931720237060910339),
 ( 0.7269869731126821222, 0.9931720237060910339),
 ( 1.000000000000000000, 1.000000000000000000) ) ) 
 REPRESENTATION_ITEM ( '' )  SURFACE ( )  );
#57330 = ORIENTED_EDGE ( 'NONE', *, *, #22087, .T. ) ;
#57331 = CARTESIAN_POINT ( 'NONE',  ( 0.9730545539215883499, 25.71816799638778406, 34.34678117142565412 ) ) ;
#57332 = EDGE_CURVE ( 'NONE', #23013, #9930, #30581, .T. ) ;
#57333 = CARTESIAN_POINT ( 'NONE',  ( -31.75000000000000000, -15.14599999999999369, 1.854850041988580043E-15 ) ) ;
#57334 = ORIENTED_EDGE ( 'NONE', *, *, #5446, .F. ) ;
#57335 = CARTESIAN_POINT ( 'NONE',  ( 0.9790724872846768845, -34.52833649645707226, -23.75140393258649496 ) ) ;
#57336 = CARTESIAN_POINT ( 'NONE',  ( 4.967162193818130511, -24.30453456948135482, 35.57684288741969425 ) ) ;
#57337 = CARTESIAN_POINT ( 'NONE',  ( 0.9787464366903553259, -22.40087524910941141, -35.41941248756537419 ) ) ;
#57338 = EDGE_CURVE ( 'NONE', #49479, #39074, #31276, .T. ) ;
#57339 = B_SPLINE_CURVE_WITH_KNOTS ( 'NONE', 3,
 ( #29020, #47832, #28092, #48132, #27784, #14017 ),
 .UNSPECIFIED., .F., .F.,
 ( 4, 2, 4 ),
 ( 1.269611854458016711E-16, 0.0002450741128632354863, 0.0004901482257263440126 ),
 .UNSPECIFIED. ) ;
#57340 = EDGE_LOOP ( 'NONE', ( #18, #53016, #21831, #51158 ) ) ;
#57341 = FACE_OUTER_BOUND ( 'NONE', #61617, .T. ) ;
#57342 = DIRECTION ( 'NONE',  ( 1.000000000000000000, 0.000000000000000000, 0.000000000000000000 ) ) ;
#57344 = B_SPLINE_CURVE_WITH_KNOTS ( 'NONE', 3,
 ( #24174, #58592, #20115, #48601, #5658, #347, #15104, #52986, #10088, #15411, #24801, #29184, #25408, #48299, #57982, #981 ),
 .UNSPECIFIED., .F., .F.,
 ( 4, 3, 3, 3, 3, 4 ),
 ( 1.084256381238943740E-17, 0.0002732102107931898912, 0.0004098135523333806666, 0.0005464168938824980580, 0.0008195847345945435521, 0.001092771384553107216 ),
 .UNSPECIFIED. ) ;
#57343 = CARTESIAN_POINT ( 'NONE',  ( 0.8751705887134553219, -19.22545746485630502, -44.08562551107074512 ) ) ;
#57345 = CONICAL_SURFACE ( 'NONE', #8348, 43.92652462719577500, 1.486293639869522343 ) ;
#57346 = CARTESIAN_POINT ( 'NONE',  ( 0.5837374860065643878, -44.18034382476633937, 18.49670552082939068 ) ) ;
#57347 = B_SPLINE_CURVE_WITH_KNOTS ( 'NONE', 3,
 ( #13043, #57140, #14273, #33379 ),
 .UNSPECIFIED., .F., .F.,
 ( 4, 4 ),
 ( 3.469446951953613804E-18, 0.005013413432710145910 ),
 .UNSPECIFIED. ) ;
#57348 = CARTESIAN_POINT ( 'NONE',  ( 1.231276596079887931, -41.24008908601417289, -7.518764738684258653 ) ) ;
#57349 = CARTESIAN_POINT ( 'NONE',  ( 0.5987334363312691865, -35.69483761714066361, 33.72597624914712355 ) ) ;
#57350 = CARTESIAN_POINT ( 'NONE',  ( 0.6252788684277206244, 46.81660596960011844, 14.82058489604466445 ) ) ;
#57351 = DIRECTION ( 'NONE',  ( -1.000000000000000000, -0.000000000000000000, -0.000000000000000000 ) ) ;
#57352 = DIRECTION ( 'NONE',  ( 0.000000000000000000, 0.000000000000000000, 1.000000000000000000 ) ) ;
#57353 = CARTESIAN_POINT ( 'NONE',  ( 0.6030672727741701600, 48.10738703097480595, 0.08725775308938291119 ) ) ;
#57354 = EDGE_CURVE ( 'NONE', #30576, #29913, #58861, .T. ) ;
#57355 = CARTESIAN_POINT ( 'NONE',  ( 0.9762797500689124330, 28.76866969768027715, -30.47438972336406238 ) ) ;
#57356 = CARTESIAN_POINT ( 'NONE',  ( 5.838029081930957709, 35.01788019483870329, -31.69878743442473734 ) ) ;
#57357 = CARTESIAN_POINT ( 'NONE',  ( 4.956445790444004018, -45.55738122058073003, 11.91902120403828036 ) ) ;
#57358 = CARTESIAN_POINT ( 'NONE',  ( 0.5834872094924170582, -23.75111410077682095, -41.59216540884688840 ) ) ;
#57359 = ADVANCED_FACE ( 'NONE', ( #60684 ), #43166, .T. ) ;
#57360 = CARTESIAN_POINT ( 'NONE',  ( 0.5997462898726536595, -45.71211507932765983, -17.94308126043611296 ) ) ;
#57361 = CARTESIAN_POINT ( 'NONE',  ( 8.000000000000012434, -80.00000000000001421, -2.649999999999992806 ) ) ;
#57362 = DIRECTION ( 'NONE',  ( 0.07500201931887538753, -0.9652320423656591819, 0.2504032777115935415 ) ) ;
#57363 = ORIENTED_EDGE ( 'NONE', *, *, #59918, .F. ) ;
#57364 = CARTESIAN_POINT ( 'NONE',  ( 0.5827359174754833671, 29.44457394064674105, -37.77623182210365371 ) ) ;
#57365 = DIRECTION ( 'NONE',  ( 0.000000000000000000, 0.000000000000000000, 1.000000000000000000 ) ) ;
#57366 = ORIENTED_EDGE ( 'NONE', *, *, #12724, .T. ) ;
#57367 = CARTESIAN_POINT ( 'NONE',  ( 0.9730545539215883499, 6.101350888304637010, 42.47233286818619291 ) ) ;
#57368 = CARTESIAN_POINT ( 'NONE',  ( 0.5549461598389362482, 25.94790012659789014, 35.66404596350370326 ) ) ;
#57369 = AXIS2_PLACEMENT_3D ( 'NONE', #23556, #23872, #28254 ) ;
#57370 = VERTEX_POINT ( 'NONE', #42859 ) ;
#57371 = ORIENTED_EDGE ( 'NONE', *, *, #16366, .T. ) ;
#57372 = CARTESIAN_POINT ( 'NONE',  ( 0.5987334363312686314, -31.08900137594245550, 38.01364097161339117 ) ) ;
#57373 = ORIENTED_EDGE ( 'NONE', *, *, #5911, .T. ) ;
#57374 = CARTESIAN_POINT ( 'NONE',  ( 0.5806925824938502512, 28.25565086187734920, 37.42780459384778879 ) ) ;
#57375 = ORIENTED_EDGE ( 'NONE', *, *, #42398, .F. ) ;
#57376 = ORIENTED_EDGE ( 'NONE', *, *, #52756, .F. ) ;
#57377 = CARTESIAN_POINT ( 'NONE',  ( 0.5819845901640492425, -11.95725023767325190, -46.37938751183695985 ) ) ;
#57378 = ORIENTED_EDGE ( 'NONE', *, *, #22659, .T. ) ;
#57379 = CARTESIAN_POINT ( 'NONE',  ( 5.917102823773431552, -4.670717611792251311, -19.56205804721567887 ) ) ;
#57380 = FACE_OUTER_BOUND ( 'NONE', #58079, .T. ) ;
#57381 = VECTOR ( 'NONE', #31940, 1000.000000000000114 ) ;
#57382 = CARTESIAN_POINT ( 'NONE',  ( 4.322998006666165516, -45.75942687572288037, -14.45630056002923780 ) ) ;
#57383 = ORIENTED_EDGE ( 'NONE', *, *, #60677, .F. ) ;
#57384 = ADVANCED_FACE ( 'NONE', ( #28736 ), #39570, .F. ) ;
#57385 = DIRECTION ( 'NONE',  ( 0.000000000000000000, 0.000000000000000000, 1.000000000000000000 ) ) ;
#57386 = CARTESIAN_POINT ( 'NONE',  ( 0.6023142530420679819, -48.10676733004997629, 0.2618396477465863015 ) ) ;
#57387 = ORIENTED_EDGE ( 'NONE', *, *, #58060, .T. ) ;
#57388 = VERTEX_POINT ( 'NONE', #47236 ) ;
#57389 = EDGE_CURVE ( 'NONE', #58614, #16223, #61608, .T. ) ;
#57390 = CARTESIAN_POINT ( 'NONE',  ( -0.2111111111111110827, -9.497654031326126400, 0.000000000000000000 ) ) ;
#57391 = VERTEX_POINT ( 'NONE', #9947 ) ;
#57392 = CARTESIAN_POINT ( 'NONE',  ( 0.6026777506516367566, 46.66034804694161409, 15.30876581490131905 ) ) ;
#57393 = CARTESIAN_POINT ( 'NONE',  ( 1.088908134280553996, -41.24246781061824407, 11.85879120571491896 ) ) ;
#57394 = CARTESIAN_POINT ( 'NONE',  ( 5.959547316686252039, 16.28190225198601127, 12.49803383497755682 ) ) ;
#57395 = ADVANCED_FACE ( 'NONE', ( #33453 ), #52218, .F. ) ;
#57396 = CARTESIAN_POINT ( 'NONE',  ( 0.8751705887134423323, -13.30665218149394669, 46.21789262997734227 ) ) ;
#57397 = B_SPLINE_CURVE_WITH_KNOTS ( 'NONE', 3,
 ( #580, #48828, #38841, #44169, #15025, #34133, #10312, #48516, #12481, #6810, #50065, #11555, #1814, #41011, #6494, #60071, #54115, #2431, #2740 ),
 .UNSPECIFIED., .F., .F.,
 ( 4, 3, 3, 3, 3, 3, 4 ),
 ( 1.734776414728241573E-18, 0.0002612768053151736064, 0.0003919133833142913049, 0.0005225499612322628135, 0.0006531865391693353080, 0.0008112755173415186647, 0.0009693688056799721394 ),
 .UNSPECIFIED. ) ;
#57398 = VERTEX_POINT ( 'NONE', #38164 ) ;
#57399 = CARTESIAN_POINT ( 'NONE',  ( 0.6023143664670691511, -12.70384782338121887, 46.39980466492338707 ) ) ;
#57400 = LINE ( 'NONE', #28923, #37768 ) ;
#57401 = CARTESIAN_POINT ( 'NONE',  ( 0.5837800304671211249, 36.83215615041540048, -29.02808304884970170 ) ) ;
#57402 = B_SPLINE_CURVE_WITH_KNOTS ( 'NONE', 3,
 ( #5358, #33912, #34216, #10403 ),
 .UNSPECIFIED., .F., .F.,
 ( 4, 4 ),
 ( 0.000000000000000000, 0.004445488388166995118 ),
 .UNSPECIFIED. ) ;
#57403 = ORIENTED_EDGE ( 'NONE', *, *, #59318, .T. ) ;
#57404 = CARTESIAN_POINT ( 'NONE',  ( 4.960386119450136633, 18.84353550694723012, 39.48870261569452822 ) ) ;
#57405 = DIRECTION ( 'NONE',  ( -1.000000000000000000, -0.000000000000000000, -0.000000000000000000 ) ) ;
#57406 = CARTESIAN_POINT ( 'NONE',  ( 1.000110580585055198, 33.29435990446771143, -25.45394038893929078 ) ) ;
#57407 = B_SPLINE_CURVE_WITH_KNOTS ( 'NONE', 3,
 ( #54581, #30792, #49913, #6967 ),
 .UNSPECIFIED., .F., .F.,
 ( 4, 4 ),
 ( 2.186012127670277422E-17, 0.004559932413162186803 ),
 .UNSPECIFIED. ) ;
#57408 = ORIENTED_EDGE ( 'NONE', *, *, #53091, .F. ) ;
#57409 = VERTEX_POINT ( 'NONE', #57518 ) ;
#57410 = DIRECTION ( 'NONE',  ( 0.000000000000000000, 0.000000000000000000, 1.000000000000000000 ) ) ;
#57411 = CARTESIAN_POINT ( 'NONE',  ( 0.2224561200757604607, 37.71651051365630281, -20.89867881469728772 ) ) ;
#57412 = CARTESIAN_POINT ( 'NONE',  ( 0.9730545539215883499, -16.88610103448528221, -39.44597740938079511 ) ) ;
#57413 = CARTESIAN_POINT ( 'NONE',  ( 4.553261556744873317, 42.54662847375970358, 10.92355122382355148 ) ) ;
#57414 = CIRCLE ( 'NONE', #6380, 43.92652462719577500 ) ;
#57415 = CARTESIAN_POINT ( 'NONE',  ( 5.894904586330512508, 18.99964780500586059, 6.598696488502780788 ) ) ;
#57416 = CARTESIAN_POINT ( 'NONE',  ( 0.1129192098497447394, -18.30288010335054949, -40.14917642626718930 ) ) ;
#57417 = DIRECTION ( 'NONE',  ( 0.09835009131224552170, -0.9951218349151971232, 0.007732607185427432805 ) ) ;
#57418 = CARTESIAN_POINT ( 'NONE',  ( 5.910764540655178756, 12.99683459030013211, 15.34873053713371327 ) ) ;
#57419 = DIRECTION ( 'NONE',  ( -0.07836865515943411409, -0.7104869166656990753, -0.6993330359244940286 ) ) ;
#57420 = CARTESIAN_POINT ( 'NONE',  ( 0.6845945791218034371, -44.02134436206625878, -16.20270845477142529 ) ) ;
#57421 = AXIS2_PLACEMENT_3D ( 'NONE', #6698, #7325, #53701 ) ;
#57422 = CARTESIAN_POINT ( 'NONE',  ( 5.901764892641288895, 7.858096707078647825, 48.33468509861089046 ) ) ;
#57423 = CARTESIAN_POINT ( 'NONE',  ( 0.1073791018717578927, 16.95003405440313315, -39.65380858626198091 ) ) ;
#57424 = ORIENTED_EDGE ( 'NONE', *, *, #40535, .F. ) ;
#57425 = DIRECTION ( 'NONE',  ( 1.000000000000000000, 0.000000000000000000, 0.000000000000000000 ) ) ;
#57426 = CARTESIAN_POINT ( 'NONE',  ( 0.2279481005628827273, -35.80664021588747659, 25.77572508238910487 ) ) ;
#57427 = FACE_OUTER_BOUND ( 'NONE', #60224, .T. ) ;
#57428 = DIRECTION ( 'NONE',  ( 0.07906939808003035641, -0.1078133555910006508, 0.9910218517487240364 ) ) ;
#57429 = CIRCLE ( 'NONE', #11454, 15.14599999999999369 ) ;
#57430 = CARTESIAN_POINT ( 'NONE',  ( 5.440000000000003055, -15.43999999999998529, 1.890854657883512518E-15 ) ) ;
#57431 = CARTESIAN_POINT ( 'NONE',  ( 0.1102144999581333024, 42.73889315046712056, 5.753800096706190637 ) ) ;
#57432 = CARTESIAN_POINT ( 'NONE',  ( -5.995132425357893702, 18.84415457712583475, -0.008513469642872414228 ) ) ;
#57433 = CARTESIAN_POINT ( 'NONE',  ( 120.0000507999999968, 0.000000000000000000, 8.000000000000000000 ) ) ;
#57434 = EDGE_CURVE ( 'NONE', #19166, #7929, #11072, .T. ) ;
#57435 = CARTESIAN_POINT ( 'NONE',  ( 0.9752132459055864455, -10.88033124649650141, 41.50604997043410549 ) ) ;
#57436 = CARTESIAN_POINT ( 'NONE',  ( 3.238741278300275361, 27.59904135366535272, -32.96375560769470781 ) ) ;
#57438 = ORIENTED_EDGE ( 'NONE', *, *, #8066, .T. ) ;
#57437 = CARTESIAN_POINT ( 'NONE',  ( 0.6023143664670691511, -46.39980466492352917, -12.70384782338073215 ) ) ;
#57439 = ORIENTED_EDGE ( 'NONE', *, *, #18681, .T. ) ;
#57440 = CARTESIAN_POINT ( 'NONE',  ( 1.157644175074337145, 36.47889980312224623, -20.64684345445932223 ) ) ;
#57441 = FACE_OUTER_BOUND ( 'NONE', #25491, .T. ) ;
#57442 = ORIENTED_EDGE ( 'NONE', *, *, #5123, .T. ) ;
#57443 = CARTESIAN_POINT ( 'NONE',  ( -6.057079549204054558, -18.90023728169077444, 3.689479881436475761 ) ) ;
#57444 = CARTESIAN_POINT ( 'NONE',  ( 0.8557997880470697982, 37.44587306708137930, -29.88293891557432858 ) ) ;
#57445 = FACE_OUTER_BOUND ( 'NONE', #12239, .T. ) ;
#57446 = ORIENTED_EDGE ( 'NONE', *, *, #40120, .T. ) ;
#57447 = AXIS2_PLACEMENT_3D ( 'NONE', #7281, #49917, #35527 ) ;
#57448 = ORIENTED_EDGE ( 'NONE', *, *, #27900, .T. ) ;
#57449 = CARTESIAN_POINT ( 'NONE',  ( 4.549368137175248350, 35.80950303116068056, 23.67244292351653101 ) ) ;
#57450 = CARTESIAN_POINT ( 'NONE',  ( 0.8751705887134553219, -29.98056538504934210, -37.60752970653818039 ) ) ;
#57451 = CARTESIAN_POINT ( 'NONE',  ( -6.063463321072278589, -16.13029782234875142, -10.51826718817319950 ) ) ;
#57452 = CARTESIAN_POINT ( 'NONE',  ( 4.962356264823608143, 22.27740539909265394, 35.70648129607319277 ) ) ;
#57453 = CARTESIAN_POINT ( 'NONE',  ( 0.2230388203127597058, 10.42432885623882122, -41.84042374003681886 ) ) ;
#57454 = EDGE_CURVE ( 'NONE', #15923, #52379, #25333, .T. ) ;
#57455 = CONICAL_SURFACE ( 'NONE', #19498, 43.08621763946400307, 1.568696531533066763 ) ;
#57456 = CARTESIAN_POINT ( 'NONE',  ( 0.9756950546413926117, 42.55388731055347762, 5.504753251347860754 ) ) ;
#57457 = EDGE_CURVE ( 'NONE', #2852, #15622, #45534, .T. ) ;
#57458 = ORIENTED_EDGE ( 'NONE', *, *, #32217, .F. ) ;
#57459 = ORIENTED_EDGE ( 'NONE', *, *, #6313, .F. ) ;
#57460 = CARTESIAN_POINT ( 'NONE',  ( 4.958415959904823644, -35.33199410137723362, 28.54565022280773690 ) ) ;
#57461 = CARTESIAN_POINT ( 'NONE',  ( 4.553261556744875094, 43.53643125131386427, 5.841123155974254466 ) ) ;
#57462 = CONICAL_SURFACE ( 'NONE', #36502, 42.08604991992415023, 1.569615340895231137 ) ;
#57463 = ORIENTED_EDGE ( 'NONE', *, *, #15207, .T. ) ;
#57464 = CARTESIAN_POINT ( 'NONE',  ( 1.154321485836933947, -37.57248783354756938, -20.73950273457881366 ) ) ;
#57465 = CARTESIAN_POINT ( 'NONE',  ( 4.549368137175248350, 35.80950303116100741, -23.67244292351601942 ) ) ;
#57466 = EDGE_CURVE ( 'NONE', #50567, #31453, #29047, .T. ) ;
#57467 = CARTESIAN_POINT ( 'NONE',  ( 0.7764146366350247463, -13.04263738120156191, 45.05474540835458441 ) ) ;
#57468 = VECTOR ( 'NONE', #4684, 1000.000000000000000 ) ;
#57469 = ORIENTED_EDGE ( 'NONE', *, *, #31649, .F. ) ;
#57470 = ORIENTED_EDGE ( 'NONE', *, *, #3741, .F. ) ;
#57471 = CARTESIAN_POINT ( 'NONE',  ( 0.9747592971366217940, 0.3237797888854979655, 42.90728926179870939 ) ) ;
#57472 = CARTESIAN_POINT ( 'NONE',  ( -6.017396004339686577, 17.40926186480779592, 7.209881890566617102 ) ) ;
#57473 = CARTESIAN_POINT ( 'NONE',  ( 0.1101816497532063233, -37.41460501058200094, -21.44450189183855571 ) ) ;
#57474 = DIRECTION ( 'NONE',  ( -1.000000000000000000, -0.000000000000000000, -0.000000000000000000 ) ) ;
#57475 = ORIENTED_EDGE ( 'NONE', *, *, #26651, .T. ) ;
#57476 = CARTESIAN_POINT ( 'NONE',  ( 0.1129192098497455998, 42.02659449688937343, -13.44310763101974260 ) ) ;
#57477 = ORIENTED_EDGE ( 'NONE', *, *, #46076, .T. ) ;
#57478 = CARTESIAN_POINT ( 'NONE',  ( -6.001507490154110336, 9.435425682280817128, 16.31148204059951112 ) ) ;
#57479 = CARTESIAN_POINT ( 'NONE',  ( 0.5837799406558225046, 27.89109207889182684, 37.70053755881976798 ) ) ;
#57480 = EDGE_CURVE ( 'NONE', #27859, #47737, #8690, .T. ) ;
#57481 = ORIENTED_EDGE ( 'NONE', *, *, #45938, .F. ) ;
#57482 = CARTESIAN_POINT ( 'NONE',  ( 5.895596859100789899, -17.30333226730986240, 10.25294473112777105 ) ) ;
#57483 = CARTESIAN_POINT ( 'NONE',  ( -5.995132425357893702, 16.32377331145320554, 9.414704407577861645 ) ) ;
#57484 = ADVANCED_FACE ( 'NONE', ( #19659 ), #57462, .T. ) ;
#57485 = CARTESIAN_POINT ( 'NONE',  ( 0.9730545539215883499, -39.83279466599050522, 15.95224156741815236 ) ) ;
#57486 = B_SPLINE_CURVE_WITH_KNOTS ( 'NONE', 3,
 ( #31509, #4828, #52151, #23969 ),
 .UNSPECIFIED., .F., .F.,
 ( 4, 4 ),
 ( 0.000000000000000000, 0.005014147105413699519 ),
 .UNSPECIFIED. ) ;
#57487 = ORIENTED_EDGE ( 'NONE', *, *, #21706, .F. ) ;
#57488 = CARTESIAN_POINT ( 'NONE',  ( 0.6031356755773454870, -29.28597628606519976, -38.16618524502111853 ) ) ;
#57489 = CARTESIAN_POINT ( 'NONE',  ( 4.691466044806102076, 20.01963481131660672, -39.84135254923116065 ) ) ;
#57490 = CARTESIAN_POINT ( 'NONE',  ( 4.549368137175248350, 42.82045902618768451, 3.018832571116707442 ) ) ;
#57491 = AXIS2_PLACEMENT_3D ( 'NONE', #33383, #61840, #27742 ) ;
#57492 = CARTESIAN_POINT ( 'NONE',  ( 2.281351352603298022, 47.71649595778620778, -4.956540261593279872 ) ) ;
#57493 = CARTESIAN_POINT ( 'NONE',  ( -6.001507490154111224, -2.444174634178017946, -18.68469198366099349 ) ) ;
#57494 = EDGE_LOOP ( 'NONE', ( #5178, #42307 ) ) ;
#57495 = CARTESIAN_POINT ( 'NONE',  ( 5.896782393890504181, 19.70854070425246363, 4.012419492879101490 ) ) ;
#57496 = CARTESIAN_POINT ( 'NONE',  ( 0.5817217712918330008, 28.18299969253300929, -37.48270911152311413 ) ) ;
#57497 = VERTEX_POINT ( 'NONE', #34076 ) ;
#57498 = B_SPLINE_CURVE_WITH_KNOTS ( 'NONE', 3,
 ( #16086, #30780, #1332, #20467, #39598, #20779 ),
 .UNSPECIFIED., .F., .F.,
 ( 4, 2, 4 ),
 ( 1.015220885719448636E-17, 0.0002291978881530150217, 0.0004583957763060198518 ),
 .UNSPECIFIED. ) ;
#57499 = PLANE ( 'NONE',  #30897 ) ;
#57500 = DIRECTION ( 'NONE',  ( -0.9990097760809876215, 5.448601141171616265E-18, -0.04449120468828354769 ) ) ;
#57501 = B_SPLINE_CURVE_WITH_KNOTS ( 'NONE', 3,
 ( #8964, #41572, #61562, #23375, #28073, #41889 ),
 .UNSPECIFIED., .F., .F.,
 ( 4, 2, 4 ),
 ( 3.361026734705063745E-18, 0.0002447193893791674854, 0.0004894387787583316099 ),
 .UNSPECIFIED. ) ;
#57502 = CARTESIAN_POINT ( 'NONE',  ( 3.680974057930773036, -27.71659654258268546, -39.15945827951701119 ) ) ;
#57503 = CARTESIAN_POINT ( 'NONE',  ( 4.975610109902397937, 30.04451009524531102, -38.59762713269398660 ) ) ;
#57504 = CARTESIAN_POINT ( 'NONE',  ( 3.661933894777862797, 47.00091140061822870, 1.882947812046177116 ) ) ;
#57505 = CARTESIAN_POINT ( 'NONE',  ( 0.5800708119828335008, -28.65679933661821721, 38.37709857409259229 ) ) ;
#57506 = CARTESIAN_POINT ( 'NONE',  ( 52.11658891626548495, 15.35644817774449145, 2.106865129802042436 ) ) ;
#57507 = CARTESIAN_POINT ( 'NONE',  ( 4.334026318920000342, 0.4760547705731076329, 0.7070397585357669490 ) ) ;
#57508 = CARTESIAN_POINT ( 'NONE',  ( 0.5835226383429291674, 11.04855730340264408, 45.57600087830647340 ) ) ;
#57509 =( BOUNDED_SURFACE ( )  B_SPLINE_SURFACE ( 3, 1, ( 
 ( #3145, #22272 ),
 ( #50759, #37012 ),
 ( #2834, #7849 ),
 ( #56072, #17268 ) ),
 .UNSPECIFIED., .F., .F., .F. ) 
 B_SPLINE_SURFACE_WITH_KNOTS ( ( 4, 4 ),
 ( 2, 2 ),
 ( 0.000000000000000000, 1.000000000000000000 ),
 ( 0.000000000000000000, 1.000000000000000000 ),
 .UNSPECIFIED. ) 
 GEOMETRIC_REPRESENTATION_ITEM ( )  RATIONAL_B_SPLINE_SURFACE ( (
 ( 1.000000000000000000, 1.000000000000000000),
 ( 0.7211978278499968642, 0.9934217856018975334),
 ( 0.7211978278499968642, 0.9934217856018975334),
 ( 1.000000000000000000, 1.000000000000000000) ) ) 
 REPRESENTATION_ITEM ( '' )  SURFACE ( )  );
#57510 = EDGE_CURVE ( 'NONE', #50764, #14922, #41778, .T. ) ;
#57511 = DIRECTION ( 'NONE',  ( -1.000000000000000000, -0.000000000000000000, -0.000000000000000000 ) ) ;
#57512 = AXIS2_PLACEMENT_3D ( 'NONE', #46809, #52390, #9484 ) ;
#57513 = CARTESIAN_POINT ( 'NONE',  ( 4.967162193818130511, 0.000000000000000000, 0.000000000000000000 ) ) ;
#57515 = ORIENTED_EDGE ( 'NONE', *, *, #18124, .T. ) ;
#57514 = CARTESIAN_POINT ( 'NONE',  ( -6.016104459813374383, -9.426230926598757165, 16.31603998697566738 ) ) ;
#57516 = VERTEX_POINT ( 'NONE', #23117 ) ;
#57517 = CIRCLE ( 'NONE', #25516, 42.08604991992415023 ) ;
#57518 = CARTESIAN_POINT ( 'NONE',  ( 0.8744876279028263033, 36.80052600666216023, 32.49725120702480297 ) ) ;
#57519 = CYLINDRICAL_SURFACE ( 'NONE', #34776, 15.99999999999999645 ) ;
#57520 = AXIS2_PLACEMENT_3D ( 'NONE', #14004, #33108, #19012 ) ;
#57521 = DIRECTION ( 'NONE',  ( 0.09835009131224564660, 0.5042575517176685063, -0.8579344853044291730 ) ) ;
#57522 = CARTESIAN_POINT ( 'NONE',  ( 0.9736507210033065185, 42.59776535855984037, -5.153758453069121614 ) ) ;
#57523 = CARTESIAN_POINT ( 'NONE',  ( 0.1155031312995260795, 9.982755425405617444, -42.98006778319857091 ) ) ;
#57524 = CIRCLE ( 'NONE', #30522, 12.50000000000000000 ) ;
#57525 =( BOUNDED_CURVE ( )  B_SPLINE_CURVE ( 3, ( #16, #34179, #18852, #24450 ),
 .UNSPECIFIED., .F., .F. ) 
 B_SPLINE_CURVE_WITH_KNOTS ( ( 4, 4 ),
 ( 0.000000000000000000, 3.141592653589793116 ),
 .UNSPECIFIED. ) 
 CURVE ( )  GEOMETRIC_REPRESENTATION_ITEM ( )  RATIONAL_B_SPLINE_CURVE ( ( 1.000000000000000000, 0.3333333333333333703, 0.3333333333333333703, 1.000000000000000000 ) ) 
 REPRESENTATION_ITEM ( '' )  );
#57526 = VERTEX_POINT ( 'NONE', #42245 ) ;
#57527 = CARTESIAN_POINT ( 'NONE',  ( 7.999999999999983125, 80.00000000000001421, -9.340760230278089508E-32 ) ) ;
#57528 = B_SPLINE_CURVE_WITH_KNOTS ( 'NONE', 3,
 ( #38456, #24027, #43156, #9302, #18413, #37532, #52835, #191, #56603, #8680, #57506, #18722, #28109, #14338, #52519, #27801, #47849, #37852 ),
 .UNSPECIFIED., .F., .F.,
 ( 4, 2, 2, 2, 2, 2, 2, 2, 4 ),
 ( 0.004151178236722271285, 0.004669824733854588579, 0.005188471230986906740, 0.005707117728119224034, 0.006225764225251541328, 0.006744410722383859490, 0.007263057219516176784, 0.007781703716648494945, 0.008300350213780812239 ),
 .UNSPECIFIED. ) ;
#57529 = CARTESIAN_POINT ( 'NONE',  ( -18.11307558806116802, -7.719455939378113030, 2.099999999999994760 ) ) ;
#57530 = CARTESIAN_POINT ( 'NONE',  ( -69.95594261585600293, 0.000000000000000000, 0.000000000000000000 ) ) ;
#57531 = ORIENTED_EDGE ( 'NONE', *, *, #9876, .F. ) ;
#57532 = CARTESIAN_POINT ( 'NONE',  ( 4.291220156522060236, 6.853930411217474372, 46.60914754877937582 ) ) ;
#57533 = CARTESIAN_POINT ( 'NONE',  ( 0.5806925824938502512, -25.69265091979982429, -39.23149310256842170 ) ) ;
#57534 = ORIENTED_EDGE ( 'NONE', *, *, #15386, .F. ) ;
#57535 = APPLICATION_CONTEXT ( 'automotive_design' ) ;
#57536 = DIRECTION ( 'NONE',  ( 1.000000000000000000, 0.000000000000000000, 0.000000000000000000 ) ) ;
#57537 = ADVANCED_FACE ( 'NONE', ( #47543 ), #17978, .F. ) ;
#57538 = VERTEX_POINT ( 'NONE', #49684 ) ;
#57539 = CARTESIAN_POINT ( 'NONE',  ( 53.13317509687642826, 15.49709605010121116, -0.3454668168334632528 ) ) ;
#57540 = CARTESIAN_POINT ( 'NONE',  ( 0.6001305935487315502, -46.60388846085714931, -11.94532529598361847 ) ) ;
#57541 = ORIENTED_EDGE ( 'NONE', *, *, #58603, .F. ) ;
#57542 = CARTESIAN_POINT ( 'NONE',  ( 0.8760168074887090262, 41.20610493656909767, -24.81951362746034917 ) ) ;
#57543 = CARTESIAN_POINT ( 'NONE',  ( 1.830465331921977246, 2.999073074481199086, 43.94748703364405884 ) ) ;
#57544 = ADVANCED_FACE ( 'NONE', ( #840 ), #2486, .T. ) ;
#57545 = CARTESIAN_POINT ( 'NONE',  ( 0.9772918015221170318, 40.52725854131377048, 10.67137155553071537 ) ) ;
#57546 = CARTESIAN_POINT ( 'NONE',  ( 4.956653778116982600, -47.27023054223759857, 8.845409907520762616 ) ) ;
#57547 = ORIENTED_EDGE ( 'NONE', *, *, #9504, .F. ) ;
#57548 = CARTESIAN_POINT ( 'NONE',  ( 0.5997462898726536595, -8.352924653000044941, -48.39194436975655123 ) ) ;
#57549 = VERTEX_POINT ( 'NONE', #29346 ) ;
#57550 = CARTESIAN_POINT ( 'NONE',  ( 0.3676999524040366896, -42.45338881270437525, 11.98584004733023534 ) ) ;
#57551 = AXIS2_PLACEMENT_3D ( 'NONE', #54779, #43968, #38952 ) ;
#57552 = ORIENTED_EDGE ( 'NONE', *, *, #52630, .T. ) ;
#57553 = ORIENTED_EDGE ( 'NONE', *, *, #32659, .T. ) ;
#57554 = CARTESIAN_POINT ( 'NONE',  ( 0.7764146366350254125, -46.85094009729996856, -2.242740660079716175 ) ) ;
#57555 = CARTESIAN_POINT ( 'NONE',  ( 0.6017666602106489515, -33.76944145963998523, 34.26316403931501497 ) ) ;
#57556 = VECTOR ( 'NONE', #29826, 1000.000000000000000 ) ;
#57557 = CARTESIAN_POINT ( 'NONE',  ( 5.895596859100789899, 10.82540956478682581, -16.95106754653256331 ) ) ;
#57558 = EDGE_LOOP ( 'NONE', ( #31027, #33041, #11758, #1402 ) ) ;
#57559 = CARTESIAN_POINT ( 'NONE',  ( 0.9736507210033064075, 0.4504567742786991236, -42.90603603725247694 ) ) ;
#57560 = CARTESIAN_POINT ( 'NONE',  ( 4.553261556744873317, 22.57774691820481294, -37.68003330573274923 ) ) ;
#57561 = EDGE_CURVE ( 'NONE', #35873, #9554, #48762, .T. ) ;
#57562 = CARTESIAN_POINT ( 'NONE',  ( 3.238018933889920792, 1.066824900591889724, 13.35175557741865404 ) ) ;
#57563 = CIRCLE ( 'NONE', #54523, 42.08604991992415023 ) ;
#57564 = ORIENTED_EDGE ( 'NONE', *, *, #46280, .F. ) ;
#57565 = B_SPLINE_CURVE_WITH_KNOTS ( 'NONE', 3,
 ( #29443, #51196, #27098, #60906, #3887, #42157 ),
 .UNSPECIFIED., .F., .F.,
 ( 4, 2, 4 ),
 ( 1.266794085606387986E-16, 0.0002450741128632359200, 0.0004901482257263450968 ),
 .UNSPECIFIED. ) ;
#57566 = ORIENTED_EDGE ( 'NONE', *, *, #32118, .F. ) ;
#57567 =( NAMED_UNIT ( * ) PLANE_ANGLE_UNIT ( ) SI_UNIT ( $, .RADIAN. ) );
#57568 = CARTESIAN_POINT ( 'NONE',  ( 0.5998501479064699549, 6.798102206413494386, 47.62484632993690781 ) ) ;
#57569 = LINE ( 'NONE', #572, #54937 ) ;
#57570 = DIRECTION ( 'NONE',  ( 1.000000000000000000, 0.000000000000000000, 0.000000000000000000 ) ) ;
#57571 = ORIENTED_EDGE ( 'NONE', *, *, #1626, .T. ) ;
#57572 = ORIENTED_EDGE ( 'NONE', *, *, #6258, .F. ) ;
#57573 = CARTESIAN_POINT ( 'NONE',  ( 0.6009452777970412107, 12.87217382175429137, 46.35353542372327951 ) ) ;
#57574 = CARTESIAN_POINT ( 'NONE',  ( 3.390910168358337362, 42.74744500291679827, -10.33213831964325813 ) ) ;
#57575 = DIRECTION ( 'NONE',  ( -1.000000000000000000, -0.000000000000000000, -0.000000000000000000 ) ) ;
#57576 = B_SPLINE_CURVE_WITH_KNOTS ( 'NONE', 3,
 ( #56458, #60851, #52069, #42697, #17967, #51443 ),
 .UNSPECIFIED., .F., .F.,
 ( 4, 2, 4 ),
 ( 1.550814302699561017E-16, 0.0002445252820015144735, 0.0004890505640028737977 ),
 .UNSPECIFIED. ) ;
#57577 = FACE_OUTER_BOUND ( 'NONE', #55086, .T. ) ;
#57578 = CARTESIAN_POINT ( 'NONE',  ( 0.8744876279028306332, -0.6840263623749832655, 49.09055060105833235 ) ) ;
#57579 = CARTESIAN_POINT ( 'NONE',  ( 2.528190830796657185, 21.22731424743293260, -36.21678155211667871 ) ) ;
#57580 = VERTEX_POINT ( 'NONE', #53742 ) ;
#57581 = CARTESIAN_POINT ( 'NONE',  ( 0.8557997880470599172, -23.15977007032294210, -41.93815086860281127 ) ) ;
#57582 = DIRECTION ( 'NONE',  ( 0.07500201931887537365, 0.9939633762263315742, 0.08007186658772948162 ) ) ;
#57583 = CARTESIAN_POINT ( 'NONE',  ( 0.6845945791218023269, -6.946890923034354515, 46.39124084584727115 ) ) ;
#57584 = FACE_OUTER_BOUND ( 'NONE', #23568, .T. ) ;
#57585 = DIRECTION ( 'NONE',  ( 0.1011922191286468292, 0.7491372366378290515, -0.6546400044837293875 ) ) ;
#57586 = EDGE_CURVE ( 'NONE', #45480, #37128, #11483, .T. ) ;
#57587 = CARTESIAN_POINT ( 'NONE',  ( 0.9762797500689124330, -34.26226594605947895, 24.13341909939818564 ) ) ;
#57588 = CARTESIAN_POINT ( 'NONE',  ( 5.959547316686252039, 20.52562247508876681, -0.003562808152693842153 ) ) ;
#57589 = ADVANCED_FACE ( 'NONE', ( #58753 ), #30384, .F. ) ;
#57590 = B_SPLINE_CURVE_WITH_KNOTS ( 'NONE', 3,
 ( #28428, #47557, #51929, #8708, #37875, #1076 ),
 .UNSPECIFIED., .F., .F.,
 ( 4, 2, 4 ),
 ( 0.000000000000000000, 0.0002291966416970791056, 0.0004583932833941582112 ),
 .UNSPECIFIED. ) ;
#57591 = ORIENTED_EDGE ( 'NONE', *, *, #47959, .T. ) ;
#57592 = EDGE_CURVE ( 'NONE', #18665, #13574, #22336, .T. ) ;
#57593 = DIRECTION ( 'NONE',  ( 1.000000000000000000, 0.000000000000000000, 0.000000000000000000 ) ) ;
#57594 =( BOUNDED_SURFACE ( )  B_SPLINE_SURFACE ( 3, 1, ( 
 ( #26061, #31074 ),
 ( #50178, #6928 ),
 ( #2856, #55788 ),
 ( #55476, #26991 ) ),
 .UNSPECIFIED., .F., .F., .F. ) 
 B_SPLINE_SURFACE_WITH_KNOTS ( ( 4, 4 ),
 ( 2, 2 ),
 ( 0.000000000000000000, 1.000000000000000000 ),
 ( 0.000000000000000000, 1.000000000000000000 ),
 .UNSPECIFIED. ) 
 GEOMETRIC_REPRESENTATION_ITEM ( )  RATIONAL_B_SPLINE_SURFACE ( (
 ( 1.000000000000000000, 1.000000000000000000),
 ( 0.7211978278499968642, 0.9934217856018975334),
 ( 0.7211978278499968642, 0.9934217856018975334),
 ( 1.000000000000000000, 1.000000000000000000) ) ) 
 REPRESENTATION_ITEM ( '' )  SURFACE ( )  );
#57595 = CARTESIAN_POINT ( 'NONE',  ( 3.240649175237395596, -40.05536204209594331, -18.18881219525537318 ) ) ;
#57596 = VECTOR ( 'NONE', #20001, 1000.000000000000000 ) ;
#57597 = CARTESIAN_POINT ( 'NONE',  ( 0.6008123274975391004, -47.38919646901772609, -12.87705747363489373 ) ) ;
#57598 = CARTESIAN_POINT ( 'NONE',  ( -4.000000000000000000, 0.3904826640788011116, -3.430483436379915141E-17 ) ) ;
#57599 = DIRECTION ( 'NONE',  ( -1.000000000000000000, -0.000000000000000000, -0.000000000000000000 ) ) ;
#57600 = EDGE_LOOP ( 'NONE', ( #41568, #6172, #38276, #47623 ) ) ;
#57601 = CARTESIAN_POINT ( 'NONE',  ( 4.956653778116975495, -2.599733001514665798, 48.02038484091099235 ) ) ;
#57602 = VECTOR ( 'NONE', #30960, 1000.000000000000227 ) ;
#57603 = CARTESIAN_POINT ( 'NONE',  ( 0.3676999524040366896, 43.13409918076302318, -9.241215893319285613 ) ) ;
#57604 = CARTESIAN_POINT ( 'NONE',  ( 4.963659409799330291, 9.199077662858906379, 43.79875484948450293 ) ) ;
#57605 = VERTEX_POINT ( 'NONE', #2053 ) ;
#57606 = CARTESIAN_POINT ( 'NONE',  ( 0.5998501479064708430, -44.64337787626261189, 17.92509395669028649 ) ) ;
#57607 = CARTESIAN_POINT ( 'NONE',  ( 4.956445790443988031, 0.000000000000000000, 0.000000000000000000 ) ) ;
#57608 = ADVANCED_FACE ( 'NONE', ( #48451, #11178, #34999, #24656, #5519, #39089, #58143, #44707, #1747, #15268 ), #53447, .F. ) ;
#57609 = ORIENTED_EDGE ( 'NONE', *, *, #6379, .F. ) ;
#57610 = CIRCLE ( 'NONE', #39647, 43.08621763946400307 ) ;
#57611 = CARTESIAN_POINT ( 'NONE',  ( 0.8753041380234530822, 16.12068986424834804, -46.38169559399161557 ) ) ;
#57612 = B_SPLINE_CURVE_WITH_KNOTS ( 'NONE', 3,
 ( #12151, #31231, #50330, #7400, #47500, #52178 ),
 .UNSPECIFIED., .F., .F.,
 ( 4, 2, 4 ),
 ( 1.823789517034659149E-17, 0.0002293319059085092764, 0.0004586638118170002841 ),
 .UNSPECIFIED. ) ;
#57613 = VERTEX_POINT ( 'NONE', #1139 ) ;
#57614 = CARTESIAN_POINT ( 'NONE',  ( 4.962356264823602814, 42.01891079680549979, 2.376285612557970772 ) ) ;
#57616 = ORIENTED_EDGE ( 'NONE', *, *, #54278, .T. ) ;
#57615 = ADVANCED_FACE ( 'NONE', ( #6428 ), #28382, .F. ) ;
#57617 = DIRECTION ( 'NONE',  ( -0.07906939808003035641, 0.09174470402934598035, -0.9926383730089368695 ) ) ;
#57618 = CARTESIAN_POINT ( 'NONE',  ( 0.3622758884714730732, 40.13994584881760375, 15.73321244754868964 ) ) ;
#57619 = ORIENTED_EDGE ( 'NONE', *, *, #56931, .T. ) ;
#57621 = CARTESIAN_POINT ( 'NONE',  ( 5.895881250540457863, 8.470336106974158952, -18.24228844863469234 ) ) ;
#57620 = B_SPLINE_CURVE_WITH_KNOTS ( 'NONE', 3,
 ( #16408, #58996, #35530, #16107 ),
 .UNSPECIFIED., .F., .F.,
 ( 4, 4 ),
 ( 5.553824967135426632E-18, 0.004042984057420970223 ),
 .UNSPECIFIED. ) ;
#57622 = VERTEX_POINT ( 'NONE', #6128 ) ;
#57623 = LINE ( 'NONE', #19450, #35786 ) ;
#57624 = EDGE_CURVE ( 'NONE', #23099, #39332, #11140, .T. ) ;
#57625 = CARTESIAN_POINT ( 'NONE',  ( 0.5837799406558225046, 40.39581629257541806, 23.82061241097095206 ) ) ;
#57626 = VERTEX_POINT ( 'NONE', #44409 ) ;
#57627 = B_SPLINE_CURVE_WITH_KNOTS ( 'NONE', 3,
 ( #24257, #53364, #19577, #38693 ),
 .UNSPECIFIED., .F., .F.,
 ( 4, 4 ),
 ( 1.192622389734054877E-18, 0.004444878191957691259 ),
 .UNSPECIFIED. ) ;
#57628 = CARTESIAN_POINT ( 'NONE',  ( -2.569797478183783568, 11.87678401312183141, 8.547745408040835713 ) ) ;
#57629 = ORIENTED_EDGE ( 'NONE', *, *, #1334, .T. ) ;
#57630 = CARTESIAN_POINT ( 'NONE',  ( 0.6041374136657475802, -23.90252055111294283, -41.74951251761564919 ) ) ;
#57631 = EDGE_CURVE ( 'NONE', #33472, #2188, #27419, .T. ) ;
#57632 = CARTESIAN_POINT ( 'NONE',  ( 1.088908134280555773, -10.35121946298442097, 41.64642044161487888 ) ) ;
#57633 = ORIENTED_EDGE ( 'NONE', *, *, #42468, .F. ) ;
#57634 = CARTESIAN_POINT ( 'NONE',  ( 0.8557997880470697982, 47.60865952216998664, 5.347802024197403803 ) ) ;
#57635 = ORIENTED_EDGE ( 'NONE', *, *, #20661, .F. ) ;
#57636 = CARTESIAN_POINT ( 'NONE',  ( 1.231276596079887264, 29.74482033789320568, 29.53849072116790353 ) ) ;
#57637 = CARTESIAN_POINT ( 'NONE',  ( 4.999999999999986677, 56.56854249492371878, 56.56854249492391062 ) ) ;
#57638 = ORIENTED_EDGE ( 'NONE', *, *, #60237, .F. ) ;
#57639 = CARTESIAN_POINT ( 'NONE',  ( 0.9772918015221174759, -34.78437337412577079, -23.37486309521597150 ) ) ;
#57640 = CARTESIAN_POINT ( 'NONE',  ( 0.1157506346131639274, 25.16801674065300531, -36.24240048817191706 ) ) ;
#57641 = CARTESIAN_POINT ( 'NONE',  ( -6.017396004339687465, -18.68180398134248676, -2.460690056887981925 ) ) ;
#57642 = CARTESIAN_POINT ( 'NONE',  ( 50.50000000000024869, 5.000000000000018652, -7.703719777548943412E-31 ) ) ;
#57643 = VECTOR ( 'NONE', #29315, 999.9999999999998863 ) ;
#57644 = AXIS2_PLACEMENT_3D ( 'NONE', #34957, #30228, #25844 ) ;
#57645 = VERTEX_POINT ( 'NONE', #2989 ) ;
#57646 = CARTESIAN_POINT ( 'NONE',  ( 2.618530812446111078, -0.1622799276207554930, -47.00745105218204856 ) ) ;
#57647 = CIRCLE ( 'NONE', #3638, 6.887500000000022382 ) ;
#57648 = CARTESIAN_POINT ( 'NONE',  ( 4.956445790443998689, -11.44166143952028314, 45.67960632101629415 ) ) ;
#57649 = CARTESIAN_POINT ( 'NONE',  ( -6.015611763856276717, -18.84324252354755203, 0.006214430185075541652 ) ) ;
#57650 = CARTESIAN_POINT ( 'NONE',  ( 2.299652685299199195, 41.78300659542229312, -25.66051606466733759 ) ) ;
#57651 = FACE_OUTER_BOUND ( 'NONE', #51768, .T. ) ;
#57652 = CARTESIAN_POINT ( 'NONE',  ( 3.238741278300274473, 7.419593128524060610, -42.34697043723804200 ) ) ;
#57653 = VECTOR ( 'NONE', #20648, 999.9999999999998863 ) ;
#57654 = DIRECTION ( 'NONE',  ( -0.9990097760809875105, 5.448601141172011466E-18, -0.04449120468828677427 ) ) ;
#57655 = EDGE_CURVE ( 'NONE', #58260, #19313, #51488, .T. ) ;
#57656 = CARTESIAN_POINT ( 'NONE',  ( 0.7762777257811881437, 38.54028505510758151, -28.45155622761391356 ) ) ;
#57657 = CARTESIAN_POINT ( 'NONE',  ( 4.956653778116966613, 0.000000000000000000, 0.000000000000000000 ) ) ;
#57658 = EDGE_CURVE ( 'NONE', #56645, #33616, #43533, .T. ) ;
#57659 = CARTESIAN_POINT ( 'NONE',  ( 0.1365634738349373045, 34.00677838472008574, -28.11408265470851475 ) ) ;
#57660 = CARTESIAN_POINT ( 'NONE',  ( 4.967162193818130511, -40.93989340068600313, -13.42934394584206359 ) ) ;
#57661 = DIRECTION ( 'NONE',  ( -1.000000000000000000, -0.000000000000000000, -0.000000000000000000 ) ) ;
#57662 = CARTESIAN_POINT ( 'NONE',  ( 0.7762783648524379521, 44.59086139387540015, 17.50713302551343986 ) ) ;
#57664 = EDGE_CURVE ( 'NONE', #55047, #15365, #41862, .T. ) ;
#57663 = CARTESIAN_POINT ( 'NONE',  ( 0.9787284016396619046, 9.897315075569602882, 40.72320165733204789 ) ) ;
#57665 = ADVANCED_FACE ( 'NONE', ( #35616 ), #3130, .F. ) ;
#57666 = CARTESIAN_POINT ( 'NONE',  ( 1.227938101723756947, -4.762198645644731165, 42.65467462194916948 ) ) ;
#57667 = CARTESIAN_POINT ( 'NONE',  ( 0.6000166863083106206, -48.63754814943186489, 6.797969676318823318 ) ) ;
#57668 = EDGE_CURVE ( 'NONE', #8537, #18131, #3595, .T. ) ;
#57669 = ORIENTED_EDGE ( 'NONE', *, *, #23698, .T. ) ;
#57670 = DIRECTION ( 'NONE',  ( -1.000000000000000000, -1.836970198721027715E-16, 2.218671295934095703E-31 ) ) ;
#57671 = CARTESIAN_POINT ( 'NONE',  ( 4.390527457369401532, 18.07658334720816384, -40.04275803588028992 ) ) ;
#57672 = CARTESIAN_POINT ( 'NONE',  ( 5.895596859100789899, -20.11288567981415909, 0.003583743010676893742 ) ) ;
#57673 = VERTEX_POINT ( 'NONE', #27119 ) ;
#57674 = CARTESIAN_POINT ( 'NONE',  ( 1.830465331921977912, -21.77017147165016198, -38.29406860041564187 ) ) ;
#57675 = CARTESIAN_POINT ( 'NONE',  ( 3.390910168358336474, 26.75129140044841947, 34.90652582171320972 ) ) ;
#57676 = ORIENTED_EDGE ( 'NONE', *, *, #57832, .F. ) ;
#57677 = EDGE_LOOP ( 'NONE', ( #1252, #28698, #34001, #43551 ) ) ;
#57678 = CARTESIAN_POINT ( 'NONE',  ( 0.8551540677456715978, -38.56334384152451378, 28.44084013485104023 ) ) ;
#57679 = VECTOR ( 'NONE', #9340, 1000.000000000000000 ) ;
#57680 = EDGE_CURVE ( 'NONE', #26613, #55183, #35779, .T. ) ;
#57681 = ORIENTED_EDGE ( 'NONE', *, *, #57190, .T. ) ;
#57682 = PRESENTATION_LAYER_ASSIGNMENT (  '', '', ( #21724 ) ) ;
#57683 = CARTESIAN_POINT ( 'NONE',  ( 4.956445790444041322, 46.25174887658561573, -8.849507104743011610 ) ) ;
#57684 = B_SPLINE_CURVE_WITH_KNOTS ( 'NONE', 3,
 ( #35135, #21025, #30402, #974 ),
 .UNSPECIFIED., .F., .F.,
 ( 4, 4 ),
 ( 0.000000000000000000, 0.005004741218457420607 ),
 .UNSPECIFIED. ) ;
#57685 = VECTOR ( 'NONE', #45153, 1000.000000000000114 ) ;
#57686 = ORIENTED_EDGE ( 'NONE', *, *, #21081, .T. ) ;
#57687 = ORIENTED_EDGE ( 'NONE', *, *, #12532, .F. ) ;
#57688 = FACE_OUTER_BOUND ( 'NONE', #41743, .T. ) ;
#57689 = ORIENTED_EDGE ( 'NONE', *, *, #22325, .T. ) ;
#57690 = FACE_OUTER_BOUND ( 'NONE', #16044, .T. ) ;
#57691 = CARTESIAN_POINT ( 'NONE',  ( 0.8751705887134423323, 47.79200036674280483, -5.393078191592203474 ) ) ;
#57692 = B_SPLINE_CURVE_WITH_KNOTS ( 'NONE', 3,
 ( #49145, #6198, #44482, #24175, #57358, #14490, #58837, #348, #19495, #38612, #27195, #12496, #50989, #45703, #26890, #45398 ),
 .UNSPECIFIED., .F., .F.,
 ( 4, 3, 3, 3, 3, 4 ),
 ( 1.551621725782133898E-17, 0.0002724568934985618896, 0.0004086836638483852969, 0.0005449104342063618503, 0.0008173270854453600597, 0.001089761613562687491 ),
 .UNSPECIFIED. ) ;
#57693 = CARTESIAN_POINT ( 'NONE',  ( 0.1129192098497447394, 9.345467776859020859, -43.12324222292247811 ) ) ;
#57694 = EDGE_LOOP ( 'NONE', ( #55146, #27047, #30694, #16038 ) ) ;
#57695 = CARTESIAN_POINT ( 'NONE',  ( 4.963659409799328515, 43.79875484948446740, 9.199077662859053817 ) ) ;
#57696 = EDGE_CURVE ( 'NONE', #30901, #29160, #3286, .T. ) ;
#57697 =( BOUNDED_SURFACE ( )  B_SPLINE_SURFACE ( 3, 1, ( 
 ( #16039, #45482 ),
 ( #2535, #50165 ),
 ( #35150, #30419 ),
 ( #40180, #59547 ) ),
 .UNSPECIFIED., .F., .F., .F. ) 
 B_SPLINE_SURFACE_WITH_KNOTS ( ( 4, 4 ),
 ( 2, 2 ),
 ( 0.000000000000000000, 1.000000000000000000 ),
 ( 0.000000000000000000, 1.000000000000000000 ),
 .UNSPECIFIED. ) 
 GEOMETRIC_REPRESENTATION_ITEM ( )  RATIONAL_B_SPLINE_SURFACE ( (
 ( 1.000000000000000000, 1.000000000000000000),
 ( 0.7269869731126821222, 0.9931720237060910339),
 ( 0.7269869731126821222, 0.9931720237060910339),
 ( 1.000000000000000000, 1.000000000000000000) ) ) 
 REPRESENTATION_ITEM ( '' )  SURFACE ( )  );
#57698 = CARTESIAN_POINT ( 'NONE',  ( 100.0000507999999968, 9.797174393178825657E-16, -8.000000000000000000 ) ) ;
#57699 = ORIENTED_EDGE ( 'NONE', *, *, #59711, .F. ) ;
#57700 = ORIENTED_EDGE ( 'NONE', *, *, #11796, .F. ) ;
#57701 = CARTESIAN_POINT ( 'NONE',  ( 0.7048096507298579061, -38.67623024744067095, 28.61383451045632853 ) ) ;
#57702 = ORIENTED_EDGE ( 'NONE', *, *, #52308, .T. ) ;
#57703 = CARTESIAN_POINT ( 'NONE',  ( -6.001507490154110336, 17.40350523682705486, -7.225628667346390976 ) ) ;
#57704 = CARTESIAN_POINT ( 'NONE',  ( 0.9730545539215883499, -30.69604515769671949, 29.98130006528850444 ) ) ;
#57705 = CARTESIAN_POINT ( 'NONE',  ( 0.9757787079277449038, -0.03949005143931162004, 42.90844198810271592 ) ) ;
#57706 = CARTESIAN_POINT ( 'NONE',  ( 0.8557997880470690211, 5.347802024197924275, -47.60865952216993691 ) ) ;
#57707 = ADVANCED_FACE ( 'NONE', ( #26810 ), #6439, .T. ) ;
#57708 = ORIENTED_EDGE ( 'NONE', *, *, #9476, .T. ) ;
#57709 = DIRECTION ( 'NONE',  ( 0.000000000000000000, 0.000000000000000000, -1.000000000000000000 ) ) ;
#57710 = CARTESIAN_POINT ( 'NONE',  ( 1.091591847532195514, 41.42852926003946124, 6.358927134815586690 ) ) ;
#57711 = ADVANCED_FACE ( 'NONE', ( #36228 ), #36829, .F. ) ;
#57712 = CARTESIAN_POINT ( 'NONE',  ( 43.00000000000000000, 9.184850993605150311E-15, -75.00000000000001421 ) ) ;
#57713 = B_SPLINE_CURVE_WITH_KNOTS ( 'NONE', 3,
 ( #23638, #42765, #61822, #18959 ),
 .UNSPECIFIED., .F., .F.,
 ( 4, 4 ),
 ( 2.101926620404615003E-17, 0.004559932413162187670 ),
 .UNSPECIFIED. ) ;
#57714 = CARTESIAN_POINT ( 'NONE',  ( 4.553261556744875094, -9.994631851593741345, 42.77437199977043036 ) ) ;
#57715 = ORIENTED_EDGE ( 'NONE', *, *, #45294, .T. ) ;
#57716 = CARTESIAN_POINT ( 'NONE',  ( 3.782542959838397056, -8.686934394837271256, 41.13119283726600628 ) ) ;
#57717 = CARTESIAN_POINT ( 'NONE',  ( 0.1155031312995260795, 37.07158905255104031, -23.92987500281993363 ) ) ;
#57718 = DIRECTION ( 'NONE',  ( 0.9990097760809871774, 5.448601141172922046E-18, 0.04449120468829421277 ) ) ;
#57719 = CARTESIAN_POINT ( 'NONE',  ( 0.6021448801613057400, -35.09405629939740123, -34.35037628733741144 ) ) ;
#57720 = CIRCLE ( 'NONE', #54867, 48.09070567114147110 ) ;
#57721 = EDGE_LOOP ( 'NONE', ( #17008, #33778, #56164, #2393 ) ) ;
#57722 = ORIENTED_EDGE ( 'NONE', *, *, #32341, .T. ) ;
#57723 = DIRECTION ( 'NONE',  ( 0.1011922191286468292, -0.1714634860903167801, -0.9799797996517967125 ) ) ;
#57724 = CARTESIAN_POINT ( 'NONE',  ( 0.8557997880470599172, 13.27832040216703469, -46.03118133706011861 ) ) ;
#57725 = CARTESIAN_POINT ( 'NONE',  ( 6.000000000000000888, -15.71999999999998820, 1.942289823447701485E-15 ) ) ;
#57726 = CARTESIAN_POINT ( 'NONE',  ( 0.5782707292762423457, 27.23478191391718894, -38.18380557001864872 ) ) ;
#57727 = CARTESIAN_POINT ( 'NONE',  ( 4.549368137175248350, 38.40568845698250300, 19.17571786012337753 ) ) ;
#57728 = CARTESIAN_POINT ( 'NONE',  ( 0.9762797500689124330, 41.46413394121034912, 6.086902470967687329 ) ) ;
#57729 = CARTESIAN_POINT ( 'NONE',  ( 3.680882792899937694, -30.65151321162973730, -36.90742604464114152 ) ) ;
#57730 = CARTESIAN_POINT ( 'NONE',  ( 0.9762797500689124330, -1.905951756780688733, 41.86516610604248712 ) ) ;
#57731 = CARTESIAN_POINT ( 'NONE',  ( -48.95476116535499500, 0.000000000000000000, -12.50000000000000000 ) ) ;
#57732 = VECTOR ( 'NONE', #52480, 1000.000000000000114 ) ;
#57733 = CARTESIAN_POINT ( 'NONE',  ( 0.6023143664670691511, -18.16777128831361665, -44.54505257464852264 ) ) ;
#57734 = CARTESIAN_POINT ( 'NONE',  ( -2.739355103387247858, 13.56174707817311642, -6.239117176226129047 ) ) ;
#57735 = EDGE_LOOP ( 'NONE', ( #37767, #38400, #35115, #4846 ) ) ;
#57736 = CONICAL_SURFACE ( 'NONE', #29722, 42.08604991992415023, 1.569615340895231137 ) ;
#57737 = B_SPLINE_CURVE_WITH_KNOTS ( 'NONE', 3,
 ( #30439, #6606, #1935, #21060 ),
 .UNSPECIFIED., .F., .F.,
 ( 4, 4 ),
 ( 4.336808689942017736E-19, 0.004048833967417083887 ),
 .UNSPECIFIED. ) ;
#57738 = VECTOR ( 'NONE', #59565, 1000.000000000000000 ) ;
#57739 = CARTESIAN_POINT ( 'NONE',  ( 0.9972139404380291339, -42.45145681504344282, 6.252633471303223445 ) ) ;
#57740 = CARTESIAN_POINT ( 'NONE',  ( 0.1092355843206037486, -34.02913268098572530, -26.49036028133769705 ) ) ;
#57741 = EDGE_CURVE ( 'NONE', #55162, #35188, #21487, .T. ) ;
#57742 = CARTESIAN_POINT ( 'NONE',  ( 5.959547316686252039, -12.49803383497762255, 16.28190225198596863 ) ) ;
#57743 = CARTESIAN_POINT ( 'NONE',  ( 3.238018933889920792, -10.88486934301749365, 7.805582089318572336 ) ) ;
#57744 = CARTESIAN_POINT ( 'NONE',  ( -2.739355103387247858, -13.13414140434199950, 7.095202359465602626 ) ) ;
#57745 = CARTESIAN_POINT ( 'NONE',  ( 0.6031357023905874470, -46.47951061918818993, 12.40899271757757916 ) ) ;
#57746 = CYLINDRICAL_SURFACE ( 'NONE', #45683, 75.00000000000001421 ) ;
#57747 = ITEM_DEFINED_TRANSFORMATION ( 'NONE', 'NONE', #14928,  #14677 ) ;
#57749 = EDGE_CURVE ( 'NONE', #50058, #35234, #33491, .T. ) ;
#57748 = CARTESIAN_POINT ( 'NONE',  ( 0.9754402186311947887, -25.97197377940579699, 34.15542855230926733 ) ) ;
#57750 = CARTESIAN_POINT ( 'NONE',  ( 0.6008123274975392114, 48.28333653898867794, -8.959573863818473427 ) ) ;
#57751 = EDGE_CURVE ( 'NONE', #9105, #16525, #39488, .T. ) ;
#57752 = CARTESIAN_POINT ( 'NONE',  ( 0.6029443199889047422, -1.573994357226665697, -49.08217786139712047 ) ) ;
#57753 = FACE_OUTER_BOUND ( 'NONE', #51311, .T. ) ;
#57754 = EDGE_CURVE ( 'NONE', #13149, #30244, #14078, .T. ) ;
#57755 = ORIENTED_EDGE ( 'NONE', *, *, #39106, .T. ) ;
#57756 = VERTEX_POINT ( 'NONE', #28969 ) ;
#57757 = CARTESIAN_POINT ( 'NONE',  ( 0.3622758884714600280, -37.74294673546600620, 20.83792692158906235 ) ) ;
#57758 = CARTESIAN_POINT ( 'NONE',  ( 5.896278296736517710, -13.98624301437829232, 14.45378794493464802 ) ) ;
#57759 = EDGE_CURVE ( 'NONE', #33684, #41967, #23048, .T. ) ;
#57760 = CARTESIAN_POINT ( 'NONE',  ( 1.092182651088180689, -34.10752689525531167, 24.36057867809628164 ) ) ;
#57761 = VERTEX_POINT ( 'NONE', #33687 ) ;
#57762 = CARTESIAN_POINT ( 'NONE',  ( 0.8744876279028263033, 32.34273794994744833, 36.93639603806145288 ) ) ;
#57763 = CARTESIAN_POINT ( 'NONE',  ( 0.1073791018717578927, -30.14884492832369745, -30.83464511437127697 ) ) ;
#57764 = CARTESIAN_POINT ( 'NONE',  ( 0.8551540677456739292, -17.49081417858754506, -44.61036085020969466 ) ) ;
#57765 = CONICAL_SURFACE ( 'NONE', #3746, 42.08604991992415023, 1.569615340895231137 ) ;
#57766 = ORIENTED_EDGE ( 'NONE', *, *, #7137, .T. ) ;
#57767 = ORIENTED_EDGE ( 'NONE', *, *, #51678, .T. ) ;
#57768 = EDGE_CURVE ( 'NONE', #4686, #26055, #16342, .T. ) ;
#57769 = DIRECTION ( 'NONE',  ( 0.09835009131224552170, -0.6119264800004727833, -0.7847759187265520575 ) ) ;
#57770 = CARTESIAN_POINT ( 'NONE',  ( 0.3676999524040366896, 21.13209774130265473, 38.72189339863005841 ) ) ;
#57771 = B_SPLINE_CURVE_WITH_KNOTS ( 'NONE', 3,
 ( #31866, #60644, #50951, #60965, #56262, #8972 ),
 .UNSPECIFIED., .F., .F.,
 ( 4, 2, 4 ),
 ( 0.006456566858647416578, 0.007625406818786683791, 0.008794246778925951871 ),
 .UNSPECIFIED. ) ;
#57772 = CARTESIAN_POINT ( 'NONE',  ( 1.088313998177379283, -39.34193117255244942, -17.14007796983277387 ) ) ;
#57773 = CARTESIAN_POINT ( 'NONE',  ( 0.5837800005270532555, 46.89600471938711479, -3.178933284798639286E-05 ) ) ;
#57774 = CARTESIAN_POINT ( 'NONE',  ( 0.8554163680231720024, 5.604726001788835177, 46.58103175710786559 ) ) ;
#57775 = CARTESIAN_POINT ( 'NONE',  ( 5.896782393890504181, 18.99788783847860074, -6.603510017755636063 ) ) ;
#57776 = CARTESIAN_POINT ( 'NONE',  ( 0.5827359174754813687, 38.21848266111710757, -28.86822142608413344 ) ) ;
#57777 = EDGE_LOOP ( 'NONE', ( #56040, #11058 ) ) ;
#57778 =( BOUNDED_SURFACE ( )  B_SPLINE_SURFACE ( 3, 1, ( 
 ( #3683, #61016 ),
 ( #50688, #22817 ),
 ( #46037, #41950 ),
 ( #56313, #31291 ) ),
 .UNSPECIFIED., .F., .F., .F. ) 
 B_SPLINE_SURFACE_WITH_KNOTS ( ( 4, 4 ),
 ( 2, 2 ),
 ( 0.000000000000000000, 1.000000000000000000 ),
 ( 0.000000000000000000, 1.000000000000000000 ),
 .UNSPECIFIED. ) 
 GEOMETRIC_REPRESENTATION_ITEM ( )  RATIONAL_B_SPLINE_SURFACE ( (
 ( 1.000000000000000000, 1.000000000000000000),
 ( 0.7282232189291693025, 0.9929344683865674037),
 ( 0.7282232189291693025, 0.9929344683865674037),
 ( 1.000000000000000000, 1.000000000000000000) ) ) 
 REPRESENTATION_ITEM ( '' )  SURFACE ( )  );
#57779 = ORIENTED_EDGE ( 'NONE', *, *, #8512, .F. ) ;
#57780 = CARTESIAN_POINT ( 'NONE',  ( 8.000000000000007105, -56.56854249492410958, 56.56854249492351983 ) ) ;
#57781 = CARTESIAN_POINT ( 'NONE',  ( 3.661921753702005677, -45.01795958545552878, -13.63871103133745777 ) ) ;
#57782 = VECTOR ( 'NONE', #18628, 1000.000000000000114 ) ;
#57783 = VERTEX_POINT ( 'NONE', #8937 ) ;
#57784 = CARTESIAN_POINT ( 'NONE',  ( 0.1155031312995260795, 41.92908014207336720, -13.74386666740468854 ) ) ;
#57785 = CARTESIAN_POINT ( 'NONE',  ( 0.1313383488274140198, 37.66088038379816538, 21.00709374781555283 ) ) ;
#57786 = CARTESIAN_POINT ( 'NONE',  ( 0.7048096507298579061, -23.32077812596851629, -42.08020459959973181 ) ) ;
#57787 = CARTESIAN_POINT ( 'NONE',  ( -4.000000000000000000, 2.309401076758531346, -5.242734410091827613 ) ) ;
#57788 = ORIENTED_EDGE ( 'NONE', *, *, #61535, .T. ) ;
#57789 = EDGE_LOOP ( 'NONE', ( #16938, #13568, #34556, #12501 ) ) ;
#57790 = CARTESIAN_POINT ( 'NONE',  ( 0.5824936645240086364, -14.24161832706174202, 44.68125430722158598 ) ) ;
#57791 = CARTESIAN_POINT ( 'NONE',  ( 4.975610109902397937, 7.237810502494091303, 48.37420290059321104 ) ) ;
#57792 = CARTESIAN_POINT ( 'NONE',  ( 0.1087620492084206830, -37.16461718700651318, -21.87505161834403822 ) ) ;
#57793 = B_SPLINE_CURVE_WITH_KNOTS ( 'NONE', 3,
 ( #58308, #11665, #48942, #49244, #11350, #25752 ),
 .UNSPECIFIED., .F., .F.,
 ( 4, 2, 4 ),
 ( 3.686287386450715076E-18, 0.0002447193893791697623, 0.0004894387787583358383 ),
 .UNSPECIFIED. ) ;
#57794 = EDGE_CURVE ( 'NONE', #53765, #23158, #36484, .T. ) ;
#57795 = CARTESIAN_POINT ( 'NONE',  ( 5.896782393890504181, -11.92541098582135994, 16.19600752337635541 ) ) ;
#57796 = EDGE_LOOP ( 'NONE', ( #16625, #4549, #44631, #38948 ) ) ;
#57797 = CARTESIAN_POINT ( 'NONE',  ( 4.967162193818129623, 32.68434214048168940, 28.07411493385305334 ) ) ;
#57798 = ORIENTED_EDGE ( 'NONE', *, *, #774, .F. ) ;
#57799 = CARTESIAN_POINT ( 'NONE',  ( -5.995132425357893702, -18.20425902871264512, -4.869002713216763034 ) ) ;
#57800 = CARTESIAN_POINT ( 'NONE',  ( 0.1135584504625008206, 9.396960478524508886, 43.11205383532893620 ) ) ;
#57801 = CONICAL_SURFACE ( 'NONE', #30801, 43.08621763946400307, 1.568696531533066763 ) ;
#57802 = ORIENTED_EDGE ( 'NONE', *, *, #53388, .F. ) ;
#57803 = CARTESIAN_POINT ( 'NONE',  ( 0.6041374136657476912, 12.28249295042045475, -46.51335992032606725 ) ) ;
#57804 = CARTESIAN_POINT ( 'NONE',  ( 0.6029303876144825880, -47.71279573267363361, 6.149480157545783143 ) ) ;
#57805 = LINE ( 'NONE', #52190, #31936 ) ;
#57806 = VECTOR ( 'NONE', #38224, 1000.000000000000000 ) ;
#57807 = CARTESIAN_POINT ( 'NONE',  ( 0.8560838555295158248, 28.55542365806940452, -37.21505896528851309 ) ) ;
#57808 = CARTESIAN_POINT ( 'NONE',  ( 3.661933894777874343, -37.68385588960657628, -28.15240967027540719 ) ) ;
#57809 = DIRECTION ( 'NONE',  ( -1.000000000000000000, -0.000000000000000000, -0.000000000000000000 ) ) ;
#57810 = CARTESIAN_POINT ( 'NONE',  ( 4.549368137175248350, 0.000000000000000000, 0.000000000000000000 ) ) ;
#57811 = CARTESIAN_POINT ( 'NONE',  ( 4.549368137175248350, -8.582197505784124658, -42.06008734272393212 ) ) ;
#57812 = ORIENTED_EDGE ( 'NONE', *, *, #43815, .F. ) ;
#57813 = CARTESIAN_POINT ( 'NONE',  ( 4.962356264823608143, 0.000000000000000000, 0.000000000000000000 ) ) ;
#57814 = VECTOR ( 'NONE', #44382, 1000.000000000000114 ) ;
#57815 = DIRECTION ( 'NONE',  ( 0.000000000000000000, 0.4999999999999990008, -0.8660254037844391517 ) ) ;
#57816 = CARTESIAN_POINT ( 'NONE',  ( 0.7764139734771250412, 3.807011500850922658, 46.74983566109357724 ) ) ;
#57817 = EDGE_LOOP ( 'NONE', ( #19294, #34939, #267, #33877 ) ) ;
#57818 = CARTESIAN_POINT ( 'NONE',  ( 3.238018933889920792, 12.84302458974305949, -3.803184422941917830 ) ) ;
#57819 = DIRECTION ( 'NONE',  ( 0.000000000000000000, 0.000000000000000000, 1.000000000000000000 ) ) ;
#57820 = ADVANCED_FACE ( 'NONE', ( #57441 ), #51978, .F. ) ;
#57821 = CARTESIAN_POINT ( 'NONE',  ( 0.8551540677456834771, -13.28067116677169679, -46.03951182599441694 ) ) ;
#57822 = CARTESIAN_POINT ( 'NONE',  ( 5.896782393890504181, 19.71107130340470448, 3.999969368646206558 ) ) ;
#57823 = CARTESIAN_POINT ( 'NONE',  ( 5.896278296736517710, -13.97836643676215296, 14.46140558085503081 ) ) ;
#57824 = CARTESIAN_POINT ( 'NONE',  ( 0.9722240750034597534, 41.29187379046135931, -11.66659272802813163 ) ) ;
#57825 = DIRECTION ( 'NONE',  ( 0.9848077530122076872, 0.09698383872753983670, 0.1440410519008966106 ) ) ;
#57827 = ADVANCED_FACE ( 'NONE', ( #47167 ), #9168, .F. ) ;
#57826 = FACE_OUTER_BOUND ( 'NONE', #11064, .T. ) ;
#57828 = CARTESIAN_POINT ( 'NONE',  ( 0.9772918015221170318, -6.561173980998255217, 41.39188147139184792 ) ) ;
#57829 = EDGE_CURVE ( 'NONE', #52266, #39018, #34263, .T. ) ;
#57830 = VECTOR ( 'NONE', #28678, 1000.000000000000114 ) ;
#57831 = CARTESIAN_POINT ( 'NONE',  ( 3.238018933889920792, 12.43622092696280390, -4.974726266180425682 ) ) ;
#57832 = EDGE_CURVE ( 'NONE', #28331, #59869, #5444, .T. ) ;
#57834 = VERTEX_POINT ( 'NONE', #25189 ) ;
#57833 = DIRECTION ( 'NONE',  ( 0.000000000000000000, 0.000000000000000000, 1.000000000000000000 ) ) ;
#57835 = ORIENTED_EDGE ( 'NONE', *, *, #17944, .F. ) ;
#57836 = CARTESIAN_POINT ( 'NONE',  ( 0.5839879882012697365, -12.39635945868993794, 46.26395995854833387 ) ) ;
#57837 = AXIS2_PLACEMENT_3D ( 'NONE', #3358, #50672, #36928 ) ;
#57838 = CARTESIAN_POINT ( 'NONE',  ( 5.965394784446460541, -10.27521535480999049, 17.76824826579336758 ) ) ;
#57839 = EDGE_CURVE ( 'NONE', #54854, #30625, #20065, .T. ) ;
#57840 = FACE_OUTER_BOUND ( 'NONE', #30116, .T. ) ;
#57841 = DIRECTION ( 'NONE',  ( -0.07439287786467652097, -0.9868880006907401192, 0.1432402660415187101 ) ) ;
#57842 = CARTESIAN_POINT ( 'NONE',  ( -1.500000000000001332, 0.000000000000000000, -5.453125000000000000 ) ) ;
#57843 = CARTESIAN_POINT ( 'NONE',  ( 0.5809828226811617480, -11.86925843957133786, -46.40184912890851621 ) ) ;
#57844 = VERTEX_POINT ( 'NONE', #6661 ) ;
#57845 = B_SPLINE_CURVE_WITH_KNOTS ( 'NONE', 3,
 ( #46852, #36520, #60594, #3580, #41845, #27404 ),
 .UNSPECIFIED., .F., .F.,
 ( 4, 2, 4 ),
 ( 1.233980214667468354E-16, 0.0002448718616795902774, 0.0004897437233590571726 ),
 .UNSPECIFIED. ) ;
#57846 = DIRECTION ( 'NONE',  ( -1.000000000000000000, -3.673819061467147552E-16, 1.925929944387234758E-32 ) ) ;
#57847 = ADVANCED_FACE ( 'NONE', ( #19584 ), #18513, .T. ) ;
#57848 = AXIS2_PLACEMENT_3D ( 'NONE', #26256, #12806, #31274 ) ;
#57849 = CARTESIAN_POINT ( 'NONE',  ( 0.2230388203127620650, -10.42432885623912320, 41.84042374003679043 ) ) ;
#57850 = CARTESIAN_POINT ( 'NONE',  ( 4.975610109902397937, 0.000000000000000000, 0.000000000000000000 ) ) ;
#57851 = ORIENTED_EDGE ( 'NONE', *, *, #19611, .F. ) ;
#57852 = ADVANCED_FACE ( 'NONE', ( #440 ), #37190, .F. ) ;
#57853 = CARTESIAN_POINT ( 'NONE',  ( 1.231276596079887264, -27.70544295162332560, -31.45926257674220494 ) ) ;
#57854 = CARTESIAN_POINT ( 'NONE',  ( 0.9730545539215883499, -21.01499094264575618, 37.40983423658466478 ) ) ;
#57855 = ORIENTED_EDGE ( 'NONE', *, *, #20975, .F. ) ;
#57856 = CARTESIAN_POINT ( 'NONE',  ( 0.6067375320500711933, -44.51755737952363745, 17.67235760802248024 ) ) ;
#57857 = ORIENTED_EDGE ( 'NONE', *, *, #46695, .F. ) ;
#57858 = CARTESIAN_POINT ( 'NONE',  ( -6.016489644550736315, -13.32727118274428513, -13.32104266208113152 ) ) ;
#57859 = DIRECTION ( 'NONE',  ( 0.000000000000000000, 0.000000000000000000, 1.000000000000000000 ) ) ;
#57860 = EDGE_LOOP ( 'NONE', ( #54234, #56094, #55815, #41648 ) ) ;
#57861 = CARTESIAN_POINT ( 'NONE',  ( 3.661933894777874343, -47.02171970420939573, 1.260571699832463421 ) ) ;
#57862 = CARTESIAN_POINT ( 'NONE',  ( 4.834790513006553603, -46.46485498443001916, 8.579428430861252508 ) ) ;
#57863 = CARTESIAN_POINT ( 'NONE',  ( 0.9787284016396609054, 40.46867782039604577, 10.89137798434224180 ) ) ;
#57864 = CARTESIAN_POINT ( 'NONE',  ( 0.5837374860065640547, -37.88763545422897039, 29.30115996485980645 ) ) ;
#57865 = ORIENTED_EDGE ( 'NONE', *, *, #33216, .T. ) ;
#57866 = FACE_OUTER_BOUND ( 'NONE', #17357, .T. ) ;
#57867 = ORIENTED_EDGE ( 'NONE', *, *, #21046, .T. ) ;
#57868 = CARTESIAN_POINT ( 'NONE',  ( 4.549368137175248350, -35.80950303116117794, 23.67244292351576718 ) ) ;
#57869 = ADVANCED_FACE ( 'NONE', ( #19901 ), #34920, .F. ) ;
#57870 = VERTEX_POINT ( 'NONE', #29886 ) ;
#57871 = ORIENTED_EDGE ( 'NONE', *, *, #39428, .F. ) ;
#57872 = CARTESIAN_POINT ( 'NONE',  ( 2.618530812446115519, -0.1622799276214294262, 47.00745105218204145 ) ) ;
#57873 = CARTESIAN_POINT ( 'NONE',  ( 0.9769922540276052558, 36.28140764446582978, -20.97596277700310807 ) ) ;
#57874 = AXIS2_PLACEMENT_3D ( 'NONE', #56152, #51758, #38015 ) ;
#57875 = AXIS2_PLACEMENT_3D ( 'NONE', #38362, #19246, #37753 ) ;
#57877 = DIRECTION ( 'NONE',  ( 0.09722883295013594329, 0.8933953294778640419, -0.4386243715416339728 ) ) ;
#57876 = B_SPLINE_CURVE_WITH_KNOTS ( 'NONE', 3,
 ( #61293, #37530, #12564, #50447, #36998, #32276 ),
 .UNSPECIFIED., .F., .F.,
 ( 4, 2, 4 ),
 ( 1.267602517345562747E-16, 0.0002450741128632351611, 0.0004901482257263435789 ),
 .UNSPECIFIED. ) ;
#57878 = EDGE_LOOP ( 'NONE', ( #43057, #31568, #39662, #58957 ) ) ;
#57879 = DIRECTION ( 'NONE',  ( -0.000000000000000000, -0.000000000000000000, -1.000000000000000000 ) ) ;
#57880 = CARTESIAN_POINT ( 'NONE',  ( -48.95476116535499500, 0.000000000000000000, 0.000000000000000000 ) ) ;
#57881 = CARTESIAN_POINT ( 'NONE',  ( 2.299652685299201860, -26.51150749201314838, 41.24829324177042622 ) ) ;
#57882 = ORIENTED_EDGE ( 'NONE', *, *, #56639, .F. ) ;
#57883 =( BOUNDED_SURFACE ( )  B_SPLINE_SURFACE ( 3, 1, ( 
 ( #40688, #46299 ),
 ( #3344, #45381 ),
 ( #13093, #22473 ),
 ( #2425, #51274 ) ),
 .UNSPECIFIED., .F., .F., .F. ) 
 B_SPLINE_SURFACE_WITH_KNOTS ( ( 4, 4 ),
 ( 2, 2 ),
 ( 0.000000000000000000, 1.000000000000000000 ),
 ( 0.000000000000000000, 1.000000000000000000 ),
 .UNSPECIFIED. ) 
 GEOMETRIC_REPRESENTATION_ITEM ( )  RATIONAL_B_SPLINE_SURFACE ( (
 ( 1.000000000000000000, 1.000000000000000000),
 ( 0.7269869731126817891, 0.9931720237060910339),
 ( 0.7269869731126817891, 0.9931720237060910339),
 ( 1.000000000000000000, 1.000000000000000000) ) ) 
 REPRESENTATION_ITEM ( '' )  SURFACE ( )  );
#57884 = VERTEX_POINT ( 'NONE', #10483 ) ;
#57885 = CARTESIAN_POINT ( 'NONE',  ( 0.5997462898726536595, 5.235280152387709940, -48.82769165002913070 ) ) ;
#57886 = LINE ( 'NONE', #24393, #18792 ) ;
#57887 = CARTESIAN_POINT ( 'NONE',  ( 0.8557997880470606944, -46.50333260518566902, 11.51622788066442027 ) ) ;
#57888 = DIRECTION ( 'NONE',  ( 0.000000000000000000, 0.000000000000000000, 1.000000000000000000 ) ) ;
#57889 = CARTESIAN_POINT ( 'NONE',  ( 0.9762797500689124330, 38.77779312671030709, 15.89363222827819300 ) ) ;
#57890 = ORIENTED_EDGE ( 'NONE', *, *, #57696, .F. ) ;
#57891 = DIRECTION ( 'NONE',  ( -1.000000000000000000, -0.000000000000000000, -0.000000000000000000 ) ) ;
#57892 = AXIS2_PLACEMENT_3D ( 'NONE', #19261, #38377, #57425 ) ;
#57893 = EDGE_LOOP ( 'NONE', ( #43634, #21675, #35982, #29606 ) ) ;
#57894 = CARTESIAN_POINT ( 'NONE',  ( 1.830465331921977468, -8.246493558563114945, 43.27090708393997431 ) ) ;
#57895 = CARTESIAN_POINT ( 'NONE',  ( 4.956445790443998689, 1.033212179477464909, 47.07940656732852602 ) ) ;
#57896 = DIRECTION ( 'NONE',  ( 0.09835009131224552170, 0.2650256080583628382, 0.9592125346408729714 ) ) ;
#57897 = CARTESIAN_POINT ( 'NONE',  ( 2.301529144917014769, 43.86846428170459689, -19.56451384728999088 ) ) ;
#57898 = CARTESIAN_POINT ( 'NONE',  ( 5.960721111146673579, 18.96073515164548340, -7.860635756377695849 ) ) ;
#57899 = AXIS2_PLACEMENT_3D ( 'NONE', #1426, #43787, #34364 ) ;
#57900 =( BOUNDED_SURFACE ( )  B_SPLINE_SURFACE ( 3, 1, ( 
 ( #24164, #34204 ),
 ( #4411, #658 ),
 ( #18551, #14787 ),
 ( #14177, #23548 ) ),
 .UNSPECIFIED., .F., .F., .F. ) 
 B_SPLINE_SURFACE_WITH_KNOTS ( ( 4, 4 ),
 ( 2, 2 ),
 ( 0.000000000000000000, 1.000000000000000000 ),
 ( 0.000000000000000000, 1.000000000000000000 ),
 .UNSPECIFIED. ) 
 GEOMETRIC_REPRESENTATION_ITEM ( )  RATIONAL_B_SPLINE_SURFACE ( (
 ( 1.000000000000000000, 1.000000000000000000),
 ( 0.9953040768229005630, 0.8617119497784937465),
 ( 0.9953040768229005630, 0.8617119497784937465),
 ( 1.000000000000000000, 1.000000000000000000) ) ) 
 REPRESENTATION_ITEM ( '' )  SURFACE ( )  );
#57901 = CARTESIAN_POINT ( 'NONE',  ( -6.016489644550736315, 2.455165042130005304, -18.68257207665193675 ) ) ;
#57902 = CARTESIAN_POINT ( 'NONE',  ( 0.8560838555295158248, -0.6537497281619772949, -46.90357604036880446 ) ) ;
#57903 = EDGE_CURVE ( 'NONE', #1293, #29313, #8131, .T. ) ;
#57904 = CARTESIAN_POINT ( 'NONE',  ( 0.5987334363312689645, -47.65150816038625692, 11.86999058604166279 ) ) ;
#57905 = CARTESIAN_POINT ( 'NONE',  ( 0.1129192098497447394, -1.898585089631814826, -44.08341142019957459 ) ) ;
#57906 = CARTESIAN_POINT ( 'NONE',  ( 0.3622758884714730732, 0.8252992914322084816, 43.10531414739106282 ) ) ;
#57907 = EDGE_CURVE ( 'NONE', #52728, #40342, #8061, .T. ) ;
#57908 = CARTESIAN_POINT ( 'NONE',  ( -6.057079549204054558, 7.802675369763562685, 17.60538236374954479 ) ) ;
#57909 = CARTESIAN_POINT ( 'NONE',  ( 5.958863334805807099, 20.35021240744030990, 2.677925489610707643 ) ) ;
#57910 = VECTOR ( 'NONE', #61239, 1000.000000000000114 ) ;
#57911 = VERTEX_POINT ( 'NONE', #21727 ) ;
#57912 = CARTESIAN_POINT ( 'NONE',  ( 1.091591847532195736, 24.22985240271725971, 34.20048601260478449 ) ) ;
#57913 = AXIS2_PLACEMENT_3D ( 'NONE', #34573, #723, #53635 ) ;
#57914 = CARTESIAN_POINT ( 'NONE',  ( 3.238741278300275361, 3.793425828152074519, 42.82436441900174628 ) ) ;
#57915 = CARTESIAN_POINT ( 'NONE',  ( 0.5809828226811617480, 47.41188724015879785, 6.791453954330491705 ) ) ;
#57916 = FACE_OUTER_BOUND ( 'NONE', #3891, .T. ) ;
#57917 = DIRECTION ( 'NONE',  ( -1.000000000000000000, -0.000000000000000000, -0.000000000000000000 ) ) ;
#57918 = VERTEX_POINT ( 'NONE', #22343 ) ;
#57919 = ADVANCED_FACE ( 'NONE', ( #40867 ), #15962, .F. ) ;
#57920 = CARTESIAN_POINT ( 'NONE',  ( 0.5809828226811544205, 17.82437196699742188, -44.45562576850583270 ) ) ;
#57921 = DIRECTION ( 'NONE',  ( -0.000000000000000000, 0.000000000000000000, 1.000000000000000000 ) ) ;
#57922 = DIRECTION ( 'NONE',  ( 2.218671295934095703E-31, -1.000000000000000000, 1.110223024625156540E-16 ) ) ;
#57923 = ORIENTED_EDGE ( 'NONE', *, *, #39006, .T. ) ;
#57924 = CARTESIAN_POINT ( 'NONE',  ( 0.5804410086790514622, -29.86002002114358689, -36.16488706179379875 ) ) ;
#57925 = CARTESIAN_POINT ( 'NONE',  ( 0.6846871229502899947, 7.109010606687386158, 47.37786444808395458 ) ) ;
#57926 = ORIENTED_EDGE ( 'NONE', *, *, #47788, .F. ) ;
#57927 = CARTESIAN_POINT ( 'NONE',  ( 3.660087539127338641, 36.93668088065486188, -30.71416465583017441 ) ) ;
#57928 = VECTOR ( 'NONE', #8057, 1000.000000000000114 ) ;
#57929 = B_SPLINE_CURVE_WITH_KNOTS ( 'NONE', 3,
 ( #48865, #10662, #30062, #9722 ),
 .UNSPECIFIED., .F., .F.,
 ( 4, 4 ),
 ( 0.000000000000000000, 0.004050076154992999881 ),
 .UNSPECIFIED. ) ;
#57930 = ORIENTED_EDGE ( 'NONE', *, *, #8388, .T. ) ;
#57931 = CARTESIAN_POINT ( 'NONE',  ( 2.281448460670570277, -47.95523685111403722, 1.314143534315736828 ) ) ;
#57932 = ORIENTED_EDGE ( 'NONE', *, *, #32694, .F. ) ;
#57933 = CARTESIAN_POINT ( 'NONE',  ( 0.1154773475650539977, 29.53133311701487784, -32.78481347175886640 ) ) ;
#57934 = LINE ( 'NONE', #939, #57296 ) ;
#57935 = ORIENTED_EDGE ( 'NONE', *, *, #37708, .F. ) ;
#57936 = CARTESIAN_POINT ( 'NONE',  ( 0.8557997880470697982, -41.93815086860240626, -23.15977007032367041 ) ) ;
#57937 = ORIENTED_EDGE ( 'NONE', *, *, #18929, .T. ) ;
#57938 = CARTESIAN_POINT ( 'NONE',  ( 0.5809828226811553087, 41.74875432577648837, 23.47450554821725532 ) ) ;
#57939 = LINE ( 'NONE', #33829, #41716 ) ;
#57940 = CARTESIAN_POINT ( 'NONE',  ( 1.231276596079881047, -31.65135013586901991, 27.48579279545509380 ) ) ;
#57941 = CARTESIAN_POINT ( 'NONE',  ( 0.8557997880470697982, -7.156447707085392018, -47.37054680076713709 ) ) ;
#57942 = EDGE_CURVE ( 'NONE', #11949, #26869, #47677, .T. ) ;
#57943 = ORIENTED_EDGE ( 'NONE', *, *, #29550, .F. ) ;
#57944 = CARTESIAN_POINT ( 'NONE',  ( 4.975801465491694664, 45.18341283946434572, 15.94009207553066787 ) ) ;
#57945 = CARTESIAN_POINT ( 'NONE',  ( 4.226256110419179812, -36.59953355730235813, -24.31668960559979453 ) ) ;
#57946 = CARTESIAN_POINT ( 'NONE',  ( 5.959828726073459926, -7.850628836606722949, -18.96492317065690969 ) ) ;
#57947 = CARTESIAN_POINT ( 'NONE',  ( 4.975801465491694664, 39.51822597168457918, 27.09127437476394817 ) ) ;
#57948 = VERTEX_POINT ( 'NONE', #26114 ) ;
#57949 = DIRECTION ( 'NONE',  ( 0.000000000000000000, -1.000000000000000000, 0.000000000000000000 ) ) ;
#57950 = CARTESIAN_POINT ( 'NONE',  ( 0.5980271706414711508, 5.412294693955235658, -48.81348490926914963 ) ) ;
#57951 = ORIENTED_EDGE ( 'NONE', *, *, #3382, .T. ) ;
#57952 = CARTESIAN_POINT ( 'NONE',  ( 2.301430502907645170, 38.87758534782506814, -28.20897229937363093 ) ) ;
#57953 = EDGE_CURVE ( 'NONE', #36851, #53765, #37540, .T. ) ;
#57954 = EDGE_LOOP ( 'NONE', ( #12785, #35738, #39901, #2193 ) ) ;
#57955 = CIRCLE ( 'NONE', #36862, 48.91267123290010943 ) ;
#57956 = CARTESIAN_POINT ( 'NONE',  ( -6.015611763856276717, 18.20278301740936655, 4.870987357968240339 ) ) ;
#57957 = CARTESIAN_POINT ( 'NONE',  ( 5.959828726073459926, 0.004526594003377396556, -20.52560994243598813 ) ) ;
#57958 = ORIENTED_EDGE ( 'NONE', *, *, #1180, .T. ) ;
#57959 = CARTESIAN_POINT ( 'NONE',  ( 0.8760168074886965917, 13.30888447662080942, -46.22580377597773094 ) ) ;
#57960 = FACE_OUTER_BOUND ( 'NONE', #51021, .T. ) ;
#57961 = EDGE_CURVE ( 'NONE', #58675, #24495, #5813, .T. ) ;
#57962 = CARTESIAN_POINT ( 'NONE',  ( 3.601714094746197414, 0.2777834434958510457, -42.02545330641159183 ) ) ;
#57963 = CYLINDRICAL_SURFACE ( 'NONE', #39514, 12.49999999999999822 ) ;
#57964 = VECTOR ( 'NONE', #39889, 1000.000000000000000 ) ;
#57965 = ORIENTED_EDGE ( 'NONE', *, *, #3414, .F. ) ;
#57966 = CYLINDRICAL_SURFACE ( 'NONE', #915, 2.649999999999992806 ) ;
#57967 = CARTESIAN_POINT ( 'NONE',  ( 4.975801465491694664, 14.85979367497109571, 45.55012473237758996 ) ) ;
#57968 = CARTESIAN_POINT ( 'NONE',  ( 1.088313998177382613, 33.56520876252064767, 26.73848503423867484 ) ) ;
#57969 = LINE ( 'NONE', #39223, #5877 ) ;
#57970 = CARTESIAN_POINT ( 'NONE',  ( 0.3676999524040323597, -13.34038000160386339, 42.04741186726771929 ) ) ;
#57971 = CARTESIAN_POINT ( 'NONE',  ( 1.657374760986086049, -8.250434774462597431, -43.27609933074585058 ) ) ;
#57972 = EDGE_CURVE ( 'NONE', #4945, #32075, #27478, .T. ) ;
#57973 =( BOUNDED_SURFACE ( )  B_SPLINE_SURFACE ( 3, 1, ( 
 ( #14289, #57774 ),
 ( #14907, #34014 ),
 ( #25505, #39961 ),
 ( #58694, #21124 ) ),
 .UNSPECIFIED., .F., .F., .F. ) 
 B_SPLINE_SURFACE_WITH_KNOTS ( ( 4, 4 ),
 ( 2, 2 ),
 ( 0.000000000000000000, 1.000000000000000000 ),
 ( 0.000000000000000000, 1.000000000000000000 ),
 .UNSPECIFIED. ) 
 GEOMETRIC_REPRESENTATION_ITEM ( )  RATIONAL_B_SPLINE_SURFACE ( (
 ( 1.000000000000000000, 1.000000000000000000),
 ( 0.9952954269826590483, 0.8620686068821307169),
 ( 0.9952954269826590483, 0.8620686068821307169),
 ( 1.000000000000000000, 1.000000000000000000) ) ) 
 REPRESENTATION_ITEM ( '' )  SURFACE ( )  );
#57974 = CARTESIAN_POINT ( 'NONE',  ( 0.2230388203127596225, 6.380812898000993272, 42.64472907182732797 ) ) ;
#57975 = AXIS2_PLACEMENT_3D ( 'NONE', #34987, #12404, #15868 ) ;
#57976 = DIRECTION ( 'NONE',  ( 0.09835009131224566048, 0.9951218349151971232, 0.007732607185434067255 ) ) ;
#57977 = EDGE_CURVE ( 'NONE', #27219, #35226, #41515, .T. ) ;
#57978 = CARTESIAN_POINT ( 'NONE',  ( 0.5988103622719990193, -41.96244039798807535, 23.52668907282270894 ) ) ;
#57979 = CARTESIAN_POINT ( 'NONE',  ( 0.6031356219577718170, 48.10744328000515679, -0.08729769678260468346 ) ) ;
#57980 = CARTESIAN_POINT ( 'NONE',  ( 0.1152339509894530906, -43.78992250378124851, -5.420828125671850017 ) ) ;
#57981 = DIRECTION ( 'NONE',  ( -1.000000000000000000, -0.000000000000000000, -0.000000000000000000 ) ) ;
#57982 = CARTESIAN_POINT ( 'NONE',  ( 0.5817216825391120505, -1.111896124582260059, 46.88281816631330656 ) ) ;
#57983 = EDGE_CURVE ( 'NONE', #35431, #52648, #25262, .T. ) ;
#57984 = CARTESIAN_POINT ( 'NONE',  ( -6.077587904424778920, 17.85108912406241899, 7.220432014686572586 ) ) ;
#57985 = CARTESIAN_POINT ( 'NONE',  ( 0.5987334308729317378, -39.71456587457169007, -28.88453156906020780 ) ) ;
#57986 = VERTEX_POINT ( 'NONE', #54912 ) ;
#57987 = CARTESIAN_POINT ( 'NONE',  ( 0.2940133293163009753, -44.10887658731336103, -0.8047085082206926199 ) ) ;
#57988 = CARTESIAN_POINT ( 'NONE',  ( 0.9790724872846784388, -1.440786257245086910, 41.88387929672208543 ) ) ;
#57989 = CARTESIAN_POINT ( 'NONE',  ( 0.6001305935487422083, 23.60027211631829047, -41.92422178329146476 ) ) ;
#57990 = VERTEX_POINT ( 'NONE', #26417 ) ;
#57991 = EDGE_CURVE ( 'NONE', #58158, #2726, #2835, .T. ) ;
#57992 = CARTESIAN_POINT ( 'NONE',  ( 5.959547316686252039, -20.35048796920738923, 2.675599016784190098 ) ) ;
#57993 = CARTESIAN_POINT ( 'NONE',  ( 1.834102595619085507, 26.25798196791792449, 35.36546518611314838 ) ) ;
#57994 = ORIENTED_EDGE ( 'NONE', *, *, #42455, .F. ) ;
#57995 = ORIENTED_EDGE ( 'NONE', *, *, #47538, .T. ) ;
#57996 =( BOUNDED_SURFACE ( )  B_SPLINE_SURFACE ( 3, 1, ( 
 ( #17924, #12301 ),
 ( #50489, #7562 ),
 ( #2866, #22000 ),
 ( #9118, #37654 ) ),
 .UNSPECIFIED., .F., .F., .F. ) 
 B_SPLINE_SURFACE_WITH_KNOTS ( ( 4, 4 ),
 ( 2, 2 ),
 ( 0.000000000000000000, 1.000000000000000000 ),
 ( 0.000000000000000000, 1.000000000000000000 ),
 .UNSPECIFIED. ) 
 GEOMETRIC_REPRESENTATION_ITEM ( )  RATIONAL_B_SPLINE_SURFACE ( (
 ( 1.000000000000000000, 1.000000000000000000),
 ( 0.9953485035131437453, 0.8621029689291523912),
 ( 0.9953485035131437453, 0.8621029689291523912),
 ( 1.000000000000000000, 1.000000000000000000) ) ) 
 REPRESENTATION_ITEM ( '' )  SURFACE ( )  );
#57997 = CARTESIAN_POINT ( 'NONE',  ( -6.001507490154111224, 4.862106078787924446, 18.20581304543299339 ) ) ;
#57998 = ORIENTED_EDGE ( 'NONE', *, *, #57991, .F. ) ;
#57999 = CARTESIAN_POINT ( 'NONE',  ( 0.9754292580325134576, -41.84984047986578304, 2.217728277718696184 ) ) ;
#58000 = VERTEX_POINT ( 'NONE', #42696 ) ;
#58001 = ORIENTED_EDGE ( 'NONE', *, *, #10726, .T. ) ;
#58002 = CARTESIAN_POINT ( 'NONE',  ( -6.078726893082806448, 19.09835798914749816, 2.459016752095430025 ) ) ;
#58003 = EDGE_LOOP ( 'NONE', ( #11446, #17930, #23297, #44505 ) ) ;
#58004 = CARTESIAN_POINT ( 'NONE',  ( 0.3676999524040323597, -44.10520818713899871, -0.8253448321555690859 ) ) ;
#58005 = CARTESIAN_POINT ( 'NONE',  ( 0.9968887458511640487, 39.38692798189865130, 17.02616470386893610 ) ) ;
#58006 = B_SPLINE_CURVE_WITH_KNOTS ( 'NONE', 3,
 ( #6822, #49456, #26575, #54441 ),
 .UNSPECIFIED., .F., .F.,
 ( 4, 4 ),
 ( 0.000000000000000000, 0.004442905043737213969 ),
 .UNSPECIFIED. ) ;
#58007 = LINE ( 'NONE', #15131, #57556 ) ;
#58008 = ORIENTED_EDGE ( 'NONE', *, *, #7949, .T. ) ;
#58009 = LINE ( 'NONE', #29212, #37715 ) ;
#58010 = VECTOR ( 'NONE', #17738, 999.9999999999998863 ) ;
#58011 = CARTESIAN_POINT ( 'NONE',  ( 0.9749527285493317930, -33.86694354778337157, -26.34702925571532361 ) ) ;
#58012 = VERTEX_POINT ( 'NONE', #18896 ) ;
#58013 = EDGE_LOOP ( 'NONE', ( #6372, #39201, #11733, #43031 ) ) ;
#58014 = CARTESIAN_POINT ( 'NONE',  ( -13.51351822333069030, -12.53706398592619387, 7.845252193381024343E-16 ) ) ;
#58015 = CONICAL_SURFACE ( 'NONE', #38093, 43.08621763946400307, 1.568696531533066763 ) ;
#58016 = DIRECTION ( 'NONE',  ( -0.07836865515943411409, 0.9873352307081191270, -0.1379401902675465030 ) ) ;
#58017 = CARTESIAN_POINT ( 'NONE',  ( 4.975610109902397937, 45.55079628452109830, 17.82061629079735354 ) ) ;
#58018 = CARTESIAN_POINT ( 'NONE',  ( 4.553261556744873317, 27.56395660609696563, 34.20186927699770507 ) ) ;
#58019 = CARTESIAN_POINT ( 'NONE',  ( 4.833616638992205949, 20.04871863793747622, 41.67905425467714053 ) ) ;
#58020 = EDGE_CURVE ( 'NONE', #58000, #9797, #5041, .T. ) ;
#58021 = ORIENTED_EDGE ( 'NONE', *, *, #54788, .T. ) ;
#58022 = CARTESIAN_POINT ( 'NONE',  ( -6.078726893082806448, 7.791390017580090088, 17.60932374802262146 ) ) ;
#58023 = CARTESIAN_POINT ( 'NONE',  ( 4.975610109902397937, -36.86873347511098586, -32.14258700041121131 ) ) ;
#58024 = ADVANCED_FACE ( 'NONE', ( #61451 ), #43974, .F. ) ;
#58025 = B_SPLINE_CURVE_WITH_KNOTS ( 'NONE', 3,
 ( #21663, #46111, #3158, #16983, #59236, #21047 ),
 .UNSPECIFIED., .F., .F.,
 ( 4, 2, 4 ),
 ( 1.502890766741732611E-16, 0.0002445252820015207077, 0.0004890505640028911449 ),
 .UNSPECIFIED. ) ;
#58026 = CARTESIAN_POINT ( 'NONE',  ( 5.895596859100789899, 19.70914391261472076, -4.009716878325650491 ) ) ;
#58027 = CARTESIAN_POINT ( 'NONE',  ( 3.782542959838393948, -41.50498340838394995, 6.676391665139376208 ) ) ;
#58028 = EDGE_LOOP ( 'NONE', ( #31876, #49307, #12917, #56237 ) ) ;
#58029 = CARTESIAN_POINT ( 'NONE',  ( 1.296416391601052487, -42.89856844656344492, -10.10050490379914656 ) ) ;
#58030 = CARTESIAN_POINT ( 'NONE',  ( 0.1140933569871964703, 37.18555914042932642, -23.75256073558256986 ) ) ;
#58031 = EDGE_CURVE ( 'NONE', #22299, #45571, #47541, .T. ) ;
#58032 = CARTESIAN_POINT ( 'NONE',  ( -2.708315649062916552, -10.16016146078295890, 10.53288422393038992 ) ) ;
#58033 = CARTESIAN_POINT ( 'NONE',  ( 0.7764139734771210444, -35.37865056912503547, 30.79596653483400104 ) ) ;
#58034 = ORIENTED_EDGE ( 'NONE', *, *, #24398, .T. ) ;
#58035 = ORIENTED_EDGE ( 'NONE', *, *, #51096, .F. ) ;
#58036 = CARTESIAN_POINT ( 'NONE',  ( 4.303969348037258058, -39.44373910178591558, -27.54579249306250688 ) ) ;
#58037 = CARTESIAN_POINT ( 'NONE',  ( 0.7762777257811899201, -13.25585385760139623, 46.03397617421224197 ) ) ;
#58038 = CARTESIAN_POINT ( 'NONE',  ( -6.016761891674565099, 7.207804629151311815, 17.41015286184805078 ) ) ;
#58039 = DIRECTION ( 'NONE',  ( -0.07906939808003034253, 0.8617947135858000651, 0.5010567851280235407 ) ) ;
#58040 = CARTESIAN_POINT ( 'NONE',  ( 0.1149546198390367230, -31.88653494661792465, 30.49910579215944040 ) ) ;
#58041 = CARTESIAN_POINT ( 'NONE',  ( 4.335381028904201628, 38.64381571559615480, -30.10668288940825832 ) ) ;
#58042 = CARTESIAN_POINT ( 'NONE',  ( 0.9968887458511660471, 37.48500720268757647, -20.88287852258405053 ) ) ;
#58043 = DIRECTION ( 'NONE',  ( 0.000000000000000000, 0.000000000000000000, -1.000000000000000000 ) ) ;
#58044 = EDGE_CURVE ( 'NONE', #30729, #59093, #27967, .T. ) ;
#58045 = CARTESIAN_POINT ( 'NONE',  ( 0.1100247026804066219, 30.61332956994582233, -30.37337782329859692 ) ) ;
#58046 = VECTOR ( 'NONE', #2684, 1000.000000000000000 ) ;
#58047 = CARTESIAN_POINT ( 'NONE',  ( 2.526464513654345989, -1.212545078562481393, -42.96196573359005555 ) ) ;
#58048 = ORIENTED_EDGE ( 'NONE', *, *, #5545, .T. ) ;
#58049 = B_SPLINE_CURVE_WITH_KNOTS ( 'NONE', 3,
 ( #51581, #27797, #4890, #24023 ),
 .UNSPECIFIED., .F., .F.,
 ( 4, 4 ),
 ( 5.818439421673296370E-18, 0.004566006591234647236 ),
 .UNSPECIFIED. ) ;
#58050 = EDGE_CURVE ( 'NONE', #50538, #14433, #53589, .T. ) ;
#58051 = CARTESIAN_POINT ( 'NONE',  ( 0.5800708057587414812, -28.65679888493032124, -38.37709891224491798 ) ) ;
#58052 = CARTESIAN_POINT ( 'NONE',  ( 2.281448460670572498, 22.83953674062072636, -42.18752512472219252 ) ) ;
#58053 = B_SPLINE_CURVE_WITH_KNOTS ( 'NONE', 3,
 ( #13936, #51803, #52416, #9510, #61499, #8902, #28012, #37750, #47133, #4177, #42438, #28614, #47741, #36816, #29851, #43364, #719, #30153, #29539, #5409, #48649, #44296, #39590, #48966, #49262 ),
 .UNSPECIFIED., .F., .F.,
 ( 4, 3, 3, 3, 3, 3, 3, 3, 4 ),
 ( 5.818439421673296370E-18, 0.0005656085177311394232, 0.001131215744874499622, 0.001696821861372765916, 0.002262427090022498151, 0.002828031679238745925, 0.003393635864401604862, 0.003977030878808132490, 0.004561030005651159000 ),
 .UNSPECIFIED. ) ;
#58054 = CARTESIAN_POINT ( 'NONE',  ( 4.975801465491694664, -42.71626295676247764, -21.70134120755185947 ) ) ;
#58055 = CARTESIAN_POINT ( 'NONE',  ( 5.896278296736517710, -15.78116101695068174, -12.46923961480650078 ) ) ;
#58056 = DIRECTION ( 'NONE',  ( 0.000000000000000000, 0.000000000000000000, -1.000000000000000000 ) ) ;
#58057 = CARTESIAN_POINT ( 'NONE',  ( 0.5839254288179541730, -41.52446060675843853, 23.86932519546715881 ) ) ;
#58058 = CARTESIAN_POINT ( 'NONE',  ( 4.962356264823608143, 0.000000000000000000, 0.000000000000000000 ) ) ;
#58059 = CARTESIAN_POINT ( 'NONE',  ( 4.833616638992205949, -45.27110352095240131, -9.466882727841984035 ) ) ;
#58060 = EDGE_CURVE ( 'NONE', #10566, #5698, #46514, .T. ) ;
#58061 = AXIS2_PLACEMENT_3D ( 'NONE', #16704, #54892, #31102 ) ;
#58062 = CARTESIAN_POINT ( 'NONE',  ( 0.6027444965799114707, 22.82978205664869265, -43.47803545623195021 ) ) ;
#58063 = CARTESIAN_POINT ( 'NONE',  ( 7.999999999999996447, 2.650000000000832134, -79.99999999999998579 ) ) ;
#58064 = CARTESIAN_POINT ( 'NONE',  ( 3.238018933889920792, 13.23534742317150581, 2.057442819521426269 ) ) ;
#58065 = CARTESIAN_POINT ( 'NONE',  ( 0.3622758884714600280, 42.62881903538200845, 6.444611261694737081 ) ) ;
#58067 = VERTEX_POINT ( 'NONE', #27348 ) ;
#58066 = CARTESIAN_POINT ( 'NONE',  ( 1.227938101723748288, 10.28900963485380693, 41.66816631169195517 ) ) ;
#58068 = ORIENTED_EDGE ( 'NONE', *, *, #43236, .T. ) ;
#58069 = CARTESIAN_POINT ( 'NONE',  ( 2.618530812446111078, -46.32565728282600759, 7.978738403554195280 ) ) ;
#58070 = CARTESIAN_POINT ( 'NONE',  ( 2.500000000000000000, -1.178949249685214307, 2.042000000000001592 ) ) ;
#58071 = CARTESIAN_POINT ( 'NONE',  ( 4.549368137175248350, -32.41327393324159800, 28.14399996863441800 ) ) ;
#58072 = ADVANCED_FACE ( 'NONE', ( #22656 ), #43600, .F. ) ;
#58073 = ORIENTED_EDGE ( 'NONE', *, *, #17002, .F. ) ;
#58074 = CARTESIAN_POINT ( 'NONE',  ( 4.956653778116959508, -15.97476558431919180, 45.35992544608522792 ) ) ;
#58075 = CARTESIAN_POINT ( 'NONE',  ( 0.5837799406558235038, -45.93814528060081415, 9.430289378148106749 ) ) ;
#58076 = CARTESIAN_POINT ( 'NONE',  ( 0.5809828226811560858, -41.74875432577632495, -23.47450554821754309 ) ) ;
#58077 =( BOUNDED_SURFACE ( )  B_SPLINE_SURFACE ( 3, 1, ( 
 ( #35742, #2804 ),
 ( #45149, #60132 ),
 ( #35430, #30699 ),
 ( #50128, #40151 ) ),
 .UNSPECIFIED., .F., .F., .F. ) 
 B_SPLINE_SURFACE_WITH_KNOTS ( ( 4, 4 ),
 ( 2, 2 ),
 ( 0.000000000000000000, 1.000000000000000000 ),
 ( 0.000000000000000000, 1.000000000000000000 ),
 .UNSPECIFIED. ) 
 GEOMETRIC_REPRESENTATION_ITEM ( )  RATIONAL_B_SPLINE_SURFACE ( (
 ( 1.000000000000000000, 1.000000000000000000),
 ( 0.7269869731126821222, 0.9931720237060910339),
 ( 0.7269869731126821222, 0.9931720237060910339),
 ( 1.000000000000000000, 1.000000000000000000) ) ) 
 REPRESENTATION_ITEM ( '' )  SURFACE ( )  );
#58078 = ORIENTED_EDGE ( 'NONE', *, *, #60535, .F. ) ;
#58079 = EDGE_LOOP ( 'NONE', ( #13435, #57469, #45927, #2153 ) ) ;
#58080 = CARTESIAN_POINT ( 'NONE',  ( 0.6029303876144825880, -23.94027529185524017, -41.72757124235813819 ) ) ;
#58081 = CARTESIAN_POINT ( 'NONE',  ( 5.880360259849739535, -31.59460303416009808, 36.09847387447805289 ) ) ;
#58082 = CARTESIAN_POINT ( 'NONE',  ( 1.154321713695929397, -39.32643513900316634, -17.18284946700669380 ) ) ;
#58083 = CARTESIAN_POINT ( 'NONE',  ( 2.643462169533613793, 13.76277278785496350, 46.02269433264237364 ) ) ;
#58084 = CARTESIAN_POINT ( 'NONE',  ( 0.2285344041767093937, -44.11262685805537132, 0.7598170683974434514 ) ) ;
#58085 = CARTESIAN_POINT ( 'NONE',  ( 0.9784957157296374497, -41.11458178947570019, -8.119373206651246733 ) ) ;
#58086 = CARTESIAN_POINT ( 'NONE',  ( 0.5998501479064699549, -5.759754759341138453, 47.76154736470748219 ) ) ;
#58087 = CARTESIAN_POINT ( 'NONE',  ( 0.9757892942422810023, 42.54806590760161100, 5.549787678908529642 ) ) ;
#58088 = ORIENTED_EDGE ( 'NONE', *, *, #50107, .T. ) ;
#58089 = VERTEX_POINT ( 'NONE', #3832 ) ;
#58090 = CARTESIAN_POINT ( 'NONE',  ( 0.6000166863083090663, -19.40010892967683986, 45.11606427011477649 ) ) ;
#58091 = CARTESIAN_POINT ( 'NONE',  ( 1.112077966505211624, 44.04403987788247576, 1.775634073803769697 ) ) ;
#58092 = VERTEX_POINT ( 'NONE', #42097 ) ;
#58093 = CARTESIAN_POINT ( 'NONE',  ( -2.708315649062910779, 8.698422600176970221, 11.76894112707814877 ) ) ;
#58094 = CARTESIAN_POINT ( 'NONE',  ( -2.708315649062916552, 7.087851317223962333, -12.80362818457438578 ) ) ;
#58095 = CARTESIAN_POINT ( 'NONE',  ( 4.956653778116989706, -40.28700667097662347, -26.26162724282415084 ) ) ;
#58096 = DIRECTION ( 'NONE',  ( -0.1011922191286467321, -0.9935638751191113727, 0.05090148176737956109 ) ) ;
#58097 = EDGE_CURVE ( 'NONE', #60198, #49001, #61153, .T. ) ;
#58098 = ORIENTED_EDGE ( 'NONE', *, *, #6670, .F. ) ;
#58099 = CARTESIAN_POINT ( 'NONE',  ( 0.5837157313716048179, 46.48964020809164310, -6.160390970077251893 ) ) ;
#58100 = CARTESIAN_POINT ( 'NONE',  ( 0.9756950546413921677, -42.55388731055342788, -5.504753251348157406 ) ) ;
#58101 = EDGE_CURVE ( 'NONE', #23682, #27212, #5762, .T. ) ;
#58102 = CARTESIAN_POINT ( 'NONE',  ( 5.200000000000002842, 0.000000000000000000, 2.500000000000000444 ) ) ;
#58103 = AXIS2_PLACEMENT_3D ( 'NONE', #23720, #42848, #19042 ) ;
#58104 = CARTESIAN_POINT ( 'NONE',  ( 0.6845945791218034371, 28.51769667890559035, -37.24442907125682467 ) ) ;
#58105 = ORIENTED_EDGE ( 'NONE', *, *, #19085, .T. ) ;
#58106 = CARTESIAN_POINT ( 'NONE',  ( 0.5997462898726536595, 4.195097405483644515, -48.92803682862019343 ) ) ;
#58108 = ORIENTED_EDGE ( 'NONE', *, *, #7323, .T. ) ;
#58107 = EDGE_CURVE ( 'NONE', #31261, #20429, #35146, .T. ) ;
#58109 = CARTESIAN_POINT ( 'NONE',  ( 0.5998501479064699549, 48.10473956285920138, -0.5236536531309904374 ) ) ;
#58110 = CARTESIAN_POINT ( 'NONE',  ( 0.5827357941260193908, 23.63272379758851471, -41.65958460246748984 ) ) ;
#58111 = EDGE_CURVE ( 'NONE', #13041, #55332, #20026, .T. ) ;
#58112 = ORIENTED_EDGE ( 'NONE', *, *, #11583, .F. ) ;
#58113 = CARTESIAN_POINT ( 'NONE',  ( 0.8560838555295158248, -44.00447048317951726, -16.24744323198929052 ) ) ;
#58114 = EDGE_CURVE ( 'NONE', #51844, #10899, #4328, .T. ) ;
#58115 = CARTESIAN_POINT ( 'NONE',  ( 0.6031356219577719280, -47.68448279784259114, 6.365832241665767555 ) ) ;
#58116 = CARTESIAN_POINT ( 'NONE',  ( 5.894904586330512508, 14.91761050190844529, 13.49052663816329911 ) ) ;
#58117 = CARTESIAN_POINT ( 'NONE',  ( 5.901764892641307547, 48.96927204603444039, 0.04315925332823173505 ) ) ;
#58118 = CARTESIAN_POINT ( 'NONE',  ( 0.1152809850208375703, 33.74116055389966107, -28.43377159234631435 ) ) ;
#58119 = CARTESIAN_POINT ( 'NONE',  ( 4.553261556744875094, 22.57774691820428714, 37.68003330573307608 ) ) ;
#58120 = EDGE_CURVE ( 'NONE', #10038, #50798, #35518, .T. ) ;
#58121 = CARTESIAN_POINT ( 'NONE',  ( -6.057079549204054558, 13.82732400278065832, -13.40284828019269625 ) ) ;
#58122 = CARTESIAN_POINT ( 'NONE',  ( -1.139999999999998570, 0.000000000000000000, 0.000000000000000000 ) ) ;
#58123 = ORIENTED_EDGE ( 'NONE', *, *, #30455, .F. ) ;
#58124 = DIRECTION ( 'NONE',  ( 0.000000000000000000, 0.000000000000000000, 1.000000000000000000 ) ) ;
#58125 = CARTESIAN_POINT ( 'NONE',  ( -1.399999999999998579, 0.000000000000000000, 0.000000000000000000 ) ) ;
#58126 = DIRECTION ( 'NONE',  ( 0.07500201931887537365, 0.9744221909196634224, 0.2118397765798812338 ) ) ;
#58127 = B_SPLINE_CURVE_WITH_KNOTS ( 'NONE', 3,
 ( #5858, #25007, #44147, #15614, #45987, #7728, #12457, #26222, #12775, #31870, #17155, #3329, #55960, #3029, #36268, #40670 ),
 .UNSPECIFIED., .F., .F.,
 ( 4, 3, 3, 3, 3, 4 ),
 ( 2.081781105835003463E-17, 0.0002612764279487748975, 0.0003919131003184784861, 0.0005225497727000651474, 0.0007837925190632454627, 0.001045051706266716084 ),
 .UNSPECIFIED. ) ;
#58128 = ORIENTED_EDGE ( 'NONE', *, *, #54717, .F. ) ;
#58129 = CARTESIAN_POINT ( 'NONE',  ( -15.98086288067142924, -12.48233498196030133, -0.6764478645581437632 ) ) ;
#58130 = CARTESIAN_POINT ( 'NONE',  ( 0.9754292589017228288, 32.52564062645490850, -26.42745104496430031 ) ) ;
#58131 = CARTESIAN_POINT ( 'NONE',  ( 0.8744876279028306332, 10.05549467470575209, -48.05452192277493850 ) ) ;
#58132 = CARTESIAN_POINT ( 'NONE',  ( -6.015611763856276717, -7.216738110653151850, -17.40650793417851361 ) ) ;
#58133 = CARTESIAN_POINT ( 'NONE',  ( 0.5809828226811544205, -28.72298383114515374, 38.32755012159135077 ) ) ;
#58134 = CARTESIAN_POINT ( 'NONE',  ( 0.6029303876144825880, 38.24575311130000443, -29.18200390284009060 ) ) ;
#58135 = CARTESIAN_POINT ( 'NONE',  ( -1.599999999999936140, -80.00000000000001421, -5.495822990132159199E-13 ) ) ;
#58136 = CARTESIAN_POINT ( 'NONE',  ( 4.975801465491694664, 32.01766832630313075, -35.64402118370923489 ) ) ;
#58137 = CARTESIAN_POINT ( 'NONE',  ( 0.3676999524040366896, -13.34038000160327364, -42.04741186726791113 ) ) ;
#58138 = CARTESIAN_POINT ( 'NONE',  ( 3.783198216974388739, 38.10565824507926891, -20.00646744835626123 ) ) ;
#58140 = EDGE_LOOP ( 'NONE', ( #36422, #40284, #41249, #51348 ) ) ;
#58139 = CARTESIAN_POINT ( 'NONE',  ( 3.238931869106855377, -38.11291514434428507, -19.89273896137469677 ) ) ;
#58141 = ORIENTED_EDGE ( 'NONE', *, *, #56127, .T. ) ;
#58142 = CARTESIAN_POINT ( 'NONE',  ( -6.077587904424778920, 18.62472241188256206, -4.890371813497390363 ) ) ;
#58143 = FACE_BOUND ( 'NONE', #9166, .T. ) ;
#58144 = CARTESIAN_POINT ( 'NONE',  ( 0.1084644655670281288, 16.86976209534724092, 39.68806829486954513 ) ) ;
#58145 = EDGE_CURVE ( 'NONE', #41543, #54380, #10362, .T. ) ;
#58146 = CARTESIAN_POINT ( 'NONE',  ( 0.1145239942831223490, -23.15231174846270079, 37.56216103216998903 ) ) ;
#58147 = CARTESIAN_POINT ( 'NONE',  ( 0.5987334308729315158, -35.69483792408773581, -33.72597592572879677 ) ) ;
#58149 = CARTESIAN_POINT ( 'NONE',  ( 0.1149546198390367369, 10.08539897964233134, -42.95615546629666426 ) ) ;
#58148 = B_SPLINE_CURVE_WITH_KNOTS ( 'NONE', 3,
 ( #49117, #16224, #6473, #6169, #25305, #54098 ),
 .UNSPECIFIED., .F., .F.,
 ( 4, 2, 4 ),
 ( 4.878909776184769953E-19, 0.0002293801035737079354, 0.0004587602071474153830 ),
 .UNSPECIFIED. ) ;
#58150 = AXIS2_PLACEMENT_3D ( 'NONE', #23397, #57809, #14630 ) ;
#58151 = CIRCLE ( 'NONE', #4124, 48.09070567114147110 ) ;
#58152 = EDGE_CURVE ( 'NONE', #61119, #19166, #25208, .T. ) ;
#58153 = EDGE_LOOP ( 'NONE', ( #56772, #39482, #29814, #17038 ) ) ;
#58154 = CARTESIAN_POINT ( 'NONE',  ( 0.3622758884714600280, -4.808133778521581192, -42.84426538328729350 ) ) ;
#58155 =( BOUNDED_SURFACE ( )  B_SPLINE_SURFACE ( 3, 1, ( 
 ( #55550, #46496 ),
 ( #8561, #31777 ),
 ( #37111, #8251 ),
 ( #27687, #46818 ) ),
 .UNSPECIFIED., .F., .F., .F. ) 
 B_SPLINE_SURFACE_WITH_KNOTS ( ( 4, 4 ),
 ( 2, 2 ),
 ( 0.000000000000000000, 1.000000000000000000 ),
 ( 0.000000000000000000, 1.000000000000000000 ),
 .UNSPECIFIED. ) 
 GEOMETRIC_REPRESENTATION_ITEM ( )  RATIONAL_B_SPLINE_SURFACE ( (
 ( 1.000000000000000000, 1.000000000000000000),
 ( 0.9953390228620291325, 0.8624445117761032620),
 ( 0.9953390228620291325, 0.8624445117761032620),
 ( 1.000000000000000000, 1.000000000000000000) ) ) 
 REPRESENTATION_ITEM ( '' )  SURFACE ( )  );
#58156 = CARTESIAN_POINT ( 'NONE',  ( -4.938558936750251149, -0.8708011863679868680, 8.896908036367455278E-17 ) ) ;
#58157 = CARTESIAN_POINT ( 'NONE',  ( 10.00000000000000533, 2.649999999999715250, 80.00000000000002842 ) ) ;
#58158 = VERTEX_POINT ( 'NONE', #26973 ) ;
#58159 = CARTESIAN_POINT ( 'NONE',  ( 0.5835871038041859915, 43.12129413706150416, 18.43335142741340960 ) ) ;
#58160 = CARTESIAN_POINT ( 'NONE',  ( 0.5832655196449144652, -25.04173839001305524, -39.65030291661683748 ) ) ;
#58161 = ORIENTED_EDGE ( 'NONE', *, *, #22781, .T. ) ;
#58162 = DIRECTION ( 'NONE',  ( 0.02222222222222222307, 0.9997530559290660479, 0.000000000000000000 ) ) ;
#58163 = ORIENTED_EDGE ( 'NONE', *, *, #1698, .F. ) ;
#58164 = DIRECTION ( 'NONE',  ( 1.000000000000000000, 0.000000000000000000, 0.000000000000000000 ) ) ;
#58165 = CARTESIAN_POINT ( 'NONE',  ( 0.8744876279028306332, 43.84003649649945089, -22.09980204357244560 ) ) ;
#58166 = B_SPLINE_CURVE_WITH_KNOTS ( 'NONE', 3,
 ( #41763, #22020, #50815, #31101, #3809, #8508 ),
 .UNSPECIFIED., .F., .F.,
 ( 4, 2, 4 ),
 ( 0.000000000000000000, 0.0002293801035737120554, 0.0004587602071474241108 ),
 .UNSPECIFIED. ) ;
#58167 = VERTEX_POINT ( 'NONE', #35773 ) ;
#58168 = CARTESIAN_POINT ( 'NONE',  ( 2.618530812446111078, -43.92476656374593347, -16.74340680741610754 ) ) ;
#58169 = CARTESIAN_POINT ( 'NONE',  ( 3.661921753701999016, 44.00646358689169801, 16.61512222072446932 ) ) ;
#58170 = CARTESIAN_POINT ( 'NONE',  ( 40.00000000000000000, 0.000000000000000000, 0.000000000000000000 ) ) ;
#58171 = CARTESIAN_POINT ( 'NONE',  ( 4.962356264823597485, -14.71877352713633158, 39.42833123173257803 ) ) ;
#58172 = B_SPLINE_CURVE_WITH_KNOTS ( 'NONE', 3,
 ( #18152, #51639, #56651, #8734 ),
 .UNSPECIFIED., .F., .F.,
 ( 4, 4 ),
 ( 8.673617379884035472E-19, 0.004444878191957666105 ),
 .UNSPECIFIED. ) ;
#58173 = ORIENTED_EDGE ( 'NONE', *, *, #60535, .T. ) ;
#58174 = CARTESIAN_POINT ( 'NONE',  ( -6.017396004339686577, -17.40836349643172198, 7.212050743684117471 ) ) ;
#58175 = CARTESIAN_POINT ( 'NONE',  ( 5.965394784446458765, 16.29267539192326097, 12.48356622107682590 ) ) ;
#58176 = ADVANCED_FACE ( 'NONE', ( #26657 ), #54335, .F. ) ;
#58177 = ORIENTED_EDGE ( 'NONE', *, *, #60509, .T. ) ;
#58178 = CARTESIAN_POINT ( 'NONE',  ( 0.5806925824938499181, 45.37089516811292356, -11.86188155343291584 ) ) ;
#58180 = EDGE_CURVE ( 'NONE', #33349, #54794, #8470, .T. ) ;
#58179 = ORIENTED_EDGE ( 'NONE', *, *, #14603, .F. ) ;
#58181 = CARTESIAN_POINT ( 'NONE',  ( -6.077587904424778920, 18.62472241188249811, 4.890371813497665698 ) ) ;
#58182 = ORIENTED_EDGE ( 'NONE', *, *, #3372, .F. ) ;
#58183 = CARTESIAN_POINT ( 'NONE',  ( 0.8557997880470599172, -37.44587306708076824, -29.88293891557508530 ) ) ;
#58184 = CARTESIAN_POINT ( 'NONE',  ( 0.9784957157296378938, 35.93906772232310942, -21.55728341518576130 ) ) ;
#58185 = EDGE_CURVE ( 'NONE', #26927, #21652, #29499, .T. ) ;
#58186 = CARTESIAN_POINT ( 'NONE',  ( 5.838029081930957709, -45.56116631979244147, -12.45974244248782092 ) ) ;
#58187 = ORIENTED_EDGE ( 'NONE', *, *, #18770, .T. ) ;
#58188 = CARTESIAN_POINT ( 'NONE',  ( 3.678834586032787346, -48.94070755074899637, -1.849192813206288255 ) ) ;
#58189 = EDGE_CURVE ( 'NONE', #49383, #39735, #50762, .T. ) ;
#58190 = CARTESIAN_POINT ( 'NONE',  ( 4.975801465491695552, -15.94009207553018648, -45.18341283946452336 ) ) ;
#58191 = CARTESIAN_POINT ( 'NONE',  ( 0.1158403557922069033, -38.46476121139301085, 21.61949241157930857 ) ) ;
#58192 = ORIENTED_EDGE ( 'NONE', *, *, #13006, .T. ) ;
#58193 = B_SPLINE_CURVE_WITH_KNOTS ( 'NONE', 3,
 ( #5111, #33358, #5716, #23941, #731, #19253 ),
 .UNSPECIFIED., .F., .F.,
 ( 4, 2, 4 ),
 ( 1.517598411722886997E-16, 0.0002445252820015209787, 0.0004890505640028902775 ),
 .UNSPECIFIED. ) ;
#58194 = AXIS2_PLACEMENT_3D ( 'NONE', #6778, #54709, #55635 ) ;
#58195 = EDGE_LOOP ( 'NONE', ( #27139, #3839, #45795, #19591, #13360 ) ) ;
#58196 = CARTESIAN_POINT ( 'NONE',  ( 4.956653778116990594, -26.26162724282345096, -40.28700667097706400 ) ) ;
#58197 = CARTESIAN_POINT ( 'NONE',  ( 4.967162193818130511, -8.839793687084915419, -42.16965968614202609 ) ) ;
#58198 = CARTESIAN_POINT ( 'NONE',  ( 0.1103878639767399555, 30.52789484587411550, 30.45925431905124015 ) ) ;
#58199 = CARTESIAN_POINT ( 'NONE',  ( 5.838029081930955932, 14.01343897760574997, -45.10752250095143268 ) ) ;
#58200 = CARTESIAN_POINT ( 'NONE',  ( -6.016761891674565099, 14.95139917749719949, -11.46828378093544210 ) ) ;
#58201 = ORIENTED_EDGE ( 'NONE', *, *, #5612, .T. ) ;
#58202 = CARTESIAN_POINT ( 'NONE',  ( 4.999999999999983125, 80.00000000000001421, -2.649999999999999467 ) ) ;
#58203 = VERTEX_POINT ( 'NONE', #21345 ) ;
#58204 = FACE_OUTER_BOUND ( 'NONE', #24683, .T. ) ;
#58205 = CARTESIAN_POINT ( 'NONE',  ( 4.956445790444002242, -40.23882117934093827, 24.46171131046763136 ) ) ;
#58206 = CARTESIAN_POINT ( 'NONE',  ( -6.010958268070873523, -17.41463273278773372, -7.197664668556627454 ) ) ;
#58207 = CARTESIAN_POINT ( 'NONE',  ( 0.6000166863083106206, -47.63401213562570291, 11.95091500980227650 ) ) ;
#58208 = CARTESIAN_POINT ( 'NONE',  ( 3.661921753702030546, 39.48008016587397861, -25.57253202031822070 ) ) ;
#58209 = SURFACE_STYLE_USAGE ( .BOTH. , #19114 ) ;
#58210 = PRESENTATION_STYLE_ASSIGNMENT (( #44172 ) ) ;
#58211 = CARTESIAN_POINT ( 'NONE',  ( -6.072942160501519915, -11.02874586101335908, -15.78514893886658399 ) ) ;
#58212 = CARTESIAN_POINT ( 'NONE',  ( 5.901764892641288895, -4.745137497649592362, -48.73884628884928816 ) ) ;
#58213 = DIRECTION ( 'NONE',  ( -1.000000000000000000, -0.000000000000000000, -0.000000000000000000 ) ) ;
#58214 = CARTESIAN_POINT ( 'NONE',  ( 4.549368137175248350, -35.80950303116083688, -23.67244292351627521 ) ) ;
#58215 = CARTESIAN_POINT ( 'NONE',  ( 1.227938101723756947, -17.20315230597815059, -39.32113113558984452 ) ) ;
#58216 = CARTESIAN_POINT ( 'NONE',  ( 0.8554163680231708922, -6.900908941296512999, -46.40671211038068122 ) ) ;
#58217 = ADVANCED_FACE ( 'NONE', ( #7219 ), #43230, .F. ) ;
#58218 = ORIENTED_EDGE ( 'NONE', *, *, #46899, .T. ) ;
#58219 = CARTESIAN_POINT ( 'NONE',  ( 1.231276596079881047, 24.17959027891106416, 34.24360064248583768 ) ) ;
#58220 = DIRECTION ( 'NONE',  ( 0.9848077530122079093, 0.1736481776669315524, -5.551115123125781470E-17 ) ) ;
#58221 = CARTESIAN_POINT ( 'NONE',  ( -6.063463321072278589, -12.93474753578249015, -14.26578980165622035 ) ) ;
#58222 = CARTESIAN_POINT ( 'NONE',  ( 0.9268187852002115479, 40.14212586201818311, 18.23085473000422496 ) ) ;
#58223 = ORIENTED_EDGE ( 'NONE', *, *, #42197, .F. ) ;
#58224 = CARTESIAN_POINT ( 'NONE',  ( 0.5987334363312690755, 32.56457253214104242, 36.75746893178311581 ) ) ;
#58225 = CARTESIAN_POINT ( 'NONE',  ( 0.9747592971366232373, 16.12077520819504528, -39.76507150545817382 ) ) ;
#58226 = AXIS2_PLACEMENT_3D ( 'NONE', #25339, #24106, #49144 ) ;
#58227 = CARTESIAN_POINT ( 'NONE',  ( 5.896782393890504181, 10.82771479451295349, -16.94953330350713117 ) ) ;
#58228 = VECTOR ( 'NONE', #18607, 999.9999999999997726 ) ;
#58229 = ORIENTED_EDGE ( 'NONE', *, *, #28910, .F. ) ;
#58230 = CARTESIAN_POINT ( 'NONE',  ( 4.833616638992205949, -43.93936707042109902, 14.43699082351635532 ) ) ;
#58231 = CARTESIAN_POINT ( 'NONE',  ( 3.661933894777889886, 6.578080033563746376, -46.57638916901656501 ) ) ;
#58232 = EDGE_LOOP ( 'NONE', ( #37645, #32168, #50505, #20920 ) ) ;
#58233 = CARTESIAN_POINT ( 'NONE',  ( 0.1064266418746773052, -17.02047513535257295, 39.62374465289867942 ) ) ;
#58234 = EDGE_LOOP ( 'NONE', ( #47318, #55121, #6164, #39567 ) ) ;
#58235 = PLANE ( 'NONE',  #8569 ) ;
#58236 = VERTEX_POINT ( 'NONE', #50461 ) ;
#58237 = FACE_OUTER_BOUND ( 'NONE', #20209, .T. ) ;
#58238 = DIRECTION ( 'NONE',  ( 0.000000000000000000, 0.000000000000000000, -1.000000000000000000 ) ) ;
#58239 = VERTEX_POINT ( 'NONE', #1911 ) ;
#58240 = CARTESIAN_POINT ( 'NONE',  ( 0.5782707292762423457, -19.08336439318405198, 42.84345407579288434 ) ) ;
#58241 = ORIENTED_EDGE ( 'NONE', *, *, #31292, .T. ) ;
#58242 = CARTESIAN_POINT ( 'NONE',  ( -99.50001199999974233, 2.999999999999992895, -1.500000000000000666 ) ) ;
#58243 = EDGE_CURVE ( 'NONE', #39657, #58899, #13510, .T. ) ;
#58244 =( BOUNDED_SURFACE ( )  B_SPLINE_SURFACE ( 3, 1, ( 
 ( #10395, #29486 ),
 ( #6895, #36077 ),
 ( #40464, #21335 ),
 ( #54830, #36685 ) ),
 .UNSPECIFIED., .F., .F., .F. ) 
 B_SPLINE_SURFACE_WITH_KNOTS ( ( 4, 4 ),
 ( 2, 2 ),
 ( 0.000000000000000000, 1.000000000000000000 ),
 ( 0.000000000000000000, 1.000000000000000000 ),
 .UNSPECIFIED. ) 
 GEOMETRIC_REPRESENTATION_ITEM ( )  RATIONAL_B_SPLINE_SURFACE ( (
 ( 1.000000000000000000, 1.000000000000000000),
 ( 0.9953390228620291325, 0.8624445117760984880),
 ( 0.9953390228620291325, 0.8624445117760984880),
 ( 1.000000000000000000, 1.000000000000000000) ) ) 
 REPRESENTATION_ITEM ( '' )  SURFACE ( )  );
#58245 = CARTESIAN_POINT ( 'NONE',  ( -6.079354080745853928, 17.84913307564929141, -7.225053888790356815 ) ) ;
#58246 = FACE_OUTER_BOUND ( 'NONE', #25140, .T. ) ;
#58247 = ADVANCED_FACE ( 'NONE', ( #7529 ), #41218, .F. ) ;
#58248 = ORIENTED_EDGE ( 'NONE', *, *, #1045, .T. ) ;
#58249 = CARTESIAN_POINT ( 'NONE',  ( 4.956653778116989706, -42.88673967249116004, -21.75875759808752008 ) ) ;
#58250 = CARTESIAN_POINT ( 'NONE',  ( 1.296416391601053153, -35.97301573625679083, -25.46074454754181460 ) ) ;
#58251 = CARTESIAN_POINT ( 'NONE',  ( 0.5837157313716013762, 32.66713943747937066, -33.64662040315945291 ) ) ;
#58252 = CARTESIAN_POINT ( 'NONE',  ( -6.078726893082806448, 17.85000270430361269, -7.222980321520601876 ) ) ;
#58253 = VERTEX_POINT ( 'NONE', #21654 ) ;
#58254 = EDGE_CURVE ( 'NONE', #19623, #21737, #61797, .T. ) ;
#58255 = CARTESIAN_POINT ( 'NONE',  ( -6.077587904424778920, -18.27312872431374657, -6.073614082125261326 ) ) ;
#58256 = CARTESIAN_POINT ( 'NONE',  ( 0.1145239942831223490, -18.15888904951765781, 40.21442812215511964 ) ) ;
#58257 = ORIENTED_EDGE ( 'NONE', *, *, #50850, .F. ) ;
#58258 = CARTESIAN_POINT ( 'NONE',  ( 0.5830081025819954244, -46.80869951554823416, -2.859665023277694118 ) ) ;
#58259 = B_SPLINE_CURVE_WITH_KNOTS ( 'NONE', 3,
 ( #37646, #23217, #56709, #13836, #32940, #5006 ),
 .UNSPECIFIED., .F., .F.,
 ( 4, 2, 4 ),
 ( 8.770652787438942800E-18, 0.0002448709889506563977, 0.0004897419779013040134 ),
 .UNSPECIFIED. ) ;
#58260 = VERTEX_POINT ( 'NONE', #54518 ) ;
#58261 =( BOUNDED_SURFACE ( )  B_SPLINE_SURFACE ( 3, 1, ( 
 ( #27329, #3499 ),
 ( #2033, #21163 ),
 ( #40305, #17946 ),
 ( #37062, #59668 ) ),
 .UNSPECIFIED., .F., .F., .F. ) 
 B_SPLINE_SURFACE_WITH_KNOTS ( ( 4, 4 ),
 ( 2, 2 ),
 ( 0.000000000000000000, 1.000000000000000000 ),
 ( 0.000000000000000000, 1.000000000000000000 ),
 .UNSPECIFIED. ) 
 GEOMETRIC_REPRESENTATION_ITEM ( )  RATIONAL_B_SPLINE_SURFACE ( (
 ( 1.000000000000000000, 1.000000000000000000),
 ( 0.7211978278499968642, 0.9934217856018975334),
 ( 0.7211978278499968642, 0.9934217856018975334),
 ( 1.000000000000000000, 1.000000000000000000) ) ) 
 REPRESENTATION_ITEM ( '' )  SURFACE ( )  );
#58262 = LINE ( 'NONE', #34495, #45530 ) ;
#58263 = CARTESIAN_POINT ( 'NONE',  ( 0.9789233960466683371, 40.45416489533057813, -10.94519389749430793 ) ) ;
#58264 = ORIENTED_EDGE ( 'NONE', *, *, #17089, .F. ) ;
#58265 = CARTESIAN_POINT ( 'NONE',  ( 0.9783242366443549720, -12.16018745800449530, -40.10566457737252932 ) ) ;
#58266 = CARTESIAN_POINT ( 'NONE',  ( 53.01455923075871368, 12.47181771929622585, 0.8542673636581270546 ) ) ;
#58267 = CARTESIAN_POINT ( 'NONE',  ( 0.6254311100348650676, 13.11433105842141345, -46.28443883864382968 ) ) ;
#58268 = EDGE_CURVE ( 'NONE', #35182, #38122, #26347, .T. ) ;
#58269 = ORIENTED_EDGE ( 'NONE', *, *, #60209, .F. ) ;
#58270 = CARTESIAN_POINT ( 'NONE',  ( 0.1155031312995260795, -40.96235978927564503, 16.40203380760271301 ) ) ;
#58271 = EDGE_CURVE ( 'NONE', #19687, #17001, #14798, .T. ) ;
#58272 = CARTESIAN_POINT ( 'NONE',  ( 0.9780303403264778428, 41.49037090854766774, -5.906668711399428950 ) ) ;
#58273 = VECTOR ( 'NONE', #40860, 1000.000000000000227 ) ;
#58274 = CARTESIAN_POINT ( 'NONE',  ( 5.960221823109900008, -17.77295928189549201, -10.26751639438361963 ) ) ;
#58275 = CARTESIAN_POINT ( 'NONE',  ( 0.8760168074887090262, -38.69913431881803945, -28.57146030081966614 ) ) ;
#58276 = CARTESIAN_POINT ( 'NONE',  ( 0.5807400328401637335, 41.75144119563919531, -23.47602859900669969 ) ) ;
#58277 = B_SPLINE_CURVE_WITH_KNOTS ( 'NONE', 3,
 ( #5330, #24459, #57952, #48572 ),
 .UNSPECIFIED., .F., .F.,
 ( 4, 4 ),
 ( 0.000000000000000000, 0.004445488388166994251 ),
 .UNSPECIFIED. ) ;
#58278 = CARTESIAN_POINT ( 'NONE',  ( -17.69733060968885852, -7.723231777284044419, 2.086255951469231373 ) ) ;
#58279 = CARTESIAN_POINT ( 'NONE',  ( 0.8557997880470690211, 46.03118133706043835, -13.27832040216591380 ) ) ;
#58280 = CARTESIAN_POINT ( 'NONE',  ( 0.6001305935487315502, -23.60027211631858535, 41.92422178329128712 ) ) ;
#58281 = DIRECTION ( 'NONE',  ( 0.07439287786467665975, -0.7991213610169907167, 0.5965490341031185473 ) ) ;
#58282 = CARTESIAN_POINT ( 'NONE',  ( 0.1158816050234198619, 39.75696437711800257, 19.13964014347531162 ) ) ;
#58283 = CARTESIAN_POINT ( 'NONE',  ( -2.708315649062910779, 10.16016146078274573, 10.53288422393059243 ) ) ;
#58285 = EDGE_CURVE ( 'NONE', #54562, #32638, #31998, .T. ) ;
#58284 = CIRCLE ( 'NONE', #37317, 42.08604991992415023 ) ;
#58286 = CARTESIAN_POINT ( 'NONE',  ( 1.227938101723756947, 29.74462687941269223, -30.94118573761281965 ) ) ;
#58287 = CARTESIAN_POINT ( 'NONE',  ( 0.5782707292762423457, -46.83939014838220771, -2.409955235114225047 ) ) ;
#58288 = VERTEX_POINT ( 'NONE', #23492 ) ;
#58289 = CARTESIAN_POINT ( 'NONE',  ( 0.5832366564991526836, 28.94058080282834311, -38.16363840618222980 ) ) ;
#58290 = CARTESIAN_POINT ( 'NONE',  ( 0.9762797500689124330, -1.905951756780688733, 41.86516610604248712 ) ) ;
#58291 = CARTESIAN_POINT ( 'NONE',  ( 0.8744876279028263033, 37.95405449045444612, -31.14225101233220627 ) ) ;
#58292 = VERTEX_POINT ( 'NONE', #61380 ) ;
#58293 = CARTESIAN_POINT ( 'NONE',  ( 0.3676999524040323597, 41.59822836379060362, 14.68121181363330408 ) ) ;
#58294 = CARTESIAN_POINT ( 'NONE',  ( 0.7413678028165012757, 25.98796241446775923, 35.62459685827271016 ) ) ;
#58295 = VERTEX_POINT ( 'NONE', #46711 ) ;
#58296 = ORIENTED_EDGE ( 'NONE', *, *, #16060, .T. ) ;
#58297 = B_SPLINE_CURVE_WITH_KNOTS ( 'NONE', 3,
 ( #18256, #23871, #42382, #52054, #40, #13249, #13873, #47366, #4415, #23554, #42684, #61744, #52357, #8844, #41770, #4116 ),
 .UNSPECIFIED., .F., .F.,
 ( 4, 3, 3, 3, 3, 4 ),
 ( 1.250973872328959318E-17, 0.0002732102107931896201, 0.0004098135523333814798, 0.0005464168938824958896, 0.0008195847345945368300, 0.001092771384553101145 ),
 .UNSPECIFIED. ) ;
#58298 = CARTESIAN_POINT ( 'NONE',  ( 5.959828726073459926, 5.308046411395249464, -19.82738831247208111 ) ) ;
#58299 = ORIENTED_EDGE ( 'NONE', *, *, #40700, .F. ) ;
#58300 = LINE ( 'NONE', #14209, #6932 ) ;
#58301 = VERTEX_POINT ( 'NONE', #24931 ) ;
#58302 = EDGE_LOOP ( 'NONE', ( #9658, #4453, #51105, #12544 ) ) ;
#58303 = CARTESIAN_POINT ( 'NONE',  ( 1.231276596079881047, -16.87422718933157739, -38.37365278131454005 ) ) ;
#58304 = ORIENTED_EDGE ( 'NONE', *, *, #169, .T. ) ;
#58305 = CARTESIAN_POINT ( 'NONE',  ( 0.5998501479064699549, -28.86886762351154090, 38.48283596221978797 ) ) ;
#58306 = DIRECTION ( 'NONE',  ( 0.000000000000000000, 1.000000000000000000, 0.000000000000000000 ) ) ;
#58307 = AXIS2_PLACEMENT_3D ( 'NONE', #40954, #25893, #12424 ) ;
#58308 = CARTESIAN_POINT ( 'NONE',  ( 0.8744876279028263033, 46.86690837902584406, -14.62336997314537790 ) ) ;
#58309 = ORIENTED_EDGE ( 'NONE', *, *, #31443, .F. ) ;
#58310 = CARTESIAN_POINT ( 'NONE',  ( 1.157644175074336035, -34.08380111710984295, -24.39870441003963109 ) ) ;
#58311 = CARTESIAN_POINT ( 'NONE',  ( -0.6543461111163950683, -4.241015250120822699, -0.1391502195351546900 ) ) ;
#58312 = ORIENTED_EDGE ( 'NONE', *, *, #32543, .F. ) ;
#58313 = EDGE_CURVE ( 'NONE', #58239, #48392, #21565, .T. ) ;
#58314 = ORIENTED_EDGE ( 'NONE', *, *, #4918, .F. ) ;
#58315 = CARTESIAN_POINT ( 'NONE',  ( 0.3676999524040366896, 43.44964275340416293, 7.620966337964807380 ) ) ;
#58316 = CARTESIAN_POINT ( 'NONE',  ( 47.91934067089189142, 12.48479467718134295, 0.6957625760541074067 ) ) ;
#58317 = CARTESIAN_POINT ( 'NONE',  ( 0.1098349054025746507, -30.64407294528969672, 30.34240357440782887 ) ) ;
#58318 = CARTESIAN_POINT ( 'NONE',  ( 2.624215991343608501, 37.21129343241604914, 30.33228621715047169 ) ) ;
#58319 = ADVANCED_FACE ( 'NONE', ( #27894 ), #13581, .F. ) ;
#58320 = VECTOR ( 'NONE', #49293, 1000.000000000000000 ) ;
#58321 = B_SPLINE_CURVE_WITH_KNOTS ( 'NONE', 3,
 ( #14019, #52502, #18705, #24012 ),
 .UNSPECIFIED., .F., .F.,
 ( 4, 4 ),
 ( 9.047210765559599389E-17, 0.005004741218457501271 ),
 .UNSPECIFIED. ) ;
#58322 = ORIENTED_EDGE ( 'NONE', *, *, #60609, .T. ) ;
#58323 = CARTESIAN_POINT ( 'NONE',  ( 0.1157506346131639274, -1.506969930895584620, -44.09840928457862930 ) ) ;
#58324 = CARTESIAN_POINT ( 'NONE',  ( -6.001507490154110336, 0.01557731607553304240, 18.84387066167321478 ) ) ;
#58325 = EDGE_CURVE ( 'NONE', #47731, #60938, #49181, .T. ) ;
#58326 = CARTESIAN_POINT ( 'NONE',  ( -2.569797478183790229, -10.02484965418634033, -10.65947181927836063 ) ) ;
#58327 = CARTESIAN_POINT ( 'NONE',  ( 1.231276596079881935, -41.24008908601427237, 7.518764738683684001 ) ) ;
#58328 = ORIENTED_EDGE ( 'NONE', *, *, #53503, .F. ) ;
#58329 = CARTESIAN_POINT ( 'NONE',  ( 0.5786265663353196143, 41.11783955080237263, 24.57327059187413099 ) ) ;
#58330 = DIRECTION ( 'NONE',  ( 0.000000000000000000, 0.000000000000000000, 1.000000000000000000 ) ) ;
#58331 = CARTESIAN_POINT ( 'NONE',  ( 2.526552050251863246, -20.43086833796931856, -37.81244156771011689 ) ) ;
#58332 = CARTESIAN_POINT ( 'NONE',  ( 0.5997462898726536595, -34.91088276334701135, -34.53667463477266608 ) ) ;
#58333 = ORIENTED_EDGE ( 'NONE', *, *, #32852, .F. ) ;
#58334 = ORIENTED_EDGE ( 'NONE', *, *, #55460, .F. ) ;
#58335 = CARTESIAN_POINT ( 'NONE',  ( 0.5809828226811617480, 33.48000389720616710, 34.25055090842165839 ) ) ;
#58336 = DIRECTION ( 'NONE',  ( 1.000000000000000000, 0.000000000000000000, 0.000000000000000000 ) ) ;
#58337 = CARTESIAN_POINT ( 'NONE',  ( 0.9789233960466714457, 15.18494337330411525, -39.06090400364393389 ) ) ;
#58338 = ADVANCED_FACE ( 'NONE', ( #5899 ), #9536, .F. ) ;
#58339 = CARTESIAN_POINT ( 'NONE',  ( 0.6039202388192953519, 33.14386950699218204, 36.23599904725224263 ) ) ;
#58340 = B_SPLINE_CURVE_WITH_KNOTS ( 'NONE', 3,
 ( #15471, #43692, #53644, #9522 ),
 .UNSPECIFIED., .F., .F.,
 ( 4, 4 ),
 ( 0.000000000000000000, 0.005014147105413706458 ),
 .UNSPECIFIED. ) ;
#58341 = CARTESIAN_POINT ( 'NONE',  ( 0.5809828226811617480, 11.86925843957166471, 46.40184912890843805 ) ) ;
#58342 = CARTESIAN_POINT ( 'NONE',  ( 0.1157991065609915715, -31.75315110184360279, 30.63788113824431747 ) ) ;
#58343 = DIRECTION ( 'NONE',  ( 0.1024043820194936311, 0.1167898032637338518, -0.9878630899050858671 ) ) ;
#58344 = CARTESIAN_POINT ( 'NONE',  ( 4.975801465491695552, 0.000000000000000000, 0.000000000000000000 ) ) ;
#58345 = CARTESIAN_POINT ( 'NONE',  ( 4.975610109902397937, -23.13264022976583334, 43.09675583078141869 ) ) ;
#58346 = CARTESIAN_POINT ( 'NONE',  ( 0.1103744047535531458, 30.52096488484627201, -30.46616790811190256 ) ) ;
#58347 = CARTESIAN_POINT ( 'NONE',  ( 0.6017666602106490625, -5.933006478841043929, 47.74032907933387548 ) ) ;
#58348 = ORIENTED_EDGE ( 'NONE', *, *, #59314, .F. ) ;
#58349 = B_SPLINE_CURVE_WITH_KNOTS ( 'NONE', 3,
 ( #48883, #316, #57632, #44219, #52953, #10059 ),
 .UNSPECIFIED., .F., .F.,
 ( 4, 2, 4 ),
 ( 9.140795285775094282E-18, 0.0002291978881530158348, 0.0004583957763060225623 ),
 .UNSPECIFIED. ) ;
#58350 = DIRECTION ( 'NONE',  ( 0.07439287786467665975, 0.4871392060437964022, 0.8701500408883694471 ) ) ;
#58351 = CARTESIAN_POINT ( 'NONE',  ( 8.000000000000012434, -80.00000000000001421, -2.147411887991766662E-31 ) ) ;
#58352 = CARTESIAN_POINT ( 'NONE',  ( 0.8753041380234465318, 23.49739456791673220, -43.11624724384784457 ) ) ;
#58353 = CARTESIAN_POINT ( 'NONE',  ( 1.227938101723748288, 25.45152231597057124, 34.55893248994515687 ) ) ;
#58354 = B_SPLINE_CURVE_WITH_KNOTS ( 'NONE', 3,
 ( #35846, #17649, #46172, #59618, #3218, #41169 ),
 .UNSPECIFIED., .F., .F.,
 ( 4, 2, 4 ),
 ( 0.000000000000000000, 0.0002447195606305743124, 0.0004894391212611486248 ),
 .UNSPECIFIED. ) ;
#58355 = CARTESIAN_POINT ( 'NONE',  ( 0.6031357023905875581, -24.09149424676645168, 41.64046004335374818 ) ) ;
#58356 = VECTOR ( 'NONE', #43534, 1000.000000000000000 ) ;
#58357 = CARTESIAN_POINT ( 'NONE',  ( 0.5819845901640492425, -41.70428411658543411, 23.55368560422327562 ) ) ;
#58358 = FACE_OUTER_BOUND ( 'NONE', #12607, .T. ) ;
#58359 = CARTESIAN_POINT ( 'NONE',  ( 0.5807400328401574052, 5.711437504336651649, -47.55718917606836982 ) ) ;
#58360 =( REPRESENTATION_RELATIONSHIP ('NONE','NONE', #44881, #19619 ) REPRESENTATION_RELATIONSHIP_WITH_TRANSFORMATION ( #51824 )SHAPE_REPRESENTATION_RELATIONSHIP( ) );
#58361 =( BOUNDED_SURFACE ( )  B_SPLINE_SURFACE ( 3, 1, ( 
 ( #26199, #55003 ),
 ( #2382, #21507 ),
 ( #35938, #49391 ),
 ( #40645, #11500 ) ),
 .UNSPECIFIED., .F., .F., .F. ) 
 B_SPLINE_SURFACE_WITH_KNOTS ( ( 4, 4 ),
 ( 2, 2 ),
 ( 0.000000000000000000, 1.000000000000000000 ),
 ( 0.000000000000000000, 1.000000000000000000 ),
 .UNSPECIFIED. ) 
 GEOMETRIC_REPRESENTATION_ITEM ( )  RATIONAL_B_SPLINE_SURFACE ( (
 ( 1.000000000000000000, 1.000000000000000000),
 ( 0.9953485035131437453, 0.8621029689291523912),
 ( 0.9953485035131437453, 0.8621029689291523912),
 ( 1.000000000000000000, 1.000000000000000000) ) ) 
 REPRESENTATION_ITEM ( '' )  SURFACE ( )  );
#58362 = CARTESIAN_POINT ( 'NONE',  ( 0.8551540677456715978, 37.45266983663495353, 29.88829867897827341 ) ) ;
#58363 = CARTESIAN_POINT ( 'NONE',  ( 5.894904586330512508, -19.93329511855185032, -2.682006297225941083 ) ) ;
#58364 = CARTESIAN_POINT ( 'NONE',  ( 1.091591847532195958, -27.65185104877846811, 31.49816065315580360 ) ) ;
#58366 = ORIENTED_EDGE ( 'NONE', *, *, #51466, .T. ) ;
#58365 = DIRECTION ( 'NONE',  ( -1.000000000000000000, 0.000000000000000000, 0.000000000000000000 ) ) ;
#58367 = ORIENTED_EDGE ( 'NONE', *, *, #21729, .F. ) ;
#58368 = CARTESIAN_POINT ( 'NONE',  ( 0.1100247026804066219, -43.12411436000287779, -0.1696715072115837497 ) ) ;
#58369 = CARTESIAN_POINT ( 'NONE',  ( 0.5998501479064699549, -48.10473956285919428, 0.5236536531313263909 ) ) ;
#58370 = CARTESIAN_POINT ( 'NONE',  ( 0.1156495703730067992, 41.91905829288828045, 13.77445117122657159 ) ) ;
#58371 = EDGE_CURVE ( 'NONE', #9098, #1997, #17022, .T. ) ;
#58372 = VERTEX_POINT ( 'NONE', #39167 ) ;
#58373 = ORIENTED_EDGE ( 'NONE', *, *, #24339, .F. ) ;
#58374 = DIRECTION ( 'NONE',  ( 0.000000000000000000, -1.000000000000000000, 0.000000000000000000 ) ) ;
#58376 = CARTESIAN_POINT ( 'NONE',  ( 50.50000000000024869, 1.836970198721029747E-14, -7.703719777548943412E-31 ) ) ;
#58375 = STYLED_ITEM ( 'NONE', ( #35955 ), #51018 ) ;
#58377 = CARTESIAN_POINT ( 'NONE',  ( 0.8551540677456715978, -13.28067116677170034, -46.03951182599441694 ) ) ;
#58378 = EDGE_CURVE ( 'NONE', #4978, #35128, #18566, .T. ) ;
#58379 = B_SPLINE_CURVE_WITH_KNOTS ( 'NONE', 3,
 ( #10494, #49014, #6065, #25200, #30820, #39957 ),
 .UNSPECIFIED., .F., .F.,
 ( 4, 2, 4 ),
 ( 0.000000000000000000, 0.0002447195606305751256, 0.0004894391212611502512 ),
 .UNSPECIFIED. ) ;
#58380 = ORIENTED_EDGE ( 'NONE', *, *, #609, .T. ) ;
#58381 = EDGE_LOOP ( 'NONE', ( #21689, #42405, #12053, #35900 ) ) ;
#58382 = CARTESIAN_POINT ( 'NONE',  ( 0.6041374136657476912, 46.42299778158155732, -12.61972904329552847 ) ) ;
#58383 = ADVANCED_FACE ( 'NONE', ( #52607 ), #49975, .F. ) ;
#58384 = CARTESIAN_POINT ( 'NONE',  ( 1.092182651088186907, 36.45430330288407816, 20.68441333815433225 ) ) ;
#58385 = CARTESIAN_POINT ( 'NONE',  ( 0.7954190325252783467, -46.22745637125051132, 13.28627193046288468 ) ) ;
#58386 = CARTESIAN_POINT ( 'NONE',  ( 2.526464513654346877, 42.43615126908567703, -6.809833384818603008 ) ) ;
#58387 = CARTESIAN_POINT ( 'NONE',  ( 0.9762797500689124330, -41.16654106227468901, -7.851158013551661874 ) ) ;
#58388 = FACE_OUTER_BOUND ( 'NONE', #7139, .T. ) ;
#58389 = CARTESIAN_POINT ( 'NONE',  ( 0.1147471544378677044, 14.94721517719480985, -41.51545431426571042 ) ) ;
#58390 = ORIENTED_EDGE ( 'NONE', *, *, #14524, .T. ) ;
#58391 = EDGE_CURVE ( 'NONE', #55418, #5254, #28986, .T. ) ;
#58392 = ORIENTED_EDGE ( 'NONE', *, *, #39795, .F. ) ;
#58393 = CARTESIAN_POINT ( 'NONE',  ( 4.833616638992205949, 2.572717262757331813, 46.17873762321152498 ) ) ;
#58394 = FACE_OUTER_BOUND ( 'NONE', #47969, .T. ) ;
#58395 = ORIENTED_EDGE ( 'NONE', *, *, #40273, .T. ) ;
#58396 = CARTESIAN_POINT ( 'NONE',  ( 2.281351352603298466, 42.18750813859391968, -22.83955855331473117 ) ) ;
#58397 = CARTESIAN_POINT ( 'NONE',  ( 0.1103936448916665869, 5.228610780659758526E-15, -43.12443171339897674 ) ) ;
#58398 = CARTESIAN_POINT ( 'NONE',  ( 0.7242486021783819394, -39.83546762662268748, 28.70796024349811049 ) ) ;
#58399 = DIRECTION ( 'NONE',  ( 0.000000000000000000, 0.000000000000000000, -1.000000000000000000 ) ) ;
#58400 = EDGE_CURVE ( 'NONE', #14042, #55289, #26768, .T. ) ;
#58401 = AXIS2_PLACEMENT_3D ( 'NONE', #36838, #50898, #27104 ) ;
#58402 = ORIENTED_EDGE ( 'NONE', *, *, #2892, .T. ) ;
#58403 = CARTESIAN_POINT ( 'NONE',  ( 0.5824935313925976299, 46.42765273256021175, -6.611447556974842321 ) ) ;
#58404 = CARTESIAN_POINT ( 'NONE',  ( 5.895881250540457863, 0.6675221664549164657, -20.10179334700245946 ) ) ;
#58405 = ADVANCED_FACE ( 'NONE', ( #30655 ), #19993, .F. ) ;
#58406 = CARTESIAN_POINT ( 'NONE',  ( 5.959547316686252039, 2.682663672454912440, -20.34955788964373724 ) ) ;
#58407 = CARTESIAN_POINT ( 'NONE',  ( 4.956445790443988031, 0.000000000000000000, 0.000000000000000000 ) ) ;
#58408 = ORIENTED_EDGE ( 'NONE', *, *, #45718, .T. ) ;
#58409 = CARTESIAN_POINT ( 'NONE',  ( 0.2279481005628787582, 42.10464047700960322, -13.17963343096747053 ) ) ;
#58410 = DIRECTION ( 'NONE',  ( 1.000000000000000000, 0.000000000000000000, 0.000000000000000000 ) ) ;
#58411 = ORIENTED_EDGE ( 'NONE', *, *, #15938, .F. ) ;
#58412 = CARTESIAN_POINT ( 'NONE',  ( -6.015611763856276717, 9.427003116184170750, 16.31561949997079353 ) ) ;
#58413 = CARTESIAN_POINT ( 'NONE',  ( 0.5809828226811553087, 23.47450554821769231, -41.74875432577623258 ) ) ;
#58414 = ORIENTED_EDGE ( 'NONE', *, *, #58254, .F. ) ;
#58415 = LINE ( 'NONE', #5789, #35919 ) ;
#58416 = FACE_OUTER_BOUND ( 'NONE', #51900, .T. ) ;
#58417 = CARTESIAN_POINT ( 'NONE',  ( 1.154321713695927842, -39.95809834491012680, 15.65787958845404582 ) ) ;
#58418 = EDGE_CURVE ( 'NONE', #38319, #42745, #25996, .T. ) ;
#58419 = VECTOR ( 'NONE', #33274, 1000.000000000000114 ) ;
#58420 = CARTESIAN_POINT ( 'NONE',  ( -6.015611763856276717, 18.84324252354755203, 0.006214430185208092740 ) ) ;
#58421 = CARTESIAN_POINT ( 'NONE',  ( 0.3263565795980685191, -4.430380094434308802, -5.351519936624961282 ) ) ;
#58422 = CARTESIAN_POINT ( 'NONE',  ( 0.9268187852002115479, 21.26638028268818204, 38.61988351329813440 ) ) ;
#58423 = CARTESIAN_POINT ( 'NONE',  ( 1.227938101723756947, -37.58536632582764980, -20.72293514920789903 ) ) ;
#58424 = CARTESIAN_POINT ( 'NONE',  ( 0.7057020205115017708, 47.89404687311023423, 0.8412108057954452711 ) ) ;
#58425 = ORIENTED_EDGE ( 'NONE', *, *, #57466, .F. ) ;
#58426 = CARTESIAN_POINT ( 'NONE',  ( 0.5832367798473394593, -24.18350431151191415, 41.34221369670675017 ) ) ;
#58427 = CARTESIAN_POINT ( 'NONE',  ( 0.9762797500689124330, 41.46413394121034912, 6.086902470967687329 ) ) ;
#58428 = CARTESIAN_POINT ( 'NONE',  ( 0.5817216825391117174, 27.44988809114352790, -38.02286938134937344 ) ) ;
#58429 = VERTEX_POINT ( 'NONE', #40109 ) ;
#58430 = CARTESIAN_POINT ( 'NONE',  ( 4.956445790443988031, 46.94638516972315756, 3.684422564749393558 ) ) ;
#58431 = CARTESIAN_POINT ( 'NONE',  ( 4.956445790444027999, 24.88142650099568698, -39.98065363916886383 ) ) ;
#58432 = CARTESIAN_POINT ( 'NONE',  ( 0.6008123274975393224, 22.32719666008250314, 43.73843664856413938 ) ) ;
#58433 = CARTESIAN_POINT ( 'NONE',  ( 3.270143674763207553, -9.482922169187890660, -9.870732238228624666 ) ) ;
#58434 = CARTESIAN_POINT ( 'NONE',  ( 45.00000000000001421, 0.000000000000000000, 0.000000000000000000 ) ) ;
#58435 = CARTESIAN_POINT ( 'NONE',  ( 0.6023142530420679819, 38.00626667377522239, -29.49327578399148209 ) ) ;
#58436 = CARTESIAN_POINT ( 'NONE',  ( 5.917102823773431552, -9.657882276496579266, -17.64128759430771609 ) ) ;
#58437 =( BOUNDED_SURFACE ( )  B_SPLINE_SURFACE ( 3, 1, ( 
 ( #14632, #42524 ),
 ( #57493, #14021 ),
 ( #52820, #13707 ),
 ( #43143, #28711 ) ),
 .UNSPECIFIED., .F., .F., .F. ) 
 B_SPLINE_SURFACE_WITH_KNOTS ( ( 4, 4 ),
 ( 2, 2 ),
 ( 0.000000000000000000, 1.000000000000000000 ),
 ( 0.000000000000000000, 1.000000000000000000 ),
 .UNSPECIFIED. ) 
 GEOMETRIC_REPRESENTATION_ITEM ( )  RATIONAL_B_SPLINE_SURFACE ( (
 ( 1.000000000000000000, 1.000000000000000000),
 ( 0.7223157951917476005, 0.9931996967497186413),
 ( 0.7223157951917476005, 0.9931996967497186413),
 ( 1.000000000000000000, 1.000000000000000000) ) ) 
 REPRESENTATION_ITEM ( '' )  SURFACE ( )  );
#58438 = FACE_OUTER_BOUND ( 'NONE', #19709, .T. ) ;
#58439 = CARTESIAN_POINT ( 'NONE',  ( 0.9791128995231621612, 29.13092919009531911, -30.12849811669700273 ) ) ;
#58441 = ORIENTED_EDGE ( 'NONE', *, *, #51394, .F. ) ;
#58440 = FACE_OUTER_BOUND ( 'NONE', #46976, .T. ) ;
#58442 = ORIENTED_EDGE ( 'NONE', *, *, #8249, .F. ) ;
#58443 = CARTESIAN_POINT ( 'NONE',  ( 0.5832367798473394593, -12.65931911325636072, 46.19266341874892845 ) ) ;
#58444 = CARTESIAN_POINT ( 'NONE',  ( 5.860006189529246790, -48.12869875779306739, -3.171667470663014576 ) ) ;
#58445 = CARTESIAN_POINT ( 'NONE',  ( 0.8744876279028306332, -31.30103973185180521, -37.82320666052162039 ) ) ;
#58446 = EDGE_CURVE ( 'NONE', #53492, #35268, #8787, .T. ) ;
#58447 = CARTESIAN_POINT ( 'NONE',  ( 0.1158516988532803382, -22.83153063445172037, 37.75795767412332538 ) ) ;
#58448 = CARTESIAN_POINT ( 'NONE',  ( 0.5832367798473389042, -47.52096797443091702, 5.981481162905551763 ) ) ;
#58449 = CARTESIAN_POINT ( 'NONE',  ( 0.9968887458511647148, 30.80284987750050618, -29.87314546208197186 ) ) ;
#58450 = EDGE_CURVE ( 'NONE', #3215, #30048, #17796, .T. ) ;
#58451 = EDGE_LOOP ( 'NONE', ( #32693, #36713, #56226, #35030 ) ) ;
#58452 = ORIENTED_EDGE ( 'NONE', *, *, #21824, .F. ) ;
#58453 = CIRCLE ( 'NONE', #31467, 1.000000000000000888 ) ;
#58454 = CARTESIAN_POINT ( 'NONE',  ( 0.1064266418746776105, -5.071708474752946394, -42.82540703015429528 ) ) ;
#58455 = EDGE_CURVE ( 'NONE', #2779, #22153, #55160, .T. ) ;
#58456 = CARTESIAN_POINT ( 'NONE',  ( 0.5980271706414711508, 28.66946741852874325, -39.87619441194936343 ) ) ;
#58457 = EDGE_CURVE ( 'NONE', #50198, #59362, #51610, .T. ) ;
#58458 = DIRECTION ( 'NONE',  ( 0.07500201931887538753, -0.7908860163360090789, 0.6073499866322951135 ) ) ;
#58459 = ORIENTED_EDGE ( 'NONE', *, *, #49230, .T. ) ;
#58460 = CIRCLE ( 'NONE', #35480, 1.000000000000000666 ) ;
#58461 = CARTESIAN_POINT ( 'NONE',  ( 0.2885700199627528884, 36.93108631019295274, -22.25146206940426907 ) ) ;
#58462 = DIRECTION ( 'NONE',  ( 0.000000000000000000, 0.000000000000000000, -1.000000000000000000 ) ) ;
#58463 = VERTEX_POINT ( 'NONE', #28124 ) ;
#58464 = EDGE_CURVE ( 'NONE', #6747, #14, #29759, .T. ) ;
#58465 = DIRECTION ( 'NONE',  ( 0.000000000000000000, 0.000000000000000000, -1.000000000000000000 ) ) ;
#58466 = ORIENTED_EDGE ( 'NONE', *, *, #9034, .T. ) ;
#58467 = ADVANCED_FACE ( 'NONE', ( #37552 ), #60384, .F. ) ;
#58468 = CARTESIAN_POINT ( 'NONE',  ( 0.5824935313925921898, -34.53515692764811007, 31.72634730057278318 ) ) ;
#58469 = FACE_OUTER_BOUND ( 'NONE', #25763, .T. ) ;
#58470 = ORIENTED_EDGE ( 'NONE', *, *, #16950, .T. ) ;
#58471 = CARTESIAN_POINT ( 'NONE',  ( 5.901463166500146684, -20.11262442202718148, 0.01446371710612135916 ) ) ;
#58472 = DIRECTION ( 'NONE',  ( -1.000000000000000000, -0.000000000000000000, -0.000000000000000000 ) ) ;
#58473 = CARTESIAN_POINT ( 'NONE',  ( 2.281448460670571166, -47.37344300043617551, 7.562315317391583136 ) ) ;
#58474 = B_SPLINE_CURVE_WITH_KNOTS ( 'NONE', 3,
 ( #12958, #23261, #61441, #27339, #46466, #4421, #46781, #47373, #18564, #3824, #22961, #18263, #56447, #13561, #8850, #27961, #6503, #35379, #16254, #54438, #30643, #33597, #28877, #35070, #50079 ),
 .UNSPECIFIED., .F., .F.,
 ( 4, 3, 3, 3, 3, 3, 3, 3, 4 ),
 ( 4.906538933386797396E-18, 0.0005656085177311406158, 0.001131215744874499622, 0.001696821861372768084, 0.002262427090022498151, 0.002828031679238745925, 0.003393635864401604862, 0.003977030878808133357, 0.004561030005651159000 ),
 .UNSPECIFIED. ) ;
#58475 = ORIENTED_EDGE ( 'NONE', *, *, #28778, .F. ) ;
#58476 = CARTESIAN_POINT ( 'NONE',  ( -6.072942160501519915, 9.969886825816056231, -16.47438979050330943 ) ) ;
#58477 = CARTESIAN_POINT ( 'NONE',  ( 5.860006189529234355, 45.66786516969951037, -15.52021937683227115 ) ) ;
#58478 = ORIENTED_EDGE ( 'NONE', *, *, #40491, .F. ) ;
#58479 = CARTESIAN_POINT ( 'NONE',  ( 0.2885700199627524998, 20.85752789928062612, -37.73587457854645777 ) ) ;
#58480 = B_SPLINE_CURVE_WITH_KNOTS ( 'NONE', 3,
 ( #59224, #35457, #6277, #21653 ),
 .UNSPECIFIED., .F., .F.,
 ( 4, 4 ),
 ( 8.441528768080324345E-17, 0.005004741218457493465 ),
 .UNSPECIFIED. ) ;
#58481 = ORIENTED_EDGE ( 'NONE', *, *, #46258, .F. ) ;
#58482 = CARTESIAN_POINT ( 'NONE',  ( 0.5827359174754828119, -18.66406616558009901, 44.10985444762177821 ) ) ;
#58483 = VERTEX_POINT ( 'NONE', #19594 ) ;
#58484 = CARTESIAN_POINT ( 'NONE',  ( 5.896782393890504181, 8.460428369634545476, -18.24684188237228000 ) ) ;
#58485 = CARTESIAN_POINT ( 'NONE',  ( 0.6029442701453591180, -30.68607053265919404, -38.33940923414107971 ) ) ;
#58486 = CARTESIAN_POINT ( 'NONE',  ( 0.9736507210033056303, 33.76542629919406835, 26.47691119766800938 ) ) ;
#58487 = ORIENTED_EDGE ( 'NONE', *, *, #42453, .F. ) ;
#58488 = DIRECTION ( 'NONE',  ( -1.000000000000000000, -0.000000000000000000, -0.000000000000000000 ) ) ;
#58489 = CARTESIAN_POINT ( 'NONE',  ( 0.5800708057587385946, 11.78915002112722554, 46.42229836006539756 ) ) ;
#58490 = DIRECTION ( 'NONE',  ( 0.000000000000000000, 0.000000000000000000, -1.000000000000000000 ) ) ;
#58492 = ORIENTED_EDGE ( 'NONE', *, *, #40198, .F. ) ;
#58491 = ADVANCED_FACE ( 'NONE', ( #55685 ), #50333, .F. ) ;
#58493 = ORIENTED_EDGE ( 'NONE', *, *, #40293, .F. ) ;
#58494 = CARTESIAN_POINT ( 'NONE',  ( 0.9787464366903563251, -30.96259958820174418, -28.24272330408581055 ) ) ;
#58495 = DIRECTION ( 'NONE',  ( 0.09835009131224567436, 0.1375559175655290955, -0.9855991218957017574 ) ) ;
#58497 = EDGE_CURVE ( 'NONE', #30064, #24857, #22541, .T. ) ;
#58496 = CARTESIAN_POINT ( 'NONE',  ( 2.301529144917015213, 40.93948199333333093, -25.12312032040467003 ) ) ;
#58498 = CARTESIAN_POINT ( 'NONE',  ( 0.8753041380234530822, 32.34805756193409110, -36.94240787824717387 ) ) ;
#58499 = CARTESIAN_POINT ( 'NONE',  ( 0.9791128995231607179, -27.06130672311420682, -32.00036113364502910 ) ) ;
#58501 = AXIS2_PLACEMENT_3D ( 'NONE', #1563, #5630, #26012 ) ;
#58500 = CARTESIAN_POINT ( 'NONE',  ( 0.6001305935487422083, -38.48510059944066342, 28.87057754790874142 ) ) ;
#58502 = VERTEX_POINT ( 'NONE', #31912 ) ;
#58503 = CARTESIAN_POINT ( 'NONE',  ( 1.157644175074339143, -40.90424016553281206, -9.156714037229400915 ) ) ;
#58504 = ORIENTED_EDGE ( 'NONE', *, *, #10630, .F. ) ;
#58505 = CIRCLE ( 'NONE', #1444, 5.100000000000000533 ) ;
#58506 = CARTESIAN_POINT ( 'NONE',  ( 0.2940135542859015905, -38.82777379878567814, -20.94384230559791860 ) ) ;
#58507 = CARTESIAN_POINT ( 'NONE',  ( -2.099999999999999645, 2.571758278209440971E-16, -5.294516984716111097 ) ) ;
#58508 = VECTOR ( 'NONE', #6453, 1000.000000000000227 ) ;
#58509 = DIRECTION ( 'NONE',  ( 1.000000000000000000, -0.000000000000000000, -0.000000000000000000 ) ) ;
#58510 = CARTESIAN_POINT ( 'NONE',  ( 4.956653778116982600, -47.94889704119054130, 3.690426056929806631 ) ) ;
#58511 = CARTESIAN_POINT ( 'NONE',  ( 3.680974057930773924, -36.90739001595152047, -30.65154904503166122 ) ) ;
#58512 =( LENGTH_UNIT ( ) NAMED_UNIT ( * ) SI_UNIT ( .MILLI., .METRE. ) );
#58513 = CARTESIAN_POINT ( 'NONE',  ( 4.303969348037246512, 46.98258166031703809, -10.35452842635794468 ) ) ;
#58514 = CARTESIAN_POINT ( 'NONE',  ( 0.2111111111111110827, -9.497654031326126400, -1.199999999999999956 ) ) ;
#58515 = CARTESIAN_POINT ( 'NONE',  ( 4.967162193818130511, -8.839793687084915419, -42.16965968614202609 ) ) ;
#58516 =( BOUNDED_SURFACE ( )  B_SPLINE_SURFACE ( 3, 1, ( 
 ( #16912, #45420 ),
 ( #55396, #29208 ),
 ( #34544, #53609 ),
 ( #49788, #60105 ) ),
 .UNSPECIFIED., .F., .F., .F. ) 
 B_SPLINE_SURFACE_WITH_KNOTS ( ( 4, 4 ),
 ( 2, 2 ),
 ( 0.000000000000000000, 1.000000000000000000 ),
 ( 0.000000000000000000, 1.000000000000000000 ),
 .UNSPECIFIED. ) 
 GEOMETRIC_REPRESENTATION_ITEM ( )  RATIONAL_B_SPLINE_SURFACE ( (
 ( 1.000000000000000000, 1.000000000000000000),
 ( 0.7282232189291693025, 0.9929344683865674037),
 ( 0.7282232189291693025, 0.9929344683865674037),
 ( 1.000000000000000000, 1.000000000000000000) ) ) 
 REPRESENTATION_ITEM ( '' )  SURFACE ( )  );
#58517 = CARTESIAN_POINT ( 'NONE',  ( 5.895596859100789899, 17.95274561709314654, -9.067916410092799140 ) ) ;
#58518 = CARTESIAN_POINT ( 'NONE',  ( 3.678748215320118753, -29.06831582091647093, 39.41631425735973693 ) ) ;
#58519 = DIRECTION ( 'NONE',  ( -1.000000000000000000, -0.000000000000000000, -0.000000000000000000 ) ) ;
#58520 = CARTESIAN_POINT ( 'NONE',  ( 0.3676999524040366896, -18.60775935196311082, -39.99627326667158655 ) ) ;
#58521 = CARTESIAN_POINT ( 'NONE',  ( 4.956653778116988818, -45.71126949320240840, -14.93973939759935021 ) ) ;
#58522 = DIRECTION ( 'NONE',  ( 0.09835009131224566048, -0.7941905447268856610, 0.5996571005210273864 ) ) ;
#58523 = EDGE_CURVE ( 'NONE', #14826, #21415, #570, .T. ) ;
#58524 = ORIENTED_EDGE ( 'NONE', *, *, #34542, .F. ) ;
#58525 = CARTESIAN_POINT ( 'NONE',  ( 2.528190830796656741, -39.24301646210592764, -14.90770925085041299 ) ) ;
#58526 = ADVANCED_FACE ( 'NONE', ( #10492 ), #60752, .F. ) ;
#58527 = EDGE_CURVE ( 'NONE', #6056, #26491, #28557, .T. ) ;
#58528 =( BOUNDED_SURFACE ( )  B_SPLINE_SURFACE ( 3, 1, ( 
 ( #11147, #44373 ),
 ( #33729, #34960 ),
 ( #24306, #9910 ),
 ( #25535, #43442 ) ),
 .UNSPECIFIED., .F., .F., .F. ) 
 B_SPLINE_SURFACE_WITH_KNOTS ( ( 4, 4 ),
 ( 2, 2 ),
 ( 0.000000000000000000, 1.000000000000000000 ),
 ( 0.000000000000000000, 1.000000000000000000 ),
 .UNSPECIFIED. ) 
 GEOMETRIC_REPRESENTATION_ITEM ( )  RATIONAL_B_SPLINE_SURFACE ( (
 ( 1.000000000000000000, 1.000000000000000000),
 ( 0.9953040768229005630, 0.8617119497784937465),
 ( 0.9953040768229005630, 0.8617119497784937465),
 ( 1.000000000000000000, 1.000000000000000000) ) ) 
 REPRESENTATION_ITEM ( '' )  SURFACE ( )  );
#58529 = CARTESIAN_POINT ( 'NONE',  ( 0.8557997880470599172, 5.347802024197243043, 47.60865952217000796 ) ) ;
#58530 = CARTESIAN_POINT ( 'NONE',  ( -6.017396004339686577, -4.878103249820940235, -18.20079405513554960 ) ) ;
#58531 = CARTESIAN_POINT ( 'NONE',  ( 1.657374760986086271, 40.21406714598089138, 17.99219972184566885 ) ) ;
#58532 = CARTESIAN_POINT ( 'NONE',  ( 0.5988103564986357874, -23.52668867203678715, 41.96244062389610008 ) ) ;
#58533 = ADVANCED_FACE ( 'NONE', ( #5453 ), #56730, .F. ) ;
#58534 = VERTEX_POINT ( 'NONE', #59317 ) ;
#58535 =( BOUNDED_SURFACE ( )  B_SPLINE_SURFACE ( 3, 1, ( 
 ( #53941, #49561 ),
 ( #39899, #10752 ),
 ( #40829, #59577 ),
 ( #48959, #30143 ) ),
 .UNSPECIFIED., .F., .F., .F. ) 
 B_SPLINE_SURFACE_WITH_KNOTS ( ( 4, 4 ),
 ( 2, 2 ),
 ( 0.000000000000000000, 1.000000000000000000 ),
 ( 0.000000000000000000, 1.000000000000000000 ),
 .UNSPECIFIED. ) 
 GEOMETRIC_REPRESENTATION_ITEM ( )  RATIONAL_B_SPLINE_SURFACE ( (
 ( 1.000000000000000000, 1.000000000000000000),
 ( 0.9953485035131437453, 0.8621029689291523912),
 ( 0.9953485035131437453, 0.8621029689291523912),
 ( 1.000000000000000000, 1.000000000000000000) ) ) 
 REPRESENTATION_ITEM ( '' )  SURFACE ( )  );
#58536 = CARTESIAN_POINT ( 'NONE',  ( 4.956445790444001354, -33.12351118015997997, 33.47194433010209025 ) ) ;
#58537 = CARTESIAN_POINT ( 'NONE',  ( 0.9757787079277436826, 16.45683390770838983, -39.62711913632683292 ) ) ;
#58538 = DIRECTION ( 'NONE',  ( 7.985424459127866231E-16, -4.551914400963141816E-15, 1.000000000000000000 ) ) ;
#58539 = ORIENTED_EDGE ( 'NONE', *, *, #11776, .F. ) ;
#58540 = CARTESIAN_POINT ( 'NONE',  ( 0.5806925824938494740, -35.14454992382308518, -31.04968555389040219 ) ) ;
#58541 = EDGE_CURVE ( 'NONE', #31029, #4050, #49009, .T. ) ;
#58542 = AXIS2_PLACEMENT_3D ( 'NONE', #12069, #49322, #20521 ) ;
#58543 = CARTESIAN_POINT ( 'NONE',  ( 1.231276596079887264, 15.85305549123172320, 38.80666698661448777 ) ) ;
#58544 = ORIENTED_EDGE ( 'NONE', *, *, #57696, .T. ) ;
#58545 = B_SPLINE_CURVE_WITH_KNOTS ( 'NONE', 3,
 ( #26534, #11214, #58482, #59733, #6780, #30303, #25924, #35963, #2089, #40358, #59419, #55026, #31235, #50335, #1172, #16526 ),
 .UNSPECIFIED., .F., .F.,
 ( 4, 3, 3, 3, 3, 4 ),
 ( 1.250973872328959318E-17, 0.0002724568934985565770, 0.0004086836638483839958, 0.0005449104342063665124, 0.0008173270854453630954, 0.001089761613562689659 ),
 .UNSPECIFIED. ) ;
#58546 = DIRECTION ( 'NONE',  ( 0.000000000000000000, 0.000000000000000000, 1.000000000000000000 ) ) ;
#58547 = AXIS2_PLACEMENT_3D ( 'NONE', #17812, #34008, #36940 ) ;
#58548 = EDGE_LOOP ( 'NONE', ( #44651, #30994, #8404, #48939 ) ) ;
#58549 = ORIENTED_EDGE ( 'NONE', *, *, #27201, .T. ) ;
#58550 = LINE ( 'NONE', #43268, #28742 ) ;
#58551 = CARTESIAN_POINT ( 'NONE',  ( 7.999999999999986677, 54.69470952478017978, -58.44237546506749226 ) ) ;
#58552 = VERTEX_POINT ( 'NONE', #34930 ) ;
#58553 = CARTESIAN_POINT ( 'NONE',  ( 5.896782393890504181, 8.471952691971306848, -18.24149403045190354 ) ) ;
#58554 = CIRCLE ( 'NONE', #32571, 42.92674063221959813 ) ;
#58555 = VERTEX_POINT ( 'NONE', #15199 ) ;
#58556 = CARTESIAN_POINT ( 'NONE',  ( 0.9772918015221170318, 19.77570429987702383, -36.94940290714458797 ) ) ;
#58557 = CARTESIAN_POINT ( 'NONE',  ( 0.9722240741986377666, 21.95618662952236733, -36.86535088273183192 ) ) ;
#58558 = VERTEX_POINT ( 'NONE', #20507 ) ;
#58559 = CARTESIAN_POINT ( 'NONE',  ( 5.895596859100789899, 16.58392706178506160, 11.37987462241481929 ) ) ;
#58560 = CARTESIAN_POINT ( 'NONE',  ( 3.390910168358336918, -36.38779999262840192, -24.69868717624702725 ) ) ;
#58561 = CARTESIAN_POINT ( 'NONE',  ( 0.2285344041767079504, -32.21686831072238277, -30.14257066915542183 ) ) ;
#58562 = CARTESIAN_POINT ( 'NONE',  ( 0.6009453534118438522, 44.27682103112805123, 18.81239552213000010 ) ) ;
#58563 = ORIENTED_EDGE ( 'NONE', *, *, #24771, .T. ) ;
#58564 = CARTESIAN_POINT ( 'NONE',  ( -6.077587904424778920, -1.842868750311850601, 19.16767738050321412 ) ) ;
#58565 = B_SPLINE_CURVE_WITH_KNOTS ( 'NONE', 3,
 ( #43103, #4225, #39029, #19918, #29283, #14594 ),
 .UNSPECIFIED., .F., .F.,
 ( 4, 2, 4 ),
 ( 1.870900726506760797E-17, 0.0002293755540694306951, 0.0004587511081388426877 ),
 .UNSPECIFIED. ) ;
#58566 = EDGE_LOOP ( 'NONE', ( #26370, #6767, #19075 ) ) ;
#58567 = DIRECTION ( 'NONE',  ( -1.000000000000000000, -0.000000000000000000, -0.000000000000000000 ) ) ;
#58568 = EDGE_LOOP ( 'NONE', ( #48267, #52217, #48260 ) ) ;
#58569 = CARTESIAN_POINT ( 'NONE',  ( 2.528100132419517365, -2.611617288031734319, -41.89789056471614970 ) ) ;
#58570 = EDGE_CURVE ( 'NONE', #24298, #49021, #23011, .T. ) ;
#58571 = CARTESIAN_POINT ( 'NONE',  ( -2.601141883200665639, -12.77988133643086677, -7.711683376289167668 ) ) ;
#58572 = EDGE_LOOP ( 'NONE', ( #34797, #784, #45672, #51637 ) ) ;
#58573 = CARTESIAN_POINT ( 'NONE',  ( 0.6001305935487315502, 12.95698906763810676, -46.33281397023051085 ) ) ;
#58574 = DIRECTION ( 'NONE',  ( -0.07906939808003032866, -0.8933371237229992268, -0.4423763258421279931 ) ) ;
#58575 = CARTESIAN_POINT ( 'NONE',  ( 53.06478623683360496, 12.48216789012032812, -0.6890828966271237421 ) ) ;
#58576 = CARTESIAN_POINT ( 'NONE',  ( 0.9772918015221170318, -22.89893354421215221, -35.09951136822897411 ) ) ;
#58577 = ORIENTED_EDGE ( 'NONE', *, *, #13530, .F. ) ;
#58578 = CARTESIAN_POINT ( 'NONE',  ( 0.1152809850208375703, -40.98195743264318480, 16.35311736271641436 ) ) ;
#58579 = CARTESIAN_POINT ( 'NONE',  ( -2.708315649062916552, -14.63219292706382824, 0.2635547933243125862 ) ) ;
#58580 = B_SPLINE_CURVE_WITH_KNOTS ( 'NONE', 3,
 ( #4566, #56892, #57188, #37841, #18400, #61587, #9291, #18708, #33123, #28398, #47519, #14324, #19324, #33431, #52506, #9595, #24015, #179, #53717 ),
 .UNSPECIFIED., .F., .F.,
 ( 4, 3, 3, 3, 3, 3, 4 ),
 ( 1.153344816771540786E-16, 0.0002618519381806248868, 0.0003927759815485954873, 0.0005237000248299407195, 0.0006546240681324947894, 0.0007855481115631294566, 0.0009699050456655082314 ),
 .UNSPECIFIED. ) ;
#58581 = CARTESIAN_POINT ( 'NONE',  ( 0.9762797500689124330, 41.59901070109202692, -5.084003725031680077 ) ) ;
#58582 = CARTESIAN_POINT ( 'NONE',  ( -4.000000000000000000, 2.309401076758496263, -5.599999999999999645 ) ) ;
#58583 = DIRECTION ( 'NONE',  ( -1.000000000000000000, -0.000000000000000000, -0.000000000000000000 ) ) ;
#58584 = VECTOR ( 'NONE', #24984, 1000.000000000000114 ) ;
#58585 = CARTESIAN_POINT ( 'NONE',  ( -16.14013041205553378, -7.933563399346938994, -1.060327575359547359 ) ) ;
#58586 = CARTESIAN_POINT ( 'NONE',  ( 4.975801465491695552, -15.94009207553018648, -45.18341283946452336 ) ) ;
#58587 = CARTESIAN_POINT ( 'NONE',  ( 0.8557997880470606944, 38.55640757422477805, -28.43566216844931915 ) ) ;
#58588 = CIRCLE ( 'NONE', #55604, 43.92652462719577500 ) ;
#58589 = CARTESIAN_POINT ( 'NONE',  ( 5.974727161628369032, -17.76736931401853070, -10.27590650342031076 ) ) ;
#58590 = CARTESIAN_POINT ( 'NONE',  ( 2.618530812446111078, 33.67725335819547894, -32.79587467115508304 ) ) ;
#58591 = B_SPLINE_CURVE_WITH_KNOTS ( 'NONE', 3,
 ( #45542, #35836, #11397, #30479, #49593, #12336, #31112, #22034, #31425, #41157, #31739, #7280, #59607, #50829, #21715, #21408, #40244, #7922, #36147 ),
 .UNSPECIFIED., .F., .F.,
 ( 4, 3, 3, 3, 3, 3, 4 ),
 ( 1.250973872328959318E-17, 0.0002732106629380534873, 0.0004098138914053662705, 0.0005464171197651318361, 0.0006830203481512379850, 0.0008196235766963388047, 0.001011968216111141161 ),
 .UNSPECIFIED. ) ;
#58592 = CARTESIAN_POINT ( 'NONE',  ( 0.5817217712918323347, -2.022005932317454846, 46.85238997124955773 ) ) ;
#58593 = ADVANCED_FACE ( 'NONE', ( #30201 ), #1112, .F. ) ;
#58594 = ADVANCED_FACE ( 'NONE', ( #1368 ), #31569, .T. ) ;
#58595 = CARTESIAN_POINT ( 'NONE',  ( -5.440000000000000391, 4.832908975360033023E-15, 0.000000000000000000 ) ) ;
#58596 = CARTESIAN_POINT ( 'NONE',  ( 0.8744876279028263033, 16.11801507201566253, 46.37412684372363714 ) ) ;
#58597 = VECTOR ( 'NONE', #50371, 1000.000000000000114 ) ;
#58598 = ORIENTED_EDGE ( 'NONE', *, *, #12343, .T. ) ;
#58599 = ADVANCED_FACE ( 'NONE', ( #26426 ), #7300, .T. ) ;
#58600 = CARTESIAN_POINT ( 'NONE',  ( 4.060580049360325461, -3.719146386383672009, -43.79081689710593395 ) ) ;
#58601 = CARTESIAN_POINT ( 'NONE',  ( 3.559346040607745287, 18.49490347406712232, -39.89196444181369117 ) ) ;
#58602 = CARTESIAN_POINT ( 'NONE',  ( 0.8751705887134423323, 28.56654290188602019, 38.69254731947842885 ) ) ;
#58603 = EDGE_CURVE ( 'NONE', #45260, #13746, #31444, .T. ) ;
#58604 = EDGE_LOOP ( 'NONE', ( #11909, #34422, #14768, #49604 ) ) ;
#58605 = CARTESIAN_POINT ( 'NONE',  ( 4.967162193818130511, 8.839793687085215623, 42.16965968614196925 ) ) ;
#58606 = CARTESIAN_POINT ( 'NONE',  ( 0.1158816050234198619, 4.242590116464622696, 43.91972757666921012 ) ) ;
#58607 =( BOUNDED_SURFACE ( )  B_SPLINE_SURFACE ( 3, 1, ( 
 ( #54906, #40546 ),
 ( #50222, #26411 ),
 ( #59926, #3514 ),
 ( #21719, #37078 ) ),
 .UNSPECIFIED., .F., .F., .F. ) 
 B_SPLINE_SURFACE_WITH_KNOTS ( ( 4, 4 ),
 ( 2, 2 ),
 ( 0.000000000000000000, 1.000000000000000000 ),
 ( 0.000000000000000000, 1.000000000000000000 ),
 .UNSPECIFIED. ) 
 GEOMETRIC_REPRESENTATION_ITEM ( )  RATIONAL_B_SPLINE_SURFACE ( (
 ( 1.000000000000000000, 1.000000000000000000),
 ( 0.9751682680413298332, 0.9999560080971552356),
 ( 0.9751682680413298332, 0.9999560080971552356),
 ( 1.000000000000000000, 1.000000000000000000) ) ) 
 REPRESENTATION_ITEM ( '' )  SURFACE ( )  );
#58608 = VERTEX_POINT ( 'NONE', #2925 ) ;
#58609 = ORIENTED_EDGE ( 'NONE', *, *, #34083, .F. ) ;
#58610 = CARTESIAN_POINT ( 'NONE',  ( 4.975610109902397937, -46.23629923292363486, -15.95788333023269878 ) ) ;
#58611 = ORIENTED_EDGE ( 'NONE', *, *, #15506, .F. ) ;
#58612 = EDGE_CURVE ( 'NONE', #8115, #47638, #2532, .T. ) ;
#58613 = CARTESIAN_POINT ( 'NONE',  ( 0.6029443449137434907, 10.88499636270525350, 47.88586839733853395 ) ) ;
#58614 = VERTEX_POINT ( 'NONE', #45879 ) ;
#58615 = ORIENTED_EDGE ( 'NONE', *, *, #29281, .T. ) ;
#58616 = CARTESIAN_POINT ( 'NONE',  ( 0.1103310638050661596, 11.08182869403236381, 41.67627416617918357 ) ) ;
#58618 = VERTEX_POINT ( 'NONE', #22665 ) ;
#58617 = EDGE_CURVE ( 'NONE', #16048, #22119, #37225, .T. ) ;
#58619 = DIRECTION ( 'NONE',  ( 1.000000000000000000, -0.000000000000000000, -0.000000000000000000 ) ) ;
#58620 = CARTESIAN_POINT ( 'NONE',  ( 0.1073791018717483448, -42.68962945260958008, 6.109314776651994627 ) ) ;
#58621 = VERTEX_POINT ( 'NONE', #27056 ) ;
#58622 = LINE ( 'NONE', #34859, #43807 ) ;
#58623 = DIRECTION ( 'NONE',  ( 0.07836865515943411409, -0.8593913859058549543, -0.5052769534812721064 ) ) ;
#58624 = ORIENTED_EDGE ( 'NONE', *, *, #38427, .F. ) ;
#58625 = VECTOR ( 'NONE', #40992, 1000.000000000000114 ) ;
#58626 = ORIENTED_EDGE ( 'NONE', *, *, #12762, .F. ) ;
#58627 = CARTESIAN_POINT ( 'NONE',  ( 0.8554163680231720024, 23.34472558242442730, 40.69679668712412735 ) ) ;
#58628 = CIRCLE ( 'NONE', #52653, 47.91270532121795611 ) ;
#58629 = CARTESIAN_POINT ( 'NONE',  ( 0.5804410086790514622, 16.34485605153925647, 43.95867983128994183 ) ) ;
#58630 = CARTESIAN_POINT ( 'NONE',  ( 4.291220156522059348, 13.00516750528174015, -45.27973736082466871 ) ) ;
#58631 = CIRCLE ( 'NONE', #26642, 4.000000000000000888 ) ;
#58632 = CARTESIAN_POINT ( 'NONE',  ( 5.981074661064941900, -16.28853686865590689, -12.48781255314283278 ) ) ;
#58633 = ORIENTED_EDGE ( 'NONE', *, *, #4093, .F. ) ;
#58634 = CARTESIAN_POINT ( 'NONE',  ( 4.549368137175248350, 19.17571786012269541, 38.40568845698284406 ) ) ;
#58635 = CARTESIAN_POINT ( 'NONE',  ( 0.1103310638050661596, 41.63362651001249759, 11.24099191367013617 ) ) ;
#58636 = CARTESIAN_POINT ( 'NONE',  ( -5.995132425357893702, -16.31525984181026701, -9.429450169548125871 ) ) ;
#58638 = EDGE_CURVE ( 'NONE', #35188, #44257, #11812, .T. ) ;
#58637 = B_SPLINE_CURVE_WITH_KNOTS ( 'NONE', 3,
 ( #44633, #6058, #59006, #35228 ),
 .UNSPECIFIED., .F., .F.,
 ( 4, 4 ),
 ( 0.000000000000000000, 0.004446090762761376394 ),
 .UNSPECIFIED. ) ;
#58639 = CARTESIAN_POINT ( 'NONE',  ( 4.549368137175248350, -32.13400537129904677, -28.46244473166662559 ) ) ;
#58640 = ORIENTED_EDGE ( 'NONE', *, *, #15565, .F. ) ;
#58641 = CARTESIAN_POINT ( 'NONE',  ( 5.959828726073459926, 14.51059719297096606, 14.51699876360205188 ) ) ;
#58642 = CARTESIAN_POINT ( 'NONE',  ( 1.227938101723748288, -25.45152231597034387, -34.55893248994532030 ) ) ;
#58643 = CARTESIAN_POINT ( 'NONE',  ( 4.291220156522059348, -47.09990378333908012, 0.9940125280386750140 ) ) ;
#58644 = CARTESIAN_POINT ( 'NONE',  ( 6.189768672337906175, 1.091423221261470733, -2.362915713819767774E-16 ) ) ;
#58645 = ORIENTED_EDGE ( 'NONE', *, *, #21700, .F. ) ;
#58646 = B_SPLINE_CURVE_WITH_KNOTS ( 'NONE', 3,
 ( #21244, #49129, #39142, #59437 ),
 .UNSPECIFIED., .F., .F.,
 ( 4, 4 ),
 ( 0.000000000000000000, 0.005013413432710145910 ),
 .UNSPECIFIED. ) ;
#58647 = ORIENTED_EDGE ( 'NONE', *, *, #29421, .T. ) ;
#58648 = CARTESIAN_POINT ( 'NONE',  ( 0.9762797500689124330, -39.75277516423506086, -13.26806888463731227 ) ) ;
#58649 = DIRECTION ( 'NONE',  ( 0.000000000000000000, 0.000000000000000000, -1.000000000000000000 ) ) ;
#58650 = ADVANCED_FACE ( 'NONE', ( #27360 ), #7511, .F. ) ;
#58651 = FACE_OUTER_BOUND ( 'NONE', #9412, .T. ) ;
#58652 = CARTESIAN_POINT ( 'NONE',  ( 4.958415959904818315, 7.056061540673139731, -44.87110372340841025 ) ) ;
#58653 = DIRECTION ( 'NONE',  ( 0.000000000000000000, 0.000000000000000000, -1.000000000000000000 ) ) ;
#58654 = CARTESIAN_POINT ( 'NONE',  ( 2.526552050251864578, 34.82218744039938940, -25.19159344346087082 ) ) ;
#58655 = CARTESIAN_POINT ( 'NONE',  ( -1.500000000000001332, 8.239576745513313235E-16, 6.728125000000022560 ) ) ;
#58656 = CARTESIAN_POINT ( 'NONE',  ( 0.3622758884714600280, 31.06363466427727360, -29.89648521331598729 ) ) ;
#58657 = CARTESIAN_POINT ( 'NONE',  ( 3.050102900204245682, -14.24207504814269498, -41.62437443975742468 ) ) ;
#58658 = B_SPLINE_CURVE_WITH_KNOTS ( 'NONE', 3,
 ( #2049, #21181, #50296, #55914 ),
 .UNSPECIFIED., .F., .F.,
 ( 4, 4 ),
 ( 0.000000000000000000, 0.004041751736740998614 ),
 .UNSPECIFIED. ) ;
#58659 = CARTESIAN_POINT ( 'NONE',  ( 0.6009452777970410997, -18.81240106508496979, -44.27681866781098563 ) ) ;
#58660 = CARTESIAN_POINT ( 'NONE',  ( 0.8551540677456834771, 5.348818140991586034, -47.61725548905984340 ) ) ;
#58661 = CARTESIAN_POINT ( 'NONE',  ( 3.270143674763207553, -4.983712007628325225, 12.74832469035450977 ) ) ;
#58662 = DIRECTION ( 'NONE',  ( -1.000000000000000000, -1.836909530733573776E-16, 1.925929944387235306E-32 ) ) ;
#58663 = CARTESIAN_POINT ( 'NONE',  ( 2.643462169533600914, 37.25264019563373097, 30.32726672320812966 ) ) ;
#58664 = CARTESIAN_POINT ( 'NONE',  ( 0.8557997880470697982, 24.73961900479251952, 41.02602466100786671 ) ) ;
#58665 = CARTESIAN_POINT ( 'NONE',  ( 0.6024113833632039894, 33.17582052207590237, -36.20644696442712274 ) ) ;
#58666 = CARTESIAN_POINT ( 'NONE',  ( 4.956445790444002242, -40.23882117934093827, 24.46171131046763136 ) ) ;
#58667 = CARTESIAN_POINT ( 'NONE',  ( 0.2940135542859015350, 44.06980801370445278, 2.023010214173724730 ) ) ;
#58668 = CARTESIAN_POINT ( 'NONE',  ( 4.960386119450148179, -16.16390115411144279, 40.65912891531809237 ) ) ;
#58669 = EDGE_CURVE ( 'NONE', #217, #30940, #29645, .T. ) ;
#58670 = AXIS2_PLACEMENT_3D ( 'NONE', #23321, #32107, #23622 ) ;
#58671 = CARTESIAN_POINT ( 'NONE',  ( 5.895596859100789899, -19.93390588528919949, -2.677233529022096992 ) ) ;
#58672 = CARTESIAN_POINT ( 'NONE',  ( 0.6028777368367060907, 49.01203641660475796, -3.059430602004723276 ) ) ;
#58674 = VERTEX_POINT ( 'NONE', #11735 ) ;
#58673 = CARTESIAN_POINT ( 'NONE',  ( 4.553261556744875094, 12.28162544311214432, 42.17465165592641796 ) ) ;
#58675 = VERTEX_POINT ( 'NONE', #41177 ) ;
#58676 = CARTESIAN_POINT ( 'NONE',  ( 0.1095718737110178143, -43.12372487139541732, -0.2569529612656323847 ) ) ;
#58677 = CARTESIAN_POINT ( 'NONE',  ( 2.879087469061463178, 43.76579968909067020, -4.544937222643484098 ) ) ;
#58678 = AXIS2_PLACEMENT_3D ( 'NONE', #25390, #44844, #35434 ) ;
#58679 = CARTESIAN_POINT ( 'NONE',  ( 0.1129192098497455998, 41.72114954716776936, 14.36305915353748297 ) ) ;
#58680 = EDGE_CURVE ( 'NONE', #35032, #40451, #40885, .T. ) ;
#58681 = ORIENTED_EDGE ( 'NONE', *, *, #18992, .F. ) ;
#58682 = ORIENTED_EDGE ( 'NONE', *, *, #3806, .F. ) ;
#58683 = CARTESIAN_POINT ( 'NONE',  ( -6.078075953587585900, 0.6118799989801743111, 19.24631853404655502 ) ) ;
#58684 = DIRECTION ( 'NONE',  ( 1.000000000000000000, 1.836970198721033632E-16, -2.218671295934095703E-31 ) ) ;
#58685 = CARTESIAN_POINT ( 'NONE',  ( 0.6023143664670691511, 6.019611522082684907, 47.72938193173974497 ) ) ;
#58686 = B_SPLINE_CURVE_WITH_KNOTS ( 'NONE', 3,
 ( #30843, #20840, #39980, #59031 ),
 .UNSPECIFIED., .F., .F.,
 ( 4, 4 ),
 ( 4.443059973708341306E-17, 0.005004948556313864282 ),
 .UNSPECIFIED. ) ;
#58687 = ORIENTED_EDGE ( 'NONE', *, *, #7058, .T. ) ;
#58688 = VERTEX_POINT ( 'NONE', #36474 ) ;
#58689 = CIRCLE ( 'NONE', #29691, 43.08621763946400307 ) ;
#58690 = CARTESIAN_POINT ( 'NONE',  ( 0.3676999524040366896, -40.57213187173863389, 17.31625533148228513 ) ) ;
#58691 = CARTESIAN_POINT ( 'NONE',  ( -5.995132425357893702, -4.869002713216444178, -18.20425902871272683 ) ) ;
#58692 = CARTESIAN_POINT ( 'NONE',  ( 0.8744876279028263033, 36.80052600666216023, 32.49725120702480297 ) ) ;
#58693 = EDGE_CURVE ( 'NONE', #41116, #13682, #447, .T. ) ;
#58694 = CARTESIAN_POINT ( 'NONE',  ( 5.895596859100789899, -2.009647457886758914, -20.01223376606161963 ) ) ;
#58695 = B_SPLINE_CURVE_WITH_KNOTS ( 'NONE', 3,
 ( #18865, #24781, #43924, #32963 ),
 .UNSPECIFIED., .F., .F.,
 ( 4, 4 ),
 ( 0.000000000000000000, 0.005004948556313801832 ),
 .UNSPECIFIED. ) ;
#58696 = AXIS2_PLACEMENT_3D ( 'NONE', #9002, #3973, #47534 ) ;
#58697 = CARTESIAN_POINT ( 'NONE',  ( -6.079354080745853928, -16.13884862108089280, 10.50383360654563170 ) ) ;
#58698 = CARTESIAN_POINT ( 'NONE',  ( -6.016489644550736315, -7.206912786933415305, 17.41053539857196952 ) ) ;
#58699 = ORIENTED_EDGE ( 'NONE', *, *, #26112, .F. ) ;
#58700 = ORIENTED_EDGE ( 'NONE', *, *, #61796, .T. ) ;
#58701 = CARTESIAN_POINT ( 'NONE',  ( 0.1119899015040008994, 43.41448048127011816, -7.883158804306861889 ) ) ;
#58702 = CARTESIAN_POINT ( 'NONE',  ( 2.643462169533613793, 25.20536747735722471, 40.89244134039119416 ) ) ;
#58703 = B_SPLINE_CURVE_WITH_KNOTS ( 'NONE', 3,
 ( #50209, #2893, #31416, #6961 ),
 .UNSPECIFIED., .F., .F.,
 ( 4, 4 ),
 ( 2.168404344971008868E-19, 0.004048833967417087357 ),
 .UNSPECIFIED. ) ;
#58704 = VERTEX_POINT ( 'NONE', #52691 ) ;
#58705 = DIRECTION ( 'NONE',  ( 0.000000000000000000, 1.000000000000000000, 0.000000000000000000 ) ) ;
#58706 = CARTESIAN_POINT ( 'NONE',  ( 0.6031357023905875581, 46.45693331047441887, 12.49325238079554268 ) ) ;
#58707 = FACE_OUTER_BOUND ( 'NONE', #14612, .T. ) ;
#58708 = ORIENTED_EDGE ( 'NONE', *, *, #7545, .T. ) ;
#58709 = CARTESIAN_POINT ( 'NONE',  ( 0.5834584762367726052, -14.06796895289726557, 44.73620724372500490 ) ) ;
#58710 = CARTESIAN_POINT ( 'NONE',  ( 0.8560838555295223751, 46.35895890951135812, -7.156798369939577853 ) ) ;
#58711 = CARTESIAN_POINT ( 'NONE',  ( 4.958415959904820092, -15.85236509608376565, -42.56649474273287126 ) ) ;
#58712 = CARTESIAN_POINT ( 'NONE',  ( 5.838029081930955932, 44.62720369181031543, -15.47506862028700070 ) ) ;
#58713 = ADVANCED_FACE ( 'NONE', ( #47702, #43332 ), #14508, .T. ) ;
#58714 = VERTEX_POINT ( 'NONE', #4441 ) ;
#58715 = FACE_OUTER_BOUND ( 'NONE', #61709, .T. ) ;
#58716 = AXIS2_PLACEMENT_3D ( 'NONE', #53244, #25366, #618 ) ;
#58717 = CARTESIAN_POINT ( 'NONE',  ( 4.291220156522059348, -27.13845918422061843, 38.50835013879571278 ) ) ;
#58718 = ORIENTED_EDGE ( 'NONE', *, *, #59252, .T. ) ;
#58719 = DIRECTION ( 'NONE',  ( -1.000000000000000000, -0.000000000000000000, -0.000000000000000000 ) ) ;
#58720 = FACE_OUTER_BOUND ( 'NONE', #35771, .T. ) ;
#58721 = EDGE_LOOP ( 'NONE', ( #45772, #22440, #59988, #20685 ) ) ;
#58722 = LINE ( 'NONE', #6396, #26870 ) ;
#58723 = CARTESIAN_POINT ( 'NONE',  ( 0.6001305935487315502, -41.92422178329186266, 23.60027211631755861 ) ) ;
#58724 = CARTESIAN_POINT ( 'NONE',  ( 1.827119703190779765, 1.232688548475426193, 43.03226500438895386 ) ) ;
#58725 = B_SPLINE_CURVE_WITH_KNOTS ( 'NONE', 3,
 ( #28560, #47683, #52669, #52981, #42, #19190, #38304, #57353, #14486, #48295, #57979, #9766, #47997, #5045, #43311, #344 ),
 .UNSPECIFIED., .F., .F.,
 ( 4, 3, 3, 3, 3, 4 ),
 ( 2.027574016683678720E-17, 0.0002618515315864419768, 0.0003927756766341985875, 0.0005236998216950574563, 0.0007855159896329904409, 0.001047349442285928304 ),
 .UNSPECIFIED. ) ;
#58726 = EDGE_CURVE ( 'NONE', #61046, #3794, #43023, .T. ) ;
#58727 = CARTESIAN_POINT ( 'NONE',  ( 0.6041374136657476912, 18.24862627831534923, -44.51224464244982215 ) ) ;
#58728 = CARTESIAN_POINT ( 'NONE',  ( 2.618530812446111078, 18.20180174657095407, -43.34075682745660885 ) ) ;
#58729 = PLANE ( 'NONE',  #49305 ) ;
#58730 = CARTESIAN_POINT ( 'NONE',  ( 5.272380000000000067, 0.000000000000000000, 0.000000000000000000 ) ) ;
#58731 =( BOUNDED_SURFACE ( )  B_SPLINE_SURFACE ( 3, 1, ( 
 ( #47871, #4920 ),
 ( #213, #57532 ),
 ( #14669, #33780 ),
 ( #52859, #9960 ) ),
 .UNSPECIFIED., .F., .F., .F. ) 
 B_SPLINE_SURFACE_WITH_KNOTS ( ( 4, 4 ),
 ( 2, 2 ),
 ( 0.000000000000000000, 1.000000000000000000 ),
 ( 0.000000000000000000, 1.000000000000000000 ),
 .UNSPECIFIED. ) 
 GEOMETRIC_REPRESENTATION_ITEM ( )  RATIONAL_B_SPLINE_SURFACE ( (
 ( 1.000000000000000000, 1.000000000000000000),
 ( 0.7282232189291693025, 0.9929344683865674037),
 ( 0.7282232189291693025, 0.9929344683865674037),
 ( 1.000000000000000000, 1.000000000000000000) ) ) 
 REPRESENTATION_ITEM ( '' )  SURFACE ( )  );
#58732 = CARTESIAN_POINT ( 'NONE',  ( 4.691466044806103852, 19.42108863068380842, -40.13652286047873474 ) ) ;
#58733 = EDGE_CURVE ( 'NONE', #3780, #1834, #37896, .T. ) ;
#58734 = CARTESIAN_POINT ( 'NONE',  ( 0.5839879882012679602, -23.94795769224416659, 41.47913983251944359 ) ) ;
#58735 = CARTESIAN_POINT ( 'NONE',  ( 4.975610109902397937, 0.000000000000000000, 0.000000000000000000 ) ) ;
#58736 = CARTESIAN_POINT ( 'NONE',  ( 0.8744876279028263033, 33.66006955981258386, -35.74003032466635688 ) ) ;
#58737 = ORIENTED_EDGE ( 'NONE', *, *, #56692, .F. ) ;
#58738 = CARTESIAN_POINT ( 'NONE',  ( 5.974727161628367256, -14.50236057684855417, 14.52429704002338973 ) ) ;
#58739 = DIRECTION ( 'NONE',  ( 0.09835009131224563272, -0.9164135549743757103, -0.3879606369183604686 ) ) ;
#58740 = FACE_OUTER_BOUND ( 'NONE', #60558, .T. ) ;
#58741 = CARTESIAN_POINT ( 'NONE',  ( 0.1152339509894530906, 44.01863748844489521, -3.049958051533963932 ) ) ;
#58742 = LINE ( 'NONE', #34064, #26105 ) ;
#58743 = CARTESIAN_POINT ( 'NONE',  ( 0.6009452777970412107, 37.89911497740571633, -29.63106797105374568 ) ) ;
#58744 = DIRECTION ( 'NONE',  ( 6.982962677686268288E-15, -6.982962677686264344E-15, 1.000000000000000000 ) ) ;
#58745 = CARTESIAN_POINT ( 'NONE',  ( 3.407937589446178528, 9.356405769959192043, -10.00592723328951195 ) ) ;
#58746 = CARTESIAN_POINT ( 'NONE',  ( 3.407937589446174087, 10.58239600294638905, 8.699069120706806046 ) ) ;
#58747 = EDGE_CURVE ( 'NONE', #52969, #34606, #57243, .T. ) ;
#58748 = CARTESIAN_POINT ( 'NONE',  ( 0.9787464366903556590, 29.26156609637415684, -30.00157899974586329 ) ) ;
#58750 = EDGE_LOOP ( 'NONE', ( #52091, #4206, #27067, #6049, #44208, #31960, #59785, #34869, #6458, #47561, #54934, #8173, #59822, #13515, #52577, #54876, #53122, #44562, #39111, #9113, #5998, #54181, #24429, #43473, #46240, #30120, #14295, #21307, #3131, #33640, #31591, #52495, #10502, #3636, #4941, #33691, #44202, #9493, #45445, #38409, #33872, #39829, #58615, #56333, #49795, #47293, #50179, #19050, #52951, #24327, #32318, #52955, #48391, #19029, #45818, #37204, #25068, #12476, #33198, #3411, #51404, #41176, #42117, #21583, #13277, #25151, #33025, #2853, #38391, #49680, #33327, #34627, #44567, #60569, #16113, #16070, #55241, #56792, #14514, #52002, #35710, #29439, #54186, #6357, #4741, #3082, #39374, #55312, #26500, #32019, #38512, #5826, #30440, #26659, #46877, #16380, #25832, #33102, #45878, #22350, #28032, #48196, #54672, #3682, #17309, #53031, #44433, #39876, #18452, #21506, #33727, #42101, #29617, #44975, #3416, #53846, #57669, #31644, #7826, #2088, #51932, #50878, #9245, #12860, #24659, #2883, #43918, #4789, #23210, #27274, #19819, #34740, #7887, #56014, #25061, #41033, #45018, #12978, #11367, #26330, #14467, #8544, #38906, #47275, #27823, #33650 ) ) ;
#58749 = CARTESIAN_POINT ( 'NONE',  ( 0.5797568665920711517, -29.79412142207816672, 36.21512994990259671 ) ) ;
#58751 = VERTEX_POINT ( 'NONE', #3841 ) ;
#58752 = CARTESIAN_POINT ( 'NONE',  ( 4.956653778116971054, 47.05699031914949160, 9.917440902361329691 ) ) ;
#58753 = FACE_OUTER_BOUND ( 'NONE', #41829, .T. ) ;
#58754 = CARTESIAN_POINT ( 'NONE',  ( 5.894904586330512508, -9.664823957841555568, 17.63861077085082485 ) ) ;
#58755 = EDGE_CURVE ( 'NONE', #20011, #53671, #4218, .T. ) ;
#58756 = CARTESIAN_POINT ( 'NONE',  ( 0.1154773475650540532, -22.71965045366799529, 37.82540301582078968 ) ) ;
#58757 = CARTESIAN_POINT ( 'NONE',  ( 0.5836750258453360374, -47.50958153310754994, 6.071582023534099370 ) ) ;
#58758 = CARTESIAN_POINT ( 'NONE',  ( 0.1152339509894530906, 9.600619954257439304, -43.06704989837540154 ) ) ;
#58759 = EDGE_CURVE ( 'NONE', #3997, #26672, #4527, .T. ) ;
#58760 = ORIENTED_EDGE ( 'NONE', *, *, #57354, .T. ) ;
#58761 = VERTEX_POINT ( 'NONE', #56770 ) ;
#58762 = CARTESIAN_POINT ( 'NONE',  ( 2.528100132419517809, 30.04137667667142964, 29.32182576174984234 ) ) ;
#58763 = CIRCLE ( 'NONE', #17801, 48.09070567114147110 ) ;
#58764 = CARTESIAN_POINT ( 'NONE',  ( 0.1100247026804066219, -10.99745200874666651, -41.69861001364769493 ) ) ;
#58765 = CIRCLE ( 'NONE', #31797, 48.09070567114147110 ) ;
#58766 = CARTESIAN_POINT ( 'NONE',  ( 1.830465331921976579, -34.54963717569211923, -27.32578684880679276 ) ) ;
#58767 = VERTEX_POINT ( 'NONE', #13899 ) ;
#58768 = ADVANCED_FACE ( 'NONE', ( #9475 ), #42582, .T. ) ;
#58769 = CARTESIAN_POINT ( 'NONE',  ( 5.960721111146673579, -0.006321279846680040275, -20.52557019979492026 ) ) ;
#58770 = CARTESIAN_POINT ( 'NONE',  ( 4.962356264823591268, 23.01169039590626753, 35.23773124060775785 ) ) ;
#58771 = ORIENTED_EDGE ( 'NONE', *, *, #10922, .T. ) ;
#58772 = CYLINDRICAL_SURFACE ( 'NONE', #54969, 2.649999999999992806 ) ;
#58773 = EDGE_LOOP ( 'NONE', ( #7543, #40767, #42361, #2366 ) ) ;
#58774 = B_SPLINE_CURVE_WITH_KNOTS ( 'NONE', 3,
 ( #14319, #19319, #33737, #4877, #18085, #56888, #28706, #37205, #56586, #43139, #23093, #175, #8983, #52500, #33427, #38439 ),
 .UNSPECIFIED., .F., .F.,
 ( 4, 3, 3, 3, 3, 4 ),
 ( 6.938893903907228378E-18, 0.0002724568934985511560, 0.0004086836638483824780, 0.0005449104342063647776, 0.0008173270854453713354, 0.001089761613562694213 ),
 .UNSPECIFIED. ) ;
#58775 = CARTESIAN_POINT ( 'NONE',  ( 0.5837799406558231707, -34.71942033614858047, 31.52467923863832411 ) ) ;
#58776 = CARTESIAN_POINT ( 'NONE',  ( 0.3622758884714600280, 29.89648521331588071, 31.06363466427737663 ) ) ;
#58777 = AXIS2_PLACEMENT_3D ( 'NONE', #54256, #21083, #25461 ) ;
#58778 = ORIENTED_EDGE ( 'NONE', *, *, #18831, .T. ) ;
#58779 = CARTESIAN_POINT ( 'NONE',  ( 3.680882792899936362, -25.57189948075158270, -40.59250320379004506 ) ) ;
#58780 = DIRECTION ( 'NONE',  ( 1.850371707708593823E-16, -1.000000000000000000, 0.000000000000000000 ) ) ;
#58781 = CARTESIAN_POINT ( 'NONE',  ( 0.5836750258453369256, 41.56963612796216978, -23.79054009282503301 ) ) ;
#58782 = CARTESIAN_POINT ( 'NONE',  ( 0.1064266418746775550, 43.12102053154801240, 0.5615180042402182492 ) ) ;
#58783 = B_SPLINE_CURVE_WITH_KNOTS ( 'NONE', 3,
 ( #10562, #523, #20279, #58448, #16813, #58757, #16492, #11180, #35925, #50305, #2683, #25888, #59383, #25271, #7061, #40026 ),
 .UNSPECIFIED., .F., .F.,
 ( 4, 3, 3, 3, 3, 4 ),
 ( 1.127622383284612036E-17, 0.0002724568934985564144, 0.0004086836638483807432, 0.0005449104342063628261, 0.0008173270854453688417, 0.001089761613562689226 ),
 .UNSPECIFIED. ) ;
#58784 = AXIS2_PLACEMENT_3D ( 'NONE', #4262, #42225, #23399 ) ;
#58785 = ORIENTED_EDGE ( 'NONE', *, *, #42614, .T. ) ;
#58786 = DIRECTION ( 'NONE',  ( -1.000000000000000000, -0.000000000000000000, -0.000000000000000000 ) ) ;
#58787 = DIRECTION ( 'NONE',  ( 0.000000000000000000, 0.000000000000000000, 1.000000000000000000 ) ) ;
#58789 = VERTEX_POINT ( 'NONE', #28581 ) ;
#58788 =( BOUNDED_SURFACE ( )  B_SPLINE_SURFACE ( 3, 1, ( 
 ( #19242, #1027 ),
 ( #10761, #28927 ),
 ( #398, #14544 ),
 ( #38357, #10136 ) ),
 .UNSPECIFIED., .F., .F., .F. ) 
 B_SPLINE_SURFACE_WITH_KNOTS ( ( 4, 4 ),
 ( 2, 2 ),
 ( 0.000000000000000000, 1.000000000000000000 ),
 ( 0.000000000000000000, 1.000000000000000000 ),
 .UNSPECIFIED. ) 
 GEOMETRIC_REPRESENTATION_ITEM ( )  RATIONAL_B_SPLINE_SURFACE ( (
 ( 1.000000000000000000, 1.000000000000000000),
 ( 0.7211978278499968642, 0.9934217856018975334),
 ( 0.7211978278499968642, 0.9934217856018975334),
 ( 1.000000000000000000, 1.000000000000000000) ) ) 
 REPRESENTATION_ITEM ( '' )  SURFACE ( )  );
#58790 = CARTESIAN_POINT ( 'NONE',  ( 4.958415959904820092, 8.053194174018676321, 44.70290837762335912 ) ) ;
#58791 = ORIENTED_EDGE ( 'NONE', *, *, #8312, .F. ) ;
#58792 = CARTESIAN_POINT ( 'NONE',  ( 0.9772918015221174759, 4.607494702701409928, 41.65462577331908278 ) ) ;
#58793 = VECTOR ( 'NONE', #60143, 1000.000000000000114 ) ;
#58794 = ORIENTED_EDGE ( 'NONE', *, *, #29923, .T. ) ;
#58795 = CARTESIAN_POINT ( 'NONE',  ( 3.660176727303386279, -36.93665184075199193, -30.71420464230603287 ) ) ;
#58796 = CARTESIAN_POINT ( 'NONE',  ( 0.3676999524040366896, -2.238562284875889041, -44.05609404179596567 ) ) ;
#58797 = EDGE_CURVE ( 'NONE', #22171, #33475, #25874, .T. ) ;
#58798 = DIRECTION ( 'NONE',  ( 0.000000000000000000, 0.000000000000000000, -1.000000000000000000 ) ) ;
#58799 = ORIENTED_EDGE ( 'NONE', *, *, #60511, .F. ) ;
#58800 = CARTESIAN_POINT ( 'NONE',  ( 0.5819845901640490204, 5.801229454883947589, 47.54333976522119087 ) ) ;
#58801 = ADVANCED_FACE ( 'NONE', ( #34848 ), #56365, .F. ) ;
#58802 = DIRECTION ( 'NONE',  ( 0.000000000000000000, 0.000000000000000000, 1.000000000000000000 ) ) ;
#58803 = DIRECTION ( 'NONE',  ( -0.1024043820194934507, 0.01315135725337230471, -0.9946559125373959365 ) ) ;
#58804 = ORIENTED_EDGE ( 'NONE', *, *, #51100, .T. ) ;
#58805 = B_SPLINE_CURVE_WITH_KNOTS ( 'NONE', 3,
 ( #56582, #32487, #9585, #56884 ),
 .UNSPECIFIED., .F., .F.,
 ( 4, 4 ),
 ( 1.517883041479706208E-18, 0.004041751736740996880 ),
 .UNSPECIFIED. ) ;
#58806 = EDGE_CURVE ( 'NONE', #61591, #13969, #28865, .T. ) ;
#58807 = B_SPLINE_CURVE_WITH_KNOTS ( 'NONE', 3,
 ( #11507, #35325, #30592, #35019, #7391, #49398 ),
 .UNSPECIFIED., .F., .F.,
 ( 4, 2, 4 ),
 ( 1.215487348918874797E-16, 0.0002448718616795927711, 0.0004897437233590640031 ),
 .UNSPECIFIED. ) ;
#58808 = EDGE_LOOP ( 'NONE', ( #57702, #47579, #59004, #17769 ) ) ;
#58809 =( BOUNDED_SURFACE ( )  B_SPLINE_SURFACE ( 3, 1, ( 
 ( #28469, #23467 ),
 ( #18789, #28784 ),
 ( #52270, #9365 ),
 ( #19400, #42915 ) ),
 .UNSPECIFIED., .F., .F., .F. ) 
 B_SPLINE_SURFACE_WITH_KNOTS ( ( 4, 4 ),
 ( 2, 2 ),
 ( 0.000000000000000000, 1.000000000000000000 ),
 ( 0.000000000000000000, 1.000000000000000000 ),
 .UNSPECIFIED. ) 
 GEOMETRIC_REPRESENTATION_ITEM ( )  RATIONAL_B_SPLINE_SURFACE ( (
 ( 1.000000000000000000, 1.000000000000000000),
 ( 0.9953040768229005630, 0.8617119497784937465),
 ( 0.9953040768229005630, 0.8617119497784937465),
 ( 1.000000000000000000, 1.000000000000000000) ) ) 
 REPRESENTATION_ITEM ( '' )  SURFACE ( )  );
#58810 = CARTESIAN_POINT ( 'NONE',  ( 0.5838002273316422741, 18.20308624554832377, 44.30203797796946930 ) ) ;
#58811 = CARTESIAN_POINT ( 'NONE',  ( 0.6000166863083106206, 28.52380356231423519, -39.97769518177558723 ) ) ;
#58812 = CARTESIAN_POINT ( 'NONE',  ( 0.8753041380234465318, -19.05925361776887073, -45.25354328012939220 ) ) ;
#58813 = CARTESIAN_POINT ( 'NONE',  ( 0.1073791018717483448, 25.86618856530710531, -34.50606437925521419 ) ) ;
#58814 = FACE_OUTER_BOUND ( 'NONE', #48487, .T. ) ;
#58815 = CARTESIAN_POINT ( 'NONE',  ( 0.6041374136657476912, -38.05989626241449031, 29.42442150067134676 ) ) ;
#58816 = ORIENTED_EDGE ( 'NONE', *, *, #2128, .F. ) ;
#58817 = ADVANCED_FACE ( 'NONE', ( #48314 ), #34807, .F. ) ;
#58818 = CARTESIAN_POINT ( 'NONE',  ( 4.967162193818130511, 28.74031574030012237, 32.10009971360082659 ) ) ;
#58819 = CIRCLE ( 'NONE', #48859, 2.649999999999992806 ) ;
#58820 = ORIENTED_EDGE ( 'NONE', *, *, #36296, .T. ) ;
#58821 = VECTOR ( 'NONE', #1208, 999.9999999999998863 ) ;
#58822 = CARTESIAN_POINT ( 'NONE',  ( 0.5837799406558232818, 36.86040723981035683, 28.99230807804954679 ) ) ;
#58823 = CARTESIAN_POINT ( 'NONE',  ( 0.5804410086790514622, 4.150428748651738609, 46.71502748642841851 ) ) ;
#58824 = CARTESIAN_POINT ( 'NONE',  ( 0.7044674535453004927, 41.61193891978847148, 26.08158856639488477 ) ) ;
#58825 = CARTESIAN_POINT ( 'NONE',  ( 3.270143674763207553, -11.02405647745176154, 8.113405361969469709 ) ) ;
#58826 = CARTESIAN_POINT ( 'NONE',  ( 0.6041374136657476912, -41.57494627055160663, 24.20487816031449668 ) ) ;
#58827 = CARTESIAN_POINT ( 'NONE',  ( 4.956445790443988031, 0.000000000000000000, 0.000000000000000000 ) ) ;
#58828 = CARTESIAN_POINT ( 'NONE',  ( 0.6021447746440204973, 37.22277672027512097, -32.03132891906035695 ) ) ;
#58829 = CARTESIAN_POINT ( 'NONE',  ( 5.838029081930957709, -16.99499549701665657, -44.07079743105749259 ) ) ;
#58830 = EDGE_CURVE ( 'NONE', #59261, #39909, #5373, .T. ) ;
#58831 = CARTESIAN_POINT ( 'NONE',  ( 5.959547316686252039, -20.52562247508876681, 0.003562808152837171945 ) ) ;
#58832 = CARTESIAN_POINT ( 'NONE',  ( 0.9762797500689124330, 9.222352665238359393, 40.88120590813919364 ) ) ;
#58833 = B_SPLINE_CURVE_WITH_KNOTS ( 'NONE', 3,
 ( #12105, #2352, #54344, #16470 ),
 .UNSPECIFIED., .F., .F.,
 ( 4, 4 ),
 ( 0.000000000000000000, 0.005013413432710155451 ),
 .UNSPECIFIED. ) ;
#58834 = CIRCLE ( 'NONE', #52855, 10.00000000000000000 ) ;
#58835 = EDGE_CURVE ( 'NONE', #12174, #1980, #11039, .T. ) ;
#58836 = CARTESIAN_POINT ( 'NONE',  ( 5.880360259849739535, 39.86101557989670852, -26.69116321728528973 ) ) ;
#58837 = CARTESIAN_POINT ( 'NONE',  ( 0.5838002273316428292, -23.82993264414535872, -41.54704836736074469 ) ) ;
#58838 = CARTESIAN_POINT ( 'NONE',  ( -5.995132425357893702, -18.19985213254575740, 4.885449473615266491 ) ) ;
#58839 = DIRECTION ( 'NONE',  ( -1.000000000000000000, 0.000000000000000000, 0.000000000000000000 ) ) ;
#58840 = CARTESIAN_POINT ( 'NONE',  ( 4.975801465491695552, -9.906103548667894998, -46.87746200127453022 ) ) ;
#58841 = ADVANCED_FACE ( 'NONE', ( #39249 ), #754, .F. ) ;
#58842 = ORIENTED_EDGE ( 'NONE', *, *, #8312, .T. ) ;
#58843 = COLOUR_RGB ( '', 0.40784314, 0.44705882, 0.49803922) ;
#58844 = DIRECTION ( 'NONE',  ( 1.000000000000000000, 0.000000000000000000, 0.000000000000000000 ) ) ;
#58845 = CARTESIAN_POINT ( 'NONE',  ( 0.7057020205115042133, 5.417413437617573990, 47.59410670607640270 ) ) ;
#58846 = CARTESIAN_POINT ( 'NONE',  ( 0.9756354156337466721, -26.01752520779890077, -34.12075394380531179 ) ) ;
#58847 = DIRECTION ( 'NONE',  ( 0.000000000000000000, 0.000000000000000000, 1.000000000000000000 ) ) ;
#58848 = CARTESIAN_POINT ( 'NONE',  ( 0.8557997880470697982, 17.48760788519276943, -44.60232077416669227 ) ) ;
#58849 = ORIENTED_EDGE ( 'NONE', *, *, #18718, .T. ) ;
#58850 = CARTESIAN_POINT ( 'NONE',  ( 0.8551540677456834771, -37.45266983663517379, 29.88829867897800696 ) ) ;
#58851 = CARTESIAN_POINT ( 'NONE',  ( 0.5804410086790514622, 10.33990028284761209, 45.74501408892737686 ) ) ;
#58852 = EDGE_CURVE ( 'NONE', #50931, #1298, #15739, .T. ) ;
#58853 = B_SPLINE_CURVE_WITH_KNOTS ( 'NONE', 3,
 ( #3426, #22561, #41685, #60747, #17868, #42605, #18476, #61667, #36993, #18174, #30023, #10942, #29100, #47916, #29404, #39452 ),
 .UNSPECIFIED., .F., .F.,
 ( 4, 3, 3, 3, 3, 4 ),
 ( 1.551621725782133898E-17, 0.0002732102107931892406, 0.0004098135523333850034, 0.0005464168938824949138, 0.0008195847345945449615, 0.001092771384553106349 ),
 .UNSPECIFIED. ) ;
#58854 = CARTESIAN_POINT ( 'NONE',  ( 1.227938101723756947, 15.63977281655895979, -39.96870412324319943 ) ) ;
#58855 = ORIENTED_EDGE ( 'NONE', *, *, #57317, .T. ) ;
#58856 = CARTESIAN_POINT ( 'NONE',  ( 0.8557997880470690211, 46.03118133706043835, -13.27832040216591380 ) ) ;
#58857 = ADVANCED_FACE ( 'NONE', ( #53601 ), #47603, .F. ) ;
#58858 = B_SPLINE_CURVE_WITH_KNOTS ( 'NONE', 3,
 ( #278, #48236, #10023, #10640 ),
 .UNSPECIFIED., .F., .F.,
 ( 4, 4 ),
 ( 2.168404344971008868E-19, 0.004048833967417089091 ),
 .UNSPECIFIED. ) ;
#58859 = CARTESIAN_POINT ( 'NONE',  ( 0.1365634738349423838, -0.7775954032165560692, -44.11641378231173860 ) ) ;
#58860 = VERTEX_POINT ( 'NONE', #10416 ) ;
#58861 = B_SPLINE_CURVE_WITH_KNOTS ( 'NONE', 3,
 ( #3669, #60371, #12810, #50986, #27193, #3359 ),
 .UNSPECIFIED., .F., .F.,
 ( 4, 2, 4 ),
 ( 1.764953265579307567E-18, 0.0002450742804987336341, 0.0004901485609974654250 ),
 .UNSPECIFIED. ) ;
#58862 = VECTOR ( 'NONE', #59153, 1000.000000000000114 ) ;
#58863 = VECTOR ( 'NONE', #35581, 1000.000000000000114 ) ;
#58864 = ORIENTED_EDGE ( 'NONE', *, *, #56470, .T. ) ;
#58865 = CARTESIAN_POINT ( 'NONE',  ( 4.962356264823608143, 0.000000000000000000, 0.000000000000000000 ) ) ;
#58866 = ORIENTED_EDGE ( 'NONE', *, *, #11055, .T. ) ;
#58867 = CARTESIAN_POINT ( 'NONE',  ( 0.1129192098497455998, 30.02178898772931603, -32.33641869102712718 ) ) ;
#58868 = CARTESIAN_POINT ( 'NONE',  ( 0.7245667037590730608, 41.24129124474298180, -24.75815201345804084 ) ) ;
#58869 = ORIENTED_EDGE ( 'NONE', *, *, #15910, .F. ) ;
#58870 = PRODUCT_DEFINITION_SHAPE ( 'NONE', 'NONE',  #62001 ) ;
#58871 = ORIENTED_EDGE ( 'NONE', *, *, #23994, .F. ) ;
#58872 = CARTESIAN_POINT ( 'NONE',  ( 0.9762797500689124330, 20.58271139965541963, -36.50584578699964311 ) ) ;
#58873 = CARTESIAN_POINT ( 'NONE',  ( 5.958863334805807099, 5.313608583996519030, -19.82594244347347612 ) ) ;
#58874 = VERTEX_POINT ( 'NONE', #20428 ) ;
#58875 = VERTEX_POINT ( 'NONE', #48616 ) ;
#58876 = CARTESIAN_POINT ( 'NONE',  ( 4.960156602257180580, -41.40608197274622171, -20.99019478193095267 ) ) ;
#58877 = CARTESIAN_POINT ( 'NONE',  ( 4.694002226626921015, -34.93533603653879993, 29.28834354244447624 ) ) ;
#58878 = AXIS2_PLACEMENT_3D ( 'NONE', #36050, #11608, #59821 ) ;
#58879 = CARTESIAN_POINT ( 'NONE',  ( 0.6023142530420679819, 24.28014345169111365, 41.53076277789750037 ) ) ;
#58880 = DIRECTION ( 'NONE',  ( 0.07836865515943411409, -0.9608836331491542593, -0.2656332009267349248 ) ) ;
#58881 = ORIENTED_EDGE ( 'NONE', *, *, #58638, .F. ) ;
#58882 = ADVANCED_FACE ( 'NONE', ( #44263 ), #7138, .F. ) ;
#58883 = CARTESIAN_POINT ( 'NONE',  ( 0.8753041380234524160, -42.34096624980190171, 24.86726573039578980 ) ) ;
#58884 = ORIENTED_EDGE ( 'NONE', *, *, #15356, .F. ) ;
#58885 = CARTESIAN_POINT ( 'NONE',  ( -2.601141883200662974, -14.85441002404436439, -1.463533500456662306 ) ) ;
#58886 = EDGE_CURVE ( 'NONE', #30413, #40820, #60247, .T. ) ;
#58887 = ORIENTED_EDGE ( 'NONE', *, *, #59980, .F. ) ;
#58888 = PRODUCT_DEFINITION_FORMATION_WITH_SPECIFIED_SOURCE ( 'ANY', '', #8800, .NOT_KNOWN. ) ;
#58889 = CARTESIAN_POINT ( 'NONE',  ( 0.6067375320500723035, -47.57460111700601857, 5.548194933739998724 ) ) ;
#58890 = CARTESIAN_POINT ( 'NONE',  ( 1.227938101723756947, -20.72293514920776758, 37.58536632582772086 ) ) ;
#58891 = VERTEX_POINT ( 'NONE', #26355 ) ;
#58892 = CARTESIAN_POINT ( 'NONE',  ( 0.8751705887134553219, 5.393078191592700854, -47.79200036674274088 ) ) ;
#58893 = CARTESIAN_POINT ( 'NONE',  ( -6.078075953587585900, -14.66587681220008577, 12.47827037599793876 ) ) ;
#58894 = CARTESIAN_POINT ( 'NONE',  ( 51.67689044586143865, 12.27139102044969654, -2.380666987245603217 ) ) ;
#58895 = CARTESIAN_POINT ( 'NONE',  ( -19.96645934342861395, -12.48232314026188838, 0.6766079297640726908 ) ) ;
#58896 = EDGE_CURVE ( 'NONE', #35725, #7287, #58025, .T. ) ;
#58897 =( BOUNDED_SURFACE ( )  B_SPLINE_SURFACE ( 3, 1, ( 
 ( #16029, #49523 ),
 ( #39538, #16644 ),
 ( #54833, #30103 ),
 ( #11966, #2521 ) ),
 .UNSPECIFIED., .F., .F., .F. ) 
 B_SPLINE_SURFACE_WITH_KNOTS ( ( 4, 4 ),
 ( 2, 2 ),
 ( 0.000000000000000000, 1.000000000000000000 ),
 ( 0.000000000000000000, 1.000000000000000000 ),
 .UNSPECIFIED. ) 
 GEOMETRIC_REPRESENTATION_ITEM ( )  RATIONAL_B_SPLINE_SURFACE ( (
 ( 1.000000000000000000, 1.000000000000000000),
 ( 0.7211978278499968642, 0.9934217856018975334),
 ( 0.7211978278499968642, 0.9934217856018975334),
 ( 1.000000000000000000, 1.000000000000000000) ) ) 
 REPRESENTATION_ITEM ( '' )  SURFACE ( )  );
#58898 = ADVANCED_FACE ( 'NONE', ( #17281 ), #9559, .F. ) ;
#58899 = VERTEX_POINT ( 'NONE', #40187 ) ;
#58900 = CARTESIAN_POINT ( 'NONE',  ( 4.956653778116990594, -39.67974989265022145, -27.17045123668512474 ) ) ;
#58901 = EDGE_CURVE ( 'NONE', #20774, #58429, #21980, .T. ) ;
#58902 = CARTESIAN_POINT ( 'NONE',  ( 0.3676999524040323597, 39.37931578712994707, 19.88014264185084912 ) ) ;
#58903 = CARTESIAN_POINT ( 'NONE',  ( 0.9785694773339257413, 41.56380497646738803, -5.365214030479795504 ) ) ;
#58904 =( NAMED_UNIT ( * ) PLANE_ANGLE_UNIT ( ) SI_UNIT ( $, .RADIAN. ) );
#58905 = CARTESIAN_POINT ( 'NONE',  ( 0.8751705887134423323, 19.22545746485661766, -44.08562551107063143 ) ) ;
#58906 = EDGE_CURVE ( 'NONE', #44407, #50007, #37107, .T. ) ;
#58907 = CARTESIAN_POINT ( 'NONE',  ( 1.231276596079887264, -11.60895935156443848, 40.28037777618019533 ) ) ;
#58908 = CARTESIAN_POINT ( 'NONE',  ( 0.8560838555295158248, 43.53454501559585310, -17.46757637357826454 ) ) ;
#58909 =( BOUNDED_SURFACE ( )  B_SPLINE_SURFACE ( 3, 1, ( 
 ( #56742, #43296 ),
 ( #4716, #33895 ),
 ( #14475, #23863 ),
 ( #23247, #655 ) ),
 .UNSPECIFIED., .F., .F., .F. ) 
 B_SPLINE_SURFACE_WITH_KNOTS ( ( 4, 4 ),
 ( 2, 2 ),
 ( 0.000000000000000000, 1.000000000000000000 ),
 ( 0.000000000000000000, 1.000000000000000000 ),
 .UNSPECIFIED. ) 
 GEOMETRIC_REPRESENTATION_ITEM ( )  RATIONAL_B_SPLINE_SURFACE ( (
 ( 1.000000000000000000, 1.000000000000000000),
 ( 0.7269869731126821222, 0.9931720237060910339),
 ( 0.7269869731126821222, 0.9931720237060910339),
 ( 1.000000000000000000, 1.000000000000000000) ) ) 
 REPRESENTATION_ITEM ( '' )  SURFACE ( )  );
#58910 = AXIS2_PLACEMENT_3D ( 'NONE', #37478, #36865, #31519 ) ;
#58911 = CARTESIAN_POINT ( 'NONE',  ( -15.98127814905383026, -7.972271164889759731, -0.6777338475379729443 ) ) ;
#58912 = CARTESIAN_POINT ( 'NONE',  ( 4.291220156522059348, 41.58924158504531476, -22.12970812474565108 ) ) ;
#58913 =( BOUNDED_SURFACE ( )  B_SPLINE_SURFACE ( 3, 1, ( 
 ( #40912, #30851 ),
 ( #22386, #55263 ),
 ( #26778, #41517 ),
 ( #17086, #59658 ) ),
 .UNSPECIFIED., .F., .F., .F. ) 
 B_SPLINE_SURFACE_WITH_KNOTS ( ( 4, 4 ),
 ( 2, 2 ),
 ( 0.000000000000000000, 1.000000000000000000 ),
 ( 0.000000000000000000, 1.000000000000000000 ),
 .UNSPECIFIED. ) 
 GEOMETRIC_REPRESENTATION_ITEM ( )  RATIONAL_B_SPLINE_SURFACE ( (
 ( 1.000000000000000000, 1.000000000000000000),
 ( 0.7269869731126817891, 0.9931720237060910339),
 ( 0.7269869731126817891, 0.9931720237060910339),
 ( 1.000000000000000000, 1.000000000000000000) ) ) 
 REPRESENTATION_ITEM ( '' )  SURFACE ( )  );
#58914 = CARTESIAN_POINT ( 'NONE',  ( 0.2285344041767086998, -26.90972407420791868, 34.96237864541611629 ) ) ;
#58915 = B_SPLINE_CURVE_WITH_KNOTS ( 'NONE', 3,
 ( #14412, #5886, #10014, #52910, #33212, #4971 ),
 .UNSPECIFIED., .F., .F.,
 ( 4, 2, 4 ),
 ( 1.738108305489988542E-18, 0.0002291459268755710208, 0.0004582918537511403070 ),
 .UNSPECIFIED. ) ;
#58916 = CARTESIAN_POINT ( 'NONE',  ( 5.895596859100789899, 5.962379729972213660, -19.20880556328539512 ) ) ;
#58917 = CARTESIAN_POINT ( 'NONE',  ( 0.7048096507298579061, 28.61383451045646353, 38.67623024744057858 ) ) ;
#58918 = CONICAL_SURFACE ( 'NONE', #10933, 42.92674063221959813, 1.485477209440487556 ) ;
#58919 = FACE_OUTER_BOUND ( 'NONE', #24702, .T. ) ;
#58920 = CARTESIAN_POINT ( 'NONE',  ( 0.6027444965799114707, -45.56734243241186988, 18.30726138816941173 ) ) ;
#58921 = ORIENTED_EDGE ( 'NONE', *, *, #48651, .T. ) ;
#58922 = CIRCLE ( 'NONE', #56958, 2.099999999999999645 ) ;
#58923 = CARTESIAN_POINT ( 'NONE',  ( 1.657374760986086271, -2.648674067819503986, -43.97584533507803428 ) ) ;
#58924 = CARTESIAN_POINT ( 'NONE',  ( 3.661921753702003457, -36.12137287706547539, -30.13100637731890785 ) ) ;
#58925 = CARTESIAN_POINT ( 'NONE',  ( 0.6041374136657476912, 23.90252055111321638, -41.74951251761550708 ) ) ;
#58926 = VERTEX_POINT ( 'NONE', #12592 ) ;
#58927 = CARTESIAN_POINT ( 'NONE',  ( 4.975801465491694664, -21.70134120755230711, 42.71626295676225027 ) ) ;
#58928 = CARTESIAN_POINT ( 'NONE',  ( 0.1158516988532803521, 4.285932436189670014, 43.91552051365456322 ) ) ;
#58929 = ADVANCED_FACE ( 'NONE', ( #35470 ), #20347, .F. ) ;
#58930 = B_SPLINE_CURVE_WITH_KNOTS ( 'NONE', 3,
 ( #46570, #22749, #41882, #56248 ),
 .UNSPECIFIED., .F., .F.,
 ( 4, 4 ),
 ( 0.000000000000000000, 0.005013413432710143308 ),
 .UNSPECIFIED. ) ;
#58931 = DIRECTION ( 'NONE',  ( -1.836909530733573776E-16, 1.000000000000000000, 0.000000000000000000 ) ) ;
#58932 = ORIENTED_EDGE ( 'NONE', *, *, #38288, .T. ) ;
#58933 = ORIENTED_EDGE ( 'NONE', *, *, #17062, .T. ) ;
#58934 = VERTEX_POINT ( 'NONE', #27285 ) ;
#58935 = ADVANCED_FACE ( 'NONE', ( #49858 ), #45982, .F. ) ;
#58936 = CARTESIAN_POINT ( 'NONE',  ( 5.960721111146673579, 16.28018152803692686, -12.50019045452721222 ) ) ;
#58937 = VERTEX_POINT ( 'NONE', #52307 ) ;
#58938 = CARTESIAN_POINT ( 'NONE',  ( 1.227938101723748288, 29.74462687941226235, 30.94118573761323177 ) ) ;
#58939 = ORIENTED_EDGE ( 'NONE', *, *, #991, .T. ) ;
#58940 = ORIENTED_EDGE ( 'NONE', *, *, #35384, .F. ) ;
#58941 = CARTESIAN_POINT ( 'NONE',  ( 0.9968887458511672683, 25.59699785741785405, 34.43855515351779673 ) ) ;
#58942 = ORIENTED_EDGE ( 'NONE', *, *, #25040, .F. ) ;
#58943 = CARTESIAN_POINT ( 'NONE',  ( 42.00000000000000711, 0.000000000000000000, 0.000000000000000000 ) ) ;
#58944 = B_SPLINE_CURVE_WITH_KNOTS ( 'NONE', 3,
 ( #7293, #17346, #54915, #59622 ),
 .UNSPECIFIED., .F., .F.,
 ( 4, 4 ),
 ( 0.000000000000000000, 0.005013413432710151114 ),
 .UNSPECIFIED. ) ;
#58945 = CARTESIAN_POINT ( 'NONE',  ( 2.526464513654344213, -17.56107808841279194, -39.22765990515338785 ) ) ;
#58946 = ORIENTED_EDGE ( 'NONE', *, *, #15871, .F. ) ;
#58947 = CARTESIAN_POINT ( 'NONE',  ( 0.3676999524040323597, 37.41430475689418245, -23.36921870497780418 ) ) ;
#58948 = AXIS2_PLACEMENT_3D ( 'NONE', #25356, #20057, #30985 ) ;
#58949 = DIRECTION ( 'NONE',  ( -0.07906939808003035641, -0.04137963570463473045, -0.9960099176394847653 ) ) ;
#58950 = EDGE_LOOP ( 'NONE', ( #44887, #9829, #60128, #5360 ) ) ;
#58951 = CARTESIAN_POINT ( 'NONE',  ( 0.5997462898726536595, 27.66511329191589397, 40.57330571557817223 ) ) ;
#58952 = AXIS2_PLACEMENT_3D ( 'NONE', #2387, #20593, #16509 ) ;
#58953 = CARTESIAN_POINT ( 'NONE',  ( 1.231276596079881935, -37.02495017545860634, -19.65781868679418309 ) ) ;
#58954 = CARTESIAN_POINT ( 'NONE',  ( 5.917102823773431552, -4.653982686480137687, 19.56604618224349679 ) ) ;
#58955 = CARTESIAN_POINT ( 'NONE',  ( 0.3622758884714600280, 0.8252992914328071139, -43.10531414739104861 ) ) ;
#58956 = ORIENTED_EDGE ( 'NONE', *, *, #45842, .F. ) ;
#58957 = ORIENTED_EDGE ( 'NONE', *, *, #38018, .T. ) ;
#58958 = CARTESIAN_POINT ( 'NONE',  ( 4.956445790444004018, -46.73954499432459642, -5.740468958468717631 ) ) ;
#58959 = EDGE_CURVE ( 'NONE', #1414, #40743, #9445, .T. ) ;
#58960 = CARTESIAN_POINT ( 'NONE',  ( -6.015611763856276717, -16.31561949997069405, -9.427003116184344833 ) ) ;
#58961 = CARTESIAN_POINT ( 'NONE',  ( 4.975610109902397937, 30.04451009524474969, 38.59762713269442713 ) ) ;
#58962 = ORIENTED_EDGE ( 'NONE', *, *, #15032, .F. ) ;
#58963 = CARTESIAN_POINT ( 'NONE',  ( 0.5819845901640485764, -46.14435291605020950, -12.83441129068581965 ) ) ;
#58964 = CARTESIAN_POINT ( 'NONE',  ( 0.6000166863083106206, -25.01014854877471549, 42.26483113981026207 ) ) ;
#58965 = EDGE_CURVE ( 'NONE', #2384, #54909, #30410, .T. ) ;
#58966 = DIRECTION ( 'NONE',  ( 0.000000000000000000, 0.000000000000000000, 1.000000000000000000 ) ) ;
#58967 = CARTESIAN_POINT ( 'NONE',  ( 0.5998501479064699549, -41.92175333043603302, -23.59887241503339439 ) ) ;
#58968 = EDGE_CURVE ( 'NONE', #17224, #17545, #28204, .T. ) ;
#58969 = VECTOR ( 'NONE', #27362, 1000.000000000000000 ) ;
#58970 = ORIENTED_EDGE ( 'NONE', *, *, #18167, .T. ) ;
#58971 = VERTEX_POINT ( 'NONE', #47321 ) ;
#58972 = CARTESIAN_POINT ( 'NONE',  ( 4.834790513006555379, 7.085748555637797708, -46.71596631057371241 ) ) ;
#58973 = EDGE_CURVE ( 'NONE', #2634, #24857, #22885, .T. ) ;
#58974 = CARTESIAN_POINT ( 'NONE',  ( 4.975801465491694664, 43.22084481528220579, -20.67815041659094888 ) ) ;
#58975 = CARTESIAN_POINT ( 'NONE',  ( 0.8560838555295223751, 3.785103201470721768, -46.75516899590834186 ) ) ;
#58976 = CARTESIAN_POINT ( 'NONE',  ( 2.282816707992322058, 36.03600438247134008, -30.13143465808543553 ) ) ;
#58977 = CARTESIAN_POINT ( 'NONE',  ( 0.1087620492084205998, 34.43219573047432647, -25.96440931622094439 ) ) ;
#58978 = CARTESIAN_POINT ( 'NONE',  ( 0.1073791018717578927, -6.109314776653017809, 42.68962945260943087 ) ) ;
#58979 = CARTESIAN_POINT ( 'NONE',  ( 0.5850706913938534814, -44.31965802246092778, -18.16120156791927798 ) ) ;
#58980 = B_SPLINE_CURVE_WITH_KNOTS ( 'NONE', 3,
 ( #57906, #35692, #41023, #15955, #35069, #1828 ),
 .UNSPECIFIED., .F., .F.,
 ( 4, 2, 4 ),
 ( 8.560751122900633232E-17, 0.0002293366620881450389, 0.0004586733241762044801 ),
 .UNSPECIFIED. ) ;
#58981 = CARTESIAN_POINT ( 'NONE',  ( 4.956445790444040433, 44.65954324082233029, -14.93530206124928128 ) ) ;
#58982 = DIRECTION ( 'NONE',  ( 0.000000000000000000, 0.000000000000000000, -1.000000000000000000 ) ) ;
#58983 = EDGE_CURVE ( 'NONE', #45131, #5101, #14546, .T. ) ;
#58984 = LINE ( 'NONE', #25171, #27911 ) ;
#58985 = CARTESIAN_POINT ( 'NONE',  ( 0.6067099128993216350, -41.12102523654870367, 24.55985149487306529 ) ) ;
#58986 = EDGE_CURVE ( 'NONE', #1638, #54620, #43884, .T. ) ;
#58987 = LINE ( 'NONE', #2272, #49056 ) ;
#58988 = LINE ( 'NONE', #30791, #12137 ) ;
#58989 = CARTESIAN_POINT ( 'NONE',  ( 0.6017667736363748743, -46.55748817282783847, 12.11362382130055515 ) ) ;
#58990 = CARTESIAN_POINT ( 'NONE',  ( 4.962356264823591268, 23.01169039590626753, 35.23773124060775785 ) ) ;
#58991 = CARTESIAN_POINT ( 'NONE',  ( 0.9741495583595161101, -26.43366215195285562, 33.79932324264177623 ) ) ;
#58992 =( BOUNDED_SURFACE ( )  B_SPLINE_SURFACE ( 3, 1, ( 
 ( #6031, #16092 ),
 ( #2269, #24871 ),
 ( #48666, #25789 ),
 ( #53647, #58660 ) ),
 .UNSPECIFIED., .F., .F., .F. ) 
 B_SPLINE_SURFACE_WITH_KNOTS ( ( 4, 4 ),
 ( 2, 2 ),
 ( 0.000000000000000000, 1.000000000000000000 ),
 ( 0.000000000000000000, 1.000000000000000000 ),
 .UNSPECIFIED. ) 
 GEOMETRIC_REPRESENTATION_ITEM ( )  RATIONAL_B_SPLINE_SURFACE ( (
 ( 1.000000000000000000, 1.000000000000000000),
 ( 0.7269869731126817891, 0.9931720237060910339),
 ( 0.7269869731126817891, 0.9931720237060910339),
 ( 1.000000000000000000, 1.000000000000000000) ) ) 
 REPRESENTATION_ITEM ( '' )  SURFACE ( )  );
#58993 = CARTESIAN_POINT ( 'NONE',  ( 0.1103936448916665869, 5.228610780659758526E-15, -43.12443171339897674 ) ) ;
#58994 = LINE ( 'NONE', #58064, #55199 ) ;
#58995 = CARTESIAN_POINT ( 'NONE',  ( 0.6029443199889047422, 49.00651123133899034, -3.146346895535882648 ) ) ;
#58997 = ORIENTED_EDGE ( 'NONE', *, *, #55821, .F. ) ;
#58996 = CARTESIAN_POINT ( 'NONE',  ( 3.782625744892855302, 37.99690091417294013, -17.98537252918400853 ) ) ;
#58998 = VERTEX_POINT ( 'NONE', #4676 ) ;
#58999 = AXIS2_PLACEMENT_3D ( 'NONE', #32475, #13069, #42207 ) ;
#59000 = CARTESIAN_POINT ( 'NONE',  ( 2.281351352603291360, -46.66131639318007984, 11.14238889600268934 ) ) ;
#59001 = CARTESIAN_POINT ( 'NONE',  ( 4.390527457369402420, 43.61304121279572854, -5.299808751228768600 ) ) ;
#59002 = CARTESIAN_POINT ( 'NONE',  ( 4.956445790444005794, -27.49627641100061837, -38.22947597953034204 ) ) ;
#59003 = ORIENTED_EDGE ( 'NONE', *, *, #57142, .F. ) ;
#59004 = ORIENTED_EDGE ( 'NONE', *, *, #35384, .T. ) ;
#59005 = CARTESIAN_POINT ( 'NONE',  ( 3.783198216974389627, 40.39102707215877786, -14.86152287314638620 ) ) ;
#59006 = CARTESIAN_POINT ( 'NONE',  ( 2.281351352603298022, 25.11567449372765637, -40.87339198768968629 ) ) ;
#59007 = CARTESIAN_POINT ( 'NONE',  ( 0.6027935024548037868, 6.106197519200845747, 47.71838037711336256 ) ) ;
#59008 = ORIENTED_EDGE ( 'NONE', *, *, #18067, .F. ) ;
#59009 = ORIENTED_EDGE ( 'NONE', *, *, #19937, .F. ) ;
#59010 = ADVANCED_FACE ( 'NONE', ( #37024 ), #45599, .F. ) ;
#59011 = CARTESIAN_POINT ( 'NONE',  ( 0.6023142530420679819, -24.28014345169140498, -41.53076277789733695 ) ) ;
#59012 = CARTESIAN_POINT ( 'NONE',  ( 0.9268187852002115479, -40.48348757851531587, 17.45971266627324425 ) ) ;
#59013 = CARTESIAN_POINT ( 'NONE',  ( 0.5832655196449151314, -38.53372662657736925, -26.72802078795826830 ) ) ;
#59014 = CARTESIAN_POINT ( 'NONE',  ( 0.5980271706414734822, 49.05158475245161043, 2.447708339390032517 ) ) ;
#59015 = ORIENTED_EDGE ( 'NONE', *, *, #40897, .F. ) ;
#59016 = CARTESIAN_POINT ( 'NONE',  ( 0.1368894036331282649, 4.870979158004423937, 43.85356186178748317 ) ) ;
#59017 = CARTESIAN_POINT ( 'NONE',  ( 0.5809828226811553087, 6.791453954330313181, 47.41188724015881917 ) ) ;
#59018 = CARTESIAN_POINT ( 'NONE',  ( 3.376099380956838925, -7.596917057716860100, 11.04514530688653906 ) ) ;
#59019 = ORIENTED_EDGE ( 'NONE', *, *, #9656, .T. ) ;
#59020 = EDGE_LOOP ( 'NONE', ( #16604, #54368, #28355, #19592, #51154 ) ) ;
#59021 = CARTESIAN_POINT ( 'NONE',  ( 0.3676999524040366896, 34.11874447324979087, 27.96179284115963171 ) ) ;
#59022 = CARTESIAN_POINT ( 'NONE',  ( 0.1119899015040009271, -40.68569793094620479, -17.07733269759378203 ) ) ;
#59023 = ORIENTED_EDGE ( 'NONE', *, *, #3108, .F. ) ;
#59024 = CARTESIAN_POINT ( 'NONE',  ( 0.5838002273316442725, 44.30203797796963272, -18.20308624554782639 ) ) ;
#59025 = CARTESIAN_POINT ( 'NONE',  ( 0.7954190325252775695, 44.76287681188606626, 17.60078418395009336 ) ) ;
#59026 = CARTESIAN_POINT ( 'NONE',  ( 5.896278296736517710, 8.461230214158247165, -18.24649453668839172 ) ) ;
#59027 = CARTESIAN_POINT ( 'NONE',  ( 0.6253024248130485407, -8.514605087301925224, 48.36264806257963755 ) ) ;
#59028 = VERTEX_POINT ( 'NONE', #61088 ) ;
#59029 = CARTESIAN_POINT ( 'NONE',  ( 0.5837799406558239479, 46.46543369090721853, -6.340900684690216060 ) ) ;
#59030 = CARTESIAN_POINT ( 'NONE',  ( 3.661921753702033655, 46.33057357019549016, -8.130748827183058580 ) ) ;
#59031 = CARTESIAN_POINT ( 'NONE',  ( 4.962356264823608143, -25.31392337492896161, 33.62202970123266965 ) ) ;
#59032 = ORIENTED_EDGE ( 'NONE', *, *, #40847, .F. ) ;
#59033 = FACE_OUTER_BOUND ( 'NONE', #8742, .T. ) ;
#59034 = EDGE_CURVE ( 'NONE', #37250, #45271, #36547, .T. ) ;
#59035 = DIRECTION ( 'NONE',  ( -1.000000000000000000, -1.836909530733573776E-16, -1.361838123766432833E-32 ) ) ;
#59036 = ORIENTED_EDGE ( 'NONE', *, *, #45144, .F. ) ;
#59037 = CARTESIAN_POINT ( 'NONE',  ( -5.331200000000000827, 0.000000000000000000, 0.000000000000000000 ) ) ;
#59038 = CARTESIAN_POINT ( 'NONE',  ( 5.860006189529234355, -43.26650951066853423, -21.31760477694627554 ) ) ;
#59039 = ORIENTED_EDGE ( 'NONE', *, *, #3890, .T. ) ;
#59040 = CARTESIAN_POINT ( 'NONE',  ( 10.00000000000000888, 0.000000000000000000, 0.000000000000000000 ) ) ;
#59041 = ADVANCED_FACE ( 'NONE', ( #24742 ), #52303, .F. ) ;
#59042 = CARTESIAN_POINT ( 'NONE',  ( 3.238931869106854489, -19.89273896137509823, 38.11291514434407901 ) ) ;
#59043 = CARTESIAN_POINT ( 'NONE',  ( 0.9762797500689124330, 36.31338395866826829, -20.92039508843077300 ) ) ;
#59044 = B_SPLINE_CURVE_WITH_KNOTS ( 'NONE', 3,
 ( #14438, #53239, #9402, #33546 ),
 .UNSPECIFIED., .F., .F.,
 ( 4, 4 ),
 ( 4.234999717485957107E-17, 0.005004948556313839128 ),
 .UNSPECIFIED. ) ;
#59045 = CARTESIAN_POINT ( 'NONE',  ( -6.001507490154111224, 18.84387066167321478, 0.01557731607559981711 ) ) ;
#59046 = CARTESIAN_POINT ( 'NONE',  ( 0.5809828226811544205, 5.711058609466008740, -47.55412398569200150 ) ) ;
#59047 = CLOSED_SHELL ( 'NONE', ( #30445, #36091, #4557, #7557, #47208, #776, #59055, #19626, #35937, #43467, #5039, #42304, #37351, #13523, #60108, #58768, #31332, #26035, #15582, #13344, #25536, #9457, #50148, #43080, #54197, #39403, #53391, #16641 ) ) ;
#59048 = CARTESIAN_POINT ( 'NONE',  ( 0.5827359174754830340, 46.35666395585288058, -12.04517879102088429 ) ) ;
#59049 = CARTESIAN_POINT ( 'NONE',  ( 4.975801465491695552, 20.67815041659141784, -43.22084481528199973 ) ) ;
#59050 = CARTESIAN_POINT ( 'NONE',  ( 1.834102595619085285, -32.53417647307985305, -29.69385636922530125 ) ) ;
#59051 = CARTESIAN_POINT ( 'NONE',  ( 4.335381028904216727, -15.96267600302249612, -46.31360299617030307 ) ) ;
#59052 = DIRECTION ( 'NONE',  ( 0.000000000000000000, 0.000000000000000000, 1.000000000000000000 ) ) ;
#59053 = CARTESIAN_POINT ( 'NONE',  ( 0.9789889208857684988, 15.15199999899948935, 39.07367136669768115 ) ) ;
#59054 = VECTOR ( 'NONE', #51429, 1000.000000000000000 ) ;
#59056 = EDGE_LOOP ( 'NONE', ( #28265, #47742, #34223, #568 ) ) ;
#59055 = ADVANCED_FACE ( 'NONE', ( #38869 ), #28500, .T. ) ;
#59057 = CARTESIAN_POINT ( 'NONE',  ( -6.079354080745853928, -14.66314846858170462, 12.48138743235270454 ) ) ;
#59059 = EDGE_CURVE ( 'NONE', #38660, #31310, #59542, .T. ) ;
#59058 = CARTESIAN_POINT ( 'NONE',  ( 0.8557997880470697982, -13.27832040216607190, -46.03118133706039572 ) ) ;
#59060 = CARTESIAN_POINT ( 'NONE',  ( 0.1156867017252034280, 44.04134645836630568, -2.702334066937902346 ) ) ;
#59061 = CARTESIAN_POINT ( 'NONE',  ( 0.5850706913938534814, 41.38834827854241638, -24.10530971368245190 ) ) ;
#59062 = DIRECTION ( 'NONE',  ( -1.000000000000000000, -0.000000000000000000, -0.000000000000000000 ) ) ;
#59063 = DIRECTION ( 'NONE',  ( -1.000000000000000000, -5.380183451256501876E-17, 1.298891185607916501E-16 ) ) ;
#59064 = CARTESIAN_POINT ( 'NONE',  ( 4.291220156522060236, 24.50578158393188843, 40.23500548361242579 ) ) ;
#59065 = LINE ( 'NONE', #40013, #28726 ) ;
#59066 = CARTESIAN_POINT ( 'NONE',  ( 4.956445790443998689, -4.175462451062247560, 46.90526157542890218 ) ) ;
#59068 = VERTEX_POINT ( 'NONE', #29129 ) ;
#59067 = CARTESIAN_POINT ( 'NONE',  ( -5.995132425357893702, -7.203480333239202338, 17.41298668506968284 ) ) ;
#59069 = ORIENTED_EDGE ( 'NONE', *, *, #30924, .F. ) ;
#59070 = CARTESIAN_POINT ( 'NONE',  ( 4.303969348037258058, -40.54345935592797900, 25.89994482339355386 ) ) ;
#59071 = B_SPLINE_CURVE_WITH_KNOTS ( 'NONE', 3,
 ( #41367, #41671, #3413, #40760 ),
 .UNSPECIFIED., .F., .F.,
 ( 4, 4 ),
 ( 0.000000000000000000, 0.004442905043737215703 ),
 .UNSPECIFIED. ) ;
#59072 = CARTESIAN_POINT ( 'NONE',  ( 3.407937589446174087, -13.69123696618924058, -0.4592810312473414314 ) ) ;
#59073 = CARTESIAN_POINT ( 'NONE',  ( 0.2940135542859014794, -42.87040774429959100, -10.41002826744088772 ) ) ;
#59074 = B_SPLINE_CURVE_WITH_KNOTS ( 'NONE', 3,
 ( #38697, #33993, #34598, #24887, #29882, #15187 ),
 .UNSPECIFIED., .F., .F.,
 ( 4, 2, 4 ),
 ( 1.764953265579307567E-18, 0.0002450742804987336341, 0.0004901485609974654250 ),
 .UNSPECIFIED. ) ;
#59075 = ORIENTED_EDGE ( 'NONE', *, *, #58901, .F. ) ;
#59076 = DIRECTION ( 'NONE',  ( -1.000000000000000000, 0.000000000000000000, 0.000000000000000000 ) ) ;
#59077 = CARTESIAN_POINT ( 'NONE',  ( 4.967162193818130511, -42.34252806656598977, 7.970725651239652265 ) ) ;
#59078 = CARTESIAN_POINT ( 'NONE',  ( 0.6001305935487422083, 37.84751346122855864, -29.70149728382397569 ) ) ;
#59079 = ORIENTED_EDGE ( 'NONE', *, *, #57749, .T. ) ;
#59080 = ORIENTED_EDGE ( 'NONE', *, *, #51270, .F. ) ;
#59081 = ADVANCED_FACE ( 'NONE', ( #43882 ), #22352, .F. ) ;
#59082 = CARTESIAN_POINT ( 'NONE',  ( 0.3676999524040366896, -0.5887207181726206162, 44.10900124961835900 ) ) ;
#59083 = CARTESIAN_POINT ( 'NONE',  ( 0.1100053167205930493, -39.91014771056767074, -16.33707796615692587 ) ) ;
#59084 = CARTESIAN_POINT ( 'NONE',  ( 0.6029443199889047422, 37.39265412695906576, 31.83279848200615803 ) ) ;
#59085 = ORIENTED_EDGE ( 'NONE', *, *, #5654, .T. ) ;
#59086 = B_SPLINE_CURVE_WITH_KNOTS ( 'NONE', 3,
 ( #44226, #1254, #24463, #5026 ),
 .UNSPECIFIED., .F., .F.,
 ( 4, 4 ),
 ( 1.962615573354719267E-17, 0.005004741218457437087 ),
 .UNSPECIFIED. ) ;
#59087 = CARTESIAN_POINT ( 'NONE',  ( 4.967162193818130511, 28.07411493385295032, 32.68434214048178177 ) ) ;
#59088 = CARTESIAN_POINT ( 'NONE',  ( 0.7954190325252775695, -11.60747917225617165, 46.67728753507120842 ) ) ;
#59089 = ORIENTED_EDGE ( 'NONE', *, *, #28002, .T. ) ;
#59090 = VECTOR ( 'NONE', #35478, 1000.000000000000114 ) ;
#59091 = CARTESIAN_POINT ( 'NONE',  ( -6.079354080745853928, 5.477739963081766916, 18.46042578449963756 ) ) ;
#59092 = CARTESIAN_POINT ( 'NONE',  ( 0.6000166863083090663, 23.17738933882476360, 43.29702189695021275 ) ) ;
#59093 = VERTEX_POINT ( 'NONE', #9713 ) ;
#59094 = B_SPLINE_CURVE_WITH_KNOTS ( 'NONE', 3,
 ( #37758, #14248, #47438, #24236, #19868, #10457 ),
 .UNSPECIFIED., .F., .F.,
 ( 4, 2, 4 ),
 ( 7.007167689862070887E-18, 0.0002448709889506557472, 0.0004897419779013045555 ),
 .UNSPECIFIED. ) ;
#59095 = CARTESIAN_POINT ( 'NONE',  ( 0.5837800304671217910, -34.81104335575551545, 31.42337653186251600 ) ) ;
#59096 = DIRECTION ( 'NONE',  ( 0.000000000000000000, 0.000000000000000000, 1.000000000000000000 ) ) ;
#59097 = VERTEX_POINT ( 'NONE', #4672 ) ;
#59098 = CARTESIAN_POINT ( 'NONE',  ( 0.6000166863083106206, -8.353387137038087218, -48.39467331274403961 ) ) ;
#59099 = CARTESIAN_POINT ( 'NONE',  ( 4.553261556744875094, -3.993093339916522488, -43.74465420371214464 ) ) ;
#59100 = CARTESIAN_POINT ( 'NONE',  ( 0.5809828226811553087, 41.20389530892342833, -24.41822904836879715 ) ) ;
#59101 = ORIENTED_EDGE ( 'NONE', *, *, #44581, .T. ) ;
#59102 = CARTESIAN_POINT ( 'NONE',  ( 4.549368137175248350, 0.000000000000000000, 0.000000000000000000 ) ) ;
#59103 = CARTESIAN_POINT ( 'NONE',  ( 0.6030672727741701600, 44.47882233696923038, -18.32928433899707343 ) ) ;
#59104 = ORIENTED_EDGE ( 'NONE', *, *, #48234, .T. ) ;
#59105 = CARTESIAN_POINT ( 'NONE',  ( 4.975801465491695552, -42.71626295676279028, 21.70134120755125906 ) ) ;
#59106 =( BOUNDED_SURFACE ( )  B_SPLINE_SURFACE ( 3, 1, ( 
 ( #50635, #41581 ),
 ( #27772, #12772 ),
 ( #26847, #32799 ),
 ( #7725, #60045 ) ),
 .UNSPECIFIED., .F., .F., .F. ) 
 B_SPLINE_SURFACE_WITH_KNOTS ( ( 4, 4 ),
 ( 2, 2 ),
 ( 0.000000000000000000, 1.000000000000000000 ),
 ( 0.000000000000000000, 1.000000000000000000 ),
 .UNSPECIFIED. ) 
 GEOMETRIC_REPRESENTATION_ITEM ( )  RATIONAL_B_SPLINE_SURFACE ( (
 ( 1.000000000000000000, 1.000000000000000000),
 ( 0.9751682680413298332, 0.9999560080971552356),
 ( 0.9751682680413298332, 0.9999560080971552356),
 ( 1.000000000000000000, 1.000000000000000000) ) ) 
 REPRESENTATION_ITEM ( '' )  SURFACE ( )  );
#59107 = ORIENTED_EDGE ( 'NONE', *, *, #16655, .F. ) ;
#59108 = CARTESIAN_POINT ( 'NONE',  ( 0.9791128995231623833, 4.199954538575370044, 41.69769557325756182 ) ) ;
#59109 = EDGE_CURVE ( 'NONE', #15825, #57224, #33446, .T. ) ;
#59110 = EDGE_LOOP ( 'NONE', ( #21123, #135, #55114, #3176 ) ) ;
#59111 = CARTESIAN_POINT ( 'NONE',  ( 2.528190830796659405, -40.87987336052400167, -9.544112854557406322 ) ) ;
#59112 = CARTESIAN_POINT ( 'NONE',  ( 0.6008122571543325074, -30.95730573212618353, -38.12085744409461796 ) ) ;
#59113 = CARTESIAN_POINT ( 'NONE',  ( 0.8554163680231738898, -45.78608427674269166, -10.23913862172186917 ) ) ;
#59114 = VERTEX_POINT ( 'NONE', #19139 ) ;
#59115 = CARTESIAN_POINT ( 'NONE',  ( 0.5827357941260221663, 6.611647889511194087, 47.43746130990116683 ) ) ;
#59116 = EDGE_CURVE ( 'NONE', #27605, #38027, #23818, .T. ) ;
#59117 = CARTESIAN_POINT ( 'NONE',  ( 0.8560838555295223751, -42.27062166135446120, -20.33635607586480631 ) ) ;
#59118 = ORIENTED_EDGE ( 'NONE', *, *, #329, .F. ) ;
#59119 = B_SPLINE_CURVE_WITH_KNOTS ( 'NONE', 3,
 ( #40792, #26653, #21966, #46098, #60156, #8158 ),
 .UNSPECIFIED., .F., .F.,
 ( 4, 2, 4 ),
 ( 1.268664800107929448E-16, 0.0002450741128632350527, 0.0004901482257263432537 ),
 .UNSPECIFIED. ) ;
#59120 = EDGE_CURVE ( 'NONE', #30566, #60037, #59474, .T. ) ;
#59121 = ORIENTED_EDGE ( 'NONE', *, *, #24811, .F. ) ;
#59122 = DIRECTION ( 'NONE',  ( -1.000000000000000000, -0.000000000000000000, -0.000000000000000000 ) ) ;
#59123 = CARTESIAN_POINT ( 'NONE',  ( 2.879087469061462734, 30.84090478284358383, 31.38375804391427337 ) ) ;
#59124 = CARTESIAN_POINT ( 'NONE',  ( 4.553261556744875094, 22.96401893593780841, -37.44587293859667199 ) ) ;
#59125 = CARTESIAN_POINT ( 'NONE',  ( 0.1092565886968785704, -5.936467125236737807, -42.71401356099877233 ) ) ;
#59126 = CARTESIAN_POINT ( 'NONE',  ( 0.5817216825391123836, -30.62363842979834772, -35.51658375362750064 ) ) ;
#59127 = CARTESIAN_POINT ( 'NONE',  ( 0.9790320750461890542, 38.54957592690705326, 16.43980925673472981 ) ) ;
#59128 = VERTEX_POINT ( 'NONE', #20360 ) ;
#59129 = CARTESIAN_POINT ( 'NONE',  ( 1.231276596079881047, -21.83837404314779462, -35.78214904347746739 ) ) ;
#59130 = CARTESIAN_POINT ( 'NONE',  ( 3.680882792899938138, 14.19444521819966631, 45.82784180332843249 ) ) ;
#59131 = ORIENTED_EDGE ( 'NONE', *, *, #4629, .T. ) ;
#59132 = CARTESIAN_POINT ( 'NONE',  ( 0.7948878604505664747, -34.66113263096703179, 34.77505617589897469 ) ) ;
#59134 = ADVANCED_FACE ( 'NONE', ( #25051 ), #29739, .T. ) ;
#59133 = CARTESIAN_POINT ( 'NONE',  ( 0.6026777506516367566, -20.03705103671176602, -44.83372588118711377 ) ) ;
#59135 = CARTESIAN_POINT ( 'NONE',  ( 0.5807400328401637335, 24.41979442053227700, -41.20655774452942666 ) ) ;
#59136 = B_SPLINE_CURVE_WITH_KNOTS ( 'NONE', 3,
 ( #51159, #46490, #12987, #8242 ),
 .UNSPECIFIED., .F., .F.,
 ( 4, 4 ),
 ( 2.069917718005272729E-17, 0.004444306975806117631 ),
 .UNSPECIFIED. ) ;
#59137 = CARTESIAN_POINT ( 'NONE',  ( -6.079354080745853928, 18.62591919961139197, -4.885497847477741296 ) ) ;
#59138 = CARTESIAN_POINT ( 'NONE',  ( 2.282816707992322947, 39.73059989313451723, -25.05945726745943958 ) ) ;
#59139 = CARTESIAN_POINT ( 'NONE',  ( -2.708315649062910779, 14.47261168455366942, 2.171184472130732956 ) ) ;
#59140 = CIRCLE ( 'NONE', #25118, 2.649999999999997691 ) ;
#59141 = CARTESIAN_POINT ( 'NONE',  ( 0.5997462898726536595, 37.72933316222010802, -31.43324751403371664 ) ) ;
#59142 = CARTESIAN_POINT ( 'NONE',  ( 0.7762783648524369529, -5.369627767360159787, 47.60264408896662047 ) ) ;
#59143 = CARTESIAN_POINT ( 'NONE',  ( 4.975801465491694664, 20.67815041659077835, 43.22084481528228395 ) ) ;
#59144 = CARTESIAN_POINT ( 'NONE',  ( -6.016761891674565099, -18.20201388312099056, 4.873659902332302174 ) ) ;
#59145 = B_SPLINE_CURVE_WITH_KNOTS ( 'NONE', 3,
 ( #38086, #8372, #15183, #39005, #10165, #38692 ),
 .UNSPECIFIED., .F., .F.,
 ( 4, 2, 4 ),
 ( 2.693102327163510278E-18, 0.0002447193893791690575, 0.0004894387787583354046 ),
 .UNSPECIFIED. ) ;
#59146 = DIRECTION ( 'NONE',  ( -1.000000000000000000, -3.135800716341489291E-16, 1.298891185607901956E-16 ) ) ;
#59147 = CARTESIAN_POINT ( 'NONE',  ( 0.9788927965476029724, 9.853064299072418208, 40.73393838741991146 ) ) ;
#59148 = B_SPLINE_CURVE_WITH_KNOTS ( 'NONE', 3,
 ( #34222, #24494, #43633, #33917, #39548, #15733 ),
 .UNSPECIFIED., .F., .F.,
 ( 4, 2, 4 ),
 ( 6.619851161367215630E-18, 0.0002291472222819930168, 0.0004582944445639794201 ),
 .UNSPECIFIED. ) ;
#59149 = CARTESIAN_POINT ( 'NONE',  ( -90.00000000000000000, 0.000000000000000000, 0.000000000000000000 ) ) ;
#59150 = CARTESIAN_POINT ( 'NONE',  ( 4.975610109902397937, -33.30777373088848492, -35.81957029655308133 ) ) ;
#59151 = ORIENTED_EDGE ( 'NONE', *, *, #44542, .F. ) ;
#59152 = CARTESIAN_POINT ( 'NONE',  ( -31.75000000000000000, 0.000000000000000000, 0.000000000000000000 ) ) ;
#59153 = DIRECTION ( 'NONE',  ( 0.09835009131224567436, -0.9632152266566440524, 0.2500873580884542813 ) ) ;
#59154 = CARTESIAN_POINT ( 'NONE',  ( 0.9740398440564311811, -39.79907313245119838, -16.03656236596792084 ) ) ;
#59155 = CARTESIAN_POINT ( 'NONE',  ( 0.5804410086790514622, 32.99440095574044562, -33.33000686209396690 ) ) ;
#59156 = CARTESIAN_POINT ( 'NONE',  ( 0.1100053167205930910, -41.60823192620016187, 11.33468317718483753 ) ) ;
#59157 = ORIENTED_EDGE ( 'NONE', *, *, #21194, .F. ) ;
#59158 = EDGE_CURVE ( 'NONE', #2547, #11109, #49842, .T. ) ;
#59159 = CARTESIAN_POINT ( 'NONE',  ( 1.000110580585050313, -0.7426652321698243853, -41.90305395940526267 ) ) ;
#59160 = DIRECTION ( 'NONE',  ( 0.1024043820194936449, -0.3927886084231637098, -0.9139094329506617376 ) ) ;
#59161 = EDGE_CURVE ( 'NONE', #35339, #55095, #10032, .T. ) ;
#59162 = B_SPLINE_CURVE_WITH_KNOTS ( 'NONE', 3,
 ( #42261, #15202, #18432, #34310 ),
 .UNSPECIFIED., .F., .F.,
 ( 4, 4 ),
 ( 0.000000000000000000, 0.005004741218457402392 ),
 .UNSPECIFIED. ) ;
#59163 =( BOUNDED_SURFACE ( )  B_SPLINE_SURFACE ( 3, 1, ( 
 ( #2943, #37115 ),
 ( #60256, #36490 ),
 ( #27692, #50869 ),
 ( #27071, #56184 ) ),
 .UNSPECIFIED., .F., .F., .F. ) 
 B_SPLINE_SURFACE_WITH_KNOTS ( ( 4, 4 ),
 ( 2, 2 ),
 ( 0.000000000000000000, 1.000000000000000000 ),
 ( 0.000000000000000000, 1.000000000000000000 ),
 .UNSPECIFIED. ) 
 GEOMETRIC_REPRESENTATION_ITEM ( )  RATIONAL_B_SPLINE_SURFACE ( (
 ( 1.000000000000000000, 1.000000000000000000),
 ( 0.9729067724841187204, 0.9999501103223794596),
 ( 0.9729067724841187204, 0.9999501103223794596),
 ( 1.000000000000000000, 1.000000000000000000) ) ) 
 REPRESENTATION_ITEM ( '' )  SURFACE ( )  );
#59164 = CARTESIAN_POINT ( 'NONE',  ( 4.962356264823597485, -14.71877352713633158, 39.42833123173257803 ) ) ;
#59165 = VERTEX_POINT ( 'NONE', #38249 ) ;
#59166 = LINE ( 'NONE', #20669, #9023 ) ;
#59167 = ADVANCED_FACE ( 'NONE', ( #289 ), #11570, .F. ) ;
#59168 = CARTESIAN_POINT ( 'NONE',  ( 1.231276596079887264, 20.88402890667827450, 36.34740854095507245 ) ) ;
#59169 = ORIENTED_EDGE ( 'NONE', *, *, #5891, .T. ) ;
#59170 = CARTESIAN_POINT ( 'NONE',  ( -3.514385190458188646, -13.03453477240703862, 0.000000000000000000 ) ) ;
#59171 = VERTEX_POINT ( 'NONE', #2460 ) ;
#59172 = CARTESIAN_POINT ( 'NONE',  ( 5.960721111146673579, 12.49016043756471284, -16.28787783074214701 ) ) ;
#59173 = ORIENTED_EDGE ( 'NONE', *, *, #28172, .F. ) ;
#59174 = CARTESIAN_POINT ( 'NONE',  ( 5.981074661064941900, 14.50705827991446029, -14.51919955600720513 ) ) ;
#59175 = CARTESIAN_POINT ( 'NONE',  ( 0.5850706913938534814, 41.56998471741228229, 23.79070617305396240 ) ) ;
#59176 = VERTEX_POINT ( 'NONE', #49467 ) ;
#59177 = CIRCLE ( 'NONE', #18200, 43.92652462719577500 ) ;
#59178 = EDGE_LOOP ( 'NONE', ( #15132, #691, #3535, #3080, #48380 ) ) ;
#59179 = FACE_OUTER_BOUND ( 'NONE', #33464, .T. ) ;
#59180 = DIRECTION ( 'NONE',  ( 0.000000000000000000, 0.000000000000000000, 1.000000000000000000 ) ) ;
#59181 =( BOUNDED_SURFACE ( )  B_SPLINE_SURFACE ( 3, 1, ( 
 ( #30888, #2372 ),
 ( #29970, #35302 ),
 ( #12122, #50004 ),
 ( #53746, #21491 ) ),
 .UNSPECIFIED., .F., .F., .F. ) 
 B_SPLINE_SURFACE_WITH_KNOTS ( ( 4, 4 ),
 ( 2, 2 ),
 ( 0.000000000000000000, 1.000000000000000000 ),
 ( 0.000000000000000000, 1.000000000000000000 ),
 .UNSPECIFIED. ) 
 GEOMETRIC_REPRESENTATION_ITEM ( )  RATIONAL_B_SPLINE_SURFACE ( (
 ( 1.000000000000000000, 1.000000000000000000),
 ( 0.9953390228620291325, 0.8624445117760984880),
 ( 0.9953390228620291325, 0.8624445117760984880),
 ( 1.000000000000000000, 1.000000000000000000) ) ) 
 REPRESENTATION_ITEM ( '' )  SURFACE ( )  );
#59182 = AXIS2_PLACEMENT_3D ( 'NONE', #32763, #60936, #18359 ) ;
#59183 = ORIENTED_EDGE ( 'NONE', *, *, #16413, .T. ) ;
#59184 = EDGE_CURVE ( 'NONE', #8307, #50661, #7458, .T. ) ;
#59185 = ORIENTED_EDGE ( 'NONE', *, *, #3762, .T. ) ;
#59186 = CARTESIAN_POINT ( 'NONE',  ( 5.901764892641288895, 13.89173340561033676, -46.95754689533012538 ) ) ;
#59187 = LINE ( 'NONE', #20378, #29374 ) ;
#59188 = CARTESIAN_POINT ( 'NONE',  ( 0.5827357941260210561, 33.60975216782532016, -34.12346967353423821 ) ) ;
#59189 = CARTESIAN_POINT ( 'NONE',  ( 0.5824935313925951874, 32.33894943514273734, -33.96219260420503616 ) ) ;
#59190 = FACE_OUTER_BOUND ( 'NONE', #12563, .T. ) ;
#59191 = ORIENTED_EDGE ( 'NONE', *, *, #28786, .T. ) ;
#59192 = LINE ( 'NONE', #53868, #42668 ) ;
#59193 = CARTESIAN_POINT ( 'NONE',  ( 0.8753041380234471980, -38.81339214172277963, -30.07754840950027386 ) ) ;
#59194 = ORIENTED_EDGE ( 'NONE', *, *, #16479, .T. ) ;
#59195 = DIRECTION ( 'NONE',  ( 0.000000000000000000, 0.000000000000000000, 1.000000000000000000 ) ) ;
#59196 = EDGE_CURVE ( 'NONE', #7974, #40686, #57517, .T. ) ;
#59197 = ORIENTED_EDGE ( 'NONE', *, *, #58523, .T. ) ;
#59198 = CARTESIAN_POINT ( 'NONE',  ( 4.956653778116981712, -42.88673967249145846, 21.75875759808692322 ) ) ;
#59199 = CARTESIAN_POINT ( 'NONE',  ( 0.9762797500689124330, -22.97506929404158171, -35.04955029839458547 ) ) ;
#59200 = ORIENTED_EDGE ( 'NONE', *, *, #19156, .F. ) ;
#59201 = CARTESIAN_POINT ( 'NONE',  ( 0.5998501479064708430, 38.48283596222029956, -28.86886762351084812 ) ) ;
#59202 = CARTESIAN_POINT ( 'NONE',  ( 0.7044674535453004927, -14.77841640690436620, -46.83376059334811004 ) ) ;
#59203 = DIRECTION ( 'NONE',  ( -0.07836865515943411409, -0.1223011693452919629, 0.9893941468723553845 ) ) ;
#59204 = DIRECTION ( 'NONE',  ( 1.000000000000000000, 0.000000000000000000, 0.000000000000000000 ) ) ;
#59205 = ORIENTED_EDGE ( 'NONE', *, *, #25338, .T. ) ;
#59206 = FACE_OUTER_BOUND ( 'NONE', #9350, .T. ) ;
#59207 = ORIENTED_EDGE ( 'NONE', *, *, #30614, .T. ) ;
#59208 = CARTESIAN_POINT ( 'NONE',  ( 1.827119703190779765, 31.30004882613801698, 29.55676396270195738 ) ) ;
#59210 = EDGE_CURVE ( 'NONE', #35184, #33035, #12467, .T. ) ;
#59209 = CARTESIAN_POINT ( 'NONE',  ( 0.9783242366443571925, 41.56959898774839246, -5.320049830998810236 ) ) ;
#59211 =( NAMED_UNIT ( * ) SI_UNIT ( $, .STERADIAN. ) SOLID_ANGLE_UNIT ( ) );
#59212 = CARTESIAN_POINT ( 'NONE',  ( 5.910764540655178756, 17.94353875551737332, -9.084638429701483275 ) ) ;
#59213 = CARTESIAN_POINT ( 'NONE',  ( -6.063463321072276813, 0.6327935495816255917, 19.24629898975586428 ) ) ;
#59214 = DIRECTION ( 'NONE',  ( 0.000000000000000000, 0.000000000000000000, 1.000000000000000000 ) ) ;
#59215 = CARTESIAN_POINT ( 'NONE',  ( 4.553261556744873317, -43.85016385001095074, -2.588956575693968976 ) ) ;
#59216 = CARTESIAN_POINT ( 'NONE',  ( 0.5806925824938499181, -30.69245420804209701, 35.45695442407318154 ) ) ;
#59217 = FACE_OUTER_BOUND ( 'NONE', #23278, .T. ) ;
#59218 = CARTESIAN_POINT ( 'NONE',  ( 5.959547316686252039, -19.82530672674358385, -5.315863417546260905 ) ) ;
#59219 = AXIS2_PLACEMENT_3D ( 'NONE', #35137, #53582, #24796 ) ;
#59220 = CARTESIAN_POINT ( 'NONE',  ( 0.2885697896453111588, -0.8047882042609548758, 43.10898998017122352 ) ) ;
#59221 = CARTESIAN_POINT ( 'NONE',  ( 5.981074661064941900, -7.862380442164262462, 18.95903134304776216 ) ) ;
#59222 = CARTESIAN_POINT ( 'NONE',  ( 0.1135584504625008068, 36.74260402655860958, 24.43221442036662694 ) ) ;
#59223 = ORIENTED_EDGE ( 'NONE', *, *, #27516, .T. ) ;
#59224 = CARTESIAN_POINT ( 'NONE',  ( 4.956653778116991482, -8.845409907520609849, -47.27023054223761989 ) ) ;
#59225 = CARTESIAN_POINT ( 'NONE',  ( 4.975610109902397937, 48.90928568712962488, -0.5754830253892166958 ) ) ;
#59226 = CARTESIAN_POINT ( 'NONE',  ( 0.9268187852002115479, -42.38381720469895697, 12.13945518000253543 ) ) ;
#59227 = ORIENTED_EDGE ( 'NONE', *, *, #1822, .F. ) ;
#59228 = EDGE_CURVE ( 'NONE', #20219, #48937, #518, .T. ) ;
#59229 = CARTESIAN_POINT ( 'NONE',  ( -6.078075953587585900, -18.89992925442658844, -3.686169885505280686 ) ) ;
#59230 = CARTESIAN_POINT ( 'NONE',  ( 20.55500000000001748, 0.000000000000000000, 0.000000000000000000 ) ) ;
#59231 = EDGE_CURVE ( 'NONE', #37909, #15172, #23553, .T. ) ;
#59232 = CARTESIAN_POINT ( 'NONE',  ( 0.6017666602106489515, -12.78804974226068047, -46.37677619531707762 ) ) ;
#59233 = B_SPLINE_CURVE_WITH_KNOTS ( 'NONE', 3,
 ( #15446, #49881, #16364, #15759, #35181, #21376, #6939, #54238, #34555, #44281, #26072, #40507, #6306, #10437, #48956, #10749, #49558, #1941, #45210 ),
 .UNSPECIFIED., .F., .F.,
 ( 4, 3, 3, 3, 3, 3, 4 ),
 ( 9.813676791237319219E-18, 0.0002732106629380556557, 0.0004098138914053659453, 0.0005464171197651452802, 0.0006830203481512486102, 0.0008196235766963462857, 0.001011968216111144197 ),
 .UNSPECIFIED. ) ;
#59234 = ORIENTED_EDGE ( 'NONE', *, *, #61962, .F. ) ;
#59235 = CARTESIAN_POINT ( 'NONE',  ( 4.833616638992205949, 34.47248434257868865, 30.83411269743576355 ) ) ;
#59236 = CARTESIAN_POINT ( 'NONE',  ( 0.5800708057587358191, -41.16170989303188321, -24.48933404430302829 ) ) ;
#59237 = EDGE_CURVE ( 'NONE', #4300, #52623, #20668, .T. ) ;
#59238 = ORIENTED_EDGE ( 'NONE', *, *, #5069, .T. ) ;
#59239 = ADVANCED_FACE ( 'NONE', ( #54772 ), #41557, .F. ) ;
#59240 = DIRECTION ( 'NONE',  ( -0.07500201931887527651, 0.4910262002617658550, 0.8679101150203188952 ) ) ;
#59241 = EDGE_CURVE ( 'NONE', #37177, #45673, #13244, .T. ) ;
#59242 = ORIENTED_EDGE ( 'NONE', *, *, #17789, .F. ) ;
#59243 = ORIENTED_EDGE ( 'NONE', *, *, #4570, .T. ) ;
#59244 = CARTESIAN_POINT ( 'NONE',  ( 2.648799415243708655, -21.10807549816135875, -44.26021477640521340 ) ) ;
#59245 = VERTEX_POINT ( 'NONE', #40410 ) ;
#59246 = CARTESIAN_POINT ( 'NONE',  ( 0.2940133293163015860, -13.32164038229105252, 42.05680024803307759 ) ) ;
#59247 = CARTESIAN_POINT ( 'NONE',  ( 0.9780106845699478857, -17.35579871403585628, -38.14587130284626681 ) ) ;
#59248 = VERTEX_POINT ( 'NONE', #41036 ) ;
#59249 = CARTESIAN_POINT ( 'NONE',  ( 3.661933894777867238, 35.71932967730839437, 30.60654590696914212 ) ) ;
#59250 = EDGE_CURVE ( 'NONE', #55904, #48168, #53836, .T. ) ;
#59251 = CARTESIAN_POINT ( 'NONE',  ( 0.5782707292762423457, 46.38083794024497308, -6.968086227103744257 ) ) ;
#59252 = EDGE_CURVE ( 'NONE', #450, #47731, #49068, .T. ) ;
#59253 =( BOUNDED_SURFACE ( )  B_SPLINE_SURFACE ( 3, 1, ( 
 ( #39317, #58377 ),
 ( #14897, #12052 ),
 ( #21423, #6986 ),
 ( #26121, #31126 ) ),
 .UNSPECIFIED., .F., .F., .F. ) 
 B_SPLINE_SURFACE_WITH_KNOTS ( ( 4, 4 ),
 ( 2, 2 ),
 ( 0.000000000000000000, 1.000000000000000000 ),
 ( 0.000000000000000000, 1.000000000000000000 ),
 .UNSPECIFIED. ) 
 GEOMETRIC_REPRESENTATION_ITEM ( )  RATIONAL_B_SPLINE_SURFACE ( (
 ( 1.000000000000000000, 1.000000000000000000),
 ( 0.9953390228620291325, 0.8624445117760984880),
 ( 0.9953390228620291325, 0.8624445117760984880),
 ( 1.000000000000000000, 1.000000000000000000) ) ) 
 REPRESENTATION_ITEM ( '' )  SURFACE ( )  );
#59254 = VERTEX_POINT ( 'NONE', #58854 ) ;
#59255 = CARTESIAN_POINT ( 'NONE',  ( 0.6028618097248863439, -18.24855319618775340, 44.51207924874646693 ) ) ;
#59256 = B_SPLINE_CURVE_WITH_KNOTS ( 'NONE', 3,
 ( #31534, #21834, #40971, #59723, #11840, #54702 ),
 .UNSPECIFIED., .F., .F.,
 ( 4, 2, 4 ),
 ( 8.805430561888389713E-18, 0.0002448709889506569940, 0.0004897419779013052060 ),
 .UNSPECIFIED. ) ;
#59257 = FACE_OUTER_BOUND ( 'NONE', #54132, .T. ) ;
#59258 = CARTESIAN_POINT ( 'NONE',  ( 0.1097557419366048670, -30.33543403792258886, 30.65094619415014776 ) ) ;
#59259 = CARTESIAN_POINT ( 'NONE',  ( 4.958415959904816539, 44.61026793747944197, 8.551488079213465099 ) ) ;
#59260 = EDGE_LOOP ( 'NONE', ( #55543, #43330, #5143, #29322 ) ) ;
#59261 = VERTEX_POINT ( 'NONE', #1844 ) ;
#59262 = AXIS2_PLACEMENT_3D ( 'NONE', #43627, #20416, #29804 ) ;
#59263 = DIRECTION ( 'NONE',  ( -1.718001593797181987E-16, 1.000000000000000000, 0.000000000000000000 ) ) ;
#59264 = VECTOR ( 'NONE', #880, 1000.000000000000000 ) ;
#59265 = CARTESIAN_POINT ( 'NONE',  ( -49.49999999999975842, 1.232595164407830946E-29, 1.078520768856852078E-29 ) ) ;
#59266 = CARTESIAN_POINT ( 'NONE',  ( 0.3622758884714600280, -41.85013935980108357, 10.35929834645850001 ) ) ;
#59267 = ORIENTED_EDGE ( 'NONE', *, *, #32038, .T. ) ;
#59268 = CARTESIAN_POINT ( 'NONE',  ( 0.9268187852002115479, -42.88685641119342762, -10.22114866706790615 ) ) ;
#59269 = CARTESIAN_POINT ( 'NONE',  ( -6.079354080745853928, 9.983157571107183159, -16.46601105789156705 ) ) ;
#59270 = CARTESIAN_POINT ( 'NONE',  ( 0.8554163680231738898, -46.86440027434178290, 2.221139355847132624 ) ) ;
#59271 = CARTESIAN_POINT ( 'NONE',  ( 0.6028618097248863439, -41.74935807801029597, -23.90242650600261598 ) ) ;
#59272 = VERTEX_POINT ( 'NONE', #40115 ) ;
#59273 = EDGE_LOOP ( 'NONE', ( #13286, #48386, #39013, #6841 ) ) ;
#59274 = CARTESIAN_POINT ( 'NONE',  ( 4.303969348037258058, 46.98258166031690308, 10.35452842635859483 ) ) ;
#59275 = CARTESIAN_POINT ( 'NONE',  ( 0.1073791018717578927, 33.91564619577771111, 26.63563652260178927 ) ) ;
#59276 =( BOUNDED_SURFACE ( )  B_SPLINE_SURFACE ( 3, 1, ( 
 ( #52309, #23504 ),
 ( #9399, #8172 ),
 ( #27595, #27908 ),
 ( #32929, #46721 ) ),
 .UNSPECIFIED., .F., .F., .F. ) 
 B_SPLINE_SURFACE_WITH_KNOTS ( ( 4, 4 ),
 ( 2, 2 ),
 ( 0.000000000000000000, 1.000000000000000000 ),
 ( 0.000000000000000000, 1.000000000000000000 ),
 .UNSPECIFIED. ) 
 GEOMETRIC_REPRESENTATION_ITEM ( )  RATIONAL_B_SPLINE_SURFACE ( (
 ( 1.000000000000000000, 1.000000000000000000),
 ( 0.9953040768229013402, 0.8617119497784988535),
 ( 0.9953040768229013402, 0.8617119497784988535),
 ( 1.000000000000000000, 1.000000000000000000) ) ) 
 REPRESENTATION_ITEM ( '' )  SURFACE ( )  );
#59277 = CARTESIAN_POINT ( 'NONE',  ( -6.016489644550737204, 7.206912786933291848, 17.41053539857202281 ) ) ;
#59279 = EDGE_CURVE ( 'NONE', #50843, #13524, #10244, .T. ) ;
#59278 = CARTESIAN_POINT ( 'NONE',  ( 4.956445790443996025, 13.43466403631381567, 45.13366650706556982 ) ) ;
#59280 = CARTESIAN_POINT ( 'NONE',  ( 0.1103310638050662151, 34.26302445194747293, -26.18709435931489793 ) ) ;
#59281 = B_SPLINE_CURVE_WITH_KNOTS ( 'NONE', 3,
 ( #9909, #24936, #25228, #19941, #48123, #33416 ),
 .UNSPECIFIED., .F., .F.,
 ( 4, 2, 4 ),
 ( 1.179429090023230705E-16, 0.0002448718616795931505, 0.0004897437233590683399 ),
 .UNSPECIFIED. ) ;
#59282 = EDGE_CURVE ( 'NONE', #34106, #8248, #16583, .T. ) ;
#59283 = B_SPLINE_CURVE_WITH_KNOTS ( 'NONE', 3,
 ( #2897, #22028, #41152, #60214 ),
 .UNSPECIFIED., .F., .F.,
 ( 4, 4 ),
 ( 2.297383214701471906E-17, 0.004564976165746187711 ),
 .UNSPECIFIED. ) ;
#59284 = CARTESIAN_POINT ( 'NONE',  ( 1.227938101723756947, 22.18841447410719780, 36.73927144310519566 ) ) ;
#59285 = CIRCLE ( 'NONE', #55304, 47.09074272231896430 ) ;
#59286 = CARTESIAN_POINT ( 'NONE',  ( 0.5807400328401574052, -38.33001520688970487, 28.72484455891627775 ) ) ;
#59287 = CARTESIAN_POINT ( 'NONE',  ( 0.5806925824938499181, -24.77160101449041463, -39.81946942793766198 ) ) ;
#59288 = DIRECTION ( 'NONE',  ( -0.1011922191286467460, 0.5266864627877126948, -0.8440151092865501026 ) ) ;
#59289 = CARTESIAN_POINT ( 'NONE',  ( 0.6031356755773454870, -6.279255973231697929, 47.69588082432145626 ) ) ;
#59290 = CARTESIAN_POINT ( 'NONE',  ( 0.7948878604505672518, -42.34838794577630949, 24.84577802550052894 ) ) ;
#59291 = DIRECTION ( 'NONE',  ( -1.000000000000000000, -0.000000000000000000, -0.000000000000000000 ) ) ;
#59292 = PRODUCT_RELATED_PRODUCT_CATEGORY ( 'part', '', ( #7765 ) ) ;
#59293 = CARTESIAN_POINT ( 'NONE',  ( 0.5998501479064699549, 5.759754759340783181, -47.76154736470751772 ) ) ;
#59294 = CARTESIAN_POINT ( 'NONE',  ( 0.6845945791218023269, -34.20288208893713744, 32.10248241996572460 ) ) ;
#59295 = CARTESIAN_POINT ( 'NONE',  ( 0.6030672727741701600, -33.95535904584762932, -34.07876014368848416 ) ) ;
#59296 = CARTESIAN_POINT ( 'NONE',  ( 0.7954190325252775695, -19.20649988843089417, -44.09776758977464084 ) ) ;
#59297 = ITEM_DEFINED_TRANSFORMATION ( 'NONE', 'NONE', #45918,  #14677 ) ;
#59298 = CARTESIAN_POINT ( 'NONE',  ( 0.6025881611877909050, -6.062907795289036450, -47.72390913208162999 ) ) ;
#59299 = CARTESIAN_POINT ( 'NONE',  ( 0.5987334308729320709, -38.99056144767197907, 29.85463154294563992 ) ) ;
#59300 = CARTESIAN_POINT ( 'NONE',  ( -6.016104459813371719, 4.871830707673312055, -18.20253432612961575 ) ) ;
#59301 = CARTESIAN_POINT ( 'NONE',  ( 0.6029443449137434907, 48.19350774417130623, 9.430023822654650445 ) ) ;
#59303 = ORIENTED_EDGE ( 'NONE', *, *, #41489, .F. ) ;
#59302 = CARTESIAN_POINT ( 'NONE',  ( 5.974727161628369032, -16.27409205901367883, -12.50710176110002081 ) ) ;
#59304 = ORIENTED_EDGE ( 'NONE', *, *, #966, .F. ) ;
#59305 = CARTESIAN_POINT ( 'NONE',  ( 3.238018933889920792, -8.435922058907914689, 10.40397574889925458 ) ) ;
#59306 = CARTESIAN_POINT ( 'NONE',  ( 0.1073791018717578927, 30.83464511437137645, -30.14884492832358731 ) ) ;
#59307 = DIRECTION ( 'NONE',  ( 0.000000000000000000, 0.000000000000000000, 1.000000000000000000 ) ) ;
#59308 = VERTEX_POINT ( 'NONE', #35709 ) ;
#59309 = VERTEX_POINT ( 'NONE', #51307 ) ;
#59310 = CARTESIAN_POINT ( 'NONE',  ( 4.553261556744875094, -20.51767157960516741, 38.84024612145369559 ) ) ;
#59311 = CARTESIAN_POINT ( 'NONE',  ( -6.063463321072278589, -4.300220425535210111, 18.77041706439363367 ) ) ;
#59312 = CARTESIAN_POINT ( 'NONE',  ( 0.1073791018717483448, -37.10214135362904386, 21.98088480513601795 ) ) ;
#59313 = AXIS2_PLACEMENT_3D ( 'NONE', #61130, #61429, #27636 ) ;
#59314 = EDGE_CURVE ( 'NONE', #52304, #46447, #4096, .T. ) ;
#59315 = VERTEX_POINT ( 'NONE', #60097 ) ;
#59316 = ORIENTED_EDGE ( 'NONE', *, *, #31343, .F. ) ;
#59317 = CARTESIAN_POINT ( 'NONE',  ( 0.1073791018717578927, 10.69234304549997105, 41.77800844988518492 ) ) ;
#59318 = EDGE_CURVE ( 'NONE', #30492, #16733, #51533, .T. ) ;
#59319 = CARTESIAN_POINT ( 'NONE',  ( 7.999999999999996447, -2.649999999999153033, -80.00000000000004263 ) ) ;
#59320 = CARTESIAN_POINT ( 'NONE',  ( 3.680974057930773924, -47.77138393978999176, 4.423547572561508545 ) ) ;
#59321 = EDGE_CURVE ( 'NONE', #22775, #46370, #53540, .T. ) ;
#59322 = ORIENTED_EDGE ( 'NONE', *, *, #27201, .F. ) ;
#59323 = CARTESIAN_POINT ( 'NONE',  ( 0.9722240741986369894, -10.54237114526854313, -41.59310805473380412 ) ) ;
#59324 = VECTOR ( 'NONE', #46348, 1000.000000000000114 ) ;
#59325 = B_SPLINE_CURVE_WITH_KNOTS ( 'NONE', 3,
 ( #49433, #50358, #25944, #15092 ),
 .UNSPECIFIED., .F., .F.,
 ( 4, 4 ),
 ( 0.000000000000000000, 0.005013413432710138971 ),
 .UNSPECIFIED. ) ;
#59326 = CARTESIAN_POINT ( 'NONE',  ( 0.1129192098497447394, 43.99990943031675528, -3.310552508128703497 ) ) ;
#59327 = EDGE_LOOP ( 'NONE', ( #39269, #53240 ) ) ;
#59328 = ORIENTED_EDGE ( 'NONE', *, *, #2414, .T. ) ;
#59329 = CARTESIAN_POINT ( 'NONE',  ( 0.2279481005628776480, 43.44433607591050617, -7.687206904737967861 ) ) ;
#59330 = CARTESIAN_POINT ( 'NONE',  ( 0.7242003506640002364, -19.12400634200194460, 45.22481681065273307 ) ) ;
#59331 = ORIENTED_EDGE ( 'NONE', *, *, #54642, .T. ) ;
#59332 = CARTESIAN_POINT ( 'NONE',  ( -6.001507490154111224, -18.20581304543301471, 4.862106078787861385 ) ) ;
#59333 = CARTESIAN_POINT ( 'NONE',  ( 0.8551540677456834771, -33.23105123575924580, 34.52115452272916940 ) ) ;
#59334 = CARTESIAN_POINT ( 'NONE',  ( 0.1073791018717483448, 42.68962945260953035, -6.109314776652274404 ) ) ;
#59335 = CARTESIAN_POINT ( 'NONE',  ( 0.5832366564991499081, 12.13301812590415096, -46.33368520589904449 ) ) ;
#59336 = ORIENTED_EDGE ( 'NONE', *, *, #15585, .T. ) ;
#59337 = CARTESIAN_POINT ( 'NONE',  ( 2.528100132419517365, 40.79053833512498528, 9.918959671395732869 ) ) ;
#59338 = CARTESIAN_POINT ( 'NONE',  ( 0.6029443449137436017, -35.30655258969704136, 34.13190416918297387 ) ) ;
#59339 = CARTESIAN_POINT ( 'NONE',  ( 0.9754402186311951217, -21.61645729243085867, -37.06569162601120127 ) ) ;
#59340 = ORIENTED_EDGE ( 'NONE', *, *, #44313, .F. ) ;
#59341 = CARTESIAN_POINT ( 'NONE',  ( 0.1129192098497455998, -35.06977877439224045, -26.77802092202373174 ) ) ;
#59342 = CARTESIAN_POINT ( 'NONE',  ( 0.8751705887134553219, -47.79200036674276220, -5.393078191592532988 ) ) ;
#59343 = ORIENTED_EDGE ( 'NONE', *, *, #53900, .T. ) ;
#59344 = DIRECTION ( 'NONE',  ( -1.000000000000000000, -0.000000000000000000, -0.000000000000000000 ) ) ;
#59345 = CARTESIAN_POINT ( 'NONE',  ( 0.5797568599927142019, -41.56795257228133522, -21.71015033618085255 ) ) ;
#59346 = EDGE_LOOP ( 'NONE', ( #10620, #57109, #56319, #57857 ) ) ;
#59347 = CARTESIAN_POINT ( 'NONE',  ( 1.092182651088186018, -41.76072632286304298, 3.578117022851349915 ) ) ;
#59348 = CARTESIAN_POINT ( 'NONE',  ( 0.3622758884714730732, -20.83792692158999316, 37.74294673546550172 ) ) ;
#59349 = CARTESIAN_POINT ( 'NONE',  ( 0.8551540677456739292, 47.61725548905997840, -5.348818140990426073 ) ) ;
#59350 = B_SPLINE_CURVE_WITH_KNOTS ( 'NONE', 3,
 ( #32304, #19142, #3764, #61391 ),
 .UNSPECIFIED., .F., .F.,
 ( 4, 4 ),
 ( 0.000000000000000000, 0.005004741218457427546 ),
 .UNSPECIFIED. ) ;
#59351 = CIRCLE ( 'NONE', #10373, 7.500000000000022204 ) ;
#59352 = CARTESIAN_POINT ( 'NONE',  ( 0.6252788684277222897, -14.62912771694895397, -46.87678480244634471 ) ) ;
#59353 =( BOUNDED_SURFACE ( )  B_SPLINE_SURFACE ( 3, 1, ( 
 ( #27949, #18246 ),
 ( #18546, #37674 ),
 ( #14782, #28545 ),
 ( #33894, #23861 ) ),
 .UNSPECIFIED., .F., .F., .F. ) 
 B_SPLINE_SURFACE_WITH_KNOTS ( ( 4, 4 ),
 ( 2, 2 ),
 ( 0.000000000000000000, 1.000000000000000000 ),
 ( 0.000000000000000000, 1.000000000000000000 ),
 .UNSPECIFIED. ) 
 GEOMETRIC_REPRESENTATION_ITEM ( )  RATIONAL_B_SPLINE_SURFACE ( (
 ( 1.000000000000000000, 1.000000000000000000),
 ( 0.7223157951917480446, 0.9931996967497186413),
 ( 0.7223157951917480446, 0.9931996967497186413),
 ( 1.000000000000000000, 1.000000000000000000) ) ) 
 REPRESENTATION_ITEM ( '' )  SURFACE ( )  );
#59354 = DIRECTION ( 'NONE',  ( 0.000000000000000000, 0.000000000000000000, 1.000000000000000000 ) ) ;
#59355 = CARTESIAN_POINT ( 'NONE',  ( 0.3676999524040366896, -41.19158123804976412, -15.78620342045500280 ) ) ;
#59356 = ADVANCED_FACE ( 'NONE', ( #22514 ), #26744, .F. ) ;
#59357 = CARTESIAN_POINT ( 'NONE',  ( 4.553261556744873317, 35.33793455049254106, 26.09156851415302825 ) ) ;
#59358 = CARTESIAN_POINT ( 'NONE',  ( 1.112077966505211180, -32.38613972894711424, -29.90264668195222697 ) ) ;
#59359 = DIRECTION ( 'NONE',  ( 0.07836865515943411409, -0.9649662368512254007, 0.2503967164834362547 ) ) ;
#59360 = CARTESIAN_POINT ( 'NONE',  ( 0.5997462898726536595, 41.43917033312134635, -26.35046094941917971 ) ) ;
#59361 = CARTESIAN_POINT ( 'NONE',  ( 0.7242486021783809402, 33.61309370897174631, -35.79345462072436845 ) ) ;
#59362 = VERTEX_POINT ( 'NONE', #3079 ) ;
#59363 = CARTESIAN_POINT ( 'NONE',  ( 0.6846871229502899947, -5.395516691087521188, 47.60345020167350327 ) ) ;
#59364 = CARTESIAN_POINT ( 'NONE',  ( 1.227938101723748288, -17.20315230597871903, 39.32113113558960293 ) ) ;
#59365 = CARTESIAN_POINT ( 'NONE',  ( -4.000000000000000000, 1.557668341133520373, -5.440303434304243346 ) ) ;
#59366 = CARTESIAN_POINT ( 'NONE',  ( 0.8753041380234530822, 5.600023814135296263, 48.78296896616787848 ) ) ;
#59367 = AXIS2_PLACEMENT_3D ( 'NONE', #35872, #11756, #54941 ) ;
#59368 = CARTESIAN_POINT ( 'NONE',  ( -6.079354080745853928, 18.62651132414721289, 4.883239819994285469 ) ) ;
#59369 = CARTESIAN_POINT ( 'NONE',  ( 5.838029081930955932, -10.96929503790549809, 45.94278642533886625 ) ) ;
#59370 = DIRECTION ( 'NONE',  ( -1.000000000000000000, 4.624120190530355775E-15, 5.067589380725346644E-15 ) ) ;
#59371 = CARTESIAN_POINT ( 'NONE',  ( 0.7948878604505663636, -2.440498608811802583, -49.03817506635828494 ) ) ;
#59372 = CARTESIAN_POINT ( 'NONE',  ( 4.390527457369402420, 35.40014937592107458, -26.01950731261247185 ) ) ;
#59373 = CARTESIAN_POINT ( 'NONE',  ( 0.6025881611877910160, 0.2181813582438441590, -48.10699274197334319 ) ) ;
#59375 = ORIENTED_EDGE ( 'NONE', *, *, #20277, .F. ) ;
#59374 = CARTESIAN_POINT ( 'NONE',  ( 0.8554163680231816613, 43.54276151446858734, 17.47092993535067507 ) ) ;
#59376 = ORIENTED_EDGE ( 'NONE', *, *, #23311, .F. ) ;
#59377 = CARTESIAN_POINT ( 'NONE',  ( 0.1310142868023677909, -34.59629828998431122, 25.74368468368876606 ) ) ;
#59378 = B_SPLINE_CURVE_WITH_KNOTS ( 'NONE', 3,
 ( #36644, #55405, #49798, #55101, #21297, #59490 ),
 .UNSPECIFIED., .F., .F.,
 ( 4, 2, 4 ),
 ( 9.828040028768063295E-18, 0.0002291459268755722677, 0.0004582918537511346691 ),
 .UNSPECIFIED. ) ;
#59379 = CARTESIAN_POINT ( 'NONE',  ( 2.624215991343620935, 32.93378783738897653, -34.92983774302933142 ) ) ;
#59380 = CARTESIAN_POINT ( 'NONE',  ( 0.5807400328401574052, 37.66660715020866945, 29.58941477093028283 ) ) ;
#59381 = ORIENTED_EDGE ( 'NONE', *, *, #56639, .T. ) ;
#59382 = CARTESIAN_POINT ( 'NONE',  ( 0.3676999524040323597, 44.06746933160595603, -2.002181318164867552 ) ) ;
#59383 = CARTESIAN_POINT ( 'NONE',  ( 0.5832366564991514624, -47.44984844891991571, 6.521686574605942255 ) ) ;
#59384 = CARTESIAN_POINT ( 'NONE',  ( 0.5988103622719989083, 41.35593060299636647, 24.57719485303652007 ) ) ;
#59385 = EDGE_CURVE ( 'NONE', #39205, #12115, #52707, .T. ) ;
#59386 = VERTEX_POINT ( 'NONE', #22819 ) ;
#59387 = ORIENTED_EDGE ( 'NONE', *, *, #22838, .F. ) ;
#59388 = ADVANCED_FACE ( 'NONE', ( #55390 ), #21993, .F. ) ;
#59389 = CARTESIAN_POINT ( 'NONE',  ( -6.015611763856276717, 7.216738110653281524, 17.40650793417846032 ) ) ;
#59390 = CARTESIAN_POINT ( 'NONE',  ( 0.1073791018717483448, -11.62916352156123168, -41.52698815987163528 ) ) ;
#59391 = CARTESIAN_POINT ( 'NONE',  ( 0.5800708057587399269, 41.78924035064556364, -23.40241940841912793 ) ) ;
#59392 = ORIENTED_EDGE ( 'NONE', *, *, #14908, .F. ) ;
#59393 = EDGE_CURVE ( 'NONE', #20504, #35226, #45319, .T. ) ;
#59394 = VECTOR ( 'NONE', #47367, 1000.000000000000227 ) ;
#59395 = ORIENTED_EDGE ( 'NONE', *, *, #26544, .F. ) ;
#59396 = CARTESIAN_POINT ( 'NONE',  ( 0.1095718737110178004, -0.2569529612660841345, 43.12372487139541732 ) ) ;
#59397 = DIRECTION ( 'NONE',  ( 0.000000000000000000, 1.000000000000000000, -3.552713678800500929E-15 ) ) ;
#59398 = B_SPLINE_CURVE_WITH_KNOTS ( 'NONE', 3,
 ( #17306, #13536, #2566, #41439, #59892, #45514, #21687, #55185, #12307, #31398, #46136, #50495, #7568, #45829, #41135, #642, #24462, #19169, #57331 ),
 .UNSPECIFIED., .F., .F.,
 ( 4, 3, 3, 3, 3, 3, 4 ),
 ( 9.813676791237319219E-18, 0.0002724573126191738581, 0.0004086839781548292326, 0.0005449106435901659821, 0.0006811373090491345443, 0.0008459866663933557135, 0.001010840725717199705 ),
 .UNSPECIFIED. ) ;
#59399 = ORIENTED_EDGE ( 'NONE', *, *, #24046, .F. ) ;
#59400 = CARTESIAN_POINT ( 'NONE',  ( 2.282803330402964459, -29.31214732841990767, -36.70551629461151322 ) ) ;
#59401 = CARTESIAN_POINT ( 'NONE',  ( 0.9752570700956809668, 41.50550328400882449, -10.88256294660668821 ) ) ;
#59402 = VERTEX_POINT ( 'NONE', #31917 ) ;
#59403 = CARTESIAN_POINT ( 'NONE',  ( 0.9722240741986376555, -33.68410525900265640, -26.58024228478330286 ) ) ;
#59404 = EDGE_CURVE ( 'NONE', #22913, #18160, #50689, .T. ) ;
#59405 = FACE_OUTER_BOUND ( 'NONE', #45272, .T. ) ;
#59406 = ORIENTED_EDGE ( 'NONE', *, *, #28358, .T. ) ;
#59407 = CARTESIAN_POINT ( 'NONE',  ( -6.063463321072278589, -11.02986456480193489, 15.78488327994846152 ) ) ;
#59408 = CARTESIAN_POINT ( 'NONE',  ( 1.231276596079887264, -21.83837404314831332, 35.78214904347716185 ) ) ;
#59409 = CARTESIAN_POINT ( 'NONE',  ( 1.088313998177381281, 42.64115081428570875, -4.827222641554805627 ) ) ;
#59410 = CARTESIAN_POINT ( 'NONE',  ( -6.072942160501519915, 16.78547611690376584, 9.436734277167797558 ) ) ;
#59411 = EDGE_CURVE ( 'NONE', #19272, #8059, #32540, .T. ) ;
#59412 = AXIS2_PLACEMENT_3D ( 'NONE', #25611, #20015, #25302 ) ;
#59413 = EDGE_LOOP ( 'NONE', ( #52625, #18276, #41903, #37419, #25921, #39558, #16598, #14578, #27630, #45495, #55406, #26021, #13922, #56085, #22227, #34379, #46274, #60806, #9029, #40757, #39117, #7398, #30458, #39518, #49168, #41341, #54535, #3627, #21364, #16331, #16570, #16949, #4326, #18531, #45686, #1669, #23314, #10744, #35119, #20123, #43355, #21666, #1805, #53750, #58466, #56543, #58771, #32105, #13753, #44835, #40904, #49662, #5868, #46047, #12993, #54549, #56950, #1617, #184, #45333, #21730, #18898, #22014, #59169, #17421, #53237, #4030, #41187, #34624, #14350, #39146, #26577, #32478, #32697, #15458, #16148, #9719, #41707, #33931, #38548, #7297, #38208, #29697, #18178, #16689, #20990, #29893, #44085, #53546, #31011, #56481, #35661, #14563, #19162, #59438, #36169, #48175, #39838, #58932, #57958, #10992, #27675, #28685, #17410, #31557, #16577, #27548, #27063, #24138, #44648, #772, #28316, #32465, #11959, #22537, #1024, #55767, #38163, #17601, #4745, #33619, #17925, #19972, #1237, #554, #44803, #32376, #61544, #42107, #2940, #15830, #56893, #10725, #10249, #56861, #7079, #2924, #36517, #39701, #11836, #50348, #8899, #25912, #31503, #13691, #5000, #12746, #20667 ) ) ;
#59414 = DIRECTION ( 'NONE',  ( 0.000000000000000000, 0.000000000000000000, 1.000000000000000000 ) ) ;
#59415 = CARTESIAN_POINT ( 'NONE',  ( 0.5997462898726536595, 4.195097405483644515, -48.92803682862019343 ) ) ;
#59416 = ORIENTED_EDGE ( 'NONE', *, *, #29011, .T. ) ;
#59417 = CARTESIAN_POINT ( 'NONE',  ( 5.896782393890504181, -7.222780579330470019, -18.77118876312469808 ) ) ;
#59418 = ORIENTED_EDGE ( 'NONE', *, *, #31621, .T. ) ;
#59419 = CARTESIAN_POINT ( 'NONE',  ( 0.5839879327111946461, -18.24507200299072807, 44.28486549479615775 ) ) ;
#59420 = ORIENTED_EDGE ( 'NONE', *, *, #36641, .F. ) ;
#59421 = FACE_OUTER_BOUND ( 'NONE', #50935, .T. ) ;
#59422 = CARTESIAN_POINT ( 'NONE',  ( 0.9775691876210963471, 24.55423032742939071, 33.96208889361105321 ) ) ;
#59423 = CARTESIAN_POINT ( 'NONE',  ( 0.1073791018717483448, -25.86618856530736466, 34.50606437925502945 ) ) ;
#59424 = VERTEX_POINT ( 'NONE', #8710 ) ;
#59425 = CARTESIAN_POINT ( 'NONE',  ( 0.1156495703730067437, 43.33634112329940535, 8.300872922536509435 ) ) ;
#59426 = CARTESIAN_POINT ( 'NONE',  ( 0.6846871229502899947, 33.25969555998791094, -34.48177377577800939 ) ) ;
#59427 = CARTESIAN_POINT ( 'NONE',  ( 42.00000000000000711, 6.547216728259810428E-15, -1.617781153285278467E-30 ) ) ;
#59428 = ORIENTED_EDGE ( 'NONE', *, *, #40316, .F. ) ;
#59429 = ADVANCED_BREP_SHAPE_REPRESENTATION ( '', ( #10859, #14677 ), #6659 ) ;
#59430 = ORIENTED_EDGE ( 'NONE', *, *, #41401, .F. ) ;
#59431 = CARTESIAN_POINT ( 'NONE',  ( 4.956653778116975495, 15.97476558431885252, 45.35992544608534160 ) ) ;
#59432 = CARTESIAN_POINT ( 'NONE',  ( 0.3676999524040366896, 30.26295534861856495, 32.09523511193457068 ) ) ;
#59433 = CARTESIAN_POINT ( 'NONE',  ( 0.9780106845699492180, 38.70451287974908183, -16.07146319402109214 ) ) ;
#59434 = CARTESIAN_POINT ( 'NONE',  ( 0.1104177457020372871, -5.633723015004581391, -42.75487793940121861 ) ) ;
#59435 = EDGE_CURVE ( 'NONE', #16733, #57918, #27311, .T. ) ;
#59436 = CARTESIAN_POINT ( 'NONE',  ( 0.5817217712918331118, -29.92824280590621555, -36.10450438046610344 ) ) ;
#59437 = CARTESIAN_POINT ( 'NONE',  ( 4.553261556744875094, 42.43205150231973732, 11.36048287389764688 ) ) ;
#59438 = ORIENTED_EDGE ( 'NONE', *, *, #46258, .T. ) ;
#59439 = CARTESIAN_POINT ( 'NONE',  ( 0.7762777257811900311, -23.17763256463740973, -41.92424087089334961 ) ) ;
#59440 = FACE_OUTER_BOUND ( 'NONE', #40175, .T. ) ;
#59441 = ORIENTED_EDGE ( 'NONE', *, *, #44588, .T. ) ;
#59442 = CARTESIAN_POINT ( 'NONE',  ( 3.678834586032788234, 42.02542406194491775, -25.14907755847229609 ) ) ;
#59443 = CARTESIAN_POINT ( 'NONE',  ( 0.5998501479064699549, -41.92175333043603302, -23.59887241503339439 ) ) ;
#59444 = CARTESIAN_POINT ( 'NONE',  ( 4.291220156522059348, -40.01826627095215372, 24.85814478139649353 ) ) ;
#59445 = CARTESIAN_POINT ( 'NONE',  ( 0.5835871038041864356, 45.19346916843720408, 12.52137362364909556 ) ) ;
#59446 = CARTESIAN_POINT ( 'NONE',  ( 4.303969348037246512, 43.57722561725959309, 20.38638383586135561 ) ) ;
#59447 = CARTESIAN_POINT ( 'NONE',  ( 5.910764540655178756, 17.95751408178354680, 9.056982194512078976 ) ) ;
#59448 = CARTESIAN_POINT ( 'NONE',  ( 0.6027444965799114707, 4.585416998493479390, 48.89286723886592512 ) ) ;
#59449 = SURFACE_SIDE_STYLE ('',( #53510 ) ) ;
#59450 = DIRECTION ( 'NONE',  ( -0.07439287786467652097, -0.9665813013808162157, -0.2453289374370237197 ) ) ;
#59451 = CARTESIAN_POINT ( 'NONE',  ( -6.016104459813371719, -17.40682403289253344, 7.215917642689006151 ) ) ;
#59452 = AXIS2_PLACEMENT_3D ( 'NONE', #6543, #35416, #38891 ) ;
#59453 = DIRECTION ( 'NONE',  ( 0.000000000000000000, 0.000000000000000000, 1.000000000000000000 ) ) ;
#59454 = FACE_OUTER_BOUND ( 'NONE', #29754, .T. ) ;
#59455 = CARTESIAN_POINT ( 'NONE',  ( 2.618530812446111078, -9.204197330484477746, 46.09782576976600410 ) ) ;
#59456 = DIRECTION ( 'NONE',  ( 0.09722883295013594329, 0.9754357953229615408, -0.1976652808305395526 ) ) ;
#59457 = VECTOR ( 'NONE', #42449, 1000.000000000000000 ) ;
#59458 = LINE ( 'NONE', #28566, #43510 ) ;
#59459 = DIRECTION ( 'NONE',  ( -1.000000000000000000, -0.000000000000000000, -0.000000000000000000 ) ) ;
#59460 = VERTEX_POINT ( 'NONE', #27826 ) ;
#59461 = EDGE_CURVE ( 'NONE', #1494, #58012, #24542, .T. ) ;
#59462 = CARTESIAN_POINT ( 'NONE',  ( 0.1092565886968784178, 10.86136484717969886, -41.73439049602441031 ) ) ;
#59463 = CARTESIAN_POINT ( 'NONE',  ( 0.1092355843206037486, 43.12343565949664992, 0.3005923759135379902 ) ) ;
#59464 = CARTESIAN_POINT ( 'NONE',  ( 0.9730545539215883499, -25.71816799638755668, -34.34678117142582465 ) ) ;
#59465 = CARTESIAN_POINT ( 'NONE',  ( 1.154321485836932393, -25.46626718279332025, 34.54400167111891307 ) ) ;
#59466 = CARTESIAN_POINT ( 'NONE',  ( 0.1087620492084204887, -41.74735017127137837, 10.81135549499707871 ) ) ;
#59467 = ORIENTED_EDGE ( 'NONE', *, *, #27230, .T. ) ;
#59468 = EDGE_CURVE ( 'NONE', #16352, #24828, #9637, .T. ) ;
#59469 = CARTESIAN_POINT ( 'NONE',  ( 0.8557997880470697982, 17.48760788519276943, -44.60232077416669227 ) ) ;
#59470 = CARTESIAN_POINT ( 'NONE',  ( 0.3622758884714730732, 43.10531414739106282, -0.8252992914323589169 ) ) ;
#59471 = B_SPLINE_CURVE_WITH_KNOTS ( 'NONE', 3,
 ( #51113, #8203, #37356, #61425, #27631, #33 ),
 .UNSPECIFIED., .F., .F.,
 ( 4, 2, 4 ),
 ( 1.218313306513762119E-16, 0.0002448718616795917411, 0.0004897437233590617263 ),
 .UNSPECIFIED. ) ;
#59472 = CARTESIAN_POINT ( 'NONE',  ( 4.553261556744875094, 22.96401893593780841, -37.44587293859667199 ) ) ;
#59473 = ORIENTED_EDGE ( 'NONE', *, *, #29485, .F. ) ;
#59474 = B_SPLINE_CURVE_WITH_KNOTS ( 'NONE', 3,
 ( #42947, #57604, #9953, #606 ),
 .UNSPECIFIED., .F., .F.,
 ( 4, 4 ),
 ( 0.000000000000000000, 0.005004741218457415403 ),
 .UNSPECIFIED. ) ;
#59475 = AXIS2_PLACEMENT_3D ( 'NONE', #56304, #42248, #23732 ) ;
#59476 =( BOUNDED_SURFACE ( )  B_SPLINE_SURFACE ( 3, 1, ( 
 ( #12920, #60487 ),
 ( #17298, #21998 ),
 ( #17603, #36417 ),
 ( #12610, #31701 ) ),
 .UNSPECIFIED., .F., .F., .F. ) 
 B_SPLINE_SURFACE_WITH_KNOTS ( ( 4, 4 ),
 ( 2, 2 ),
 ( 0.000000000000000000, 1.000000000000000000 ),
 ( 0.000000000000000000, 1.000000000000000000 ),
 .UNSPECIFIED. ) 
 GEOMETRIC_REPRESENTATION_ITEM ( )  RATIONAL_B_SPLINE_SURFACE ( (
 ( 1.000000000000000000, 1.000000000000000000),
 ( 0.7282232189291694135, 0.9929344683865672927),
 ( 0.7282232189291694135, 0.9929344683865672927),
 ( 1.000000000000000000, 1.000000000000000000) ) ) 
 REPRESENTATION_ITEM ( '' )  SURFACE ( )  );
#59477 = CARTESIAN_POINT ( 'NONE',  ( 0.3622758884714730732, 17.25816669464937902, 39.50828911767005280 ) ) ;
#59478 = VERTEX_POINT ( 'NONE', #48466 ) ;
#59479 = CARTESIAN_POINT ( 'NONE',  ( 0.8751705887134423323, 34.63284514348585930, -33.37254303619518225 ) ) ;
#59480 = CARTESIAN_POINT ( 'NONE',  ( 4.553261556744873317, -43.85016385001095074, -2.588956575693968976 ) ) ;
#59481 = EDGE_LOOP ( 'NONE', ( #47286, #50940, #5708, #23403 ) ) ;
#59482 = CARTESIAN_POINT ( 'NONE',  ( -6.063463321072278589, 9.969191071288406647, 16.47530521306399010 ) ) ;
#59483 = ORIENTED_EDGE ( 'NONE', *, *, #41186, .F. ) ;
#59484 = CARTESIAN_POINT ( 'NONE',  ( 2.624215991343608501, -34.92983774302990696, 32.93378783738836546 ) ) ;
#59485 = CARTESIAN_POINT ( 'NONE',  ( 0.1152809850208375425, 20.21276301475716153, 39.22230862403461060 ) ) ;
#59486 = ORIENTED_EDGE ( 'NONE', *, *, #3246, .F. ) ;
#59487 = EDGE_CURVE ( 'NONE', #17561, #50265, #46749, .T. ) ;
#59488 = VERTEX_POINT ( 'NONE', #38479 ) ;
#59489 = CARTESIAN_POINT ( 'NONE',  ( 4.553261556744875094, 1.633632119647590697, -43.89613664004262716 ) ) ;
#59490 = CARTESIAN_POINT ( 'NONE',  ( 1.231276596079881047, 28.52807286890743654, 30.71523773966879745 ) ) ;
#59491 = AXIS2_PLACEMENT_3D ( 'NONE', #16862, #26232, #45375 ) ;
#59492 = VERTEX_POINT ( 'NONE', #9327 ) ;
#59493 = VERTEX_POINT ( 'NONE', #15282 ) ;
#59494 = CARTESIAN_POINT ( 'NONE',  ( 0.9757619758474602722, -0.06449181910561185838, -42.90842306541549078 ) ) ;
#59495 = CARTESIAN_POINT ( 'NONE',  ( 0.6008122571543325074, -25.82835962906537830, -41.76661812185638922 ) ) ;
#59496 = AXIS2_PLACEMENT_3D ( 'NONE', #33301, #56457, #52369 ) ;
#59497 = B_SPLINE_CURVE_WITH_KNOTS ( 'NONE', 3,
 ( #32737, #61212, #23330, #42760, #23029, #38074 ),
 .UNSPECIFIED., .F., .F.,
 ( 4, 2, 4 ),
 ( 0.000000000000000000, 0.0002293801035737088299, 0.0004587602071474176598 ),
 .UNSPECIFIED. ) ;
#59498 = CARTESIAN_POINT ( 'NONE',  ( 0.5998501479064708430, 23.59887241503295741, 41.92175333043627461 ) ) ;
#59499 = CARTESIAN_POINT ( 'NONE',  ( 4.975801465491694664, -47.84403947906841381, 2.564218696447319257 ) ) ;
#59500 = VERTEX_POINT ( 'NONE', #5833 ) ;
#59501 = CARTESIAN_POINT ( 'NONE',  ( 4.291220156522060236, -42.97446925027709597, -19.30243481954249773 ) ) ;
#59502 = CARTESIAN_POINT ( 'NONE',  ( 4.967162193818130511, 43.02067033766018511, 2.375726030842731706 ) ) ;
#59503 = CONICAL_SURFACE ( 'NONE', #32524, 43.08621763946400307, 1.568696531533066763 ) ;
#59504 = ORIENTED_EDGE ( 'NONE', *, *, #55010, .F. ) ;
#59505 = VERTEX_POINT ( 'NONE', #43180 ) ;
#59506 = CARTESIAN_POINT ( 'NONE',  ( 2.526552050251863690, -36.59987178591165957, -22.53110080776695412 ) ) ;
#59507 = FACE_OUTER_BOUND ( 'NONE', #7679, .T. ) ;
#59508 = CARTESIAN_POINT ( 'NONE',  ( 3.661921753702000348, 29.39588796543542060, 36.72210362380682369 ) ) ;
#59509 = ORIENTED_EDGE ( 'NONE', *, *, #11399, .T. ) ;
#59510 = CARTESIAN_POINT ( 'NONE',  ( -6.078457390727109555, -16.14063570603395803, -10.50116136637322484 ) ) ;
#59511 = CARTESIAN_POINT ( 'NONE',  ( 3.238018933889920792, -12.07617426668426575, -5.794265048159754627 ) ) ;
#59512 = CARTESIAN_POINT ( 'NONE',  ( 53.06478614550846373, 12.48216827162963405, 0.6888196380807342090 ) ) ;
#59513 = CARTESIAN_POINT ( 'NONE',  ( 0.6029303876144825880, -29.18200390284022205, -38.24575311129990496 ) ) ;
#59514 = VERTEX_POINT ( 'NONE', #53461 ) ;
#59515 = CARTESIAN_POINT ( 'NONE',  ( 0.8760168074886965917, 47.56749362999704545, 7.161346975773871470 ) ) ;
#59516 = ORIENTED_EDGE ( 'NONE', *, *, #1180, .F. ) ;
#59517 = ADVANCED_FACE ( 'NONE', ( #5531 ), #52341, .F. ) ;
#59518 = CARTESIAN_POINT ( 'NONE',  ( -90.00000000000000000, 8.434754829127421589E-16, 6.887500000000022382 ) ) ;
#59519 = CARTESIAN_POINT ( 'NONE',  ( 0.8554163680231708922, -13.02474486562516631, -45.07284652978098194 ) ) ;
#59520 = B_SPLINE_CURVE_WITH_KNOTS ( 'NONE', 3,
 ( #15177, #23951, #10468, #14567 ),
 .UNSPECIFIED., .F., .F.,
 ( 4, 4 ),
 ( 0.000000000000000000, 0.004442905043737213969 ),
 .UNSPECIFIED. ) ;
#59521 = EDGE_CURVE ( 'NONE', #36737, #50427, #10116, .T. ) ;
#59522 = PRESENTATION_STYLE_ASSIGNMENT (( #25713 ) ) ;
#59523 = CARTESIAN_POINT ( 'NONE',  ( -6.078075953587585900, -18.27673012847640166, -6.062698248962985481 ) ) ;
#59524 = CIRCLE ( 'NONE', #494, 10.00000000000000000 ) ;
#59525 = ORIENTED_EDGE ( 'NONE', *, *, #39159, .F. ) ;
#59526 = CARTESIAN_POINT ( 'NONE',  ( 4.833616638992208614, 43.64812679991120348, -15.29495699393680219 ) ) ;
#59527 = ADVANCED_FACE ( 'NONE', ( #4598 ), #58731, .F. ) ;
#59528 = CARTESIAN_POINT ( 'NONE',  ( 5.959547316686252039, -2.675599016784684814, 20.35048796920732173 ) ) ;
#59529 = CARTESIAN_POINT ( 'NONE',  ( 4.956653778116988818, -43.37017594958040689, -20.77844580450608447 ) ) ;
#59530 = CARTESIAN_POINT ( 'NONE',  ( 0.8560838555295223751, -2.480523550130904642, -46.84250032821665854 ) ) ;
#59531 = CARTESIAN_POINT ( 'NONE',  ( 4.963659409799330291, 14.83726297270280092, 42.22332985082316270 ) ) ;
#59532 = CARTESIAN_POINT ( 'NONE',  ( 0.9722240741986373225, -37.44729083276440207, 20.94823706911186534 ) ) ;
#59533 = FACE_OUTER_BOUND ( 'NONE', #13494, .T. ) ;
#59534 = CARTESIAN_POINT ( 'NONE',  ( 4.956445790443991584, 38.51510088324707226, 27.09474218539341450 ) ) ;
#59535 =( BOUNDED_SURFACE ( )  B_SPLINE_SURFACE ( 3, 1, ( 
 ( #55655, #7419 ),
 ( #56277, #60659 ),
 ( #61280, #41912 ),
 ( #60979, #13394 ) ),
 .UNSPECIFIED., .F., .F., .F. ) 
 B_SPLINE_SURFACE_WITH_KNOTS ( ( 4, 4 ),
 ( 2, 2 ),
 ( 0.000000000000000000, 1.000000000000000000 ),
 ( 0.000000000000000000, 1.000000000000000000 ),
 .UNSPECIFIED. ) 
 GEOMETRIC_REPRESENTATION_ITEM ( )  RATIONAL_B_SPLINE_SURFACE ( (
 ( 1.000000000000000000, 1.000000000000000000),
 ( 0.7282232189291693025, 0.9929344683865674037),
 ( 0.7282232189291693025, 0.9929344683865674037),
 ( 1.000000000000000000, 1.000000000000000000) ) ) 
 REPRESENTATION_ITEM ( '' )  SURFACE ( )  );
#59536 = AXIS2_PLACEMENT_3D ( 'NONE', #26519, #26206, #1460 ) ;
#59537 = ADVANCED_FACE ( 'NONE', ( #29059 ), #31609, .T. ) ;
#59538 = CARTESIAN_POINT ( 'NONE',  ( 4.303969348037258058, 16.39840148505153650, -45.22910199346958393 ) ) ;
#59539 = CARTESIAN_POINT ( 'NONE',  ( 0.1155031312995260795, 36.88774152132017292, 24.21231418076512298 ) ) ;
#59540 = ORIENTED_EDGE ( 'NONE', *, *, #16920, .F. ) ;
#59541 = CARTESIAN_POINT ( 'NONE',  ( 0.5987334363312691865, -19.32301417642171515, -45.14625155657866173 ) ) ;
#59542 = CIRCLE ( 'NONE', #48547, 48.91267123290010943 ) ;
#59543 = CARTESIAN_POINT ( 'NONE',  ( 5.959547316686252039, -18.96456592444106448, 7.851524054666073837 ) ) ;
#59544 = CARTESIAN_POINT ( 'NONE',  ( -7.853389858698435866, 8.173624800449486472, 5.691590806814991163E-14 ) ) ;
#59545 = ORIENTED_EDGE ( 'NONE', *, *, #634, .F. ) ;
#59546 = EDGE_CURVE ( 'NONE', #25455, #18232, #30300, .T. ) ;
#59547 = CARTESIAN_POINT ( 'NONE',  ( 5.860006189529234355, -9.426589201135168850, -47.30296539008834600 ) ) ;
#59548 = CARTESIAN_POINT ( 'NONE',  ( 5.896782393890504181, -15.78847575145207038, -12.45994062280484016 ) ) ;
#59549 = ADVANCED_FACE ( 'NONE', ( #35631 ), #58361, .F. ) ;
#59550 = CARTESIAN_POINT ( 'NONE',  ( 0.6009452777970410997, -12.87217382175461822, -46.35353542372318714 ) ) ;
#59551 =( BOUNDED_SURFACE ( )  B_SPLINE_SURFACE ( 3, 1, ( 
 ( #29420, #34758 ),
 ( #53825, #33525 ),
 ( #48527, #19126 ),
 ( #25038, #58216 ) ),
 .UNSPECIFIED., .F., .F., .F. ) 
 B_SPLINE_SURFACE_WITH_KNOTS ( ( 4, 4 ),
 ( 2, 2 ),
 ( 0.000000000000000000, 1.000000000000000000 ),
 ( 0.000000000000000000, 1.000000000000000000 ),
 .UNSPECIFIED. ) 
 GEOMETRIC_REPRESENTATION_ITEM ( )  RATIONAL_B_SPLINE_SURFACE ( (
 ( 1.000000000000000000, 1.000000000000000000),
 ( 0.9952954269826590483, 0.8620686068821339365),
 ( 0.9952954269826590483, 0.8620686068821339365),
 ( 1.000000000000000000, 1.000000000000000000) ) ) 
 REPRESENTATION_ITEM ( '' )  SURFACE ( )  );
#59552 = ORIENTED_EDGE ( 'NONE', *, *, #43591, .T. ) ;
#59553 = CARTESIAN_POINT ( 'NONE',  ( 4.214292481396495482, -11.25702090725073035, 0.000000000000000000 ) ) ;
#59554 = CARTESIAN_POINT ( 'NONE',  ( 4.967162193818130511, 42.16965968614205451, -8.839793687084773310 ) ) ;
#59555 = ORIENTED_EDGE ( 'NONE', *, *, #6397, .T. ) ;
#59556 = CARTESIAN_POINT ( 'NONE',  ( 2.600000000000000533, -11.64055411052240352, 0.000000000000000000 ) ) ;
#59557 = VERTEX_POINT ( 'NONE', #59087 ) ;
#59558 = ORIENTED_EDGE ( 'NONE', *, *, #21221, .T. ) ;
#59559 = CARTESIAN_POINT ( 'NONE',  ( 0.7764139734771241530, 21.75555916458111838, 41.55401444317116244 ) ) ;
#59560 = ORIENTED_EDGE ( 'NONE', *, *, #27240, .F. ) ;
#59561 = CARTESIAN_POINT ( 'NONE',  ( 0.7246131072078570989, 42.06185227555113926, -23.33689307364207721 ) ) ;
#59562 = EDGE_CURVE ( 'NONE', #44630, #13851, #53758, .T. ) ;
#59563 = B_SPLINE_CURVE_WITH_KNOTS ( 'NONE', 3,
 ( #54146, #51537, #36866, #44809 ),
 .UNSPECIFIED., .F., .F.,
 ( 4, 4 ),
 ( 0.000000000000000000, 0.005004948556313789688 ),
 .UNSPECIFIED. ) ;
#59564 = ORIENTED_EDGE ( 'NONE', *, *, #51896, .T. ) ;
#59565 = DIRECTION ( 'NONE',  ( 0.07906939808003035641, 0.3030506235706640905, -0.9496885541274535658 ) ) ;
#59566 =( REPRESENTATION_RELATIONSHIP ('NONE','NONE', #44881, #53251 ) REPRESENTATION_RELATIONSHIP_WITH_TRANSFORMATION ( #25177 )SHAPE_REPRESENTATION_RELATIONSHIP( ) );
#59567 = CARTESIAN_POINT ( 'NONE',  ( -6.016104459813374383, 2.464823636987713673, -18.68131780085928995 ) ) ;
#59568 = ORIENTED_EDGE ( 'NONE', *, *, #25244, .T. ) ;
#59569 = CARTESIAN_POINT ( 'NONE',  ( 4.553261556744875094, 0.000000000000000000, 0.000000000000000000 ) ) ;
#59570 = B_SPLINE_CURVE_WITH_KNOTS ( 'NONE', 3,
 ( #2572, #16080, #6950, #45223, #2257, #21387 ),
 .UNSPECIFIED., .F., .F.,
 ( 4, 2, 4 ),
 ( 1.523643551133495791E-16, 0.0002445252820015197861, 0.0004890505640028871333 ),
 .UNSPECIFIED. ) ;
#59571 = CARTESIAN_POINT ( 'NONE',  ( 3.661933894777883669, -5.960912430808857465, -46.65939013686185888 ) ) ;
#59572 = CARTESIAN_POINT ( 'NONE',  ( 0.1103744047535531458, -30.52096488484648518, 30.46616790811169295 ) ) ;
#59573 = CARTESIAN_POINT ( 'NONE',  ( 0.6254087463353930065, 13.11428234126299053, 46.28445368454758579 ) ) ;
#59574 = VERTEX_POINT ( 'NONE', #6757 ) ;
#59575 = B_SPLINE_CURVE_WITH_KNOTS ( 'NONE', 3,
 ( #43943, #39861, #49217, #33596 ),
 .UNSPECIFIED., .F., .F.,
 ( 4, 4 ),
 ( 3.273069708340168845E-17, 0.005004948556313846934 ),
 .UNSPECIFIED. ) ;
#59576 = EDGE_LOOP ( 'NONE', ( #33248, #61033, #21839, #56799 ) ) ;
#59577 = CARTESIAN_POINT ( 'NONE',  ( 0.7044674535452954967, -45.83030039157709012, 17.64614090470532659 ) ) ;
#59578 = CARTESIAN_POINT ( 'NONE',  ( -1.600000000000000089, -11.64055411052240352, 0.000000000000000000 ) ) ;
#59579 = CARTESIAN_POINT ( 'NONE',  ( 0.08486401232817714080, 0.000000000000000000, 0.000000000000000000 ) ) ;
#59580 = EDGE_LOOP ( 'NONE', ( #19995, #15011 ) ) ;
#59581 = DIRECTION ( 'NONE',  ( 0.000000000000000000, 0.000000000000000000, 1.000000000000000000 ) ) ;
#59582 = DIRECTION ( 'NONE',  ( -1.000000000000000000, 0.000000000000000000, 0.000000000000000000 ) ) ;
#59583 = CARTESIAN_POINT ( 'NONE',  ( 4.390527457369401532, 7.328357084871000460, -43.31836237746345120 ) ) ;
#59584 = EDGE_CURVE ( 'NONE', #33012, #11927, #45038, .T. ) ;
#59586 = ORIENTED_EDGE ( 'NONE', *, *, #43659, .F. ) ;
#59585 = AXIS2_PLACEMENT_3D ( 'NONE', #3694, #18137, #32865 ) ;
#59587 = VERTEX_POINT ( 'NONE', #7073 ) ;
#59588 = CARTESIAN_POINT ( 'NONE',  ( 0.8560838555295214869, 21.73747136795201129, -41.56747734237908531 ) ) ;
#59589 = CARTESIAN_POINT ( 'NONE',  ( 2.533389852662419894, 42.24569141318911392, 12.35929159601054295 ) ) ;
#59590 = ADVANCED_FACE ( 'NONE', ( #12133 ), #42622, .T. ) ;
#59591 = CARTESIAN_POINT ( 'NONE',  ( 0.3622758884714600280, 11.95365414648497193, -41.42293301073613776 ) ) ;
#59592 = VECTOR ( 'NONE', #13102, 1000.000000000000114 ) ;
#59593 = CARTESIAN_POINT ( 'NONE',  ( -6.078726893082806448, -12.94330610022628214, -14.25709887966570832 ) ) ;
#59594 = EDGE_CURVE ( 'NONE', #46515, #55636, #25901, .T. ) ;
#59595 = LINE ( 'NONE', #12027, #38126 ) ;
#59596 = CYLINDRICAL_SURFACE ( 'NONE', #6175, 0.7500000000000015543 ) ;
#59597 = EDGE_CURVE ( 'NONE', #17218, #12553, #4880, .T. ) ;
#59598 = CARTESIAN_POINT ( 'NONE',  ( 0.6031356755773454870, 12.45109777649109617, -46.46822857981031518 ) ) ;
#59599 = ADVANCED_FACE ( 'NONE', ( #39406 ), #53973, .F. ) ;
#59600 = DIRECTION ( 'NONE',  ( 0.000000000000000000, 0.000000000000000000, -1.000000000000000000 ) ) ;
#59601 = CARTESIAN_POINT ( 'NONE',  ( 0.5987334363312690755, 43.97851324882841340, 21.85070431118181844 ) ) ;
#59602 = CARTESIAN_POINT ( 'NONE',  ( 4.967162193818130511, 7.970725651240403664, -42.34252806656584056 ) ) ;
#59603 = CARTESIAN_POINT ( 'NONE',  ( -6.016489644550737204, -17.41053539857204768, 7.206912786933230564 ) ) ;
#59604 = LINE ( 'NONE', #35833, #2122 ) ;
#59605 = CYLINDRICAL_SURFACE ( 'NONE', #55471, 2.649999999999997691 ) ;
#59606 = CARTESIAN_POINT ( 'NONE',  ( 2.114184763561894886, 5.677447754278171364E-15, -44.03514965515262247 ) ) ;
#59607 = CARTESIAN_POINT ( 'NONE',  ( 0.9787464366903548818, -22.69932013610837274, 35.22889237896830394 ) ) ;
#59608 = CARTESIAN_POINT ( 'NONE',  ( 0.1084644655670282121, -0.3976617192055414418, -43.12277244437005663 ) ) ;
#59609 = EDGE_CURVE ( 'NONE', #38461, #50490, #41537, .T. ) ;
#59610 = CARTESIAN_POINT ( 'NONE',  ( 4.000000000000003553, -0.7779732554280840429, -5.566455648918319454 ) ) ;
#59611 = CARTESIAN_POINT ( 'NONE',  ( 0.6021447746440204973, 48.25112305616622876, 9.130731783772414900 ) ) ;
#59613 = VERTEX_POINT ( 'NONE', #39718 ) ;
#59612 = CARTESIAN_POINT ( 'NONE',  ( 0.8560838555295158248, 23.34035564869604684, -40.68907263964262455 ) ) ;
#59614 = ORIENTED_EDGE ( 'NONE', *, *, #52897, .T. ) ;
#59615 = B_SPLINE_CURVE_WITH_KNOTS ( 'NONE', 3,
 ( #2190, #51044, #31338, #60140 ),
 .UNSPECIFIED., .F., .F.,
 ( 4, 4 ),
 ( 7.589415207398531038E-19, 0.004444878191957666105 ),
 .UNSPECIFIED. ) ;
#59616 = DIRECTION ( 'NONE',  ( -1.000000000000000000, -1.836909530733573776E-16, 1.925929944387235853E-32 ) ) ;
#59617 = CARTESIAN_POINT ( 'NONE',  ( 4.956653778116966613, 0.000000000000000000, 0.000000000000000000 ) ) ;
#59619 = EDGE_CURVE ( 'NONE', #28607, #41301, #35012, .T. ) ;
#59618 = CARTESIAN_POINT ( 'NONE',  ( 0.7242003506640009025, 44.58862645969713867, 20.56370746153588058 ) ) ;
#59620 = ORIENTED_EDGE ( 'NONE', *, *, #14476, .T. ) ;
#59621 = ORIENTED_EDGE ( 'NONE', *, *, #32413, .T. ) ;
#59622 = CARTESIAN_POINT ( 'NONE',  ( 4.975610109902397937, -17.43163075979644816, -45.70106843599929647 ) ) ;
#59623 = CARTESIAN_POINT ( 'NONE',  ( 0.6009453534118440743, 5.846398087358736895, 47.75104957283900831 ) ) ;
#59624 = EDGE_CURVE ( 'NONE', #50243, #24298, #60920, .T. ) ;
#59625 = VERTEX_POINT ( 'NONE', #50928 ) ;
#59626 = VERTEX_POINT ( 'NONE', #3005 ) ;
#59627 = CARTESIAN_POINT ( 'NONE',  ( 0.6845945791218023269, 45.46290160446743300, 11.55556569002393452 ) ) ;
#59628 = CARTESIAN_POINT ( 'NONE',  ( 2.788021980263895028, 5.971756191165462832E-15, 46.99417130740431503 ) ) ;
#59629 = CARTESIAN_POINT ( 'NONE',  ( 0.5837799406558229487, -38.71456609132658855, -26.46556105465191067 ) ) ;
#59630 = VECTOR ( 'NONE', #23316, 1000.000000000000000 ) ;
#59631 = VERTEX_POINT ( 'NONE', #17129 ) ;
#59632 = CARTESIAN_POINT ( 'NONE',  ( 0.3622758884714730732, 40.13994584881760375, 15.73321244754868964 ) ) ;
#59633 = ADVANCED_FACE ( 'NONE', ( #22436 ), #28752, .F. ) ;
#59634 = EDGE_CURVE ( 'NONE', #21079, #45374, #3546, .T. ) ;
#59635 = B_SPLINE_CURVE_WITH_KNOTS ( 'NONE', 3,
 ( #4290, #14051, #61313, #27504 ),
 .UNSPECIFIED., .F., .F.,
 ( 4, 4 ),
 ( 2.256078575551061230E-17, 0.004564976165746191181 ),
 .UNSPECIFIED. ) ;
#59636 = CARTESIAN_POINT ( 'NONE',  ( 0.1129192098497447394, 14.78321943369649283, -41.57412910645673776 ) ) ;
#59637 = VERTEX_POINT ( 'NONE', #32776 ) ;
#59638 = ORIENTED_EDGE ( 'NONE', *, *, #42528, .F. ) ;
#59639 = CARTESIAN_POINT ( 'NONE',  ( 1.827326673878744367, 42.82501343454095633, -4.394636550976192879 ) ) ;
#59640 = CARTESIAN_POINT ( 'NONE',  ( 5.880360259849752858, -21.25991003419982661, 43.00389496650577570 ) ) ;
#59641 = ORIENTED_EDGE ( 'NONE', *, *, #23266, .T. ) ;
#59642 = CARTESIAN_POINT ( 'NONE',  ( 0.6001305935487422083, -11.94532529598410520, 46.60388846085702852 ) ) ;
#59643 = CARTESIAN_POINT ( 'NONE',  ( 0.6254087463353924514, 44.70339519268190998, 17.77193046492968520 ) ) ;
#59644 = CARTESIAN_POINT ( 'NONE',  ( 0.6009452777970412107, 46.57942614304341333, 12.02913818029328930 ) ) ;
#59645 = CARTESIAN_POINT ( 'NONE',  ( 2.879087469061463178, -43.82752541487803200, -3.905085503749960552 ) ) ;
#59646 = ORIENTED_EDGE ( 'NONE', *, *, #30346, .T. ) ;
#59647 = DIRECTION ( 'NONE',  ( -1.000000000000000000, -0.000000000000000000, -0.000000000000000000 ) ) ;
#59648 = CARTESIAN_POINT ( 'NONE',  ( 0.6029303876144825880, 18.28892193312799819, 44.49541906039135597 ) ) ;
#59649 = DIRECTION ( 'NONE',  ( -1.000000000000000000, -0.000000000000000000, -0.000000000000000000 ) ) ;
#59650 =( BOUNDED_SURFACE ( )  B_SPLINE_SURFACE ( 3, 1, ( 
 ( #32468, #42499 ),
 ( #36877, #56565 ),
 ( #31855, #18064 ),
 ( #46575, #26836 ) ),
 .UNSPECIFIED., .F., .F., .F. ) 
 B_SPLINE_SURFACE_WITH_KNOTS ( ( 4, 4 ),
 ( 2, 2 ),
 ( 0.000000000000000000, 1.000000000000000000 ),
 ( 0.000000000000000000, 1.000000000000000000 ),
 .UNSPECIFIED. ) 
 GEOMETRIC_REPRESENTATION_ITEM ( )  RATIONAL_B_SPLINE_SURFACE ( (
 ( 1.000000000000000000, 1.000000000000000000),
 ( 0.9953485035131437453, 0.8621029689291523912),
 ( 0.9953485035131437453, 0.8621029689291523912),
 ( 1.000000000000000000, 1.000000000000000000) ) ) 
 REPRESENTATION_ITEM ( '' )  SURFACE ( )  );
#59651 = CARTESIAN_POINT ( 'NONE',  ( 0.9752132459055864455, -21.65565338840788812, -37.04276540031529663 ) ) ;
#59652 = ORIENTED_EDGE ( 'NONE', *, *, #17944, .T. ) ;
#59653 = CARTESIAN_POINT ( 'NONE',  ( 0.6846871229502932144, 46.49193983736607549, -11.56285438919583797 ) ) ;
#59654 = CARTESIAN_POINT ( 'NONE',  ( 10.00000000000001599, -56.56854249492331377, -56.56854249492430142 ) ) ;
#59655 = DIRECTION ( 'NONE',  ( 0.000000000000000000, 0.000000000000000000, 1.000000000000000000 ) ) ;
#59656 = CARTESIAN_POINT ( 'NONE',  ( 4.975801465491695552, 15.94009207552985252, 45.18341283946464415 ) ) ;
#59657 = ORIENTED_EDGE ( 'NONE', *, *, #21671, .F. ) ;
#59658 = CARTESIAN_POINT ( 'NONE',  ( 0.8551540677456834771, -24.74404575822746466, -41.03346287276453097 ) ) ;
#59659 = CARTESIAN_POINT ( 'NONE',  ( 0.1101816497532063094, -42.73758747687833903, 5.763501205266392091 ) ) ;
#59660 = EDGE_CURVE ( 'NONE', #34351, #450, #45980, .T. ) ;
#59661 = B_SPLINE_CURVE_WITH_KNOTS ( 'NONE', 3,
 ( #14936, #487, #38749, #44379, #19629, #1405, #57804, #25233, #11150, #39670, #58115, #34045, #49344, #43765, #5487, #5180 ),
 .UNSPECIFIED., .F., .F.,
 ( 4, 3, 3, 3, 3, 4 ),
 ( 1.995049841954898532E-17, 0.0002618515315864414347, 0.0003927756766341999970, 0.0005236998216950569142, 0.0007855159896329919587, 0.001047349442285928304 ),
 .UNSPECIFIED. ) ;
#59662 = EDGE_CURVE ( 'NONE', #6071, #52266, #19910, .T. ) ;
#59663 = CARTESIAN_POINT ( 'NONE',  ( 5.895596859100789899, -13.98490190264553412, -14.45512718677593611 ) ) ;
#59664 = CARTESIAN_POINT ( 'NONE',  ( 0.2285344041767113366, 10.55674979585326234, 42.83755599988411689 ) ) ;
#59665 = DIRECTION ( 'NONE',  ( -1.000000000000000000, -1.836909530733580185E-16, 1.836909530733574022E-16 ) ) ;
#59666 = CARTESIAN_POINT ( 'NONE',  ( -6.063463321072278589, -18.27076090991269552, -6.082741836727592499 ) ) ;
#59667 = CARTESIAN_POINT ( 'NONE',  ( 1.231276596079887264, 29.74482033789320568, 29.53849072116790353 ) ) ;
#59668 = CARTESIAN_POINT ( 'NONE',  ( 0.8753041380234524160, 48.93739466471257060, -4.033575498629233813 ) ) ;
#59669 = CIRCLE ( 'NONE', #32688, 15.43999999999999240 ) ;
#59670 = EDGE_CURVE ( 'NONE', #43965, #4156, #49721, .T. ) ;
#59671 = CARTESIAN_POINT ( 'NONE',  ( 0.6026777506516367566, 41.06112623026730546, -26.93566972138011195 ) ) ;
#59672 = EDGE_CURVE ( 'NONE', #3477, #6245, #37779, .T. ) ;
#59673 = DIRECTION ( 'NONE',  ( -1.000000000000000000, -0.000000000000000000, -0.000000000000000000 ) ) ;
#59674 = ORIENTED_EDGE ( 'NONE', *, *, #8724, .T. ) ;
#59675 = AXIS2_PLACEMENT_3D ( 'NONE', #36194, #29929, #11445 ) ;
#59676 = VECTOR ( 'NONE', #28587, 999.9999999999998863 ) ;
#59677 = EDGE_CURVE ( 'NONE', #35241, #31407, #15344, .T. ) ;
#59678 = CARTESIAN_POINT ( 'NONE',  ( 5.959828726073459926, 17.77343634131827699, 10.26672511661762144 ) ) ;
#59679 = CARTESIAN_POINT ( 'NONE',  ( 4.960386119450153508, -30.07757850721712245, -31.77696863790710324 ) ) ;
#59680 = CARTESIAN_POINT ( 'NONE',  ( 6.999999999999991118, 80.00000000000001421, -2.649999999999999467 ) ) ;
#59681 = CARTESIAN_POINT ( 'NONE',  ( 0.5834584762367747146, -34.65810993668216611, -31.59195157995216263 ) ) ;
#59682 = CARTESIAN_POINT ( 'NONE',  ( -6.078726893082806448, 18.62710865126528859, 4.881072071039118221 ) ) ;
#59683 = CARTESIAN_POINT ( 'NONE',  ( 5.917102823773431552, 5.966888710896763648, -19.20640406644395171 ) ) ;
#59684 = ITEM_DEFINED_TRANSFORMATION ( 'NONE', 'NONE', #9903,  #14677 ) ;
#59685 = CARTESIAN_POINT ( 'NONE',  ( 0.5998501479064708430, -44.64337787626261189, 17.92509395669028649 ) ) ;
#59686 = EDGE_CURVE ( 'NONE', #20443, #10729, #7091, .T. ) ;
#59687 = CARTESIAN_POINT ( 'NONE',  ( 3.727782113643637096, 35.63527235512886904, -25.74694428629857867 ) ) ;
#59688 = CARTESIAN_POINT ( 'NONE',  ( 0.9785694773339246311, 29.29415779573593426, -29.96978019193998222 ) ) ;
#59690 = ORIENTED_EDGE ( 'NONE', *, *, #20257, .T. ) ;
#59689 = CARTESIAN_POINT ( 'NONE',  ( 0.7242003506639960175, -45.19983343645225915, 19.18298025445989907 ) ) ;
#59691 = ORIENTED_EDGE ( 'NONE', *, *, #20881, .T. ) ;
#59692 = FACE_OUTER_BOUND ( 'NONE', #12662, .T. ) ;
#59693 = CARTESIAN_POINT ( 'NONE',  ( 0.5806925824938499181, -8.338382001838064994, 46.14860504863594315 ) ) ;
#59694 = DIRECTION ( 'NONE',  ( -1.807003620809173399E-16, 1.000000000000000000, 0.000000000000000000 ) ) ;
#59695 = VERTEX_POINT ( 'NONE', #34015 ) ;
#59696 = CARTESIAN_POINT ( 'NONE',  ( 0.7954190325252787908, -38.68220061605148885, -28.58653703871143037 ) ) ;
#59697 = CARTESIAN_POINT ( 'NONE',  ( 0.6041374136657475802, 38.27243465845341319, -29.14743607025044980 ) ) ;
#59698 = B_SPLINE_CURVE_WITH_KNOTS ( 'NONE', 3,
 ( #28185, #60450, #47015, #27269 ),
 .UNSPECIFIED., .F., .F.,
 ( 4, 4 ),
 ( 8.355534721610420292E-17, 0.005004741218457496935 ),
 .UNSPECIFIED. ) ;
#59699 = ORIENTED_EDGE ( 'NONE', *, *, #59521, .T. ) ;
#59700 = ORIENTED_EDGE ( 'NONE', *, *, #52128, .T. ) ;
#59701 = DIRECTION ( 'NONE',  ( 1.000000000000000000, 0.000000000000000000, 0.000000000000000000 ) ) ;
#59702 = CARTESIAN_POINT ( 'NONE',  ( 4.975610109902397937, 0.000000000000000000, 0.000000000000000000 ) ) ;
#59703 = CARTESIAN_POINT ( 'NONE',  ( 5.974727161628369032, 7.868887636447618128, -18.95664195401509744 ) ) ;
#59704 = ORIENTED_EDGE ( 'NONE', *, *, #39777, .T. ) ;
#59705 = B_SPLINE_CURVE_WITH_KNOTS ( 'NONE', 3,
 ( #28076, #24928, #15222, #5169, #10206, #5777, #39658, #58099, #29001, #34329, #59029, #15836, #49030, #58403, #11137, #39045 ),
 .UNSPECIFIED., .F., .F.,
 ( 4, 3, 3, 3, 3, 4 ),
 ( 1.040890552917501732E-17, 0.0002732102107931913548, 0.0004098135523333831061, 0.0005464168938825005517, 0.0008195847345945455036, 0.001092771384553108084 ),
 .UNSPECIFIED. ) ;
#59706 = ORIENTED_EDGE ( 'NONE', *, *, #57759, .T. ) ;
#59707 = B_SPLINE_CURVE_WITH_KNOTS ( 'NONE', 3,
 ( #4232, #23067, #42196, #38726 ),
 .UNSPECIFIED., .F., .F.,
 ( 4, 4 ),
 ( 0.000000000000000000, 0.004447772540403804181 ),
 .UNSPECIFIED. ) ;
#59708 = CARTESIAN_POINT ( 'NONE',  ( 3.376099380956842921, 8.317686564981586983, 10.51306205816325701 ) ) ;
#59709 = DIRECTION ( 'NONE',  ( 0.000000000000000000, 0.000000000000000000, 1.000000000000000000 ) ) ;
#59710 = VERTEX_POINT ( 'NONE', #48399 ) ;
#59711 = EDGE_CURVE ( 'NONE', #4749, #26927, #16907, .T. ) ;
#59712 = CARTESIAN_POINT ( 'NONE',  ( 1.227938101723748288, -29.74462687941204209, -30.94118573761343782 ) ) ;
#59713 = CARTESIAN_POINT ( 'NONE',  ( 41.99999999999999289, 72.00000000000004263, -4.718528363748728716E-31 ) ) ;
#59714 = AXIS2_PLACEMENT_3D ( 'NONE', #6293, #43646, #25429 ) ;
#59715 = VERTEX_POINT ( 'NONE', #782 ) ;
#59716 = CARTESIAN_POINT ( 'NONE',  ( 4.975610109902397937, -44.31543648230385202, -20.70245146161840211 ) ) ;
#59717 = CARTESIAN_POINT ( 'NONE',  ( 0.5807400328401574052, -0.5448834511086588783, -47.89582301953904420 ) ) ;
#59718 = COLOUR_RGB ( '', 0.08235294, 0.09019608, 0.10196078) ;
#59719 = VERTEX_POINT ( 'NONE', #58086 ) ;
#59720 = VECTOR ( 'NONE', #12294, 1000.000000000000114 ) ;
#59721 = CARTESIAN_POINT ( 'NONE',  ( 0.8753041380234524160, 27.35839019124417248, -40.77568900725792389 ) ) ;
#59722 = CARTESIAN_POINT ( 'NONE',  ( 0.5837157313716021534, -19.82270906330415983, 42.50055610193381028 ) ) ;
#59723 = CARTESIAN_POINT ( 'NONE',  ( 0.7056313189692701160, 45.00499400157819707, -13.20224067631960274 ) ) ;
#59724 = CARTESIAN_POINT ( 'NONE',  ( 4.322998006666179727, -20.30542865297618960, -43.48102276965694557 ) ) ;
#59725 = B_SPLINE_CURVE_WITH_KNOTS ( 'NONE', 3,
 ( #2214, #26977, #45797, #26049 ),
 .UNSPECIFIED., .F., .F.,
 ( 4, 4 ),
 ( 0.000000000000000000, 0.004445488388166995118 ),
 .UNSPECIFIED. ) ;
#59726 = EDGE_LOOP ( 'NONE', ( #61346, #7879, #48548, #14325 ) ) ;
#59727 = CARTESIAN_POINT ( 'NONE',  ( 5.895596859100789899, -15.78680134203122165, 12.46214614742294913 ) ) ;
#59728 = CARTESIAN_POINT ( 'NONE',  ( 0.5806925824938494740, -19.24316026636509136, 42.76591101925167493 ) ) ;
#59729 = ORIENTED_EDGE ( 'NONE', *, *, #22912, .T. ) ;
#59730 = FACE_OUTER_BOUND ( 'NONE', #17344, .T. ) ;
#59731 =( BOUNDED_SURFACE ( )  B_SPLINE_SURFACE ( 3, 1, ( 
 ( #40879, #36167 ),
 ( #55231, #50541 ),
 ( #7619, #22054 ),
 ( #12666, #3228 ) ),
 .UNSPECIFIED., .F., .F., .F. ) 
 B_SPLINE_SURFACE_WITH_KNOTS ( ( 4, 4 ),
 ( 2, 2 ),
 ( 0.000000000000000000, 1.000000000000000000 ),
 ( 0.000000000000000000, 1.000000000000000000 ),
 .UNSPECIFIED. ) 
 GEOMETRIC_REPRESENTATION_ITEM ( )  RATIONAL_B_SPLINE_SURFACE ( (
 ( 1.000000000000000000, 1.000000000000000000),
 ( 0.9953040768229005630, 0.8617119497784937465),
 ( 0.9953040768229005630, 0.8617119497784937465),
 ( 1.000000000000000000, 1.000000000000000000) ) ) 
 REPRESENTATION_ITEM ( '' )  SURFACE ( )  );
#59732 = ORIENTED_EDGE ( 'NONE', *, *, #43622, .F. ) ;
#59733 = CARTESIAN_POINT ( 'NONE',  ( 0.5832367798473394593, -18.58036934788106009, 44.14510605973673307 ) ) ;
#59734 = ORIENTED_EDGE ( 'NONE', *, *, #19124, .F. ) ;
#59735 = LINE ( 'NONE', #41279, #54659 ) ;
#59737 = AXIS2_PLACEMENT_3D ( 'NONE', #53908, #1287, #11030 ) ;
#59736 = CARTESIAN_POINT ( 'NONE',  ( 0.9769922540276034795, 24.50223020450938449, 33.99959220478024946 ) ) ;
#59738 = CARTESIAN_POINT ( 'NONE',  ( 0.1135584504625006819, -43.81516248351064036, 5.213788323169063155 ) ) ;
#59739 = ORIENTED_EDGE ( 'NONE', *, *, #8000, .F. ) ;
#59740 = CARTESIAN_POINT ( 'NONE',  ( 0.1157991065609915854, -27.44727329912610259, -34.54836543138876692 ) ) ;
#59741 = CARTESIAN_POINT ( 'NONE',  ( 4.975801465491694664, -36.39623109580487892, 31.15993731089061924 ) ) ;
#59742 = ADVANCED_FACE ( 'NONE', ( #18673 ), #15615, .T. ) ;
#59743 = DIRECTION ( 'NONE',  ( -1.000000000000000000, -0.000000000000000000, -0.000000000000000000 ) ) ;
#59744 = EDGE_LOOP ( 'NONE', ( #54013, #6977, #54853, #33994 ) ) ;
#59745 = EDGE_CURVE ( 'NONE', #48631, #59245, #54919, .T. ) ;
#59746 = ORIENTED_EDGE ( 'NONE', *, *, #57454, .F. ) ;
#59747 = LINE ( 'NONE', #36278, #33542 ) ;
#59748 = CARTESIAN_POINT ( 'NONE',  ( 5.901764892641307547, 47.37867283933467633, -12.37953260115135734 ) ) ;
#59749 = CARTESIAN_POINT ( 'NONE',  ( 0.9783242366443563043, 38.68706413997891502, -16.11352098194802807 ) ) ;
#59750 = CARTESIAN_POINT ( 'NONE',  ( 2.299746137290198611, -15.18165008456612597, -46.62401568286382769 ) ) ;
#59751 = CARTESIAN_POINT ( 'NONE',  ( 5.895596859100789899, 12.98817590332826200, -15.35693556399487392 ) ) ;
#59752 = CARTESIAN_POINT ( 'NONE',  ( 5.719999999999998863, -15.99999999999998934, 1.959434878635764737E-15 ) ) ;
#59753 = EDGE_LOOP ( 'NONE', ( #40492, #18269, #51795, #17205 ) ) ;
#59754 = EDGE_CURVE ( 'NONE', #42198, #60067, #37622, .T. ) ;
#59755 = AXIS2_PLACEMENT_3D ( 'NONE', #51433, #42388, #8527 ) ;
#59756 = CARTESIAN_POINT ( 'NONE',  ( 3.680974057930773924, 46.78530430706938859, -10.62112035260193288 ) ) ;
#59757 = EDGE_CURVE ( 'NONE', #54380, #60616, #9600, .T. ) ;
#59758 = PLANE ( 'NONE',  #10840 ) ;
#59759 = ORIENTED_EDGE ( 'NONE', *, *, #51347, .T. ) ;
#59760 = EDGE_CURVE ( 'NONE', #28153, #58558, #30568, .T. ) ;
#59761 = CARTESIAN_POINT ( 'NONE',  ( 5.974727161628369032, 19.82156119440438147, 5.327229920347495096 ) ) ;
#59762 = CARTESIAN_POINT ( 'NONE',  ( 0.8744876279028306332, -34.64280934553560343, 34.78829991575276637 ) ) ;
#59763 = CARTESIAN_POINT ( 'NONE',  ( 0.6027444965799114707, 44.18742767652119596, 21.42451285839772623 ) ) ;
#59764 = CARTESIAN_POINT ( 'NONE',  ( 4.553261556744873317, -9.994631851593151595, -42.77437199977056537 ) ) ;
#59765 = CARTESIAN_POINT ( 'NONE',  ( 2.624215991343620935, 28.09277600149274789, -38.92973006074482356 ) ) ;
#59766 = CARTESIAN_POINT ( 'NONE',  ( -5.331200000000000827, 1.887314203987178256E-15, -15.38218000000000174 ) ) ;
#59767 = CARTESIAN_POINT ( 'NONE',  ( 0.9762797500689124330, -0.8945891712298984499, -41.89897964629236782 ) ) ;
#59768 = CARTESIAN_POINT ( 'NONE',  ( 0.1152809850208375703, -12.34233989415304755, -42.36286024841751185 ) ) ;
#59769 = CARTESIAN_POINT ( 'NONE',  ( 0.6000166863083106206, 27.66667954482573322, 40.57558779207487021 ) ) ;
#59770 = CARTESIAN_POINT ( 'NONE',  ( -6.016489644550737204, 18.20227673842151361, -4.872725758886001124 ) ) ;
#59771 = AXIS2_PLACEMENT_3D ( 'NONE', #13366, #18683, #33099 ) ;
#59772 = CARTESIAN_POINT ( 'NONE',  ( 0.8744876279028306332, 17.78802839418675674, 45.75954650373076049 ) ) ;
#59773 = B_SPLINE_CURVE_WITH_KNOTS ( 'NONE', 3,
 ( #18836, #4681, #24436, #5306, #52313, #14747 ),
 .UNSPECIFIED., .F., .F.,
 ( 4, 2, 4 ),
 ( 0.000000000000000000, 0.0002450742804987339593, 0.0004901485609974679187 ),
 .UNSPECIFIED. ) ;
#59775 = ADVANCED_FACE ( 'NONE', ( #61552 ), #26367, .F. ) ;
#59774 = CARTESIAN_POINT ( 'NONE',  ( 2.643462169533600914, 44.89050350746150997, -17.09809940585614996 ) ) ;
#59776 = AXIS2_PLACEMENT_3D ( 'NONE', #19934, #14614, #15223 ) ;
#59777 = CIRCLE ( 'NONE', #2703, 4.000000000000000000 ) ;
#59778 = CARTESIAN_POINT ( 'NONE',  ( 2.526464513654345545, 12.29060355381851188, 41.18424249084321076 ) ) ;
#59779 = CARTESIAN_POINT ( 'NONE',  ( 5.000000000000007994, -54.69470952477976766, 58.44237546506786884 ) ) ;
#59780 = CARTESIAN_POINT ( 'NONE',  ( 0.5804410086790514622, 40.07081992599716358, 24.36902218624511107 ) ) ;
#59781 = EDGE_CURVE ( 'NONE', #23596, #25998, #51933, .T. ) ;
#59782 = PRODUCT_DEFINITION_SHAPE ( 'NONE', 'NONE',  #61978 ) ;
#59783 = CARTESIAN_POINT ( 'NONE',  ( 2.526552050251864134, 29.52128340070600743, 31.23611603144874493 ) ) ;
#59784 = CARTESIAN_POINT ( 'NONE',  ( 4.549368137175248350, -18.79584381673559079, 38.59302160394720005 ) ) ;
#59785 = ORIENTED_EDGE ( 'NONE', *, *, #16394, .T. ) ;
#59786 = CARTESIAN_POINT ( 'NONE',  ( 0.1073791018717483448, 10.69234304550053949, -41.77800844988504991 ) ) ;
#59787 = CARTESIAN_POINT ( 'NONE',  ( 0.5835226383429296115, -19.90526368527538992, -42.46201775899989883 ) ) ;
#59788 = CARTESIAN_POINT ( 'NONE',  ( 0.9752132459055863345, -26.30543738863321579, -33.89922943039202607 ) ) ;
#59789 = CARTESIAN_POINT ( 'NONE',  ( 1.088908134280557105, -25.50067491870061431, 34.51503525510842962 ) ) ;
#59790 = CARTESIAN_POINT ( 'NONE',  ( 0.8744876279028306332, -6.955970791788286256, 48.60004650947653460 ) ) ;
#59791 = ORIENTED_EDGE ( 'NONE', *, *, #34749, .F. ) ;
#59792 = FACE_OUTER_BOUND ( 'NONE', #24471, .T. ) ;
#59793 = CARTESIAN_POINT ( 'NONE',  ( 5.959547316686252039, 14.51128755440541340, -14.51632612601513728 ) ) ;
#59794 = VECTOR ( 'NONE', #57419, 1000.000000000000114 ) ;
#59795 = CARTESIAN_POINT ( 'NONE',  ( 0.5997462898726536595, -13.47075269803155351, 47.22383351542719510 ) ) ;
#59796 = VERTEX_POINT ( 'NONE', #13988 ) ;
#59797 = EDGE_CURVE ( 'NONE', #45480, #37463, #12627, .T. ) ;
#59798 = CARTESIAN_POINT ( 'NONE',  ( 4.958415959904820092, -39.33684062738365839, -22.71160327406363422 ) ) ;
#59799 = ORIENTED_EDGE ( 'NONE', *, *, #52354, .F. ) ;
#59800 = CARTESIAN_POINT ( 'NONE',  ( -6.015611763856276717, 4.870987357968431297, -18.20278301740931681 ) ) ;
#59801 = CARTESIAN_POINT ( 'NONE',  ( 0.6030672727741701600, -29.35514790473179403, 38.11303703924417619 ) ) ;
#59802 = ORIENTED_EDGE ( 'NONE', *, *, #39719, .F. ) ;
#59803 = FACE_OUTER_BOUND ( 'NONE', #54616, .T. ) ;
#59804 = VERTEX_POINT ( 'NONE', #9884 ) ;
#59805 = CARTESIAN_POINT ( 'NONE',  ( 1.157644175074338699, 35.63734157974641192, 22.06767229699724453 ) ) ;
#59806 = CARTESIAN_POINT ( 'NONE',  ( 4.960386119450146403, -42.32154583640180334, -11.10509895001766090 ) ) ;
#59807 = ORIENTED_EDGE ( 'NONE', *, *, #13193, .F. ) ;
#59808 = CARTESIAN_POINT ( 'NONE',  ( 5.917102823773431552, -9.672968949170799746, -17.63301987068918208 ) ) ;
#59809 = ORIENTED_EDGE ( 'NONE', *, *, #51394, .T. ) ;
#59810 = CARTESIAN_POINT ( 'NONE',  ( 4.322998006666179727, -2.120302895115950381, -47.94177812210863721 ) ) ;
#59811 = ORIENTED_EDGE ( 'NONE', *, *, #31695, .T. ) ;
#59812 = ORIENTED_EDGE ( 'NONE', *, *, #22213, .T. ) ;
#59813 = CARTESIAN_POINT ( 'NONE',  ( -6.017396004339686577, -9.422598049764511430, -16.31807101179380126 ) ) ;
#59814 = LINE ( 'NONE', #46060, #44439 ) ;
#59815 = LINE ( 'NONE', #16927, #41467 ) ;
#59816 = DIRECTION ( 'NONE',  ( 0.09722883295013594329, -0.5223840607312690842, -0.8471490111763481101 ) ) ;
#59817 = CARTESIAN_POINT ( 'NONE',  ( 0.6846871229502932144, 33.25969555998742777, 34.48177377577847835 ) ) ;
#59818 = VERTEX_POINT ( 'NONE', #43418 ) ;
#59819 = CARTESIAN_POINT ( 'NONE',  ( 3.390910168358336918, 6.179655656472472280, 43.54203707339684826 ) ) ;
#59820 = CARTESIAN_POINT ( 'NONE',  ( 0.9783242366443540838, -17.88363875728391506, 37.90131864467907263 ) ) ;
#59821 = DIRECTION ( 'NONE',  ( -1.000000000000000000, 0.000000000000000000, 0.000000000000000000 ) ) ;
#59822 = ORIENTED_EDGE ( 'NONE', *, *, #55168, .T. ) ;
#59823 = ORIENTED_EDGE ( 'NONE', *, *, #54630, .F. ) ;
#59824 = CARTESIAN_POINT ( 'NONE',  ( -6.016761891674565099, 18.84319130225482297, 0.003433883959850178927 ) ) ;
#59825 = DIRECTION ( 'NONE',  ( -1.000000000000000000, -1.836909530733573776E-16, 1.925929944387235853E-32 ) ) ;
#59826 = DIRECTION ( 'NONE',  ( -1.000000000000000000, -5.380183451256491399E-17, -1.298891185607892835E-16 ) ) ;
#59827 = ORIENTED_EDGE ( 'NONE', *, *, #10609, .F. ) ;
#59828 = CARTESIAN_POINT ( 'NONE',  ( 0.6254087463353910081, -34.49952850220948619, -33.52637152047068980 ) ) ;
#59829 = CARTESIAN_POINT ( 'NONE',  ( 3.050102900204245682, -34.14444597521366376, 27.74134204078410448 ) ) ;
#59830 = CARTESIAN_POINT ( 'NONE',  ( -18.11268303252489176, -12.32233744059949743, 2.099999999999994760 ) ) ;
#59831 = ADVANCED_FACE ( 'NONE', ( #458 ), #32797, .F. ) ;
#59832 = AXIS2_PLACEMENT_3D ( 'NONE', #34966, #11774, #35271 ) ;
#59833 = ORIENTED_EDGE ( 'NONE', *, *, #36070, .F. ) ;
#59834 = CARTESIAN_POINT ( 'NONE',  ( -6.015611763856276717, -14.94556629257417590, -11.47596948473826650 ) ) ;
#59835 = ORIENTED_EDGE ( 'NONE', *, *, #18507, .F. ) ;
#59836 = ADVANCED_FACE ( 'NONE', ( #49944 ), #39210, .F. ) ;
#59837 = CARTESIAN_POINT ( 'NONE',  ( -2.739355103387247858, -11.80442426703883640, -9.138004961410429061 ) ) ;
#59838 = FACE_OUTER_BOUND ( 'NONE', #47491, .T. ) ;
#59839 = B_SPLINE_CURVE_WITH_KNOTS ( 'NONE', 3,
 ( #39182, #4370, #23507, #23825 ),
 .UNSPECIFIED., .F., .F.,
 ( 4, 4 ),
 ( 7.351626287044712563E-17, 0.005004741218457496067 ),
 .UNSPECIFIED. ) ;
#59840 = CARTESIAN_POINT ( 'NONE',  ( 1.500000000000001332, 0.000000000000000000, -7.400000000000022560 ) ) ;
#59841 = STYLED_ITEM ( 'NONE', ( #33826 ), #24273 ) ;
#59842 = EDGE_LOOP ( 'NONE', ( #40769, #12132, #16281, #31549 ) ) ;
#59843 = CARTESIAN_POINT ( 'NONE',  ( 0.9745511491811745808, 21.74846188963830329, -36.98831798234355972 ) ) ;
#59844 = CARTESIAN_POINT ( 'NONE',  ( 3.782625744892853970, -39.11333962259882213, 15.40729592310875695 ) ) ;
#59845 = CARTESIAN_POINT ( 'NONE',  ( 4.691466044806103852, -3.249105306918109726, -44.46979273209134220 ) ) ;
#59846 = CARTESIAN_POINT ( 'NONE',  ( 0.1073791018717483448, -16.95003405440287381, -39.65380858626208038 ) ) ;
#59847 = CARTESIAN_POINT ( 'NONE',  ( 0.9752132459055847802, 37.04276540031541742, -21.65565338840778153 ) ) ;
#59848 = CARTESIAN_POINT ( 'NONE',  ( 0.5988103564986355654, -44.21009236284897526, 18.96890181990811186 ) ) ;
#59849 = CARTESIAN_POINT ( 'NONE',  ( 0.9730545539215883499, 33.73144377768558400, 26.52009130076782739 ) ) ;
#59850 = ADVANCED_FACE ( 'NONE', ( #11125 ), #2760, .F. ) ;
#59851 = CARTESIAN_POINT ( 'NONE',  ( 0.8557997880470599172, 7.156447707086380561, -47.37054680076698077 ) ) ;
#59852 = CARTESIAN_POINT ( 'NONE',  ( 0.5832366564991513513, -29.37287047358855574, -37.83193087518338160 ) ) ;
#59853 = AXIS2_PLACEMENT_3D ( 'NONE', #54078, #29671, #54384 ) ;
#59854 = ORIENTED_EDGE ( 'NONE', *, *, #44390, .F. ) ;
#59855 = CIRCLE ( 'NONE', #17845, 0.02570000000000176310 ) ;
#59856 = CARTESIAN_POINT ( 'NONE',  ( 0.8560838555295223751, -18.91252766612315739, 42.92655508376904550 ) ) ;
#59857 = CARTESIAN_POINT ( 'NONE',  ( -6.016761891674565099, 18.68243340030205957, -2.456125503350522710 ) ) ;
#59858 = CARTESIAN_POINT ( 'NONE',  ( 0.8744876279028306332, 16.11801507201633399, -46.37412684372340266 ) ) ;
#59859 = ORIENTED_EDGE ( 'NONE', *, *, #42724, .T. ) ;
#59860 = CARTESIAN_POINT ( 'NONE',  ( 4.999999999999997335, 8.388739760877188892E-13, -80.00000000000001421 ) ) ;
#59861 = CARTESIAN_POINT ( 'NONE',  ( 0.2885700199627517781, -39.51953436244184559, 17.24062365614525305 ) ) ;
#59862 = ORIENTED_EDGE ( 'NONE', *, *, #42954, .T. ) ;
#59863 = CARTESIAN_POINT ( 'NONE',  ( 0.1129192098497447394, 3.754263797494919341, -43.96427289429421137 ) ) ;
#59864 = EDGE_CURVE ( 'NONE', #1874, #3017, #39635, .T. ) ;
#59865 = CARTESIAN_POINT ( 'NONE',  ( 0.9754402186311948997, -41.49454543482922730, -10.92425836141462803 ) ) ;
#59866 = ORIENTED_EDGE ( 'NONE', *, *, #51532, .F. ) ;
#59867 = CARTESIAN_POINT ( 'NONE',  ( 0.5850706913938534814, -47.46255051844958217, 6.431767090162647804 ) ) ;
#59868 = VECTOR ( 'NONE', #45237, 999.9999999999997726 ) ;
#59869 = VERTEX_POINT ( 'NONE', #1080 ) ;
#59870 = ORIENTED_EDGE ( 'NONE', *, *, #24358, .F. ) ;
#59871 = CARTESIAN_POINT ( 'NONE',  ( 0.9752132459055846692, -5.369621847647896296, 42.57112816680952960 ) ) ;
#59872 = ORIENTED_EDGE ( 'NONE', *, *, #50497, .T. ) ;
#59873 = FACE_OUTER_BOUND ( 'NONE', #26204, .T. ) ;
#59874 = B_SPLINE_CURVE_WITH_KNOTS ( 'NONE', 3,
 ( #25199, #53385, #54297, #6064, #777, #24910 ),
 .UNSPECIFIED., .F., .F.,
 ( 4, 2, 4 ),
 ( 0.004120275011746842714, 0.005288420935197119671, 0.006456566858647395761 ),
 .UNSPECIFIED. ) ;
#59875 = EDGE_CURVE ( 'NONE', #28712, #20981, #43618, .T. ) ;
#59876 = ORIENTED_EDGE ( 'NONE', *, *, #44796, .F. ) ;
#59877 = CARTESIAN_POINT ( 'NONE',  ( 5.917102823773431552, -7.220356195166304225, -18.77115272077518071 ) ) ;
#59878 = PRESENTATION_LAYER_ASSIGNMENT (  '', '', ( #35892 ) ) ;
#59879 = CARTESIAN_POINT ( 'NONE',  ( 0.9756008150404598123, 16.55159915785279168, 39.58764833544681494 ) ) ;
#59880 = EDGE_CURVE ( 'NONE', #25604, #14082, #49316, .T. ) ;
#59881 = EDGE_LOOP ( 'NONE', ( #45943, #10652, #7363, #5923 ) ) ;
#59882 = B_SPLINE_CURVE_WITH_KNOTS ( 'NONE', 3,
 ( #6483, #38832, #10932, #49128, #6180, #25626 ),
 .UNSPECIFIED., .F., .F.,
 ( 4, 2, 4 ),
 ( 1.474357996003774831E-17, 0.0002293319059085075146, 0.0004586638118170002841 ),
 .UNSPECIFIED. ) ;
#59883 = DIRECTION ( 'NONE',  ( 1.836766033387207149E-16, -1.000000000000000000, 0.000000000000000000 ) ) ;
#59884 = CARTESIAN_POINT ( 'NONE',  ( 0.8557997880470599172, 11.51622788066458369, 46.50333260518563350 ) ) ;
#59885 = CARTESIAN_POINT ( 'NONE',  ( 0.8751705887134423323, 5.393078191592057813, 47.79200036674281904 ) ) ;
#59886 = VECTOR ( 'NONE', #13643, 1000.000000000000000 ) ;
#59887 = CARTESIAN_POINT ( 'NONE',  ( 0.5998501479064708430, -41.39809967730470674, -24.50586714782589937 ) ) ;
#59888 = EDGE_LOOP ( 'NONE', ( #32519, #26073, #33016, #15878 ) ) ;
#59889 = CARTESIAN_POINT ( 'NONE',  ( 0.5836750258453349272, 44.18029554260635194, 18.49664649301206509 ) ) ;
#59890 = VERTEX_POINT ( 'NONE', #59017 ) ;
#59891 = CARTESIAN_POINT ( 'NONE',  ( 3.680974057930773924, -1.849713332884082684, 47.94008194857087091 ) ) ;
#59892 = CARTESIAN_POINT ( 'NONE',  ( 0.9754402186311939005, 26.26956909363317294, 33.92707563620654554 ) ) ;
#59893 = CARTESIAN_POINT ( 'NONE',  ( 4.553261556744875094, 12.71466023209559104, -42.04612920360213479 ) ) ;
#59894 = ORIENTED_EDGE ( 'NONE', *, *, #12329, .T. ) ;
#59895 = CARTESIAN_POINT ( 'NONE',  ( 0.1129192098497447394, 42.02659449688918869, 13.44310763102032702 ) ) ;
#59896 = CARTESIAN_POINT ( 'NONE',  ( 0.7948884756798503259, 46.31693274517635217, 16.29234131974172683 ) ) ;
#59897 = CARTESIAN_POINT ( 'NONE',  ( 0.6023142530420679819, -41.79260242564383532, -23.82662387835852158 ) ) ;
#59898 = EDGE_CURVE ( 'NONE', #38431, #38620, #20613, .T. ) ;
#59899 = CONICAL_SURFACE ( 'NONE', #878, 2.041999999999999815, 1.047197551196591858 ) ;
#59900 = AXIS2_PLACEMENT_3D ( 'NONE', #41209, #31163, #50270 ) ;
#59901 = EDGE_LOOP ( 'NONE', ( #50837, #26323, #53328, #39036 ) ) ;
#59902 = ORIENTED_EDGE ( 'NONE', *, *, #46280, .T. ) ;
#59903 = CARTESIAN_POINT ( 'NONE',  ( 5.896278296736517710, 0.6775463355849699054, -20.10144051001119436 ) ) ;
#59904 = CARTESIAN_POINT ( 'NONE',  ( 0.1103310638050662429, 34.16271402810833280, 26.31782144882252439 ) ) ;
#59905 = EDGE_CURVE ( 'NONE', #50801, #14312, #36328, .T. ) ;
#59906 = CARTESIAN_POINT ( 'NONE',  ( 0.5997462898726536595, 41.43917033312096265, 26.35046094941977302 ) ) ;
#59907 = CARTESIAN_POINT ( 'NONE',  ( 0.6041374136657476912, -47.67304777898703350, 6.452348380035114239 ) ) ;
#59908 = B_SPLINE_CURVE_WITH_KNOTS ( 'NONE', 3,
 ( #13884, #48304, #38615, #43319, #14494, #61447 ),
 .UNSPECIFIED., .F., .F.,
 ( 4, 2, 4 ),
 ( 1.015220885719448636E-17, 0.0002291978881530203343, 0.0004583957763060304770 ),
 .UNSPECIFIED. ) ;
#59909 = ADVANCED_FACE ( 'NONE', ( #5760 ), #48594, .F. ) ;
#59910 =( BOUNDED_SURFACE ( )  B_SPLINE_SURFACE ( 3, 1, ( 
 ( #47359, #13545 ),
 ( #8506, #37357 ),
 ( #27322, #17625 ),
 ( #3194, #4403 ) ),
 .UNSPECIFIED., .F., .F., .F. ) 
 B_SPLINE_SURFACE_WITH_KNOTS ( ( 4, 4 ),
 ( 2, 2 ),
 ( 0.000000000000000000, 1.000000000000000000 ),
 ( 0.000000000000000000, 1.000000000000000000 ),
 .UNSPECIFIED. ) 
 GEOMETRIC_REPRESENTATION_ITEM ( )  RATIONAL_B_SPLINE_SURFACE ( (
 ( 1.000000000000000000, 1.000000000000000000),
 ( 0.9952954269826590483, 0.8620686068821339365),
 ( 0.9952954269826590483, 0.8620686068821339365),
 ( 1.000000000000000000, 1.000000000000000000) ) ) 
 REPRESENTATION_ITEM ( '' )  SURFACE ( )  );
#59911 = CARTESIAN_POINT ( 'NONE',  ( 1.657374760986086271, -13.71672357020459643, -41.86576097183517930 ) ) ;
#59912 = CARTESIAN_POINT ( 'NONE',  ( 5.896278296736517710, 12.98123568145699736, -15.36276341667902479 ) ) ;
#59913 = CARTESIAN_POINT ( 'NONE',  ( 0.6030672727741701600, 12.53539249098714770, -46.44558360017000354 ) ) ;
#59914 = LINE ( 'NONE', #46458, #15847 ) ;
#59915 = VECTOR ( 'NONE', #28332, 1000.000000000000114 ) ;
#59916 = DIRECTION ( 'NONE',  ( 0.000000000000000000, 0.000000000000000000, 1.000000000000000000 ) ) ;
#59917 = DIRECTION ( 'NONE',  ( 0.000000000000000000, 0.000000000000000000, 1.000000000000000000 ) ) ;
#59918 = EDGE_CURVE ( 'NONE', #4178, #9990, #51578, .T. ) ;
#59919 = CARTESIAN_POINT ( 'NONE',  ( 3.050102900204245682, 41.14650753732696131, -15.56888456694172973 ) ) ;
#59920 = CARTESIAN_POINT ( 'NONE',  ( 0.5998501479064708430, -33.64490850298820845, -34.38546660123286358 ) ) ;
#59921 = CARTESIAN_POINT ( 'NONE',  ( 1.227938101723756947, 42.65467462194918369, 4.762198645644581951 ) ) ;
#59922 = CARTESIAN_POINT ( 'NONE',  ( 4.956653778116966613, 0.000000000000000000, 0.000000000000000000 ) ) ;
#59923 = DIRECTION ( 'NONE',  ( 1.000000000000000000, 0.000000000000000000, 0.000000000000000000 ) ) ;
#59924 =( BOUNDED_SURFACE ( )  B_SPLINE_SURFACE ( 3, 1, ( 
 ( #1974, #35526 ),
 ( #54904, #50219 ),
 ( #2594, #4731 ),
 ( #47083, #14188 ) ),
 .UNSPECIFIED., .F., .F., .F. ) 
 B_SPLINE_SURFACE_WITH_KNOTS ( ( 4, 4 ),
 ( 2, 2 ),
 ( 0.000000000000000000, 1.000000000000000000 ),
 ( 0.000000000000000000, 1.000000000000000000 ),
 .UNSPECIFIED. ) 
 GEOMETRIC_REPRESENTATION_ITEM ( )  RATIONAL_B_SPLINE_SURFACE ( (
 ( 1.000000000000000000, 1.000000000000000000),
 ( 0.7211978278499968642, 0.9934217856018975334),
 ( 0.7211978278499968642, 0.9934217856018975334),
 ( 1.000000000000000000, 1.000000000000000000) ) ) 
 REPRESENTATION_ITEM ( '' )  SURFACE ( )  );
#59925 = CARTESIAN_POINT ( 'NONE',  ( 5.965394784446460541, -18.95742317323939830, -7.868087674480889859 ) ) ;
#59926 = CARTESIAN_POINT ( 'NONE',  ( -6.017396004339686577, 18.68211039806563534, 2.458362590802854797 ) ) ;
#59927 = CARTESIAN_POINT ( 'NONE',  ( 4.553261556744875094, -36.69060082144763868, -24.15241969627107110 ) ) ;
#59929 = ORIENTED_EDGE ( 'NONE', *, *, #14859, .T. ) ;
#59928 = CARTESIAN_POINT ( 'NONE',  ( 0.6001305935487422083, 47.76436356026967900, -5.760103278697539686 ) ) ;
#59930 = ORIENTED_EDGE ( 'NONE', *, *, #44868, .T. ) ;
#59931 = CARTESIAN_POINT ( 'NONE',  ( 3.376099380956842921, -6.056959685666165605, -11.95916481190396041 ) ) ;
#59932 = CARTESIAN_POINT ( 'NONE',  ( 4.226256110419179812, 1.821314936738874568, -43.90341742835515504 ) ) ;
#59933 = CARTESIAN_POINT ( 'NONE',  ( -2.708315649062916552, -12.80362818457440710, -7.087851317223917036 ) ) ;
#59934 = ORIENTED_EDGE ( 'NONE', *, *, #27378, .T. ) ;
#59935 = ORIENTED_EDGE ( 'NONE', *, *, #34721, .T. ) ;
#59936 = CARTESIAN_POINT ( 'NONE',  ( -6.079354080745853928, 12.00499765711184708, -15.05566293794136179 ) ) ;
#59937 = CARTESIAN_POINT ( 'NONE',  ( -6.057079549204054558, -18.90023728169072470, -3.689479881436749764 ) ) ;
#59938 = UNCERTAINTY_MEASURE_WITH_UNIT (LENGTH_MEASURE( 1.000000000000000082E-05 ), #42091, 'distance_accuracy_value', 'NONE');
#59939 = AXIS2_PLACEMENT_3D ( 'NONE', #1752, #36233, #11810 ) ;
#59940 = ORIENTED_EDGE ( 'NONE', *, *, #44863, .T. ) ;
#59941 = ORIENTED_EDGE ( 'NONE', *, *, #14553, .F. ) ;
#59942 = CARTESIAN_POINT ( 'NONE',  ( 0.5837374860065638327, 47.89569815517037199, -0.1816420316517112499 ) ) ;
#59943 = AXIS2_PLACEMENT_3D ( 'NONE', #29855, #10140, #28933 ) ;
#59944 = CARTESIAN_POINT ( 'NONE',  ( 30.00000000000001421, -18.99999999999999289, 2.326828918379968998E-15 ) ) ;
#59945 = CARTESIAN_POINT ( 'NONE',  ( 0.5824935313925965197, -38.86802447473060340, -26.23956650719635775 ) ) ;
#59946 = EDGE_CURVE ( 'NONE', #31616, #43286, #7890, .T. ) ;
#59947 = ORIENTED_EDGE ( 'NONE', *, *, #20583, .T. ) ;
#59948 = CARTESIAN_POINT ( 'NONE',  ( 30.00000000000001066, 4.342925291379521108E-15, -1.386669559958810165E-30 ) ) ;
#59949 = ADVANCED_FACE ( 'NONE', ( #58388 ), #15592, .F. ) ;
#59950 = CARTESIAN_POINT ( 'NONE',  ( 0.7954196712028475114, -19.20650004025030100, 44.09776749253649086 ) ) ;
#59951 = B_SPLINE_CURVE_WITH_KNOTS ( 'NONE', 3,
 ( #12642, #32050, #22330, #7593, #17027, #55516, #21711, #27030, #32354, #13251, #17634, #16710, #3204, #40852, #36757, #55830, #36447, #50214, #51127 ),
 .UNSPECIFIED., .F., .F.,
 ( 4, 3, 3, 3, 3, 3, 4 ),
 ( 1.250973872328959318E-17, 0.0002732106629380587999, 0.0004098138914053716915, 0.0005464171197651381245, 0.0006830203481512576091, 0.0008196235766963599467, 0.001011968216111139643 ),
 .UNSPECIFIED. ) ;
#59952 = CARTESIAN_POINT ( 'NONE',  ( 0.1092355843206037486, 0.3005923759133873885, -43.12343565949664992 ) ) ;
#59953 = ORIENTED_EDGE ( 'NONE', *, *, #14428, .F. ) ;
#59954 = EDGE_CURVE ( 'NONE', #539, #58203, #55696, .T. ) ;
#59955 = ORIENTED_EDGE ( 'NONE', *, *, #48321, .F. ) ;
#59956 = CARTESIAN_POINT ( 'NONE',  ( -2.601141883200662974, 12.25953444924679658, -8.514648704269580648 ) ) ;
#59957 = CARTESIAN_POINT ( 'NONE',  ( 5.974727161628367256, 7.840226266082543916, -18.96851388233650582 ) ) ;
#59958 = AXIS2_PLACEMENT_3D ( 'NONE', #51966, #27555, #42596 ) ;
#59959 = VERTEX_POINT ( 'NONE', #36479 ) ;
#59960 = CARTESIAN_POINT ( 'NONE',  ( 5.895881250540457863, 14.91370150166961039, -13.49478377475528568 ) ) ;
#59961 = CARTESIAN_POINT ( 'NONE',  ( 0.6031357023905875581, 34.04794059289648800, -33.98625823839265081 ) ) ;
#59962 = CARTESIAN_POINT ( 'NONE',  ( 0.6031356755773454870, 46.46822857981026544, 12.45109777649125782 ) ) ;
#59963 = CARTESIAN_POINT ( 'NONE',  ( -2.739355103387247858, 11.53562761125311553, -9.475065306662095566 ) ) ;
#59964 = ORIENTED_EDGE ( 'NONE', *, *, #15560, .T. ) ;
#59965 = CARTESIAN_POINT ( 'NONE',  ( 2.648799415243696664, -48.79107182468962378, 4.893748408692157881 ) ) ;
#59966 = CARTESIAN_POINT ( 'NONE',  ( -2.708315649062910779, -7.087851317223882397, -12.80362818457442842 ) ) ;
#59967 = CARTESIAN_POINT ( 'NONE',  ( 0.7246131072078549895, 29.92944207473653506, -37.65685186358364689 ) ) ;
#59968 = DIRECTION ( 'NONE',  ( -1.000000000000000000, -0.000000000000000000, 1.925929944387235853E-32 ) ) ;
#59969 = ORIENTED_EDGE ( 'NONE', *, *, #8729, .F. ) ;
#59970 = CARTESIAN_POINT ( 'NONE',  ( 0.1104177457020372732, 42.75487793940123993, -5.633723015004433066 ) ) ;
#59971 = CARTESIAN_POINT ( 'NONE',  ( 1.500000000000001332, 0.000000000000000000, -6.728125000000023448 ) ) ;
#59972 = CARTESIAN_POINT ( 'NONE',  ( 4.962356264823608143, -28.94323483023595145, -30.55363735178127271 ) ) ;
#59973 = CARTESIAN_POINT ( 'NONE',  ( 0.3622758884714730732, 29.89648521331631414, -31.06363466427696807 ) ) ;
#59974 = EDGE_CURVE ( 'NONE', #49600, #40342, #12989, .T. ) ;
#59975 = VERTEX_POINT ( 'NONE', #42122 ) ;
#59976 = CARTESIAN_POINT ( 'NONE',  ( 4.335381028904201628, -40.49335964728638970, 27.56890770668767132 ) ) ;
#59977 = EDGE_CURVE ( 'NONE', #53499, #61466, #39208, .T. ) ;
#59978 = CARTESIAN_POINT ( 'NONE',  ( -2.708315649062916552, 12.54007339125014830, -7.544341609839853469 ) ) ;
#59979 = CARTESIAN_POINT ( 'NONE',  ( 0.9762797500689124330, 40.55021165774351743, 10.58324712448433580 ) ) ;
#59980 = EDGE_CURVE ( 'NONE', #10639, #2564, #31760, .T. ) ;
#59981 = CARTESIAN_POINT ( 'NONE',  ( 1.088313998177378172, -15.69908095455125796, -39.93881167962116052 ) ) ;
#59982 = CARTESIAN_POINT ( 'NONE',  ( 4.322998006666165516, 40.45864630878482870, 25.80712523194289432 ) ) ;
#59983 = CARTESIAN_POINT ( 'NONE',  ( 0.5807400328401637335, 11.87003418057307869, -46.40483864045133089 ) ) ;
#59984 = CARTESIAN_POINT ( 'NONE',  ( 0.7762783648524387292, -47.60264408896656363, -5.369627767360320547 ) ) ;
#59985 = CARTESIAN_POINT ( 'NONE',  ( 0.1101816497532063094, -41.68997876247040324, -11.03018586750479990 ) ) ;
#59986 = CARTESIAN_POINT ( 'NONE',  ( 0.5827357941260205010, 38.21849163199676980, 28.86820951701446702 ) ) ;
#59987 = CARTESIAN_POINT ( 'NONE',  ( 0.7762777257811908083, -19.15108781300962448, 43.90991299786893620 ) ) ;
#59988 = ORIENTED_EDGE ( 'NONE', *, *, #57069, .T. ) ;
#59989 = CARTESIAN_POINT ( 'NONE',  ( -6.016761891674565099, 2.462934516564073917, -18.68153697670638991 ) ) ;
#59990 = FACE_OUTER_BOUND ( 'NONE', #14654, .T. ) ;
#59991 = DIRECTION ( 'NONE',  ( -1.000000000000000000, -5.380183451256491399E-17, -1.298891185607892835E-16 ) ) ;
#59992 = CARTESIAN_POINT ( 'NONE',  ( 0.1135584504625007790, 44.05918809782512824, -2.395828937073182008 ) ) ;
#59993 = EDGE_CURVE ( 'NONE', #17686, #19345, #13797, .T. ) ;
#59994 = CARTESIAN_POINT ( 'NONE',  ( 0.5850706913938533704, 41.56998471741261625, -23.79070617305337976 ) ) ;
#59995 = APPLICATION_PROTOCOL_DEFINITION ( 'draft international standard', 'automotive_design', 1998, #15591 ) ;
#59996 = CARTESIAN_POINT ( 'NONE',  ( 0.8744876279028306332, -2.462621419132613454, -49.03351451941336592 ) ) ;
#59997 = CARTESIAN_POINT ( 'NONE',  ( 0.9780106845699478857, -7.279703251777206674, 41.27150550950986485 ) ) ;
#59998 = CARTESIAN_POINT ( 'NONE',  ( 0.9783242366443536397, 29.32669543984089700, -29.93792619379875575 ) ) ;
#60000 = EDGE_LOOP ( 'NONE', ( #1154, #52584, #15413, #56330 ) ) ;
#59999 = CARTESIAN_POINT ( 'NONE',  ( 4.960386119450145515, 42.78128882305005476, -9.175935446106471716 ) ) ;
#60001 = VERTEX_POINT ( 'NONE', #60866 ) ;
#60003 = AXIS2_PLACEMENT_3D ( 'NONE', #6724, #40614, #25867 ) ;
#60002 = FACE_OUTER_BOUND ( 'NONE', #15552, .T. ) ;
#60004 = CARTESIAN_POINT ( 'NONE',  ( 1.479689385636123067, -18.90469049123688805, -39.80196631698275667 ) ) ;
#60005 = CARTESIAN_POINT ( 'NONE',  ( 2.301430502907644726, -7.543848632415566691, 47.43735983879639662 ) ) ;
#60006 = CARTESIAN_POINT ( 'NONE',  ( -4.915099999999998914, 0.000000000000000000, 10.00000000000000000 ) ) ;
#60007 = ORIENTED_EDGE ( 'NONE', *, *, #29011, .F. ) ;
#60008 = CARTESIAN_POINT ( 'NONE',  ( 0.5998501479064699549, 12.95623334615437550, 46.33007877220744319 ) ) ;
#60009 = FACE_OUTER_BOUND ( 'NONE', #34642, .T. ) ;
#60010 = LINE ( 'NONE', #50005, #58046 ) ;
#60011 = ORIENTED_EDGE ( 'NONE', *, *, #33911, .F. ) ;
#60012 = ORIENTED_EDGE ( 'NONE', *, *, #26903, .F. ) ;
#60013 = CARTESIAN_POINT ( 'NONE',  ( 0.6001305935487315502, -17.92615948558509231, -44.64600790884048820 ) ) ;
#60014 = CARTESIAN_POINT ( 'NONE',  ( 0.1102847568649952675, -39.87696813145917929, -16.41780866919029336 ) ) ;
#60015 = FACE_OUTER_BOUND ( 'NONE', #24691, .T. ) ;
#60016 = ORIENTED_EDGE ( 'NONE', *, *, #19206, .T. ) ;
#60017 = EDGE_CURVE ( 'NONE', #1398, #34923, #30180, .T. ) ;
#60018 = EDGE_CURVE ( 'NONE', #12019, #855, #25755, .T. ) ;
#60019 = CARTESIAN_POINT ( 'NONE',  ( 0.1155031312995260795, -42.63802226078201585, -11.35520542398358579 ) ) ;
#60020 = CARTESIAN_POINT ( 'NONE',  ( 0.08486401232817714080, 0.000000000000000000, 0.000000000000000000 ) ) ;
#60021 = EDGE_LOOP ( 'NONE', ( #59121, #48005, #19768, #49948 ) ) ;
#60022 = B_SPLINE_CURVE_WITH_KNOTS ( 'NONE', 3,
 ( #41814, #23003, #42132, #17999 ),
 .UNSPECIFIED., .F., .F.,
 ( 4, 4 ),
 ( 1.843143693225357538E-18, 0.004444878191957663503 ),
 .UNSPECIFIED. ) ;
#60023 =( BOUNDED_SURFACE ( )  B_SPLINE_SURFACE ( 3, 1, ( 
 ( #38334, #57085 ),
 ( #56783, #9486 ),
 ( #33322, #48024 ),
 ( #28593, #23293 ) ),
 .UNSPECIFIED., .F., .F., .F. ) 
 B_SPLINE_SURFACE_WITH_KNOTS ( ( 4, 4 ),
 ( 2, 2 ),
 ( 0.000000000000000000, 1.000000000000000000 ),
 ( 0.000000000000000000, 1.000000000000000000 ),
 .UNSPECIFIED. ) 
 GEOMETRIC_REPRESENTATION_ITEM ( )  RATIONAL_B_SPLINE_SURFACE ( (
 ( 1.000000000000000000, 1.000000000000000000),
 ( 0.9754377213608244057, 0.9999580625633939235),
 ( 0.9754377213608244057, 0.9999580625633939235),
 ( 1.000000000000000000, 1.000000000000000000) ) ) 
 REPRESENTATION_ITEM ( '' )  SURFACE ( )  );
#60024 = DIRECTION ( 'NONE',  ( -1.000000000000000000, -0.000000000000000000, -0.000000000000000000 ) ) ;
#60025 = CARTESIAN_POINT ( 'NONE',  ( 0.000000000000000000, 0.000000000000000000, -1.199999999999999956 ) ) ;
#60026 = ORIENTED_EDGE ( 'NONE', *, *, #41598, .F. ) ;
#60027 = EDGE_CURVE ( 'NONE', #50598, #1887, #55599, .T. ) ;
#60028 = ADVANCED_FACE ( 'NONE', ( #7626 ), #28600, .T. ) ;
#60029 = FACE_OUTER_BOUND ( 'NONE', #14981, .T. ) ;
#60030 = CARTESIAN_POINT ( 'NONE',  ( 4.553261556744875094, 0.000000000000000000, 0.000000000000000000 ) ) ;
#60031 = ORIENTED_EDGE ( 'NONE', *, *, #12674, .F. ) ;
#60032 = CARTESIAN_POINT ( 'NONE',  ( 0.5806925824938499181, -7.260877859416734026, -46.33035738103254175 ) ) ;
#60033 = EDGE_CURVE ( 'NONE', #43892, #56469, #1579, .T. ) ;
#60034 = FACE_OUTER_BOUND ( 'NONE', #18075, .T. ) ;
#60035 = CARTESIAN_POINT ( 'NONE',  ( -2.339468227445729021, -3.268109542640674547, -5.599999999999982769 ) ) ;
#60036 = CARTESIAN_POINT ( 'NONE',  ( 2.643462169533613793, -40.89244134039129364, 25.20536747735708261 ) ) ;
#60037 = VERTEX_POINT ( 'NONE', #13282 ) ;
#60038 = CARTESIAN_POINT ( 'NONE',  ( -90.00000000000000000, 0.000000000000000000, -6.728125000000022560 ) ) ;
#60039 = CARTESIAN_POINT ( 'NONE',  ( 0.1149546198390368479, 39.87261812082539336, -18.89764242475886391 ) ) ;
#60040 = ORIENTED_EDGE ( 'NONE', *, *, #12201, .F. ) ;
#60041 = CARTESIAN_POINT ( 'NONE',  ( 0.1313383488274136590, 42.83318330237617744, 4.995828979989608065 ) ) ;
#60042 = AXIS2_PLACEMENT_3D ( 'NONE', #38719, #23669, #28061 ) ;
#60043 = EDGE_CURVE ( 'NONE', #14283, #29362, #21593, .T. ) ;
#60044 = ORIENTED_EDGE ( 'NONE', *, *, #45600, .F. ) ;
#60045 = CARTESIAN_POINT ( 'NONE',  ( 0.6001305935487422083, -17.92615948558511008, -44.64600790884048109 ) ) ;
#60046 = VERTEX_POINT ( 'NONE', #35860 ) ;
#60047 = CARTESIAN_POINT ( 'NONE',  ( 0.1310142868023686513, 41.48473022063163995, 11.77532653407853047 ) ) ;
#60048 = CARTESIAN_POINT ( 'NONE',  ( 0.5980894510889457338, -17.76188940524976800, 44.71414919659875409 ) ) ;
#60049 = ADVANCED_FACE ( 'NONE', ( #32389 ), #23629, .F. ) ;
#60050 = AXIS2_PLACEMENT_3D ( 'NONE', #1746, #49376, #35615 ) ;
#60051 = CARTESIAN_POINT ( 'NONE',  ( 0.1104177457020372871, -26.24862037251758196, 34.21590786698995856 ) ) ;
#60052 = ORIENTED_EDGE ( 'NONE', *, *, #47462, .T. ) ;
#60053 = CARTESIAN_POINT ( 'NONE',  ( 0.6001305935487315502, -44.24520387813841893, 18.89378601235985755 ) ) ;
#60054 = CARTESIAN_POINT ( 'NONE',  ( 1.000433927950263424, -0.7419564671726880389, 41.90308077282223564 ) ) ;
#60055 = CARTESIAN_POINT ( 'NONE',  ( 0.5806925824938502512, -41.60618895332704170, 21.63671424046659908 ) ) ;
#60056 = ORIENTED_EDGE ( 'NONE', *, *, #56174, .F. ) ;
#60057 = APPLICATION_CONTEXT ( 'automotive_design' ) ;
#60058 = ORIENTED_EDGE ( 'NONE', *, *, #24201, .T. ) ;
#60059 = CARTESIAN_POINT ( 'NONE',  ( 0.8557997880470599172, 17.48760788519217257, 44.60232077416692675 ) ) ;
#60060 = CARTESIAN_POINT ( 'NONE',  ( 0.5809828226811617480, -6.791453954330657794, 47.41188724015877654 ) ) ;
#60061 = CARTESIAN_POINT ( 'NONE',  ( 0.7056313189692676735, 27.13780443373282480, -38.25295040221118370 ) ) ;
#60062 = CARTESIAN_POINT ( 'NONE',  ( 4.549368137175248350, -35.80950303116083688, -23.67244292351627521 ) ) ;
#60063 = CARTESIAN_POINT ( 'NONE',  ( 0.5998501479064708430, -37.84527566984837677, -29.69975237324600315 ) ) ;
#60064 = ORIENTED_EDGE ( 'NONE', *, *, #46094, .F. ) ;
#60065 = CARTESIAN_POINT ( 'NONE',  ( 0.1073791018717483448, 37.10214135362888754, -21.98088480513627729 ) ) ;
#60066 = CARTESIAN_POINT ( 'NONE',  ( 4.967162193818130511, 38.83676580803792433, -18.65818244221215849 ) ) ;
#60067 = VERTEX_POINT ( 'NONE', #21745 ) ;
#60068 = CARTESIAN_POINT ( 'NONE',  ( 0.9758171775293914552, -30.33669560438090684, 30.34506652060231602 ) ) ;
#60069 = CARTESIAN_POINT ( 'NONE',  ( 4.956653778116973719, 27.17045123668471973, 39.67974989265048436 ) ) ;
#60070 = CARTESIAN_POINT ( 'NONE',  ( 4.549368137175248350, 40.58005590356690817, -13.99871866169321599 ) ) ;
#60071 = CARTESIAN_POINT ( 'NONE',  ( 0.1145239942831223490, -42.76278809080708498, 10.87609467618780457 ) ) ;
#60072 = ADVANCED_FACE ( 'NONE', ( #40884 ), #45246, .F. ) ;
#60073 = CARTESIAN_POINT ( 'NONE',  ( -2.739355103387247858, 7.136887160706410604, -13.11153723277179139 ) ) ;
#60074 = CARTESIAN_POINT ( 'NONE',  ( 4.956445790444041322, 46.25174887658561573, -8.849507104743011610 ) ) ;
#60075 = CARTESIAN_POINT ( 'NONE',  ( 0.8551540677456715978, -43.91216198251552072, 19.17641535420838039 ) ) ;
#60076 = CARTESIAN_POINT ( 'NONE',  ( 4.956445790443988031, 0.000000000000000000, 0.000000000000000000 ) ) ;
#60077 = EDGE_CURVE ( 'NONE', #36411, #8407, #44599, .T. ) ;
#60078 = FACE_OUTER_BOUND ( 'NONE', #24033, .T. ) ;
#60079 = CARTESIAN_POINT ( 'NONE',  ( 0.6000166863083106206, -35.63988196839337519, -33.78790160675033860 ) ) ;
#60080 = VECTOR ( 'NONE', #42402, 1000.000000000000000 ) ;
#60081 = CARTESIAN_POINT ( 'NONE',  ( 0.3676999524040323597, -0.5887207181719652516, -44.10900124961835900 ) ) ;
#60082 = LINE ( 'NONE', #9005, #33860 ) ;
#60083 = CARTESIAN_POINT ( 'NONE',  ( 0.5782707292762442330, -41.52883855096524712, -21.79660345823360146 ) ) ;
#60084 = FACE_OUTER_BOUND ( 'NONE', #2099, .T. ) ;
#60085 = CARTESIAN_POINT ( 'NONE',  ( 5.894904586330512508, 16.58261916749260223, -11.38183436918451186 ) ) ;
#60086 = CARTESIAN_POINT ( 'NONE',  ( 0.8751705887134553219, -37.60752970653848593, 29.98056538504896906 ) ) ;
#60087 = CARTESIAN_POINT ( 'NONE',  ( 0.5997462898726536595, 28.52220283460625438, 39.97543715340569292 ) ) ;
#60088 = VECTOR ( 'NONE', #26565, 1000.000000000000000 ) ;
#60089 = ORIENTED_EDGE ( 'NONE', *, *, #43894, .F. ) ;
#60090 = CARTESIAN_POINT ( 'NONE',  ( 5.895881250540457863, -2.017740640757351933, 20.01140685496492466 ) ) ;
#60091 = CARTESIAN_POINT ( 'NONE',  ( 0.8760168074886960365, 29.98565522133346306, -37.61398439004503302 ) ) ;
#60092 = CARTESIAN_POINT ( 'NONE',  ( 0.9730545539215883499, -25.71816799638802920, 34.34678117142546938 ) ) ;
#60093 = ORIENTED_EDGE ( 'NONE', *, *, #56624, .T. ) ;
#60094 = CARTESIAN_POINT ( 'NONE',  ( 0.9762797500689124330, -0.8945891712298984499, -41.89897964629236782 ) ) ;
#60095 = CARTESIAN_POINT ( 'NONE',  ( 3.238018933889920792, 6.194554405862141344, 11.87581525961341633 ) ) ;
#60096 = EDGE_CURVE ( 'NONE', #7798, #1309, #7769, .T. ) ;
#60097 = CARTESIAN_POINT ( 'NONE',  ( 0.5806925824938499181, -35.14454992382352572, 31.04968555388990836 ) ) ;
#60098 =( BOUNDED_SURFACE ( )  B_SPLINE_SURFACE ( 3, 1, ( 
 ( #33288, #38927 ),
 ( #5355, #5652 ),
 ( #24798, #43004 ),
 ( #38003, #14792 ) ),
 .UNSPECIFIED., .F., .F., .F. ) 
 B_SPLINE_SURFACE_WITH_KNOTS ( ( 4, 4 ),
 ( 2, 2 ),
 ( 0.000000000000000000, 1.000000000000000000 ),
 ( 0.000000000000000000, 1.000000000000000000 ),
 .UNSPECIFIED. ) 
 GEOMETRIC_REPRESENTATION_ITEM ( )  RATIONAL_B_SPLINE_SURFACE ( (
 ( 1.000000000000000000, 1.000000000000000000),
 ( 0.7282232189291693025, 0.9929344683865674037),
 ( 0.7282232189291693025, 0.9929344683865674037),
 ( 1.000000000000000000, 1.000000000000000000) ) ) 
 REPRESENTATION_ITEM ( '' )  SURFACE ( )  );
#60099 = ORIENTED_EDGE ( 'NONE', *, *, #40135, .T. ) ;
#60100 = ADVANCED_FACE ( 'NONE', ( #14216 ), #60023, .F. ) ;
#60101 = CARTESIAN_POINT ( 'NONE',  ( 1.827326673878744145, 43.03225468313000590, 1.232746109312326199 ) ) ;
#60102 = ORIENTED_EDGE ( 'NONE', *, *, #39057, .F. ) ;
#60103 = EDGE_CURVE ( 'NONE', #58608, #5237, #14825, .T. ) ;
#60104 = DIRECTION ( 'NONE',  ( 1.000000000000000000, 0.000000000000000000, 0.000000000000000000 ) ) ;
#60105 = CARTESIAN_POINT ( 'NONE',  ( 0.8554163680231816613, -8.703479761964905137, -46.10265624825630937 ) ) ;
#60106 = ORIENTED_EDGE ( 'NONE', *, *, #37223, .T. ) ;
#60107 = CARTESIAN_POINT ( 'NONE',  ( 0.6846871229502899947, 28.47437962186182858, -38.52803883689271203 ) ) ;
#60108 = ADVANCED_FACE ( 'NONE', ( #19222 ), #56595, .T. ) ;
#60109 = ORIENTED_EDGE ( 'NONE', *, *, #19960, .T. ) ;
#60110 = DIRECTION ( 'NONE',  ( -1.000000000000000000, -1.836909530733573776E-16, 1.925929944387235853E-32 ) ) ;
#60111 = CARTESIAN_POINT ( 'NONE',  ( 4.958415959904823644, -43.93947138327067137, -11.51202885600005210 ) ) ;
#60112 = EDGE_LOOP ( 'NONE', ( #13263, #35144, #50233, #56091 ) ) ;
#60113 = CARTESIAN_POINT ( 'NONE',  ( -6.057079549204054558, 13.83914966176556582, -13.39063731638611898 ) ) ;
#60114 = ORIENTED_EDGE ( 'NONE', *, *, #2112, .F. ) ;
#60115 = CARTESIAN_POINT ( 'NONE',  ( 5.895596859100789899, 16.58392706178521792, -11.37987462241457948 ) ) ;
#60116 = B_SPLINE_CURVE_WITH_KNOTS ( 'NONE', 3,
 ( #51516, #23043, #8606, #23960, #38389, #18974 ),
 .UNSPECIFIED., .F., .F.,
 ( 4, 2, 4 ),
 ( 9.745765416140531346E-18, 0.0002291978881530150488, 0.0004583957763060203397 ),
 .UNSPECIFIED. ) ;
#60117 = ORIENTED_EDGE ( 'NONE', *, *, #42104, .T. ) ;
#60118 = ORIENTED_EDGE ( 'NONE', *, *, #13457, .F. ) ;
#60119 = CARTESIAN_POINT ( 'NONE',  ( 5.910764540655177868, -15.77444817831453427, -12.47669920847786962 ) ) ;
#60120 = CARTESIAN_POINT ( 'NONE',  ( -13.59350196068900196, -12.08345367038092810, 3.000000000000023981 ) ) ;
#60121 = CARTESIAN_POINT ( 'NONE',  ( 4.956445790443991584, 39.12691469763999663, 26.20348443209871903 ) ) ;
#60122 = CARTESIAN_POINT ( 'NONE',  ( 5.958863334805807099, -19.82594244347349033, -5.313608583996449752 ) ) ;
#60123 = CARTESIAN_POINT ( 'NONE',  ( 4.833616638992205949, -46.17873762321150366, 2.572717262757815870 ) ) ;
#60124 = VERTEX_POINT ( 'NONE', #5386 ) ;
#60125 = CARTESIAN_POINT ( 'NONE',  ( 0.9749527285493316819, 10.82939760924503680, 41.51939261707886430 ) ) ;
#60126 = CARTESIAN_POINT ( 'NONE',  ( 0.9788927965476018622, -17.51217498749385371, 38.07440531169427089 ) ) ;
#60127 = EDGE_LOOP ( 'NONE', ( #20538, #56196, #43443, #21758 ) ) ;
#60128 = ORIENTED_EDGE ( 'NONE', *, *, #35991, .F. ) ;
#60129 = VECTOR ( 'NONE', #37147, 1000.000000000000000 ) ;
#60130 = CARTESIAN_POINT ( 'NONE',  ( -6.078457390727109555, -17.34717774342088248, 8.358823803363188532 ) ) ;
#60131 = CARTESIAN_POINT ( 'NONE',  ( 5.901764892641307547, 25.34839938110013335, 41.89809203598559861 ) ) ;
#60132 = CARTESIAN_POINT ( 'NONE',  ( 2.624215991343608501, -42.26352390376111856, 22.77108897942121857 ) ) ;
#60133 = ORIENTED_EDGE ( 'NONE', *, *, #43869, .F. ) ;
#60134 = CARTESIAN_POINT ( 'NONE',  ( 0.1073791018717578927, -43.12183934961191056, -0.4849339620931655825 ) ) ;
#60135 = CARTESIAN_POINT ( 'NONE',  ( 0.7413678028165011646, -34.77333832429343374, 27.11643475006381721 ) ) ;
#60136 = ORIENTED_EDGE ( 'NONE', *, *, #4638, .F. ) ;
#60137 = CARTESIAN_POINT ( 'NONE',  ( 0.3676999524040323597, 25.91024933382809436, -35.70167450949183774 ) ) ;
#60138 = ORIENTED_EDGE ( 'NONE', *, *, #16286, .F. ) ;
#60139 = LINE ( 'NONE', #25396, #21366 ) ;
#60140 = CARTESIAN_POINT ( 'NONE',  ( 4.956653778116974607, -32.11725092155068495, 35.79382859084104496 ) ) ;
#60141 = CARTESIAN_POINT ( 'NONE',  ( 0.9783242366443560822, 9.975869637871808138, -40.70401104528534120 ) ) ;
#60142 =( LENGTH_UNIT ( ) NAMED_UNIT ( * ) SI_UNIT ( .MILLI., .METRE. ) );
#60143 = DIRECTION ( 'NONE',  ( -0.1011922191286467737, -0.7658109114536917339, 0.6350541572860427531 ) ) ;
#60144 = EDGE_CURVE ( 'NONE', #57948, #25296, #35427, .T. ) ;
#60145 = ORIENTED_EDGE ( 'NONE', *, *, #20960, .T. ) ;
#60146 = CARTESIAN_POINT ( 'NONE',  ( 0.6845945791218023269, -44.02134436206650037, 16.20270845477079646 ) ) ;
#60147 = DIRECTION ( 'NONE',  ( -1.000000000000000000, -0.000000000000000000, -0.000000000000000000 ) ) ;
#60148 = DIRECTION ( 'NONE',  ( -1.000000000000000000, -0.000000000000000000, -0.000000000000000000 ) ) ;
#60149 = CARTESIAN_POINT ( 'NONE',  ( 0.1102144999581333024, 21.67128446981380208, -37.28370465375335385 ) ) ;
#60150 = CARTESIAN_POINT ( 'NONE',  ( 0.9730545539215883499, -33.73144377768539215, -26.52009130076805832 ) ) ;
#60151 = CARTESIAN_POINT ( 'NONE',  ( 4.956653778116975495, -35.79382859084138602, 32.11725092155030836 ) ) ;
#60152 = CARTESIAN_POINT ( 'NONE',  ( -49.49999999999975842, -5.000000000000000000, 6.123233995736873765E-16 ) ) ;
#60153 = CARTESIAN_POINT ( 'NONE',  ( -6.015611763856276717, -7.216738110653151850, -17.40650793417851361 ) ) ;
#60154 = CARTESIAN_POINT ( 'NONE',  ( 4.975610109902397937, 0.000000000000000000, 0.000000000000000000 ) ) ;
#60155 = FACE_OUTER_BOUND ( 'NONE', #37966, .T. ) ;
#60156 = CARTESIAN_POINT ( 'NONE',  ( 0.5988103622719989083, 33.58571533649112695, 34.44344971428038349 ) ) ;
#60157 = ORIENTED_EDGE ( 'NONE', *, *, #11796, .T. ) ;
#60158 = CARTESIAN_POINT ( 'NONE',  ( 2.706805983486679779, -3.064257645287458587, -43.90200950301765204 ) ) ;
#60159 = CARTESIAN_POINT ( 'NONE',  ( 0.5782707292762423457, 10.16715070324166881, -45.78608304152248110 ) ) ;
#60160 = CARTESIAN_POINT ( 'NONE',  ( 53.14999999999999858, 15.50000000000000711, 1.598617295522242905E-15 ) ) ;
#60161 = ORIENTED_EDGE ( 'NONE', *, *, #6711, .T. ) ;
#60162 = ADVANCED_FACE ( 'NONE', ( #19523 ), #37721, .T. ) ;
#60163 = CARTESIAN_POINT ( 'NONE',  ( 4.975610109902397937, -33.30777373088848492, -35.81957029655308133 ) ) ;
#60164 = CARTESIAN_POINT ( 'NONE',  ( 0.6008123274975393224, 44.43158642411502512, -20.91383941305027605 ) ) ;
#60165 = EDGE_CURVE ( 'NONE', #3794, #40968, #46609, .T. ) ;
#60166 = CARTESIAN_POINT ( 'NONE',  ( 4.553261556744875094, 0.000000000000000000, 0.000000000000000000 ) ) ;
#60167 = AXIS2_PLACEMENT_3D ( 'NONE', #23195, #22893, #13190 ) ;
#60168 = ORIENTED_EDGE ( 'NONE', *, *, #39856, .T. ) ;
#60169 = DIRECTION ( 'NONE',  ( -0.000000000000000000, 1.000000000000000000, 1.224646799147353207E-16 ) ) ;
#60170 = CARTESIAN_POINT ( 'NONE',  ( 0.9749527285493289064, -41.37154756071288375, -11.38116287125098047 ) ) ;
#60171 = EDGE_CURVE ( 'NONE', #20018, #10739, #21991, .T. ) ;
#60172 = CARTESIAN_POINT ( 'NONE',  ( -6.078075953587585900, -19.21613803895143491, -1.239037172606074488 ) ) ;
#60174 = ORIENTED_EDGE ( 'NONE', *, *, #34770, .T. ) ;
#60173 =( BOUNDED_SURFACE ( )  B_SPLINE_SURFACE ( 3, 1, ( 
 ( #19439, #57611 ),
 ( #15364, #57301 ),
 ( #297, #52622 ),
 ( #14745, #38256 ) ),
 .UNSPECIFIED., .F., .F., .F. ) 
 B_SPLINE_SURFACE_WITH_KNOTS ( ( 4, 4 ),
 ( 2, 2 ),
 ( 0.000000000000000000, 1.000000000000000000 ),
 ( 0.000000000000000000, 1.000000000000000000 ),
 .UNSPECIFIED. ) 
 GEOMETRIC_REPRESENTATION_ITEM ( )  RATIONAL_B_SPLINE_SURFACE ( (
 ( 1.000000000000000000, 1.000000000000000000),
 ( 0.9953485035131437453, 0.8621029689291515030),
 ( 0.9953485035131437453, 0.8621029689291515030),
 ( 1.000000000000000000, 1.000000000000000000) ) ) 
 REPRESENTATION_ITEM ( '' )  SURFACE ( )  );
#60175 = CARTESIAN_POINT ( 'NONE',  ( 0.5998501479064708430, 28.86886762351073088, 38.48283596222038483 ) ) ;
#60176 = ORIENTED_EDGE ( 'NONE', *, *, #22806, .T. ) ;
#60177 = EDGE_CURVE ( 'NONE', #12115, #17815, #43970, .T. ) ;
#60178 = EDGE_LOOP ( 'NONE', ( #42530, #34571 ) ) ;
#60179 = CARTESIAN_POINT ( 'NONE',  ( 0.9730545539215883499, -5.099196237955184507, 42.60426903087352457 ) ) ;
#60180 = ORIENTED_EDGE ( 'NONE', *, *, #49357, .T. ) ;
#60181 = CARTESIAN_POINT ( 'NONE',  ( 0.5980271706414711508, -49.10762822256506865, -0.7000665654016452466 ) ) ;
#60182 = VERTEX_POINT ( 'NONE', #44893 ) ;
#60183 = CARTESIAN_POINT ( 'NONE',  ( -5.995132425357893702, 16.31525984181033095, 9.429450169548012184 ) ) ;
#60184 = CARTESIAN_POINT ( 'NONE',  ( 2.044598208318018973, -0.02734949455884180813, 44.03824229377359245 ) ) ;
#60185 = ORIENTED_EDGE ( 'NONE', *, *, #9195, .T. ) ;
#60186 = CARTESIAN_POINT ( 'NONE',  ( 5.896782393890504181, -19.39652907507979052, 5.319844614046219000 ) ) ;
#60187 = EDGE_CURVE ( 'NONE', #14690, #3069, #24191, .T. ) ;
#60188 = FACE_OUTER_BOUND ( 'NONE', #26075, .T. ) ;
#60189 = CARTESIAN_POINT ( 'NONE',  ( 4.975610109902397937, -43.81605102859442979, -21.73943604138302987 ) ) ;
#60190 = LINE ( 'NONE', #31391, #61626 ) ;
#60191 = ORIENTED_EDGE ( 'NONE', *, *, #1552, .T. ) ;
#60192 = CARTESIAN_POINT ( 'NONE',  ( 4.833616638992205949, -30.15290813935876812, -35.06988470649558565 ) ) ;
#60193 = EDGE_CURVE ( 'NONE', #60737, #19581, #27200, .T. ) ;
#60194 = ORIENTED_EDGE ( 'NONE', *, *, #42028, .T. ) ;
#60195 = CARTESIAN_POINT ( 'NONE',  ( 0.5797568599927139799, -30.75502584278100215, 35.40273568639684498 ) ) ;
#60196 = CARTESIAN_POINT ( 'NONE',  ( 0.8751705887134553219, 47.55935879196470495, -7.160166390003808168 ) ) ;
#60197 = CARTESIAN_POINT ( 'NONE',  ( 4.553261556744873317, -24.94552653848474222, 36.15605442441679429 ) ) ;
#60198 = VERTEX_POINT ( 'NONE', #39885 ) ;
#60199 = FACE_OUTER_BOUND ( 'NONE', #37053, .T. ) ;
#60200 = CARTESIAN_POINT ( 'NONE',  ( 0.7413678028165010536, 8.900374941533167217, -43.18876494726807636 ) ) ;
#60201 = CARTESIAN_POINT ( 'NONE',  ( 0.5998501479064708430, -41.39809967730470674, -24.50586714782589937 ) ) ;
#60202 = VERTEX_POINT ( 'NONE', #58620 ) ;
#60203 = ORIENTED_EDGE ( 'NONE', *, *, #49623, .F. ) ;
#60204 = CARTESIAN_POINT ( 'NONE',  ( 0.8554163680231720024, -0.6539261334255729308, 46.91244881397518895 ) ) ;
#60205 = CARTESIAN_POINT ( 'NONE',  ( 0.3676999524040366896, 42.11837424242170158, 13.11461530118771179 ) ) ;
#60206 = DIRECTION ( 'NONE',  ( -1.000000000000000000, -0.000000000000000000, -0.000000000000000000 ) ) ;
#60207 = CARTESIAN_POINT ( 'NONE',  ( -6.077587904424778920, -18.27702681447052768, 6.061873655649367088 ) ) ;
#60208 = STYLED_ITEM ( 'NONE', ( #50078 ), #30206 ) ;
#60209 = EDGE_CURVE ( 'NONE', #16660, #38361, #38423, .T. ) ;
#60210 = CARTESIAN_POINT ( 'NONE',  ( 0.5824936645240084143, 5.056360923409078723, -46.62264893002680566 ) ) ;
#60211 = CARTESIAN_POINT ( 'NONE',  ( 0.7764139734771229318, -24.48247842768736149, -40.00810819002430208 ) ) ;
#60212 = CARTESIAN_POINT ( 'NONE',  ( -31.74999999999995737, 0.000000000000000000, 0.000000000000000000 ) ) ;
#60213 = CARTESIAN_POINT ( 'NONE',  ( 4.962356264823608143, 0.000000000000000000, 0.000000000000000000 ) ) ;
#60214 = CARTESIAN_POINT ( 'NONE',  ( 4.549368137175248350, -13.99871866169335810, -40.58005590356685843 ) ) ;
#60215 = FACE_OUTER_BOUND ( 'NONE', #5173, .T. ) ;
#60216 = CARTESIAN_POINT ( 'NONE',  ( 3.221118495291108719, 41.11142598507491641, -15.64007906423297101 ) ) ;
#60217 = CARTESIAN_POINT ( 'NONE',  ( 0.5834584762367742705, -13.72010822659117046, -44.84411465581428047 ) ) ;
#60218 = CARTESIAN_POINT ( 'NONE',  ( 5.974727161628367256, 20.34732802718247768, -2.694421823322708853 ) ) ;
#60219 = CARTESIAN_POINT ( 'NONE',  ( 0.5998501479064708430, -5.759754759340450114, -47.76154736470756745 ) ) ;
#60220 = CARTESIAN_POINT ( 'NONE',  ( 0.1102847568649952675, -0.09217763870870740450, -43.12433804869904463 ) ) ;
#60221 = CARTESIAN_POINT ( 'NONE',  ( 0.6008122571543325074, 17.36801345829917054, 45.93372028235526727 ) ) ;
#60222 = CARTESIAN_POINT ( 'NONE',  ( 4.549368137175248350, 8.166781970325731166, -42.14271863032826104 ) ) ;
#60224 = EDGE_LOOP ( 'NONE', ( #15684, #38505 ) ) ;
#60223 = CARTESIAN_POINT ( 'NONE',  ( 4.322998006666179727, 47.25487450103535991, -8.359821156455987889 ) ) ;
#60226 = ORIENTED_EDGE ( 'NONE', *, *, #50907, .F. ) ;
#60225 = B_SPLINE_CURVE_WITH_KNOTS ( 'NONE', 3,
 ( #10146, #58654, #29242, #44005 ),
 .UNSPECIFIED., .F., .F.,
 ( 4, 4 ),
 ( 1.084202172485504434E-18, 0.004048833967417089959 ),
 .UNSPECIFIED. ) ;
#60227 = CARTESIAN_POINT ( 'NONE',  ( 4.956653778116982600, -47.05699031914957686, 9.917440902360995736 ) ) ;
#60228 = CARTESIAN_POINT ( 'NONE',  ( 1.657374760986086271, 2.996577793790630384, -43.95350917478609176 ) ) ;
#60229 = CARTESIAN_POINT ( 'NONE',  ( -6.010958268070873523, -13.31406649671953168, -13.33459572764771650 ) ) ;
#60230 = EDGE_LOOP ( 'NONE', ( #43231, #43657, #29387, #47821 ) ) ;
#60231 = ORIENTED_EDGE ( 'NONE', *, *, #55941, .F. ) ;
#60232 = DIRECTION ( 'NONE',  ( 0.000000000000000000, 0.000000000000000000, 1.000000000000000000 ) ) ;
#60233 = CARTESIAN_POINT ( 'NONE',  ( 4.960156602257181468, -20.99019478193080701, 41.40608197274629276 ) ) ;
#60234 = ORIENTED_EDGE ( 'NONE', *, *, #3537, .F. ) ;
#60235 = EDGE_LOOP ( 'NONE', ( #14542, #31441, #5603, #24601 ) ) ;
#60236 = CARTESIAN_POINT ( 'NONE',  ( 4.958415959904820092, -38.82150677285500961, -23.58165739950888096 ) ) ;
#60237 = EDGE_CURVE ( 'NONE', #52026, #40574, #8542, .T. ) ;
#60238 = CARTESIAN_POINT ( 'NONE',  ( 4.956653778116990594, -35.79382859084093127, -32.11725092155079864 ) ) ;
#60239 = CARTESIAN_POINT ( 'NONE',  ( 0.5806925824938502512, 11.40214825760292250, 45.48860711711456872 ) ) ;
#60240 = ADVANCED_FACE ( 'NONE', ( #5682 ), #55254, .F. ) ;
#60241 = ORIENTED_EDGE ( 'NONE', *, *, #60365, .T. ) ;
#60242 = LINE ( 'NONE', #7948, #49048 ) ;
#60243 = CONICAL_SURFACE ( 'NONE', #59262, 43.08621763946400307, 1.568696531533066763 ) ;
#60244 = DIRECTION ( 'NONE',  ( 1.836766033387207149E-16, -1.000000000000000000, 0.000000000000000000 ) ) ;
#60245 = EDGE_CURVE ( 'NONE', #39259, #40034, #57793, .T. ) ;
#60246 = AXIS2_PLACEMENT_3D ( 'NONE', #55798, #18227, #50488 ) ;
#60247 = B_SPLINE_CURVE_WITH_KNOTS ( 'NONE', 3,
 ( #59554, #7864, #50771, #26983 ),
 .UNSPECIFIED., .F., .F.,
 ( 4, 4 ),
 ( 0.000000000000000000, 0.005004741218457418005 ),
 .UNSPECIFIED. ) ;
#60248 = CARTESIAN_POINT ( 'NONE',  ( 0.1101816497532063094, 21.67974746580497580, 37.27878591512682505 ) ) ;
#60249 = VERTEX_POINT ( 'NONE', #10738 ) ;
#60250 = VERTEX_POINT ( 'NONE', #697 ) ;
#60251 = CARTESIAN_POINT ( 'NONE',  ( 0.5806925824938499181, 10.33919002968644385, 45.74192291403583965 ) ) ;
#60252 = ORIENTED_EDGE ( 'NONE', *, *, #58097, .F. ) ;
#60253 = CARTESIAN_POINT ( 'NONE',  ( 0.9730545539215883499, 21.01499094264601908, -37.40983423658450846 ) ) ;
#60254 = CARTESIAN_POINT ( 'NONE',  ( 45.00000000000001421, 0.000000000000000000, 0.000000000000000000 ) ) ;
#60255 = FACE_OUTER_BOUND ( 'NONE', #30372, .T. ) ;
#60256 = CARTESIAN_POINT ( 'NONE',  ( 5.894904586330512508, -2.014437969560491037, 20.01178282233833627 ) ) ;
#60257 = CARTESIAN_POINT ( 'NONE',  ( 0.5837374860065633886, 12.22086613152827539, -46.31070423340719344 ) ) ;
#60258 = EDGE_CURVE ( 'NONE', #15021, #59128, #58007, .T. ) ;
#60259 = VERTEX_POINT ( 'NONE', #5990 ) ;
#60260 = DIRECTION ( 'NONE',  ( 0.000000000000000000, 1.000000000000000000, -1.287488025362403787E-15 ) ) ;
#60261 = CARTESIAN_POINT ( 'NONE',  ( 4.960386119450149955, 36.33710775634317258, -24.37316279386498863 ) ) ;
#60262 =( BOUNDED_SURFACE ( )  B_SPLINE_SURFACE ( 3, 1, ( 
 ( #46531, #3270 ),
 ( #13636, #45607 ),
 ( #51202, #8284 ),
 ( #22715, #40926 ) ),
 .UNSPECIFIED., .F., .F., .F. ) 
 B_SPLINE_SURFACE_WITH_KNOTS ( ( 4, 4 ),
 ( 2, 2 ),
 ( 0.000000000000000000, 1.000000000000000000 ),
 ( 0.000000000000000000, 1.000000000000000000 ),
 .UNSPECIFIED. ) 
 GEOMETRIC_REPRESENTATION_ITEM ( )  RATIONAL_B_SPLINE_SURFACE ( (
 ( 1.000000000000000000, 1.000000000000000000),
 ( 0.7223157951917476005, 0.9931996967497186413),
 ( 0.7223157951917476005, 0.9931996967497186413),
 ( 1.000000000000000000, 1.000000000000000000) ) ) 
 REPRESENTATION_ITEM ( '' )  SURFACE ( )  );
#60263 = VERTEX_POINT ( 'NONE', #25130 ) ;
#60264 = DIRECTION ( 'NONE',  ( 0.000000000000000000, 0.000000000000000000, 1.000000000000000000 ) ) ;
#60265 = FACE_OUTER_BOUND ( 'NONE', #23133, .T. ) ;
#60266 = CARTESIAN_POINT ( 'NONE',  ( 2.282803330402962239, 9.607084330193609745, 45.98043973397309259 ) ) ;
#60267 = FILL_AREA_STYLE_COLOUR ( '', #11411 ) ;
#60268 = ORIENTED_EDGE ( 'NONE', *, *, #10922, .F. ) ;
#60269 = B_SPLINE_CURVE_WITH_KNOTS ( 'NONE', 3,
 ( #45684, #59756, #17783, #8062 ),
 .UNSPECIFIED., .F., .F.,
 ( 4, 4 ),
 ( 0.000000000000000000, 0.004445488388166995118 ),
 .UNSPECIFIED. ) ;
#60270 = CARTESIAN_POINT ( 'NONE',  ( 0.5998501479064708430, 34.38546660123297727, -33.64490850298808056 ) ) ;
#60271 = CARTESIAN_POINT ( 'NONE',  ( 1.000110580585048536, 20.71550333451957826, -36.43192836468320905 ) ) ;
#60272 = CARTESIAN_POINT ( 'NONE',  ( 0.5850706913938533704, 23.79070617305381319, 41.56998471741236756 ) ) ;
#60273 = PRODUCT_DEFINITION_SHAPE ( 'NONE', 'NONE',  #2291 ) ;
#60274 = CARTESIAN_POINT ( 'NONE',  ( 0.6031356755773454870, -41.66225520948420780, 24.05374386753643989 ) ) ;
#60275 = CARTESIAN_POINT ( 'NONE',  ( 0.6021448801613057400, -42.91582863034458484, 23.86991394198654959 ) ) ;
#60276 =( BOUNDED_SURFACE ( )  B_SPLINE_SURFACE ( 3, 1, ( 
 ( #58436, #34669 ),
 ( #15562, #59064 ),
 ( #6420, #10547 ),
 ( #44098, #11475 ) ),
 .UNSPECIFIED., .F., .F., .F. ) 
 B_SPLINE_SURFACE_WITH_KNOTS ( ( 4, 4 ),
 ( 2, 2 ),
 ( 0.000000000000000000, 1.000000000000000000 ),
 ( 0.000000000000000000, 1.000000000000000000 ),
 .UNSPECIFIED. ) 
 GEOMETRIC_REPRESENTATION_ITEM ( )  RATIONAL_B_SPLINE_SURFACE ( (
 ( 1.000000000000000000, 1.000000000000000000),
 ( 0.7282232189291693025, 0.9929344683865674037),
 ( 0.7282232189291693025, 0.9929344683865674037),
 ( 1.000000000000000000, 1.000000000000000000) ) ) 
 REPRESENTATION_ITEM ( '' )  SURFACE ( )  );
#60277 = CARTESIAN_POINT ( 'NONE',  ( 0.9757402383260949108, 42.90839848328079853, 0.08489923450653533155 ) ) ;
#60278 = CARTESIAN_POINT ( 'NONE',  ( -6.057079549204054558, -18.27326637954045196, -6.076098001357041589 ) ) ;
#60279 = CARTESIAN_POINT ( 'NONE',  ( 0.6846871229502932144, 11.56285438919632469, 46.49193983736596181 ) ) ;
#60280 = FACE_OUTER_BOUND ( 'NONE', #22533, .T. ) ;
#60281 = CARTESIAN_POINT ( 'NONE',  ( 0.7056759521544949676, 11.69106431276068747, -45.42100664177186076 ) ) ;
#60282 = ORIENTED_EDGE ( 'NONE', *, *, #22373, .F. ) ;
#60283 = ADVANCED_FACE ( 'NONE', ( #1303 ), #36095, .F. ) ;
#60284 = LINE ( 'NONE', #17396, #53905 ) ;
#60285 = CARTESIAN_POINT ( 'NONE',  ( 3.660087539127302669, -16.63102164621066237, 45.06758728829461802 ) ) ;
#60286 = CARTESIAN_POINT ( 'NONE',  ( 0.7056555295713298204, -0.8411712675124666250, -47.89404551051137560 ) ) ;
#60287 = LINE ( 'NONE', #60596, #39026 ) ;
#60288 = CARTESIAN_POINT ( 'NONE',  ( 0.8554163680231738898, 28.56078411578483056, -37.22213163970264560 ) ) ;
#60289 = CARTESIAN_POINT ( 'NONE',  ( 0.9790850452238870627, -31.04767048625561898, 28.14923600455417230 ) ) ;
#60290 = EDGE_CURVE ( 'NONE', #13776, #55407, #6970, .T. ) ;
#60291 = APPLICATION_PROTOCOL_DEFINITION ( 'draft international standard', 'automotive_design', 1998, #34463 ) ;
#60292 = DIRECTION ( 'NONE',  ( -0.07500201931887529039, -0.8144017028153767157, 0.5754342391181688221 ) ) ;
#60293 = B_SPLINE_CURVE_WITH_KNOTS ( 'NONE', 3,
 ( #5223, #39712, #15276, #24354 ),
 .UNSPECIFIED., .F., .F.,
 ( 4, 4 ),
 ( 0.000000000000000000, 0.005004741218457427546 ),
 .UNSPECIFIED. ) ;
#60294 = ADVANCED_FACE ( 'NONE', ( #42570 ), #54561, .T. ) ;
#60295 = CARTESIAN_POINT ( 'NONE',  ( 4.956653778116994147, 35.79382859084161339, -32.11725092155005967 ) ) ;
#60297 = VERTEX_POINT ( 'NONE', #37888 ) ;
#60296 = CARTESIAN_POINT ( 'NONE',  ( 5.910764540655177868, -18.51025558288800354, -7.865855117234652916 ) ) ;
#60298 = ORIENTED_EDGE ( 'NONE', *, *, #53158, .T. ) ;
#60299 = DIRECTION ( 'NONE',  ( -0.1011922191286467460, 0.7235494112461693383, -0.6828150439710168884 ) ) ;
#60300 = CARTESIAN_POINT ( 'NONE',  ( 0.5830082357119548142, -8.069412620820072490, 46.19650002860918647 ) ) ;
#60301 = CARTESIAN_POINT ( 'NONE',  ( 10.00000000000000533, 8.397924308530857731E-13, -80.00000000000001421 ) ) ;
#60302 = ORIENTED_EDGE ( 'NONE', *, *, #18296, .F. ) ;
#60303 = CARTESIAN_POINT ( 'NONE',  ( 3.376099380956838925, -11.30600709870817688, 7.202956831470493704 ) ) ;
#60304 = FACE_OUTER_BOUND ( 'NONE', #8820, .T. ) ;
#60305 = CARTESIAN_POINT ( 'NONE',  ( 0.1102144999581332885, 5.753800096706042311, -42.73889315046714188 ) ) ;
#60306 = ORIENTED_EDGE ( 'NONE', *, *, #1042, .F. ) ;
#60307 = ORIENTED_EDGE ( 'NONE', *, *, #26746, .T. ) ;
#60308 = AXIS2_PLACEMENT_3D ( 'NONE', #4434, #4136, #23889 ) ;
#60309 = PRESENTATION_STYLE_ASSIGNMENT (( #60940 ) ) ;
#60310 = EDGE_CURVE ( 'NONE', #32695, #6090, #42981, .T. ) ;
#60311 = CARTESIAN_POINT ( 'NONE',  ( -6.015611763856276717, -18.20278301740933102, -4.870987357968367348 ) ) ;
#60312 = CARTESIAN_POINT ( 'NONE',  ( 0.9787284016396613495, 32.77352223152413302, -26.11957579036502608 ) ) ;
#60313 = ORIENTED_EDGE ( 'NONE', *, *, #4711, .T. ) ;
#60314 = EDGE_CURVE ( 'NONE', #22780, #27827, #17559, .T. ) ;
#60315 = CARTESIAN_POINT ( 'NONE',  ( 0.5786265663353153954, 47.58023467411538121, 5.535668456754111233 ) ) ;
#60316 = CARTESIAN_POINT ( 'NONE',  ( 0.1129192098497455998, -42.55567333040708888, -11.66046547873770756 ) ) ;
#60317 = EDGE_CURVE ( 'NONE', #11680, #40793, #54131, .T. ) ;
#60318 = CARTESIAN_POINT ( 'NONE',  ( 0.3622758884714730732, -26.89560658783362612, -33.69533458712334806 ) ) ;
#60319 = CARTESIAN_POINT ( 'NONE',  ( 0.8557997880470599172, 33.22501220301901270, 34.51495345639560952 ) ) ;
#60320 = EDGE_LOOP ( 'NONE', ( #24515, #50341, #53369, #902 ) ) ;
#60321 = CARTESIAN_POINT ( 'NONE',  ( 0.7948878604505666967, 21.93744113805909635, -43.92547465438033072 ) ) ;
#60322 = CARTESIAN_POINT ( 'NONE',  ( 50.50000000000024869, -4.999999999999982236, 6.123233995736707118E-16 ) ) ;
#60323 = EDGE_LOOP ( 'NONE', ( #34084, #48867, #22243, #8956 ) ) ;
#60324 = CARTESIAN_POINT ( 'NONE',  ( 1.227938101723748288, -26.79402671879349640, 33.52879263017854328 ) ) ;
#60325 = CARTESIAN_POINT ( 'NONE',  ( -6.078457390727109555, -17.34717774342076169, -8.358823803363440774 ) ) ;
#60326 = CARTESIAN_POINT ( 'NONE',  ( 0.3676999524040366896, 39.37931578713023839, -19.88014264185028068 ) ) ;
#60327 = SURFACE_STYLE_USAGE ( .BOTH. , #45051 ) ;
#60328 = ADVANCED_FACE ( 'NONE', ( #46650 ), #8562, .T. ) ;
#60329 = CIRCLE ( 'NONE', #28338, 42.08604991992415023 ) ;
#60330 = VERTEX_POINT ( 'NONE', #22827 ) ;
#60331 = EDGE_LOOP ( 'NONE', ( #33857, #16082, #44751, #44273 ) ) ;
#60332 = CARTESIAN_POINT ( 'NONE',  ( 0.6845945791218023269, 36.27071225238075414, -29.74629310382962188 ) ) ;
#60333 = CARTESIAN_POINT ( 'NONE',  ( 0.5827357941260191687, 41.65958460246774564, 23.63272379758808484 ) ) ;
#60334 = ORIENTED_EDGE ( 'NONE', *, *, #29222, .T. ) ;
#60335 = CARTESIAN_POINT ( 'NONE',  ( 0.6845945791218034371, -18.95641467630732535, -42.90758514917641264 ) ) ;
#60336 = ORIENTED_EDGE ( 'NONE', *, *, #10998, .F. ) ;
#60337 = DIRECTION ( 'NONE',  ( -1.000000000000000000, -0.000000000000000000, -0.000000000000000000 ) ) ;
#60338 = ORIENTED_EDGE ( 'NONE', *, *, #47231, .F. ) ;
#60339 = CARTESIAN_POINT ( 'NONE',  ( 4.960386119450146403, -21.43901005587111541, -38.14191018416091339 ) ) ;
#60340 = CARTESIAN_POINT ( 'NONE',  ( -6.016104459813374383, 7.215917642689303690, -17.40682403289241265 ) ) ;
#60341 = CARTESIAN_POINT ( 'NONE',  ( 0.1081432562775997697, -26.58728936586542346, 33.95357233988183054 ) ) ;
#60342 = ORIENTED_EDGE ( 'NONE', *, *, #29200, .F. ) ;
#60343 = CARTESIAN_POINT ( 'NONE',  ( 5.959828726073459926, -14.51699876360210162, 14.51059719297091455 ) ) ;
#60344 = CARTESIAN_POINT ( 'NONE',  ( 4.967162193818129623, -43.02067033766018511, 2.375726030842427061 ) ) ;
#60345 = ORIENTED_EDGE ( 'NONE', *, *, #9911, .T. ) ;
#60346 = AXIS2_PLACEMENT_3D ( 'NONE', #54055, #20567, #57833 ) ;
#60347 = ORIENTED_EDGE ( 'NONE', *, *, #9987, .T. ) ;
#60348 = CARTESIAN_POINT ( 'NONE',  ( 2.500000000000000000, 0.000000000000000000, 0.000000000000000000 ) ) ;
#60349 = CARTESIAN_POINT ( 'NONE',  ( 4.958415959904823644, 24.01335991617007792, -38.55596580762981773 ) ) ;
#60350 = CARTESIAN_POINT ( 'NONE',  ( 0.6028777368367060907, 32.95046403715527106, 36.41162931052673457 ) ) ;
#60351 = CARTESIAN_POINT ( 'NONE',  ( 0.1103878639767399417, 26.21398130517517444, -34.24245495762994551 ) ) ;
#60352 = CARTESIAN_POINT ( 'NONE',  ( 0.8751705887134553219, -0.8911681664085087107, -48.08707113907594533 ) ) ;
#60353 = EDGE_LOOP ( 'NONE', ( #20367, #20074, #33276, #30799 ) ) ;
#60354 = CARTESIAN_POINT ( 'NONE',  ( 5.895596859100789899, -11.92767122914683675, -16.19440774656085935 ) ) ;
#60355 = CARTESIAN_POINT ( 'NONE',  ( -6.001507490154111224, 18.68469198366100059, -2.444174634177952665 ) ) ;
#60356 = ORIENTED_EDGE ( 'NONE', *, *, #42592, .F. ) ;
#60357 = EDGE_CURVE ( 'NONE', #37103, #39646, #28751, .T. ) ;
#60358 = CARTESIAN_POINT ( 'NONE',  ( 0.9752570700956799676, -30.50353876750651949, 30.17732761204926817 ) ) ;
#60359 = CARTESIAN_POINT ( 'NONE',  ( 0.9780106845699489959, -27.29611424684454235, 31.80021058858961069 ) ) ;
#60360 = CARTESIAN_POINT ( 'NONE',  ( 0.9762797500689124330, -17.18051571332144434, 38.22505284509125545 ) ) ;
#60361 = CARTESIAN_POINT ( 'NONE',  ( 0.3622758884714730732, -0.8252992914325094631, -43.10531414739105571 ) ) ;
#60362 = CARTESIAN_POINT ( 'NONE',  ( 5.981074661064941900, -12.50143471347293556, 16.27808421740004619 ) ) ;
#60363 = CARTESIAN_POINT ( 'NONE',  ( -6.063463321072278589, 9.995861580988218975, -16.45913739335064463 ) ) ;
#60364 = LINE ( 'NONE', #50976, #59592 ) ;
#60365 = EDGE_CURVE ( 'NONE', #23595, #1395, #51941, .T. ) ;
#60366 = CARTESIAN_POINT ( 'NONE',  ( 3.376099380956842921, -2.682194557846140359, -13.13446671874909377 ) ) ;
#60367 = DIRECTION ( 'NONE',  ( -1.000000000000000000, -0.000000000000000000, -0.000000000000000000 ) ) ;
#60368 = EDGE_CURVE ( 'NONE', #58292, #48331, #36995, .T. ) ;
#60369 = CARTESIAN_POINT ( 'NONE',  ( 0.8744876279028263033, -35.88078294188978390, 33.50999053799454686 ) ) ;
#60370 = CARTESIAN_POINT ( 'NONE',  ( 3.240649175237395596, 43.74621574345733421, 4.640422989829291467 ) ) ;
#60371 = CARTESIAN_POINT ( 'NONE',  ( 0.5988103564986357874, -46.62176022926377783, -11.86435738293427100 ) ) ;
#60372 = CARTESIAN_POINT ( 'NONE',  ( 0.6024113833632039894, -1.356364261510525138, -49.08871708540531387 ) ) ;
#60373 = CARTESIAN_POINT ( 'NONE',  ( 0.5848930533535030563, 40.25661832390738937, 24.05572205340763148 ) ) ;
#60374 = VECTOR ( 'NONE', #6573, 1000.000000000000114 ) ;
#60375 = LINE ( 'NONE', #12499, #8450 ) ;
#60376 = CARTESIAN_POINT ( 'NONE',  ( 0.2224561200757580182, 26.84793396060980797, -33.74134531362606282 ) ) ;
#60377 =( REPRESENTATION_RELATIONSHIP ('NONE','NONE', #44881, #53251 ) REPRESENTATION_RELATIONSHIP_WITH_TRANSFORMATION ( #25479 )SHAPE_REPRESENTATION_RELATIONSHIP( ) );
#60378 = EDGE_CURVE ( 'NONE', #11845, #22472, #19782, .T. ) ;
#60379 =( BOUNDED_SURFACE ( )  B_SPLINE_SURFACE ( 3, 1, ( 
 ( #4581, #14034 ),
 ( #14646, #29038 ),
 ( #33135, #48150 ),
 ( #5203, #41926 ) ),
 .UNSPECIFIED., .F., .F., .F. ) 
 B_SPLINE_SURFACE_WITH_KNOTS ( ( 4, 4 ),
 ( 2, 2 ),
 ( 0.000000000000000000, 1.000000000000000000 ),
 ( 0.000000000000000000, 1.000000000000000000 ),
 .UNSPECIFIED. ) 
 GEOMETRIC_REPRESENTATION_ITEM ( )  RATIONAL_B_SPLINE_SURFACE ( (
 ( 1.000000000000000000, 1.000000000000000000),
 ( 0.9953040768229005630, 0.8617119497784937465),
 ( 0.9953040768229005630, 0.8617119497784937465),
 ( 1.000000000000000000, 1.000000000000000000) ) ) 
 REPRESENTATION_ITEM ( '' )  SURFACE ( )  );
#60380 = ORIENTED_EDGE ( 'NONE', *, *, #35711, .F. ) ;
#60381 = CARTESIAN_POINT ( 'NONE',  ( 0.9722240750034563117, 37.44729079646494796, 20.94823713380351293 ) ) ;
#60382 = EDGE_CURVE ( 'NONE', #45184, #1908, #34614, .T. ) ;
#60383 = CARTESIAN_POINT ( 'NONE',  ( 5.880360259849739535, -47.05949693022701297, -9.312491912827962182 ) ) ;
#60384 = CYLINDRICAL_SURFACE ( 'NONE', #58547, 72.00000000000002842 ) ;
#60385 = ORIENTED_EDGE ( 'NONE', *, *, #47192, .F. ) ;
#60386 = CARTESIAN_POINT ( 'NONE',  ( 4.549368137175248350, 0.000000000000000000, 0.000000000000000000 ) ) ;
#60387 = AXIS2_PLACEMENT_3D ( 'NONE', #22372, #27072, #9197 ) ;
#60388 = CARTESIAN_POINT ( 'NONE',  ( 0.8557997880470599172, -41.93815086860273311, 23.15977007032308421 ) ) ;
#60389 = ORIENTED_EDGE ( 'NONE', *, *, #24991, .T. ) ;
#60390 = FACE_OUTER_BOUND ( 'NONE', #13262, .T. ) ;
#60391 = ORIENTED_EDGE ( 'NONE', *, *, #46563, .F. ) ;
#60392 = DIRECTION ( 'NONE',  ( -3.273063162220391312E-16, 1.000000000000000000, 1.047380211910525220E-14 ) ) ;
#60393 = CARTESIAN_POINT ( 'NONE',  ( 3.660087539127331535, -45.06758728829456828, -16.63102164621081158 ) ) ;
#60394 = ORIENTED_EDGE ( 'NONE', *, *, #34044, .T. ) ;
#60395 = CARTESIAN_POINT ( 'NONE',  ( 0.6041374136657475802, 18.24862627831472750, 44.51224464245006374 ) ) ;
#60396 = CARTESIAN_POINT ( 'NONE',  ( 0.1102144999581333162, 26.15241010112978515, 34.28951223307537788 ) ) ;
#60397 = VERTEX_POINT ( 'NONE', #28441 ) ;
#60398 = CARTESIAN_POINT ( 'NONE',  ( 5.917102823773431552, -18.51940219202224114, -7.843561722958756199 ) ) ;
#60399 = DIRECTION ( 'NONE',  ( -0.07439287786467649322, -0.3693942911085712488, 0.9262902123089757911 ) ) ;
#60400 = ADVANCED_FACE ( 'NONE', ( #10584 ), #51604, .F. ) ;
#60401 = B_SPLINE_CURVE_WITH_KNOTS ( 'NONE', 3,
 ( #34349, #24945, #53423, #44083, #1111, #20253 ),
 .UNSPECIFIED., .F., .F.,
 ( 4, 2, 4 ),
 ( 8.492412771929966223E-17, 0.0002293366620881452558, 0.0004586733241762056185 ),
 .UNSPECIFIED. ) ;
#60402 = ORIENTED_EDGE ( 'NONE', *, *, #41326, .T. ) ;
#60403 = CARTESIAN_POINT ( 'NONE',  ( 7.000000000000016875, -58.44237546506768410, -54.69470952477996661 ) ) ;
#60404 = ORIENTED_EDGE ( 'NONE', *, *, #23986, .T. ) ;
#60405 = CARTESIAN_POINT ( 'NONE',  ( 0.1158403557922069033, -1.452093878213947642, 44.10024637745998888 ) ) ;
#60406 = ADVANCED_FACE ( 'NONE', ( #5845 ), #18889, .F. ) ;
#60407 = ORIENTED_EDGE ( 'NONE', *, *, #18507, .T. ) ;
#60408 = ORIENTED_EDGE ( 'NONE', *, *, #8085, .T. ) ;
#60409 = CARTESIAN_POINT ( 'NONE',  ( 5.917102823773431552, -15.77849770028341680, -12.47111576298980928 ) ) ;
#60411 = CARTESIAN_POINT ( 'NONE',  ( 0.9762797500689124330, -7.469026406146330288, 41.23758515880862774 ) ) ;
#60410 = B_SPLINE_CURVE_WITH_KNOTS ( 'NONE', 3,
 ( #7278, #36145, #50521, #37071, #27337, #42087 ),
 .UNSPECIFIED., .F., .F.,
 ( 4, 2, 4 ),
 ( 1.951563910473907981E-18, 0.0002447193893791697081, 0.0004894387787583374646 ),
 .UNSPECIFIED. ) ;
#60412 = CARTESIAN_POINT ( 'NONE',  ( 0.6028777368367060907, -25.38243257499183869, -42.03893369112811484 ) ) ;
#60413 = CARTESIAN_POINT ( 'NONE',  ( 5.901463166500145796, 19.00451910135526390, -6.583777340316079751 ) ) ;
#60414 = CARTESIAN_POINT ( 'NONE',  ( -6.016761891674564211, -16.32039929810250456, -9.418621820384668553 ) ) ;
#60415 = ORIENTED_EDGE ( 'NONE', *, *, #23663, .F. ) ;
#60416 = CARTESIAN_POINT ( 'NONE',  ( 0.9268187852002115479, 5.219396237290944818, 43.77798802853757820 ) ) ;
#60417 = CARTESIAN_POINT ( 'NONE',  ( 5.896782393890504181, 17.94821721415859628, 9.076760749925794514 ) ) ;
#60418 = CARTESIAN_POINT ( 'NONE',  ( 3.894904216938897878, 0.8163068198993449487, 43.94835577870902910 ) ) ;
#60419 = VERTEX_POINT ( 'NONE', #34706 ) ;
#60420 = VECTOR ( 'NONE', #51830, 1000.000000000000000 ) ;
#60421 = ORIENTED_EDGE ( 'NONE', *, *, #51608, .F. ) ;
#60422 = CARTESIAN_POINT ( 'NONE',  ( 0.9730545539215883499, 42.47233286818616449, 6.101350888304794218 ) ) ;
#60423 = CARTESIAN_POINT ( 'NONE',  ( 3.240649175237397372, 32.28332734583069907, 29.88397050058092219 ) ) ;
#60424 = CARTESIAN_POINT ( 'NONE',  ( 0.5817216825391126056, -44.14976101355541260, 15.81244935654816786 ) ) ;
#60425 = ORIENTED_EDGE ( 'NONE', *, *, #21775, .F. ) ;
#60426 = CARTESIAN_POINT ( 'NONE',  ( 0.8557997880470690211, 43.90420959842208504, -19.17299735371961944 ) ) ;
#60427 = CARTESIAN_POINT ( 'NONE',  ( 4.975610109902397937, -33.30777373088901072, 35.81957029655259817 ) ) ;
#60428 = ORIENTED_EDGE ( 'NONE', *, *, #46996, .F. ) ;
#60429 = CARTESIAN_POINT ( 'NONE',  ( 0.5839879882012686263, 47.48621496524031471, 6.251648354650349404 ) ) ;
#60430 = ORIENTED_EDGE ( 'NONE', *, *, #61384, .T. ) ;
#60431 = EDGE_CURVE ( 'NONE', #26687, #40968, #24639, .T. ) ;
#60432 = CARTESIAN_POINT ( 'NONE',  ( 0.8760168074887090262, 29.98565522133295502, 37.61398439004543803 ) ) ;
#60433 = CARTESIAN_POINT ( 'NONE',  ( 0.3676999524040323597, -41.19158123804999860, 15.78620342045440239 ) ) ;
#60434 = CARTESIAN_POINT ( 'NONE',  ( 0.9780303403264770656, 9.399973085119292193, -40.84091232323437737 ) ) ;
#60435 = CARTESIAN_POINT ( 'NONE',  ( 2.706805983486679779, -43.40490398453981413, 7.265701852721114129 ) ) ;
#60436 = EDGE_CURVE ( 'NONE', #29055, #35054, #16782, .T. ) ;
#60437 = SURFACE_SIDE_STYLE ('',( #46687 ) ) ;
#60438 =( NAMED_UNIT ( * ) SI_UNIT ( $, .STERADIAN. ) SOLID_ANGLE_UNIT ( ) );
#60439 = ORIENTED_EDGE ( 'NONE', *, *, #59993, .T. ) ;
#60440 = DIRECTION ( 'NONE',  ( -1.000000000000000000, -0.000000000000000000, -0.000000000000000000 ) ) ;
#60441 = DIRECTION ( 'NONE',  ( 0.000000000000000000, 0.000000000000000000, 1.000000000000000000 ) ) ;
#60442 = EDGE_CURVE ( 'NONE', #36056, #2992, #33988, .T. ) ;
#60443 = CARTESIAN_POINT ( 'NONE',  ( -5.331200000000000827, 0.000000000000000000, 0.000000000000000000 ) ) ;
#60444 = ADVANCED_FACE ( 'NONE', ( #42888 ), #48872, .F. ) ;
#60445 = CARTESIAN_POINT ( 'NONE',  ( 0.1104177457020373426, -16.50753524010271889, -39.83992599038879945 ) ) ;
#60446 = EDGE_CURVE ( 'NONE', #37050, #38361, #34100, .T. ) ;
#60447 = CARTESIAN_POINT ( 'NONE',  ( 0.9736507210033059634, 37.38294557109065863, -21.06291100879400702 ) ) ;
#60448 = CARTESIAN_POINT ( 'NONE',  ( 0.5848930533535030563, -45.99261677209132415, 9.162547944927917243 ) ) ;
#60449 = CARTESIAN_POINT ( 'NONE',  ( 0.5806925824938499181, -38.35106547415185929, -26.98922265166007861 ) ) ;
#60450 = CARTESIAN_POINT ( 'NONE',  ( 4.960156602257180580, -34.56254177294248109, -30.99165383632803028 ) ) ;
#60451 = LINE ( 'NONE', #22883, #23666 ) ;
#60452 =( BOUNDED_SURFACE ( )  B_SPLINE_SURFACE ( 3, 1, ( 
 ( #52282, #47294 ),
 ( #51981, #42610 ),
 ( #4343, #61671 ),
 ( #37927, #56984 ) ),
 .UNSPECIFIED., .F., .F., .F. ) 
 B_SPLINE_SURFACE_WITH_KNOTS ( ( 4, 4 ),
 ( 2, 2 ),
 ( 0.000000000000000000, 1.000000000000000000 ),
 ( 0.000000000000000000, 1.000000000000000000 ),
 .UNSPECIFIED. ) 
 GEOMETRIC_REPRESENTATION_ITEM ( )  RATIONAL_B_SPLINE_SURFACE ( (
 ( 1.000000000000000000, 1.000000000000000000),
 ( 0.7269869731126817891, 0.9931720237060910339),
 ( 0.7269869731126817891, 0.9931720237060910339),
 ( 1.000000000000000000, 1.000000000000000000) ) ) 
 REPRESENTATION_ITEM ( '' )  SURFACE ( )  );
#60453 = VECTOR ( 'NONE', #21264, 1000.000000000000227 ) ;
#60454 = EDGE_CURVE ( 'NONE', #22251, #25443, #37669, .T. ) ;
#60455 = CARTESIAN_POINT ( 'NONE',  ( 0.8753041380234465318, 10.05717963662801573, 48.06237057854693973 ) ) ;
#60456 = CARTESIAN_POINT ( 'NONE',  ( 3.238018933889920792, 12.22151767825371493, -5.481058110236103786 ) ) ;
#60457 = VERTEX_POINT ( 'NONE', #40347 ) ;
#60458 = CARTESIAN_POINT ( 'NONE',  ( 0.8744876279028306332, 46.30617036199629410, -16.31222353896820110 ) ) ;
#60459 = CARTESIAN_POINT ( 'NONE',  ( 0.5807400328401637335, 44.04145271122591510, -18.83234461715135311 ) ) ;
#60460 = DIRECTION ( 'NONE',  ( -0.000000000000000000, -0.000000000000000000, -1.000000000000000000 ) ) ;
#60461 = CARTESIAN_POINT ( 'NONE',  ( 0.2940133293163018635, -18.59037414415147182, 40.00798093828915825 ) ) ;
#60462 = ORIENTED_EDGE ( 'NONE', *, *, #46410, .F. ) ;
#60463 = CYLINDRICAL_SURFACE ( 'NONE', #61299, 72.00000000000002842 ) ;
#60464 = CARTESIAN_POINT ( 'NONE',  ( 0.6021447746440204973, 44.13029411860373585, -21.54201197878266427 ) ) ;
#60465 = B_SPLINE_CURVE_WITH_KNOTS ( 'NONE', 3,
 ( #20338, #53514, #33830, #10629, #10317, #29411 ),
 .UNSPECIFIED., .F., .F.,
 ( 4, 2, 4 ),
 ( 7.023086426956682172E-18, 0.0002445244328975388660, 0.0004890488657950706848 ),
 .UNSPECIFIED. ) ;
#60466 = B_SPLINE_CURVE_WITH_KNOTS ( 'NONE', 3,
 ( #43623, #9767, #57057, #19191 ),
 .UNSPECIFIED., .F., .F.,
 ( 4, 4 ),
 ( 2.380737581618758185E-07, 0.002336974151641576809 ),
 .UNSPECIFIED. ) ;
#60467 = VERTEX_POINT ( 'NONE', #59408 ) ;
#60468 = CARTESIAN_POINT ( 'NONE',  ( 0.7762777257811930287, -33.23866587527452054, -34.49689427664301888 ) ) ;
#60469 = CARTESIAN_POINT ( 'NONE',  ( -6.016104459813374383, -13.32039631884674868, -13.32794178585011480 ) ) ;
#60470 = CIRCLE ( 'NONE', #50470, 9.500000000000000000 ) ;
#60471 = CARTESIAN_POINT ( 'NONE',  ( 0.7242486021783847150, 36.85241720405513632, 32.44858715864577903 ) ) ;
#60472 = VERTEX_POINT ( 'NONE', #59099 ) ;
#60473 = CARTESIAN_POINT ( 'NONE',  ( 5.896278296736517710, -2.007758883826791241, 20.01239325714938744 ) ) ;
#60474 = AXIS2_PLACEMENT_3D ( 'NONE', #20495, #34294, #48999 ) ;
#60475 = ORIENTED_EDGE ( 'NONE', *, *, #6403, .T. ) ;
#60476 = ORIENTED_EDGE ( 'NONE', *, *, #22218, .T. ) ;
#60477 = CARTESIAN_POINT ( 'NONE',  ( 0.1147471544378676211, 44.05242651652063302, 2.517122658869559881 ) ) ;
#60478 = ORIENTED_EDGE ( 'NONE', *, *, #43963, .T. ) ;
#60479 = CARTESIAN_POINT ( 'NONE',  ( 0.5786265663353196143, 5.535668456753938038, 47.58023467411540963 ) ) ;
#60480 = CIRCLE ( 'NONE', #4435, 5.000000000000000888 ) ;
#60481 = ORIENTED_EDGE ( 'NONE', *, *, #21779, .T. ) ;
#60482 = CARTESIAN_POINT ( 'NONE',  ( 5.910764540655177868, -7.214026563325304231, -18.77389302230093904 ) ) ;
#60483 = ADVANCED_FACE ( 'NONE', ( #26209 ), #61656, .F. ) ;
#60484 = CARTESIAN_POINT ( 'NONE',  ( 0.9756354156337433414, 16.29989858042629791, 39.69194847698937423 ) ) ;
#60485 = ORIENTED_EDGE ( 'NONE', *, *, #14451, .F. ) ;
#60486 = CARTESIAN_POINT ( 'NONE',  ( 0.1156867017252034419, 15.12161881791919882, 41.45213446374913246 ) ) ;
#60487 = CARTESIAN_POINT ( 'NONE',  ( 0.8554163680231738898, -46.74230100997658610, -4.045092014350424314 ) ) ;
#60488 = CARTESIAN_POINT ( 'NONE',  ( 0.5998501479064699549, 46.33007877220738635, -12.95623334615453892 ) ) ;
#60489 = DIRECTION ( 'NONE',  ( 0.000000000000000000, 0.000000000000000000, 1.000000000000000000 ) ) ;
#60490 = ORIENTED_EDGE ( 'NONE', *, *, #29681, .F. ) ;
#60491 = CARTESIAN_POINT ( 'NONE',  ( 0.5839879882012700696, 44.25011577017269815, 18.32896541547087566 ) ) ;
#60492 = ORIENTED_EDGE ( 'NONE', *, *, #844, .T. ) ;
#60493 = CARTESIAN_POINT ( 'NONE',  ( 0.8751705887134423323, -0.8911681664091769539, 48.08707113907594533 ) ) ;
#60494 = ORIENTED_EDGE ( 'NONE', *, *, #38994, .F. ) ;
#60495 = CARTESIAN_POINT ( 'NONE',  ( 0.1155031312995260795, -12.71598718139274098, 42.25216328822068590 ) ) ;
#60496 = CARTESIAN_POINT ( 'NONE',  ( 0.1310142868023668195, -41.81449350725036851, 10.54463319394661447 ) ) ;
#60497 = ORIENTED_EDGE ( 'NONE', *, *, #7861, .T. ) ;
#60498 = DIRECTION ( 'NONE',  ( -1.000000000000000000, -3.135800716341489291E-16, 1.298891185607901956E-16 ) ) ;
#60499 = CARTESIAN_POINT ( 'NONE',  ( -6.057079549204054558, 7.802675369763813151, -17.60538236374943111 ) ) ;
#60500 = CARTESIAN_POINT ( 'NONE',  ( 0.6029443199889047422, 28.09518699877417092, 40.27652057164711152 ) ) ;
#60501 = CARTESIAN_POINT ( 'NONE',  ( 4.975610109902397937, -4.123593823332411645, 48.73854102369035957 ) ) ;
#60502 = ORIENTED_EDGE ( 'NONE', *, *, #38134, .T. ) ;
#60503 = B_SPLINE_CURVE_WITH_KNOTS ( 'NONE', 3,
 ( #36583, #51810, #31560, #11864, #40682, #40075, #32729, #60350, #26862, #55042, #35978, #21241, #8909, #7108, #50351, #55347 ),
 .UNSPECIFIED., .F., .F.,
 ( 4, 3, 3, 3, 3, 4 ),
 ( 1.962735358247463844E-17, 0.0002612764279487754396, 0.0003919131003184795703, 0.0005225497727000676411, 0.0007837925190632380901, 0.001045051706266724757 ),
 .UNSPECIFIED. ) ;
#60504 = ORIENTED_EDGE ( 'NONE', *, *, #41048, .F. ) ;
#60505 = CARTESIAN_POINT ( 'NONE',  ( 4.956445790443996025, 13.43466403631381567, 45.13366650706556982 ) ) ;
#60506 = CARTESIAN_POINT ( 'NONE',  ( 5.960721111146673579, 18.96557324978287085, -7.848955554238317589 ) ) ;
#60507 = CARTESIAN_POINT ( 'NONE',  ( 1.827326673878743035, 12.32830836993820967, -41.24690799101795591 ) ) ;
#60508 = B_SPLINE_CURVE_WITH_KNOTS ( 'NONE', 3,
 ( #8406, #47882, #56328, #37890 ),
 .UNSPECIFIED., .F., .F.,
 ( 4, 4 ),
 ( 0.000000000000000000, 0.004444103432399268763 ),
 .UNSPECIFIED. ) ;
#60509 = EDGE_CURVE ( 'NONE', #51483, #14125, #36203, .T. ) ;
#60510 = CARTESIAN_POINT ( 'NONE',  ( 0.6028618097248862329, 6.106174977919045510, -47.71844004092982772 ) ) ;
#60511 = EDGE_CURVE ( 'NONE', #52112, #18772, #20656, .T. ) ;
#60512 = CARTESIAN_POINT ( 'NONE',  ( 0.5835871038041838821, 4.829953511217432549, -46.64660761492717000 ) ) ;
#60513 = VECTOR ( 'NONE', #56729, 1000.000000000000000 ) ;
#60514 = DIRECTION ( 'NONE',  ( 1.000000000000000000, 0.000000000000000000, 0.000000000000000000 ) ) ;
#60515 = EDGE_CURVE ( 'NONE', #13905, #51708, #27974, .T. ) ;
#60516 = CARTESIAN_POINT ( 'NONE',  ( -6.078457390727109555, -19.21674198601421324, -1.229365072086556987 ) ) ;
#60517 = EDGE_CURVE ( 'NONE', #57645, #25309, #39095, .T. ) ;
#60518 = AXIS2_PLACEMENT_3D ( 'NONE', #31294, #20666, #55085 ) ;
#60519 = ADVANCED_FACE ( 'NONE', ( #60034 ), #38845, .F. ) ;
#60520 = CARTESIAN_POINT ( 'NONE',  ( 4.335381028904216727, -36.63547605605806012, -32.52074325427298618 ) ) ;
#60521 = DIRECTION ( 'NONE',  ( 0.09835009131224552170, 0.1222230102475009711, -0.9876177374393962927 ) ) ;
#60522 = CIRCLE ( 'NONE', #3507, 42.92674063221959813 ) ;
#60523 = CARTESIAN_POINT ( 'NONE',  ( 0.1103744047535531458, -21.59576373962443085, 37.32746539760782412 ) ) ;
#60524 = CARTESIAN_POINT ( 'NONE',  ( 2.526464513654347321, 27.11556434133549232, 33.34586834545783773 ) ) ;
#60525 = DIRECTION ( 'NONE',  ( -1.000000000000000000, -0.000000000000000000, -0.000000000000000000 ) ) ;
#60526 = CARTESIAN_POINT ( 'NONE',  ( 3.783278058412226752, 9.462251542474405142, -41.98530666033905590 ) ) ;
#60527 = CARTESIAN_POINT ( 'NONE',  ( 5.960221823109900008, 10.26751639438368180, -17.77295928189545648 ) ) ;
#60528 = B_SPLINE_CURVE_WITH_KNOTS ( 'NONE', 3,
 ( #976, #20408, #30099, #6261 ),
 .UNSPECIFIED., .F., .F.,
 ( 4, 4 ),
 ( 0.000000000000000000, 0.004442905043737217438 ),
 .UNSPECIFIED. ) ;
#60530 =( BOUNDED_SURFACE ( )  B_SPLINE_SURFACE ( 3, 1, ( 
 ( #47877, #29366 ),
 ( #10581, #29068 ),
 ( #29672, #43498 ),
 ( #57229, #48787 ) ),
 .UNSPECIFIED., .F., .F., .F. ) 
 B_SPLINE_SURFACE_WITH_KNOTS ( ( 4, 4 ),
 ( 2, 2 ),
 ( 0.000000000000000000, 1.000000000000000000 ),
 ( 0.000000000000000000, 1.000000000000000000 ),
 .UNSPECIFIED. ) 
 GEOMETRIC_REPRESENTATION_ITEM ( )  RATIONAL_B_SPLINE_SURFACE ( (
 ( 1.000000000000000000, 1.000000000000000000),
 ( 0.7211978278499970862, 0.9934217856018976445),
 ( 0.7211978278499970862, 0.9934217856018976445),
 ( 1.000000000000000000, 1.000000000000000000) ) ) 
 REPRESENTATION_ITEM ( '' )  SURFACE ( )  );
#60529 = CARTESIAN_POINT ( 'NONE',  ( 0.6029442701453592290, 17.04172866834603184, 46.05566967434899794 ) ) ;
#60531 = FACE_OUTER_BOUND ( 'NONE', #58750, .T. ) ;
#60533 = ORIENTED_EDGE ( 'NONE', *, *, #47864, .F. ) ;
#60532 = CARTESIAN_POINT ( 'NONE',  ( 0.9730545539215892381, 39.83279466599039154, 15.95224156741843835 ) ) ;
#60534 = ORIENTED_EDGE ( 'NONE', *, *, #4992, .T. ) ;
#60535 = EDGE_CURVE ( 'NONE', #35558, #9042, #13650, .T. ) ;
#60536 = CARTESIAN_POINT ( 'NONE',  ( -6.078075953587585900, 13.83625866741016353, -13.39227838478774935 ) ) ;
#60537 = CARTESIAN_POINT ( 'NONE',  ( 0.2224561200757594337, 31.02237548791951838, -29.94832483818005642 ) ) ;
#60538 = CARTESIAN_POINT ( 'NONE',  ( 0.5980894510889448457, -47.60453381548688156, -6.974827154143931729 ) ) ;
#60539 = EDGE_LOOP ( 'NONE', ( #4834, #37124, #36357, #16680, #19911, #24225 ) ) ;
#60540 = EDGE_CURVE ( 'NONE', #42210, #55527, #20425, .T. ) ;
#60541 = ORIENTED_EDGE ( 'NONE', *, *, #28623, .T. ) ;
#60542 = LINE ( 'NONE', #30493, #36345 ) ;
#60543 = CARTESIAN_POINT ( 'NONE',  ( -6.077587904424778920, 15.42837212129410673, 11.52221137980054699 ) ) ;
#60544 = ORIENTED_EDGE ( 'NONE', *, *, #25249, .F. ) ;
#60545 = VERTEX_POINT ( 'NONE', #44735 ) ;
#60546 = CARTESIAN_POINT ( 'NONE',  ( 4.694002226626920127, -26.36364849202824701, -37.19197238161631702 ) ) ;
#60547 =( BOUNDED_SURFACE ( )  B_SPLINE_SURFACE ( 3, 1, ( 
 ( #60207, #17319 ),
 ( #31724, #7908 ),
 ( #27023, #51116 ),
 ( #22631, #27634 ) ),
 .UNSPECIFIED., .F., .F., .F. ) 
 B_SPLINE_SURFACE_WITH_KNOTS ( ( 4, 4 ),
 ( 2, 2 ),
 ( 0.000000000000000000, 1.000000000000000000 ),
 ( 0.000000000000000000, 1.000000000000000000 ),
 .UNSPECIFIED. ) 
 GEOMETRIC_REPRESENTATION_ITEM ( )  RATIONAL_B_SPLINE_SURFACE ( (
 ( 1.000000000000000000, 1.000000000000000000),
 ( 0.9953485035131437453, 0.8621029689291515030),
 ( 0.9953485035131437453, 0.8621029689291515030),
 ( 1.000000000000000000, 1.000000000000000000) ) ) 
 REPRESENTATION_ITEM ( '' )  SURFACE ( )  );
#60548 = CARTESIAN_POINT ( 'NONE',  ( 0.5998501479064699549, 46.60114184914301205, 11.94461217097485672 ) ) ;
#60549 = CARTESIAN_POINT ( 'NONE',  ( 0.9756008150404614776, -41.40938772927938061, 11.24277293639973507 ) ) ;
#60550 =( BOUNDED_SURFACE ( )  B_SPLINE_SURFACE ( 3, 1, ( 
 ( #24550, #28938 ),
 ( #38671, #4795 ),
 ( #14552, #57726 ),
 ( #19249, #10144 ) ),
 .UNSPECIFIED., .F., .F., .F. ) 
 B_SPLINE_SURFACE_WITH_KNOTS ( ( 4, 4 ),
 ( 2, 2 ),
 ( 0.000000000000000000, 1.000000000000000000 ),
 ( 0.000000000000000000, 1.000000000000000000 ),
 .UNSPECIFIED. ) 
 GEOMETRIC_REPRESENTATION_ITEM ( )  RATIONAL_B_SPLINE_SURFACE ( (
 ( 1.000000000000000000, 1.000000000000000000),
 ( 0.9952954269826590483, 0.8620686068821307169),
 ( 0.9952954269826590483, 0.8620686068821307169),
 ( 1.000000000000000000, 1.000000000000000000) ) ) 
 REPRESENTATION_ITEM ( '' )  SURFACE ( )  );
#60551 = ORIENTED_EDGE ( 'NONE', *, *, #21638, .F. ) ;
#60552 = CARTESIAN_POINT ( 'NONE',  ( 4.956653778116966613, 0.000000000000000000, 0.000000000000000000 ) ) ;
#60553 = B_SPLINE_CURVE_WITH_KNOTS ( 'NONE', 3,
 ( #50964, #41594, #50350, #26861 ),
 .UNSPECIFIED., .F., .F.,
 ( 4, 4 ),
 ( 1.398578778534940505E-17, 0.005004948556313816577 ),
 .UNSPECIFIED. ) ;
#60554 = CARTESIAN_POINT ( 'NONE',  ( 3.678834586032787346, -48.77537454663707450, 4.424387806648834243 ) ) ;
#60555 = ADVANCED_FACE ( 'NONE', ( #6769 ), #47665, .T. ) ;
#60556 = CARTESIAN_POINT ( 'NONE',  ( 0.1097557419366048670, 21.75515245866073144, 37.23482781437652989 ) ) ;
#60557 = VERTEX_POINT ( 'NONE', #50937 ) ;
#60558 = EDGE_LOOP ( 'NONE', ( #60031, #6684, #37590, #5266 ) ) ;
#60559 = DIRECTION ( 'NONE',  ( -1.000000000000000000, -1.836909530733573776E-16, 1.925929944387235853E-32 ) ) ;
#60560 = VECTOR ( 'NONE', #375, 1000.000000000000114 ) ;
#60561 = ORIENTED_EDGE ( 'NONE', *, *, #23551, .F. ) ;
#60562 = CARTESIAN_POINT ( 'NONE',  ( -6.016761891674564211, 4.873659902332621918, -18.20201388312090529 ) ) ;
#60563 = CARTESIAN_POINT ( 'NONE',  ( 1.231276596079887264, -0.5545928549379750550, 41.91621640586514985 ) ) ;
#60564 = CARTESIAN_POINT ( 'NONE',  ( 4.975801465491695552, 31.15993731089124097, -36.39623109580435312 ) ) ;
#60565 = CARTESIAN_POINT ( 'NONE',  ( 0.5835871038041862136, -38.74013687519667570, 26.42794444886935779 ) ) ;
#60566 = CARTESIAN_POINT ( 'NONE',  ( 1.296416391601052487, -43.83799569129288898, -4.531832724885665797 ) ) ;
#60567 = CIRCLE ( 'NONE', #18559, 48.09070567114147110 ) ;
#60568 = B_SPLINE_CURVE_WITH_KNOTS ( 'NONE', 3,
 ( #49174, #24441, #47954, #24132 ),
 .UNSPECIFIED., .F., .F.,
 ( 4, 4 ),
 ( 2.030239133983568861E-17, 0.004444306975806114161 ),
 .UNSPECIFIED. ) ;
#60569 = ORIENTED_EDGE ( 'NONE', *, *, #9742, .F. ) ;
#60570 = CARTESIAN_POINT ( 'NONE',  ( 5.880360259849739535, 15.37531919565236116, -45.44137230084866275 ) ) ;
#60571 = CARTESIAN_POINT ( 'NONE',  ( 0.2885697896453112143, -10.38006191081390917, -41.84838128162056847 ) ) ;
#60572 = CARTESIAN_POINT ( 'NONE',  ( 0.1103878639767399278, 39.82320122342704138, -16.54784522866428986 ) ) ;
#60573 = ORIENTED_EDGE ( 'NONE', *, *, #7457, .F. ) ;
#60574 = CARTESIAN_POINT ( 'NONE',  ( -0.6543461111163939581, -4.241015250120822699, -5.460849780464846148 ) ) ;
#60575 = CARTESIAN_POINT ( 'NONE',  ( 4.553261556744875094, 0.000000000000000000, 0.000000000000000000 ) ) ;
#60576 = CARTESIAN_POINT ( 'NONE',  ( 0.9752132459055858904, 30.50512806189410497, 30.17566824627255428 ) ) ;
#60577 = CARTESIAN_POINT ( 'NONE',  ( 0.7954190325252772364, 38.68220061605128279, 28.58653703871169682 ) ) ;
#60578 = ORIENTED_EDGE ( 'NONE', *, *, #52188, .F. ) ;
#60579 = CARTESIAN_POINT ( 'NONE',  ( 0.5998501479064708430, -12.95623334615534716, 46.33007877220716608 ) ) ;
#60580 = CARTESIAN_POINT ( 'NONE',  ( 0.6001305935487315502, -37.84751346122875759, 29.70149728382373056 ) ) ;
#60581 = CARTESIAN_POINT ( 'NONE',  ( 3.782625744892853525, -14.09172058606395872, -39.60633175414385931 ) ) ;
#60582 = B_SPLINE_CURVE_WITH_KNOTS ( 'NONE', 3,
 ( #1668, #24582, #39017, #38703, #16112, #34603 ),
 .UNSPECIFIED., .F., .F.,
 ( 4, 2, 4 ),
 ( 7.589415207398531038E-19, 0.0002447193893791721475, 0.0004894387787583435361 ),
 .UNSPECIFIED. ) ;
#60583 = CARTESIAN_POINT ( 'NONE',  ( 0.9754292580325133466, -23.03905107044544565, 35.00756479216186534 ) ) ;
#60584 = CARTESIAN_POINT ( 'NONE',  ( 2.643462169533600914, 40.89244134039076783, 25.20536747735794236 ) ) ;
#60585 = CARTESIAN_POINT ( 'NONE',  ( 4.962356264823609031, -24.61258717641066696, -34.13877780978592824 ) ) ;
#60586 = CARTESIAN_POINT ( 'NONE',  ( 0.9756354156337447847, -5.471460801653127426, -42.55820231551296473 ) ) ;
#60587 = CARTESIAN_POINT ( 'NONE',  ( 4.967162193818130511, 38.44485641567072776, 19.45289607368836116 ) ) ;
#60588 = ADVANCED_FACE ( 'NONE', ( #3014 ), #59650, .F. ) ;
#60589 = CARTESIAN_POINT ( 'NONE',  ( 0.5837374860065639437, 38.10878877974146661, 29.01294733976374474 ) ) ;
#60590 = CARTESIAN_POINT ( 'NONE',  ( 3.661921753702020332, -9.674343372738375635, -46.03301211240026447 ) ) ;
#60591 = ORIENTED_EDGE ( 'NONE', *, *, #31173, .F. ) ;
#60592 = ADVANCED_FACE ( 'NONE', ( #47191 ), #34082, .F. ) ;
#60593 = CARTESIAN_POINT ( 'NONE',  ( -6.072942160501519027, 15.42355008158960672, 11.52901839575762111 ) ) ;
#60594 = CARTESIAN_POINT ( 'NONE',  ( 0.7056759521544968550, -25.94340635086248881, 39.07286137501344570 ) ) ;
#60595 = DIRECTION ( 'NONE',  ( -1.000000000000000000, -0.000000000000000000, -0.000000000000000000 ) ) ;
#60596 = CARTESIAN_POINT ( 'NONE',  ( -2.569797478183790229, 10.02484965418626395, 10.65947181927842990 ) ) ;
#60597 = CARTESIAN_POINT ( 'NONE',  ( 0.6039202388192953519, -19.71856863334384613, 44.97490148850911140 ) ) ;
#60598 = CARTESIAN_POINT ( 'NONE',  ( 2.299746137290199055, 46.11346518359594882, -16.66822325406706184 ) ) ;
#60599 = APPLICATION_PROTOCOL_DEFINITION ( 'draft international standard', 'automotive_design', 1998, #2759 ) ;
#60600 = CARTESIAN_POINT ( 'NONE',  ( 3.783198216974391404, 3.901161703632050504, 42.86118135813606500 ) ) ;
#60601 = CARTESIAN_POINT ( 'NONE',  ( 0.3676999524040366896, 36.51379593394493384, -24.75264207750488055 ) ) ;
#60602 = CARTESIAN_POINT ( 'NONE',  ( 3.661933894777877452, -18.07631262299097941, -43.42669785866236509 ) ) ;
#60604 = ORIENTED_EDGE ( 'NONE', *, *, #58450, .T. ) ;
#60603 = DIRECTION ( 'NONE',  ( 0.000000000000000000, 0.000000000000000000, 1.000000000000000000 ) ) ;
#60605 = ORIENTED_EDGE ( 'NONE', *, *, #51689, .T. ) ;
#60606 = CARTESIAN_POINT ( 'NONE',  ( 5.880360259849739535, 47.04104239318766645, -9.405269135694755533 ) ) ;
#60607 = CARTESIAN_POINT ( 'NONE',  ( -5.995132425357893702, 7.219211173946491478, 17.40647075750118944 ) ) ;
#60608 = CARTESIAN_POINT ( 'NONE',  ( 4.975610109902397937, -10.32228546579766260, 47.81108480154320972 ) ) ;
#60609 = EDGE_CURVE ( 'NONE', #49088, #40811, #58628, .T. ) ;
#60610 = VECTOR ( 'NONE', #1654, 1000.000000000000000 ) ;
#60611 = ORIENTED_EDGE ( 'NONE', *, *, #37814, .F. ) ;
#60612 = CARTESIAN_POINT ( 'NONE',  ( 0.1129192098497455998, -13.01845098534629486, 42.16007260106758281 ) ) ;
#60613 = CARTESIAN_POINT ( 'NONE',  ( -6.063463321072278589, -6.665223333113649673, 18.06641221712787626 ) ) ;
#60614 = CARTESIAN_POINT ( 'NONE',  ( 0.1103878639767399555, 5.580746265797033701, -42.76182653383951759 ) ) ;
#60615 = ORIENTED_EDGE ( 'NONE', *, *, #30106, .T. ) ;
#60616 = VERTEX_POINT ( 'NONE', #13679 ) ;
#60617 = CARTESIAN_POINT ( 'NONE',  ( 0.9775691876210979014, 25.16245705919257603, -33.51394431776540017 ) ) ;
#60618 = AXIS2_PLACEMENT_3D ( 'NONE', #17256, #2194, #21332 ) ;
#60619 = CARTESIAN_POINT ( 'NONE',  ( -6.016489644550736315, -18.20227673842140348, -4.872725758886381264 ) ) ;
#60620 = CARTESIAN_POINT ( 'NONE',  ( 0.5998501479064708430, 41.39809967730453621, 24.50586714782619424 ) ) ;
#60621 = CARTESIAN_POINT ( 'NONE',  ( 0.5997462898726536595, 44.01516392039513903, -21.77652348757843015 ) ) ;
#60622 = CARTESIAN_POINT ( 'NONE',  ( 0.7954196712028480665, -23.29293472883161442, -42.08256091708695124 ) ) ;
#60623 =( BOUNDED_SURFACE ( )  B_SPLINE_SURFACE ( 3, 1, ( 
 ( #11968, #31049 ),
 ( #50158, #26343 ),
 ( #12885, #45474 ),
 ( #36390, #12577 ) ),
 .UNSPECIFIED., .F., .F., .F. ) 
 B_SPLINE_SURFACE_WITH_KNOTS ( ( 4, 4 ),
 ( 2, 2 ),
 ( 0.000000000000000000, 1.000000000000000000 ),
 ( 0.000000000000000000, 1.000000000000000000 ),
 .UNSPECIFIED. ) 
 GEOMETRIC_REPRESENTATION_ITEM ( )  RATIONAL_B_SPLINE_SURFACE ( (
 ( 1.000000000000000000, 1.000000000000000000),
 ( 0.7282232189291693025, 0.9929344683865674037),
 ( 0.7282232189291693025, 0.9929344683865674037),
 ( 1.000000000000000000, 1.000000000000000000) ) ) 
 REPRESENTATION_ITEM ( '' )  SURFACE ( )  );
#60624 = EDGE_CURVE ( 'NONE', #15275, #41417, #37488, .T. ) ;
#60625 = CARTESIAN_POINT ( 'NONE',  ( -6.078457390727109555, -11.02028633642652444, -15.79075046033844210 ) ) ;
#60626 = FACE_OUTER_BOUND ( 'NONE', #28582, .T. ) ;
#60627 = EDGE_LOOP ( 'NONE', ( #28530, #36544, #59340, #39763 ) ) ;
#60628 = CARTESIAN_POINT ( 'NONE',  ( 0.8760168074887090262, -47.80016357497245849, -5.394043284319338660 ) ) ;
#60629 = B_SPLINE_CURVE_WITH_KNOTS ( 'NONE', 3,
 ( #41539, #25875, #11477, #30562, #12112, #16478, #2047, #50594, #21178, #35609, #7675, #31187, #54668, #11797, #49992, #45320 ),
 .UNSPECIFIED., .F., .F.,
 ( 4, 3, 3, 3, 3, 4 ),
 ( 2.501947744657918636E-17, 0.0002618515315864419768, 0.0003927756766342000512, 0.0005236998216950560468, 0.0007855159896329864293, 0.001047349442285929605 ),
 .UNSPECIFIED. ) ;
#60630 = ORIENTED_EDGE ( 'NONE', *, *, #18755, .T. ) ;
#60631 = CARTESIAN_POINT ( 'NONE',  ( 4.553261556744875094, 0.000000000000000000, 0.000000000000000000 ) ) ;
#60632 = CARTESIAN_POINT ( 'NONE',  ( 0.1313383488274128263, 34.59671037481836464, 25.74310646082161824 ) ) ;
#60633 = CARTESIAN_POINT ( 'NONE',  ( 0.9783242366443551941, 4.461546119134775168, -41.67048231582345608 ) ) ;
#60634 = CARTESIAN_POINT ( 'NONE',  ( 1.227938101723756947, 10.28900963485438425, -41.66816631169181306 ) ) ;
#60635 = ORIENTED_EDGE ( 'NONE', *, *, #56080, .T. ) ;
#60637 = ADVANCED_FACE ( 'NONE', ( #56252 ), #25613, .T. ) ;
#60636 = ORIENTED_EDGE ( 'NONE', *, *, #48849, .F. ) ;
#60638 = FACE_OUTER_BOUND ( 'NONE', #18426, .T. ) ;
#60639 = CARTESIAN_POINT ( 'NONE',  ( 0.5837374860065626114, 41.56971235019486244, 23.79054246377985038 ) ) ;
#60640 = ORIENTED_EDGE ( 'NONE', *, *, #38979, .T. ) ;
#60641 = CARTESIAN_POINT ( 'NONE',  ( 0.3622758884714730732, 26.89560658783340585, 33.69533458712353280 ) ) ;
#60642 =( BOUNDED_SURFACE ( )  B_SPLINE_SURFACE ( 3, 1, ( 
 ( #28643, #37457 ),
 ( #51825, #19268 ),
 ( #37778, #13960 ),
 ( #57432, #14266 ) ),
 .UNSPECIFIED., .F., .F., .F. ) 
 B_SPLINE_SURFACE_WITH_KNOTS ( ( 4, 4 ),
 ( 2, 2 ),
 ( 0.000000000000000000, 1.000000000000000000 ),
 ( 0.000000000000000000, 1.000000000000000000 ),
 .UNSPECIFIED. ) 
 GEOMETRIC_REPRESENTATION_ITEM ( )  RATIONAL_B_SPLINE_SURFACE ( (
 ( 1.000000000000000000, 1.000000000000000000),
 ( 0.7223157951917480446, 0.9931996967497186413),
 ( 0.7223157951917480446, 0.9931996967497186413),
 ( 1.000000000000000000, 1.000000000000000000) ) ) 
 REPRESENTATION_ITEM ( '' )  SURFACE ( )  );
#60643 = VERTEX_POINT ( 'NONE', #8638 ) ;
#60644 = CARTESIAN_POINT ( 'NONE',  ( 4.000000000000003553, 0.3904826640788058856, -2.008738634413572465E-15 ) ) ;
#60645 = ADVANCED_FACE ( 'NONE', ( #23070 ), #15225, .F. ) ;
#60646 = AXIS2_PLACEMENT_3D ( 'NONE', #57880, #29086, #6170 ) ;
#60647 = VERTEX_POINT ( 'NONE', #36255 ) ;
#60648 = CARTESIAN_POINT ( 'NONE',  ( 1.129531546211701931, 8.434754829127421589E-16, 6.887500000000022382 ) ) ;
#60649 = CARTESIAN_POINT ( 'NONE',  ( 0.7954190325252785687, 44.09776758977471189, -19.20649988843073430 ) ) ;
#60650 = B_SPLINE_CURVE_WITH_KNOTS ( 'NONE', 3,
 ( #18168, #4028, #13786, #32577, #14092, #47594, #57261, #61964, #37283, #47907, #23169, #13468, #51345, #9675, #56046, #28783, #19101, #42295, #8429 ),
 .UNSPECIFIED., .F., .F.,
 ( 4, 3, 3, 3, 3, 3, 4 ),
 ( 1.138109825968292890E-16, 0.0002618519381806302536, 0.0003927759815486006373, 0.0005237000248299482005, 0.0006546240681324976083, 0.0007855481115631354197, 0.0009699050456655131103 ),
 .UNSPECIFIED. ) ;
#60651 = VECTOR ( 'NONE', #18007, 1000.000000000000000 ) ;
#60652 = CARTESIAN_POINT ( 'NONE',  ( 0.6031356755852232965, 4.336951783013129340E-16, 48.10744332413860747 ) ) ;
#60653 = EDGE_LOOP ( 'NONE', ( #8671, #40813, #36632, #38103 ) ) ;
#60654 = CARTESIAN_POINT ( 'NONE',  ( 0.1156867017252034557, 43.28642761383349580, 8.557335549546971620 ) ) ;
#60655 = AXIS2_PLACEMENT_3D ( 'NONE', #2166, #36348, #45133 ) ;
#60656 = CARTESIAN_POINT ( 'NONE',  ( 5.895596859100789899, -18.51552686702056150, -7.855154234585556949 ) ) ;
#60657 = EDGE_LOOP ( 'NONE', ( #52696, #48257, #48685, #2951 ) ) ;
#60658 = DIRECTION ( 'NONE',  ( -1.000000000000000000, -1.836909530733573776E-16, -1.361838123766432833E-32 ) ) ;
#60659 = CARTESIAN_POINT ( 'NONE',  ( 4.291220156522060236, -27.13845918422007131, -38.50835013879611068 ) ) ;
#60660 = CARTESIAN_POINT ( 'NONE',  ( -5.571549742892843327, -9.254395351074540699, -1.199999999999999956 ) ) ;
#60661 = CARTESIAN_POINT ( 'NONE',  ( 0.7246131072078556556, -37.65685186358372505, -29.92944207473638585 ) ) ;
#60662 = ORIENTED_EDGE ( 'NONE', *, *, #56160, .F. ) ;
#60663 = ADVANCED_FACE ( 'NONE', ( #3314 ), #2013, .F. ) ;
#60664 = AXIS2_PLACEMENT_3D ( 'NONE', #41098, #16968, #45175 ) ;
#60665 = CARTESIAN_POINT ( 'NONE',  ( 7.926250449004538012, -8.756654308845361001, -4.239809459443226272E-16 ) ) ;
#60666 = CARTESIAN_POINT ( 'NONE',  ( 7.000000000000016875, -56.56854249492410958, 56.56854249492351983 ) ) ;
#60667 = ORIENTED_EDGE ( 'NONE', *, *, #43872, .T. ) ;
#60668 = EDGE_CURVE ( 'NONE', #61502, #29664, #61443, .T. ) ;
#60669 = CARTESIAN_POINT ( 'NONE',  ( 0.5786265663353196143, 18.99608782658092920, -43.97352617418595599 ) ) ;
#60670 = CARTESIAN_POINT ( 'NONE',  ( 4.963659409799330291, 25.25989740981497889, 36.94443854030229346 ) ) ;
#60671 = CARTESIAN_POINT ( 'NONE',  ( 5.901463166500146684, 16.57349776239452055, -11.39460584050806347 ) ) ;
#60672 = DIRECTION ( 'NONE',  ( -1.000000000000000000, -0.000000000000000000, -0.000000000000000000 ) ) ;
#60673 = B_SPLINE_CURVE_WITH_KNOTS ( 'NONE', 3,
 ( #45863, #51437, #51755, #3515 ),
 .UNSPECIFIED., .F., .F.,
 ( 4, 4 ),
 ( 5.682377955034955683E-17, 0.005004948556313868618 ),
 .UNSPECIFIED. ) ;
#60674 = CARTESIAN_POINT ( 'NONE',  ( 0.5850706913938533704, -6.071602062250300413, -47.50996714391789055 ) ) ;
#60675 = CARTESIAN_POINT ( 'NONE',  ( 0.8560838555295223751, -45.77741231505103059, 10.23725333375835689 ) ) ;
#60676 = CARTESIAN_POINT ( 'NONE',  ( 30.00000000000001066, 4.342925291379521108E-15, -1.386669559958810165E-30 ) ) ;
#60677 = EDGE_CURVE ( 'NONE', #50567, #32701, #31658, .T. ) ;
#60678 = CARTESIAN_POINT ( 'NONE',  ( 0.6023142530420679819, 38.32506243004152680, 29.07781306567114754 ) ) ;
#60679 = B_SPLINE_CURVE_WITH_KNOTS ( 'NONE', 3,
 ( #8812, #53557, #24769, #11288, #54169, #53865 ),
 .UNSPECIFIED., .F., .F.,
 ( 4, 2, 4 ),
 ( 6.805474077711127748E-18, 0.0002291472222819931524, 0.0004582944445639795285 ),
 .UNSPECIFIED. ) ;
#60680 = CARTESIAN_POINT ( 'NONE',  ( 0.6001305935487422083, 48.10757715638249010, -0.5236757026884415467 ) ) ;
#60681 = CARTESIAN_POINT ( 'NONE',  ( 1.231276596079881047, 19.39962232756238691, 37.16088568059176112 ) ) ;
#60682 = DIRECTION ( 'NONE',  ( -1.000000000000000000, -0.000000000000000000, -0.000000000000000000 ) ) ;
#60683 = CARTESIAN_POINT ( 'NONE',  ( 5.960721111146673579, 7.848955554238242982, 18.96557324978290282 ) ) ;
#60684 = FACE_OUTER_BOUND ( 'NONE', #1087, .T. ) ;
#60685 = CARTESIAN_POINT ( 'NONE',  ( 3.782625744892852637, -40.81794195064407660, 10.05652618993522651 ) ) ;
#60686 = CARTESIAN_POINT ( 'NONE',  ( 5.894904586330512508, 16.58122937421121534, -11.38385894595667835 ) ) ;
#60687 = EDGE_CURVE ( 'NONE', #25777, #39735, #18888, .T. ) ;
#60688 = CARTESIAN_POINT ( 'NONE',  ( 2.301529144917016545, -44.85388898587012818, -17.18548816179607996 ) ) ;
#60689 = CARTESIAN_POINT ( 'NONE',  ( 0.5832655196449136881, 46.44668467208332174, 6.476161358813500968 ) ) ;
#60690 = CARTESIAN_POINT ( 'NONE',  ( 0.8751705887134553219, -42.09020928323357680, -23.27176129838411001 ) ) ;
#60691 = ORIENTED_EDGE ( 'NONE', *, *, #55858, .F. ) ;
#60692 = AXIS2_PLACEMENT_3D ( 'NONE', #25024, #57891, #29399 ) ;
#60693 = CARTESIAN_POINT ( 'NONE',  ( 0.5806925824938494740, -38.35106547415225009, 26.98922265165951018 ) ) ;
#60694 = CARTESIAN_POINT ( 'NONE',  ( 4.553261556744875094, -33.30082861731464305, -28.64601855797546648 ) ) ;
#60695 = CARTESIAN_POINT ( 'NONE',  ( 0.9730545539215883499, -39.44597740938048958, -16.88610103448599986 ) ) ;
#60696 = CARTESIAN_POINT ( 'NONE',  ( 5.895596859100789899, 10.81936814621369969, 16.95492424427734690 ) ) ;
#60697 = EDGE_LOOP ( 'NONE', ( #43957, #36375, #36433, #8879 ) ) ;
#60698 = CARTESIAN_POINT ( 'NONE',  ( 6.999999999999995559, 56.56854249492450037, -56.56854249492312192 ) ) ;
#60699 = CARTESIAN_POINT ( 'NONE',  ( 0.5998501479064708430, 24.50586714782604858, -41.39809967730462859 ) ) ;
#60700 = ORIENTED_EDGE ( 'NONE', *, *, #50841, .T. ) ;
#60701 = CARTESIAN_POINT ( 'NONE',  ( 5.272379999999998290, 0.000000000000000000, 12.55882000000000076 ) ) ;
#60702 = ORIENTED_EDGE ( 'NONE', *, *, #51962, .F. ) ;
#60703 = EDGE_CURVE ( 'NONE', #45553, #8059, #18682, .T. ) ;
#60704 = DIRECTION ( 'NONE',  ( -1.000000000000000000, -0.000000000000000000, -0.000000000000000000 ) ) ;
#60705 = CARTESIAN_POINT ( 'NONE',  ( 0.5807400328401637335, -33.48217046439086175, -34.25275203086271603 ) ) ;
#60706 = VERTEX_POINT ( 'NONE', #56866 ) ;
#60707 = CARTESIAN_POINT ( 'NONE',  ( 3.660087539127329759, -42.51124390328615732, -22.37124151181823706 ) ) ;
#60708 = CARTESIAN_POINT ( 'NONE',  ( 0.1103744047535531458, 26.22174028894823650, 34.23648668783401661 ) ) ;
#60709 = EDGE_LOOP ( 'NONE', ( #2789, #61030, #58493, #38519 ) ) ;
#60710 = CARTESIAN_POINT ( 'NONE',  ( 0.5837799406558225046, -7.890001094198478171, -46.22760465685791331 ) ) ;
#60711 = CARTESIAN_POINT ( 'NONE',  ( 0.2224561200757604607, -15.79689521915838135, -40.12166550582807645 ) ) ;
#60712 = EDGE_CURVE ( 'NONE', #24826, #18401, #54806, .T. ) ;
#60713 = VECTOR ( 'NONE', #58574, 999.9999999999998863 ) ;
#60714 = VERTEX_POINT ( 'NONE', #53097 ) ;
#60715 = B_SPLINE_CURVE_WITH_KNOTS ( 'NONE', 3,
 ( #48282, #57962, #32964, #61730 ),
 .UNSPECIFIED., .F., .F.,
 ( 4, 4 ),
 ( 0.001752131338475893668, 0.004041751736741000349 ),
 .UNSPECIFIED. ) ;
#60716 = ADVANCED_FACE ( 'NONE', ( #61863 ), #30028, .F. ) ;
#60717 = CARTESIAN_POINT ( 'NONE',  ( 3.270143674763207553, -3.806843787665823431, -13.14781761974173335 ) ) ;
#60718 = VERTEX_POINT ( 'NONE', #19299 ) ;
#60719 = CARTESIAN_POINT ( 'NONE',  ( 0.5838002273316430513, -37.91535410490848079, -29.26514720557058880 ) ) ;
#60720 = ORIENTED_EDGE ( 'NONE', *, *, #22407, .F. ) ;
#60721 = ADVANCED_FACE ( 'NONE', ( #468 ), #8426, .F. ) ;
#60722 = ORIENTED_EDGE ( 'NONE', *, *, #35309, .T. ) ;
#60723 = CARTESIAN_POINT ( 'NONE',  ( 4.956445790444018229, -5.251077430595369577, -46.79705371022334504 ) ) ;
#60724 = CARTESIAN_POINT ( 'NONE',  ( 0.9754292580325133466, -7.544321912686871023, 41.22390900656750290 ) ) ;
#60725 = CARTESIAN_POINT ( 'NONE',  ( 0.7764139734771252632, -44.59376569072301777, 14.54085734844269062 ) ) ;
#60726 = CARTESIAN_POINT ( 'NONE',  ( -2.739355103387248747, -7.962282735394911271, -12.62733624295516854 ) ) ;
#60727 = DIRECTION ( 'NONE',  ( 0.000000000000000000, 0.000000000000000000, -1.000000000000000000 ) ) ;
#60728 = VERTEX_POINT ( 'NONE', #48109 ) ;
#60729 = CARTESIAN_POINT ( 'NONE',  ( 2.879087469061463178, 5.945365031249853160, 43.59764112229663624 ) ) ;
#60730 = CARTESIAN_POINT ( 'NONE',  ( 10.00000000000002132, -85.00000000000001421, -1.925929944387237167E-31 ) ) ;
#60731 = CARTESIAN_POINT ( 'NONE',  ( 3.221118495291109163, 0.4792704474710423601, 43.98331182960114916 ) ) ;
#60732 = ORIENTED_EDGE ( 'NONE', *, *, #59797, .T. ) ;
#60733 = ORIENTED_EDGE ( 'NONE', *, *, #26361, .F. ) ;
#60734 = CARTESIAN_POINT ( 'NONE',  ( -6.078726893082806448, -17.34758611460008382, 8.357948149232223400 ) ) ;
#60735 = CARTESIAN_POINT ( 'NONE',  ( 4.553261556744873317, 31.71129487083125653, 30.39627186743183174 ) ) ;
#60736 = CARTESIAN_POINT ( 'NONE',  ( 1.231276596079881047, 40.19859528295886975, 11.88905834349143653 ) ) ;
#60737 = VERTEX_POINT ( 'NONE', #52171 ) ;
#60738 = CARTESIAN_POINT ( 'NONE',  ( 5.895596859100789899, -2.016778947467960048, -20.01151633159111043 ) ) ;
#60739 = AXIS2_PLACEMENT_3D ( 'NONE', #45737, #3396, #50410 ) ;
#60740 = EDGE_CURVE ( 'NONE', #35873, #18521, #31637, .T. ) ;
#60741 = VERTEX_POINT ( 'NONE', #19002 ) ;
#60743 = CARTESIAN_POINT ( 'NONE',  ( 0.7762777257811932508, 34.49689427664313257, -33.23866587527439265 ) ) ;
#60742 = CONICAL_SURFACE ( 'NONE', #28743, 47.91270532121795611, 0.04450589592585343229 ) ;
#60744 = B_SPLINE_CURVE_WITH_KNOTS ( 'NONE', 3,
 ( #41807, #22994, #17991, #61179, #37108, #18298, #56480, #26753, #45888, #2935, #38643, #19528, #57386, #29214, #43656, #52399 ),
 .UNSPECIFIED., .F., .F.,
 ( 4, 3, 3, 3, 3, 4 ),
 ( 2.027574016683678720E-17, 0.0002618515315864419768, 0.0003927756766341985875, 0.0005236998216950574563, 0.0007855159896329904409, 0.001047349442285928304 ),
 .UNSPECIFIED. ) ;
#60745 = EDGE_CURVE ( 'NONE', #536, #1749, #36683, .T. ) ;
#60746 = CARTESIAN_POINT ( 'NONE',  ( -6.072942160501519915, 7.781335985898532037, -17.61405610765392993 ) ) ;
#60747 = CARTESIAN_POINT ( 'NONE',  ( 0.5830082357119562575, -41.73162262790440735, -21.39401102599778426 ) ) ;
#60748 = CARTESIAN_POINT ( 'NONE',  ( 2.359973842542475886, -41.34914904924381318, -15.11237134059111220 ) ) ;
#60749 = EDGE_CURVE ( 'NONE', #46130, #15298, #34023, .T. ) ;
#60750 = SURFACE_STYLE_USAGE ( .BOTH. , #60437 ) ;
#60751 = DIRECTION ( 'NONE',  ( -1.000000000000000000, -0.000000000000000000, -0.000000000000000000 ) ) ;
#60752 =( BOUNDED_SURFACE ( )  B_SPLINE_SURFACE ( 3, 1, ( 
 ( #25815, #49613 ),
 ( #34306, #6673 ),
 ( #34612, #53992 ),
 ( #11418, #773 ) ),
 .UNSPECIFIED., .F., .F., .F. ) 
 B_SPLINE_SURFACE_WITH_KNOTS ( ( 4, 4 ),
 ( 2, 2 ),
 ( 0.000000000000000000, 1.000000000000000000 ),
 ( 0.000000000000000000, 1.000000000000000000 ),
 .UNSPECIFIED. ) 
 GEOMETRIC_REPRESENTATION_ITEM ( )  RATIONAL_B_SPLINE_SURFACE ( (
 ( 1.000000000000000000, 1.000000000000000000),
 ( 0.7211978278499970862, 0.9934217856018976445),
 ( 0.7211978278499970862, 0.9934217856018976445),
 ( 1.000000000000000000, 1.000000000000000000) ) ) 
 REPRESENTATION_ITEM ( '' )  SURFACE ( )  );
#60753 = VERTEX_POINT ( 'NONE', #57465 ) ;
#60754 = CARTESIAN_POINT ( 'NONE',  ( 4.975610109902397937, -32.45573888811652807, 36.59336579715199633 ) ) ;
#60755 = CARTESIAN_POINT ( 'NONE',  ( 0.7056759521545009628, 28.49525089474759909, -37.25277849452807999 ) ) ;
#60756 = CARTESIAN_POINT ( 'NONE',  ( 0.6846871229502932144, 7.109010606688070055, -47.37786444808385511 ) ) ;
#60757 = CARTESIAN_POINT ( 'NONE',  ( 0.2279481005628818391, 9.075716850154307735, 43.17562797144632469 ) ) ;
#60758 = CARTESIAN_POINT ( 'NONE',  ( 5.895596859100789899, 19.71057157537855176, 4.002693016503615198 ) ) ;
#60759 = CARTESIAN_POINT ( 'NONE',  ( 3.782542959838397056, 31.89521442703278353, 27.38490734054377995 ) ) ;
#60760 = EDGE_CURVE ( 'NONE', #7392, #1703, #33713, .T. ) ;
#60761 = CARTESIAN_POINT ( 'NONE',  ( 0.8560838555295223751, -8.701885300215751684, -46.09392613244852299 ) ) ;
#60762 = AXIS2_PLACEMENT_3D ( 'NONE', #50579, #55579, #12707 ) ;
#60763 = DIRECTION ( 'NONE',  ( -0.07500201931887527651, 0.2442817726706026926, 0.9667994169624839484 ) ) ;
#60764 = B_SPLINE_CURVE_WITH_KNOTS ( 'NONE', 3,
 ( #58736, #1417, #59361, #16790, #35281, #25550 ),
 .UNSPECIFIED., .F., .F.,
 ( 4, 2, 4 ),
 ( 2.710505431213761085E-18, 0.0002447193893791735028, 0.0004894387787583442950 ),
 .UNSPECIFIED. ) ;
#60765 = EDGE_CURVE ( 'NONE', #52785, #21034, #7641, .T. ) ;
#60766 = B_SPLINE_CURVE_WITH_KNOTS ( 'NONE', 3,
 ( #48638, #18928, #5697, #24843, #1865, #37736, #56796, #13926, #33029, #4776, #4465, #19538, #23604, #47419, #38652, #38052, #14534, #29221, #14837 ),
 .UNSPECIFIED., .F., .F.,
 ( 4, 3, 3, 3, 3, 3, 4 ),
 ( 1.153344816771540786E-16, 0.0002618519381806257000, 0.0003927759815485966800, 0.0005237000248299429964, 0.0006546240681324979336, 0.0007855481115631330344, 0.0009699050456655101829 ),
 .UNSPECIFIED. ) ;
#60767 = DIRECTION ( 'NONE',  ( 1.000000000000000000, -0.000000000000000000, -0.000000000000000000 ) ) ;
#60768 = CARTESIAN_POINT ( 'NONE',  ( 0.5809828226811553087, -29.58751527316153940, -37.66417181417581617 ) ) ;
#60769 = ORIENTED_EDGE ( 'NONE', *, *, #20697, .F. ) ;
#60770 = CARTESIAN_POINT ( 'NONE',  ( 3.407937589446174087, -7.243367523631106586, 11.62731850632881780 ) ) ;
#60771 = CARTESIAN_POINT ( 'NONE',  ( 5.959547316686252039, 17.77749189599203206, 10.25972575517536178 ) ) ;
#60772 = CARTESIAN_POINT ( 'NONE',  ( 0.6254311100348659558, -38.58047947916347908, 28.73641524052507279 ) ) ;
#60773 = DIRECTION ( 'NONE',  ( 1.000000000000000000, 0.000000000000000000, 0.000000000000000000 ) ) ;
#60774 = ORIENTED_EDGE ( 'NONE', *, *, #58097, .T. ) ;
#60775 = CARTESIAN_POINT ( 'NONE',  ( -6.077587904424778920, 5.484810954822468609, -18.45840919970596516 ) ) ;
#60776 = CARTESIAN_POINT ( 'NONE',  ( 4.553261556744873317, 38.16266689001211887, -21.75202109381124771 ) ) ;
#60777 = SURFACE_STYLE_FILL_AREA ( #8462 ) ;
#60778 = VERTEX_POINT ( 'NONE', #21444 ) ;
#60779 = CARTESIAN_POINT ( 'NONE',  ( 4.967162193818130511, -2.375726030842277403, -43.02067033766020643 ) ) ;
#60780 = CARTESIAN_POINT ( 'NONE',  ( 4.975610109902397937, 0.000000000000000000, 0.000000000000000000 ) ) ;
#60781 = CARTESIAN_POINT ( 'NONE',  ( 0.5549461598389365813, -11.70502281787141463, 42.52305417417608169 ) ) ;
#60782 = ORIENTED_EDGE ( 'NONE', *, *, #38584, .T. ) ;
#60783 = CARTESIAN_POINT ( 'NONE',  ( 5.896782393890504181, -2.006887468070398750, 20.01245835894516389 ) ) ;
#60784 = CIRCLE ( 'NONE', #34793, 18.99999999999999645 ) ;
#60785 = ORIENTED_EDGE ( 'NONE', *, *, #33268, .T. ) ;
#60786 = ORIENTED_EDGE ( 'NONE', *, *, #40976, .T. ) ;
#60787 = CARTESIAN_POINT ( 'NONE',  ( 0.1064266379913940685, -42.82540706760018878, -5.071708164746911329 ) ) ;
#60788 = EDGE_CURVE ( 'NONE', #12584, #16352, #21879, .T. ) ;
#60789 = ORIENTED_EDGE ( 'NONE', *, *, #40629, .T. ) ;
#60790 = CARTESIAN_POINT ( 'NONE',  ( 5.896782393890504181, 5.952874097602693482, -19.21169895808549200 ) ) ;
#60791 = ORIENTED_EDGE ( 'NONE', *, *, #49782, .T. ) ;
#60792 = EDGE_CURVE ( 'NONE', #10506, #38229, #40648, .T. ) ;
#60793 = FACE_OUTER_BOUND ( 'NONE', #57032, .T. ) ;
#60794 = CARTESIAN_POINT ( 'NONE',  ( 0.7413678028165009426, -0.4803394418903486063, 44.09371118187726069 ) ) ;
#60795 = EDGE_CURVE ( 'NONE', #57613, #23682, #44306, .T. ) ;
#60796 = EDGE_LOOP ( 'NONE', ( #61536, #26182, #47040, #51038 ) ) ;
#60797 = ADVANCED_FACE ( 'NONE', ( #6077 ), #21620, .F. ) ;
#60798 = CARTESIAN_POINT ( 'NONE',  ( 4.553261556744875094, 31.71129487083167220, -30.39627186743139831 ) ) ;
#60799 = AXIS2_PLACEMENT_3D ( 'NONE', #45525, #60206, #32342 ) ;
#60800 = CARTESIAN_POINT ( 'NONE',  ( 0.3676999524040323597, -31.10876963919482563, -31.27610965031216139 ) ) ;
#60801 = CARTESIAN_POINT ( 'NONE',  ( 0.5830082357119570347, -44.21081432357497221, -15.64084178632068500 ) ) ;
#60802 = CARTESIAN_POINT ( 'NONE',  ( 0.5837799406558226156, -30.20780738208704719, 35.87104574366253473 ) ) ;
#60804 = ORIENTED_EDGE ( 'NONE', *, *, #11848, .T. ) ;
#60803 = EDGE_CURVE ( 'NONE', #45637, #21937, #29409, .T. ) ;
#60805 = CARTESIAN_POINT ( 'NONE',  ( -2.271448787322325728E-15, -4.618802153517061804, -5.599999999999999645 ) ) ;
#60806 = ORIENTED_EDGE ( 'NONE', *, *, #61164, .T. ) ;
#60807 = VECTOR ( 'NONE', #30465, 1000.000000000000000 ) ;
#60808 = LINE ( 'NONE', #17928, #53710 ) ;
#60809 =( BOUNDED_SURFACE ( )  B_SPLINE_SURFACE ( 3, 1, ( 
 ( #60183, #46731 ),
 ( #22917, #46121 ),
 ( #17294, #36720 ),
 ( #61099, #17597 ) ),
 .UNSPECIFIED., .F., .F., .F. ) 
 B_SPLINE_SURFACE_WITH_KNOTS ( ( 4, 4 ),
 ( 2, 2 ),
 ( 0.000000000000000000, 1.000000000000000000 ),
 ( 0.000000000000000000, 1.000000000000000000 ),
 .UNSPECIFIED. ) 
 GEOMETRIC_REPRESENTATION_ITEM ( )  RATIONAL_B_SPLINE_SURFACE ( (
 ( 1.000000000000000000, 1.000000000000000000),
 ( 0.7223157951917476005, 0.9931996967497186413),
 ( 0.7223157951917476005, 0.9931996967497186413),
 ( 1.000000000000000000, 1.000000000000000000) ) ) 
 REPRESENTATION_ITEM ( '' )  SURFACE ( )  );
#60810 = ORIENTED_EDGE ( 'NONE', *, *, #58455, .F. ) ;
#60811 = CARTESIAN_POINT ( 'NONE',  ( 0.1156495703730067853, -12.42380213276527279, 42.33901385007647633 ) ) ;
#60812 = EDGE_CURVE ( 'NONE', #17449, #23651, #55462, .T. ) ;
#60813 = CARTESIAN_POINT ( 'NONE',  ( 0.2885700199627521667, 11.93479339212609425, 41.43179222486424607 ) ) ;
#60814 = EDGE_LOOP ( 'NONE', ( #33746, #41673, #48928, #56428 ) ) ;
#60815 = CARTESIAN_POINT ( 'NONE',  ( 0.5832366564991500191, -46.33368520589909423, -12.13301812590398931 ) ) ;
#60816 = CARTESIAN_POINT ( 'NONE',  ( -6.016761891674564211, -4.880293656734836283, -18.20023637398604066 ) ) ;
#60817 = CARTESIAN_POINT ( 'NONE',  ( 0.5824935313925918567, -1.931035634062136630, -46.85626189138252329 ) ) ;
#60818 = STYLED_ITEM ( 'NONE', ( #41382 ), #10540 ) ;
#60819 = VERTEX_POINT ( 'NONE', #58397 ) ;
#60820 = FACE_OUTER_BOUND ( 'NONE', #32323, .T. ) ;
#60821 = CARTESIAN_POINT ( 'NONE',  ( 0.9790850452238869517, -41.81167860008601167, 2.849712776106803958 ) ) ;
#60822 = CARTESIAN_POINT ( 'NONE',  ( 0.9757787079277453479, -16.45683390770812338, 39.62711913632693239 ) ) ;
#60823 = CARTESIAN_POINT ( 'NONE',  ( 0.6025881611877909050, 6.495537368245871690, -47.66695236827169424 ) ) ;
#60824 = DIRECTION ( 'NONE',  ( 0.000000000000000000, 0.000000000000000000, -1.000000000000000000 ) ) ;
#60825 = CARTESIAN_POINT ( 'NONE',  ( -7.459310946700270506E-14, -4.618802153517020948, -5.242734410091827613 ) ) ;
#60826 =( BOUNDED_SURFACE ( )  B_SPLINE_SURFACE ( 3, 1, ( 
 ( #60362, #26564 ),
 ( #17478, #55984 ),
 ( #31894, #59765 ),
 ( #36600, #50975 ) ),
 .UNSPECIFIED., .F., .F., .F. ) 
 B_SPLINE_SURFACE_WITH_KNOTS ( ( 4, 4 ),
 ( 2, 2 ),
 ( 0.000000000000000000, 1.000000000000000000 ),
 ( 0.000000000000000000, 1.000000000000000000 ),
 .UNSPECIFIED. ) 
 GEOMETRIC_REPRESENTATION_ITEM ( )  RATIONAL_B_SPLINE_SURFACE ( (
 ( 1.000000000000000000, 1.000000000000000000),
 ( 0.7269869731126817891, 0.9931720237060910339),
 ( 0.7269869731126817891, 0.9931720237060910339),
 ( 1.000000000000000000, 1.000000000000000000) ) ) 
 REPRESENTATION_ITEM ( '' )  SURFACE ( )  );
#60827 = CARTESIAN_POINT ( 'NONE',  ( 0.5806925824938499181, 46.89268439822727430, -0.5463627657667492477 ) ) ;
#60828 = DIRECTION ( 'NONE',  ( -0.000000000000000000, -0.000000000000000000, 1.000000000000000000 ) ) ;
#60829 = AXIS2_PLACEMENT_3D ( 'NONE', #5008, #48560, #52946 ) ;
#60830 = CARTESIAN_POINT ( 'NONE',  ( 3.678834586032788678, -23.78917523055212513, -42.80989969012353669 ) ) ;
#60831 = VECTOR ( 'NONE', #25643, 1000.000000000000114 ) ;
#60832 = DIRECTION ( 'NONE',  ( 0.000000000000000000, 0.000000000000000000, 1.000000000000000000 ) ) ;
#60833 = FACE_OUTER_BOUND ( 'NONE', #27122, .T. ) ;
#60834 = LINE ( 'NONE', #13252, #33074 ) ;
#60835 = EDGE_CURVE ( 'NONE', #59460, #15516, #993, .T. ) ;
#60836 = CARTESIAN_POINT ( 'NONE',  ( 0.7242486021783860473, 16.18710914557469138, 46.35718886950788686 ) ) ;
#60837 = CARTESIAN_POINT ( 'NONE',  ( 0.5848930533535030563, 46.50190038545817828, -6.070118856207339597 ) ) ;
#60838 = CARTESIAN_POINT ( 'NONE',  ( -2.700785417809981936, -13.56184546075580322, 3.000000000000003997 ) ) ;
#60839 = B_SPLINE_CURVE_WITH_KNOTS ( 'NONE', 3,
 ( #53783, #15310, #24380, #10597, #10915, #39432 ),
 .UNSPECIFIED., .F., .F.,
 ( 4, 2, 4 ),
 ( 0.000000000000000000, 0.0002293801035737099683, 0.0004587602071474199367 ),
 .UNSPECIFIED. ) ;
#60840 = DIRECTION ( 'NONE',  ( 0.000000000000000000, 0.000000000000000000, 1.000000000000000000 ) ) ;
#60841 = ADVANCED_FACE ( 'NONE', ( #49325 ), #10824, .T. ) ;
#60842 = CARTESIAN_POINT ( 'NONE',  ( -2.569797478183783568, 3.352038560005916601, -14.24379821351254094 ) ) ;
#60843 = CARTESIAN_POINT ( 'NONE',  ( 0.8760168074886960365, 11.58706983520261069, 46.68716261866180162 ) ) ;
#60844 = CARTESIAN_POINT ( 'NONE',  ( 0.6016117650947691020, -47.41192139277011108, 12.79299668139902835 ) ) ;
#60846 = EDGE_LOOP ( 'NONE', ( #26220, #16155, #23695, #33868 ) ) ;
#60845 = CARTESIAN_POINT ( 'NONE',  ( 4.962356264823608143, 42.01891079680549268, -2.376285612557975213 ) ) ;
#60847 = ORIENTED_EDGE ( 'NONE', *, *, #60171, .T. ) ;
#60848 = AXIS2_PLACEMENT_3D ( 'NONE', #17257, #51359, #8444 ) ;
#60849 = CARTESIAN_POINT ( 'NONE',  ( 0.5804410086790514622, 43.38796872094628299, -17.80460676694615785 ) ) ;
#60850 = CARTESIAN_POINT ( 'NONE',  ( 0.7764139734771249302, -18.93147429300290341, -42.91433038042463721 ) ) ;
#60851 = CARTESIAN_POINT ( 'NONE',  ( 0.7762777257811945830, -34.49689427664289809, 33.23866587527464844 ) ) ;
#60852 = VERTEX_POINT ( 'NONE', #16139 ) ;
#60853 = ORIENTED_EDGE ( 'NONE', *, *, #36439, .F. ) ;
#60854 = DIRECTION ( 'NONE',  ( 0.000000000000000000, -0.7071067811865487940, 0.7071067811865461294 ) ) ;
#60855 = CARTESIAN_POINT ( 'NONE',  ( 0.6000166863083090663, -39.66797998683833271, -28.95297645272843567 ) ) ;
#60856 =( GEOMETRIC_REPRESENTATION_CONTEXT ( 3 ) GLOBAL_UNCERTAINTY_ASSIGNED_CONTEXT ( ( #26122 ) ) GLOBAL_UNIT_ASSIGNED_CONTEXT ( ( #60994, #13104, #55363 ) ) REPRESENTATION_CONTEXT ( 'NONE', 'WORKASPACE' ) );
#60857 = ORIENTED_EDGE ( 'NONE', *, *, #56910, .T. ) ;
#60858 = ORIENTED_EDGE ( 'NONE', *, *, #40466, .T. ) ;
#60859 = CARTESIAN_POINT ( 'NONE',  ( 1.231276596079887264, 19.39962232756291272, -37.16088568059149111 ) ) ;
#60860 = DIRECTION ( 'NONE',  ( 0.000000000000000000, 0.4999999999999990008, -0.8660254037844391517 ) ) ;
#60861 = DIRECTION ( 'NONE',  ( 0.000000000000000000, 0.000000000000000000, 1.000000000000000000 ) ) ;
#60862 = CONICAL_SURFACE ( 'NONE', #35768, 43.92652462719577500, 1.486293639869522343 ) ;
#60863 = EDGE_LOOP ( 'NONE', ( #2506, #31124, #11659, #21805 ) ) ;
#60864 = EDGE_LOOP ( 'NONE', ( #45066, #54673, #33618, #30807 ) ) ;
#60865 = B_SPLINE_CURVE_WITH_KNOTS ( 'NONE', 3,
 ( #31316, #45744, #2794, #21926 ),
 .UNSPECIFIED., .F., .F.,
 ( 4, 4 ),
 ( 0.000000000000000000, 0.005004741218457433617 ),
 .UNSPECIFIED. ) ;
#60866 = CARTESIAN_POINT ( 'NONE',  ( 0.1129192098497447394, -13.01845098534572820, -42.16007260106777466 ) ) ;
#60867 = EDGE_CURVE ( 'NONE', #2711, #18038, #44688, .T. ) ;
#60868 = CARTESIAN_POINT ( 'NONE',  ( 0.1084644655670282676, 21.90577137312941147, 37.14658555883740121 ) ) ;
#60869 = EDGE_CURVE ( 'NONE', #34397, #15656, #45277, .T. ) ;
#60870 = ORIENTED_EDGE ( 'NONE', *, *, #51828, .T. ) ;
#60871 = CIRCLE ( 'NONE', #6845, 48.09070567114147110 ) ;
#60872 = ORIENTED_EDGE ( 'NONE', *, *, #6308, .T. ) ;
#60873 = EDGE_CURVE ( 'NONE', #59710, #51483, #3983, .T. ) ;
#60874 = FACE_OUTER_BOUND ( 'NONE', #32034, .T. ) ;
#60875 = AXIS2_PLACEMENT_3D ( 'NONE', #36655, #16933, #26614 ) ;
#60876 = EDGE_LOOP ( 'NONE', ( #48848, #51806, #58390, #53922 ) ) ;
#60877 = CARTESIAN_POINT ( 'NONE',  ( 1.227938101723756947, 20.72293514920803048, -37.58536632582757875 ) ) ;
#60878 = CARTESIAN_POINT ( 'NONE',  ( 3.782625744892854414, 23.52694838945772915, -34.83849600047044248 ) ) ;
#60879 = CARTESIAN_POINT ( 'NONE',  ( 0.6031356755773454870, 34.01708126935042031, -34.01711753073222866 ) ) ;
#60880 = EDGE_CURVE ( 'NONE', #7194, #49527, #16638, .T. ) ;
#60881 = CARTESIAN_POINT ( 'NONE',  ( 0.6001305935487315502, -29.70149728382410714, -37.84751346122845916 ) ) ;
#60882 = CARTESIAN_POINT ( 'NONE',  ( 0.5987334363312690755, -2.178790225517574619, 49.05930879685593027 ) ) ;
#60883 = VERTEX_POINT ( 'NONE', #46822 ) ;
#60884 = CARTESIAN_POINT ( 'NONE',  ( 0.7056759521544980762, 16.06728742641350394, 44.06348946547473133 ) ) ;
#60885 = CARTESIAN_POINT ( 'NONE',  ( -6.072942160501519915, 18.62280723096624868, -4.898490903052839407 ) ) ;
#60886 = B_SPLINE_CURVE_WITH_KNOTS ( 'NONE', 3,
 ( #33735, #488, #34046, #9916 ),
 .UNSPECIFIED., .F., .F.,
 ( 4, 4 ),
 ( 0.000000000000000000, 0.005014147105413701254 ),
 .UNSPECIFIED. ) ;
#60887 = CARTESIAN_POINT ( 'NONE',  ( 0.7048096507298635682, 47.58126109679103166, -7.115188260603352965 ) ) ;
#60888 = B_SPLINE_CURVE_WITH_KNOTS ( 'NONE', 3,
 ( #25566, #5514, #44703, #30564, #1743, #49071 ),
 .UNSPECIFIED., .F., .F.,
 ( 4, 2, 4 ),
 ( 0.000000000000000000, 0.0002447195606305748003, 0.0004894391212611496006 ),
 .UNSPECIFIED. ) ;
#60889 = EDGE_LOOP ( 'NONE', ( #17269, #42841, #25892, #40636 ) ) ;
#60890 = CARTESIAN_POINT ( 'NONE',  ( 0.2940133293163012529, 15.98885808696028832, -41.11686961154860143 ) ) ;
#60891 = CARTESIAN_POINT ( 'NONE',  ( 0.3676999524040366896, 30.26295534861856495, 32.09523511193457068 ) ) ;
#60892 = CARTESIAN_POINT ( 'NONE',  ( 0.9756008150404603674, 30.44122083654219679, 30.24019526051556639 ) ) ;
#60893 = CARTESIAN_POINT ( 'NONE',  ( 4.956445790444004018, -43.56224489968086999, -17.88487823385623443 ) ) ;
#60894 = B_SPLINE_CURVE_WITH_KNOTS ( 'NONE', 3,
 ( #27689, #28916, #57096, #8889 ),
 .UNSPECIFIED., .F., .F.,
 ( 4, 4 ),
 ( 1.192622389734054685E-18, 0.004444878191957673044 ),
 .UNSPECIFIED. ) ;
#60895 = EDGE_CURVE ( 'NONE', #23287, #5908, #23426, .T. ) ;
#60896 = CIRCLE ( 'NONE', #58878, 4.000000000000000888 ) ;
#60897 = VERTEX_POINT ( 'NONE', #17675 ) ;
#60898 = CARTESIAN_POINT ( 'NONE',  ( 0.1119899015040013435, 19.90994828224765101, 39.37709064406269022 ) ) ;
#60899 = CARTESIAN_POINT ( 'NONE',  ( 4.975610109902397937, 8.374023221152469887, -48.19050883970174226 ) ) ;
#60900 = CARTESIAN_POINT ( 'NONE',  ( 4.975610109902397937, -40.67634447773578898, -27.16402781375298403 ) ) ;
#60901 = CARTESIAN_POINT ( 'NONE',  ( 5.860006189529246790, 36.25227510158463673, 31.81514841426769635 ) ) ;
#60902 = CARTESIAN_POINT ( 'NONE',  ( 0.1152339509894530906, -18.06478845168980385, -40.25675233611048753 ) ) ;
#60904 = CARTESIAN_POINT ( 'NONE',  ( 0.5806925824938494740, -46.75147433417404841, 3.677228565731047283 ) ) ;
#60903 = AXIS2_PLACEMENT_3D ( 'NONE', #53733, #29956, #7048 ) ;
#60905 = CARTESIAN_POINT ( 'NONE',  ( 0.3676999524040323597, -7.853951980432424484, 43.40813312746703190 ) ) ;
#60906 = CARTESIAN_POINT ( 'NONE',  ( 0.6254311100348673991, -46.28443883864387942, -13.11433105842126601 ) ) ;
#60907 = CARTESIAN_POINT ( 'NONE',  ( 0.9788927965476020843, -1.541996045496603074, -41.88029203369348608 ) ) ;
#60908 =( BOUNDED_SURFACE ( )  B_SPLINE_SURFACE ( 3, 1, ( 
 ( #12955, #61747 ),
 ( #37070, #22958 ),
 ( #42688, #51430 ),
 ( #46462, #27958 ) ),
 .UNSPECIFIED., .F., .F., .F. ) 
 B_SPLINE_SURFACE_WITH_KNOTS ( ( 4, 4 ),
 ( 2, 2 ),
 ( 0.000000000000000000, 1.000000000000000000 ),
 ( 0.000000000000000000, 1.000000000000000000 ),
 .UNSPECIFIED. ) 
 GEOMETRIC_REPRESENTATION_ITEM ( )  RATIONAL_B_SPLINE_SURFACE ( (
 ( 1.000000000000000000, 1.000000000000000000),
 ( 0.7223157951917476005, 0.9931996967497186413),
 ( 0.7223157951917476005, 0.9931996967497186413),
 ( 1.000000000000000000, 1.000000000000000000) ) ) 
 REPRESENTATION_ITEM ( '' )  SURFACE ( )  );
#60909 = CARTESIAN_POINT ( 'NONE',  ( 3.678748215320120973, -12.15226684749034014, 47.44402201296672672 ) ) ;
#60910 = EDGE_LOOP ( 'NONE', ( #3529, #27536, #38574, #29344 ) ) ;
#60911 = CARTESIAN_POINT ( 'NONE',  ( 0.7056555295713303755, 11.58338207350465154, -46.47980662829223064 ) ) ;
#60912 = CARTESIAN_POINT ( 'NONE',  ( 2.528100132419516477, -41.78722613136653763, 4.010175916105612970 ) ) ;
#60913 = CARTESIAN_POINT ( 'NONE',  ( 0.5997462898726536595, -13.47075269803089803, -47.22383351542737984 ) ) ;
#60914 = CARTESIAN_POINT ( 'NONE',  ( 4.975610109902397937, 8.374023221152469887, -48.19050883970174226 ) ) ;
#60915 = DIRECTION ( 'NONE',  ( -1.000000000000000000, -0.000000000000000000, -0.000000000000000000 ) ) ;
#60916 = CARTESIAN_POINT ( 'NONE',  ( 2.000000000000010658, -3.464101615137748169, 0.000000000000000000 ) ) ;
#60917 = B_SPLINE_CURVE_WITH_KNOTS ( 'NONE', 3,
 ( #36970, #21924, #50117, #22540 ),
 .UNSPECIFIED., .F., .F.,
 ( 4, 4 ),
 ( 0.000000000000000000, 0.004445488388166990781 ),
 .UNSPECIFIED. ) ;
#60918 = APPLICATION_PROTOCOL_DEFINITION ( 'draft international standard', 'automotive_design', 1998, #38386 ) ;
#60919 = CARTESIAN_POINT ( 'NONE',  ( 0.5835871038041877679, -25.34891654652388837, 39.45461801638514743 ) ) ;
#60920 = B_SPLINE_CURVE_WITH_KNOTS ( 'NONE', 3,
 ( #42191, #60622, #51232, #3611, #8023, #61248 ),
 .UNSPECIFIED., .F., .F.,
 ( 4, 2, 4 ),
 ( 1.292312595306281327E-16, 0.0002450741128632353779, 0.0004901482257263415189 ),
 .UNSPECIFIED. ) ;
#60921 = EDGE_CURVE ( 'NONE', #27918, #37400, #60022, .T. ) ;
#60922 = CARTESIAN_POINT ( 'NONE',  ( 5.910764540655177868, 16.57257352145941098, 11.39522028505748708 ) ) ;
#60923 = VECTOR ( 'NONE', #36619, 1000.000000000000114 ) ;
#60924 = CARTESIAN_POINT ( 'NONE',  ( 0.6026112563231247332, -1.748029877735236770, 49.07632205504760492 ) ) ;
#60925 =( BOUNDED_SURFACE ( )  B_SPLINE_SURFACE ( 3, 1, ( 
 ( #50441, #40455 ),
 ( #2508, #21947 ),
 ( #7828, #45767 ),
 ( #2813, #59519 ) ),
 .UNSPECIFIED., .F., .F., .F. ) 
 B_SPLINE_SURFACE_WITH_KNOTS ( ( 4, 4 ),
 ( 2, 2 ),
 ( 0.000000000000000000, 1.000000000000000000 ),
 ( 0.000000000000000000, 1.000000000000000000 ),
 .UNSPECIFIED. ) 
 GEOMETRIC_REPRESENTATION_ITEM ( )  RATIONAL_B_SPLINE_SURFACE ( (
 ( 1.000000000000000000, 1.000000000000000000),
 ( 0.9952954269826590483, 0.8620686068821339365),
 ( 0.9952954269826590483, 0.8620686068821339365),
 ( 1.000000000000000000, 1.000000000000000000) ) ) 
 REPRESENTATION_ITEM ( '' )  SURFACE ( )  );
#60927 = EDGE_LOOP ( 'NONE', ( #15301, #48995, #17848, #21623 ) ) ;
#60926 = CARTESIAN_POINT ( 'NONE',  ( 0.6023142530420679819, -46.53533807097421260, -12.19802990522784469 ) ) ;
#60928 = ORIENTED_EDGE ( 'NONE', *, *, #29335, .F. ) ;
#60929 = CARTESIAN_POINT ( 'NONE',  ( 0.1100053167205930771, -43.12409768020066281, 0.1794603581042977236 ) ) ;
#60930 = CARTESIAN_POINT ( 'NONE',  ( 5.860006189529246790, -43.25137511473236174, -21.34829429597512629 ) ) ;
#60931 = DIRECTION ( 'NONE',  ( -1.000000000000000000, -0.000000000000000000, -0.000000000000000000 ) ) ;
#60932 =( BOUNDED_SURFACE ( )  B_SPLINE_SURFACE ( 3, 1, ( 
 ( #34950, #44362 ),
 ( #44065, #43434 ),
 ( #33718, #6382 ),
 ( #1093, #6082 ) ),
 .UNSPECIFIED., .F., .F., .F. ) 
 B_SPLINE_SURFACE_WITH_KNOTS ( ( 4, 4 ),
 ( 2, 2 ),
 ( 0.000000000000000000, 1.000000000000000000 ),
 ( 0.000000000000000000, 1.000000000000000000 ),
 .UNSPECIFIED. ) 
 GEOMETRIC_REPRESENTATION_ITEM ( )  RATIONAL_B_SPLINE_SURFACE ( (
 ( 1.000000000000000000, 1.000000000000000000),
 ( 0.7269869731126821222, 0.9931720237060910339),
 ( 0.7269869731126821222, 0.9931720237060910339),
 ( 1.000000000000000000, 1.000000000000000000) ) ) 
 REPRESENTATION_ITEM ( '' )  SURFACE ( )  );
#60933 = B_SPLINE_CURVE_WITH_KNOTS ( 'NONE', 3,
 ( #61660, #24091, #23170, #33817 ),
 .UNSPECIFIED., .F., .F.,
 ( 4, 4 ),
 ( 2.385053804394773788E-17, 0.004559932413162187670 ),
 .UNSPECIFIED. ) ;
#60934 = ORIENTED_EDGE ( 'NONE', *, *, #23981, .T. ) ;
#60935 = CARTESIAN_POINT ( 'NONE',  ( 0.5830082357119558134, 22.29740569870308775, 41.25600240020573040 ) ) ;
#60936 = DIRECTION ( 'NONE',  ( 0.000000000000000000, 0.000000000000000000, 1.000000000000000000 ) ) ;
#60937 = CARTESIAN_POINT ( 'NONE',  ( 0.8760168074886960365, 33.37827814204077015, 34.63873394077499057 ) ) ;
#60938 = VERTEX_POINT ( 'NONE', #3861 ) ;
#60939 = VERTEX_POINT ( 'NONE', #13604 ) ;
#60940 = SURFACE_STYLE_USAGE ( .BOTH. , #23665 ) ;
#60941 = VECTOR ( 'NONE', #33195, 1000.000000000000000 ) ;
#60942 = DIRECTION ( 'NONE',  ( -0.7071067811865364705, 0.000000000000000000, 0.7071067811865584529 ) ) ;
#60943 = CARTESIAN_POINT ( 'NONE',  ( 0.6017667736363749853, 41.48674115080369518, 24.35549005323431260 ) ) ;
#60944 = CARTESIAN_POINT ( 'NONE',  ( 2.359973842542475886, -43.99839348535093109, 1.509061079190917587 ) ) ;
#60945 = CARTESIAN_POINT ( 'NONE',  ( 5.895596859100789899, -18.51552686702066808, 7.855154234585303819 ) ) ;
#60946 = CARTESIAN_POINT ( 'NONE',  ( 0.6253024248130480967, 37.83345337727645585, -31.30613411085905895 ) ) ;
#60947 = CARTESIAN_POINT ( 'NONE',  ( -6.016104459813374383, -7.215917642689192668, 17.40682403289246238 ) ) ;
#60948 = EDGE_CURVE ( 'NONE', #43360, #24504, #16659, .T. ) ;
#60949 = ORIENTED_EDGE ( 'NONE', *, *, #20893, .T. ) ;
#60950 = FACE_OUTER_BOUND ( 'NONE', #44959, .T. ) ;
#60951 = CARTESIAN_POINT ( 'NONE',  ( 2.648799415243696664, 18.22894499609882502, -45.52167645879051605 ) ) ;
#60952 = ORIENTED_EDGE ( 'NONE', *, *, #60895, .T. ) ;
#60953 = CARTESIAN_POINT ( 'NONE',  ( 0.6031357023905875581, -47.69018446756504659, -6.322524267548415011 ) ) ;
#60954 = DIRECTION ( 'NONE',  ( -1.000000000000000000, -0.000000000000000000, -0.000000000000000000 ) ) ;
#60955 = EDGE_CURVE ( 'NONE', #61570, #50394, #32710, .T. ) ;
#60956 = CARTESIAN_POINT ( 'NONE',  ( 2.533389852662419894, 38.94530847225836823, -20.51130126867280268 ) ) ;
#60957 = CARTESIAN_POINT ( 'NONE',  ( 0.7954196712028472893, -7.138712347928534818, 47.56618050291063327 ) ) ;
#60958 = VERTEX_POINT ( 'NONE', #40894 ) ;
#60959 = EDGE_LOOP ( 'NONE', ( #30954, #40869, #44486, #10109 ) ) ;
#60960 = FACE_OUTER_BOUND ( 'NONE', #25899, .T. ) ;
#60961 = LINE ( 'NONE', #3624, #1982 ) ;
#60962 = CARTESIAN_POINT ( 'NONE',  ( 4.975610109902397937, 0.000000000000000000, 0.000000000000000000 ) ) ;
#60963 = CIRCLE ( 'NONE', #33989, 43.08621763946400307 ) ;
#60964 = ORIENTED_EDGE ( 'NONE', *, *, #53361, .F. ) ;
#60965 = CARTESIAN_POINT ( 'NONE',  ( 4.000000000000003553, 1.557668341133516154, -0.1596965656957575475 ) ) ;
#60966 = ORIENTED_EDGE ( 'NONE', *, *, #3890, .F. ) ;
#60967 = CARTESIAN_POINT ( 'NONE',  ( 1.657374760986086271, 43.46266450627546618, 7.203279896490761836 ) ) ;
#60968 = CARTESIAN_POINT ( 'NONE',  ( 4.962356264823608143, 0.000000000000000000, 0.000000000000000000 ) ) ;
#60969 = ADVANCED_FACE ( 'NONE', ( #60255 ), #46647, .F. ) ;
#60970 = AXIS2_PLACEMENT_3D ( 'NONE', #15209, #33395, #52165 ) ;
#60971 = CARTESIAN_POINT ( 'NONE',  ( 4.691466044806102964, 29.64918311951129226, -33.30232861642401332 ) ) ;
#60972 = VERTEX_POINT ( 'NONE', #56183 ) ;
#60973 = FACE_OUTER_BOUND ( 'NONE', #44666, .T. ) ;
#60974 = CARTESIAN_POINT ( 'NONE',  ( 0.1156867017252034280, -27.60855798176574183, 34.41962134368514370 ) ) ;
#60975 = ADVANCED_FACE ( 'NONE', ( #13293 ), #17660, .T. ) ;
#60976 = ORIENTED_EDGE ( 'NONE', *, *, #48542, .T. ) ;
#60977 = CARTESIAN_POINT ( 'NONE',  ( -19.26650277682250589, -12.38848617149161946, 1.677297214494516631 ) ) ;
#60978 = CARTESIAN_POINT ( 'NONE',  ( 4.960156602257182357, 46.28683144126590321, 3.546989772330050084 ) ) ;
#60979 = CARTESIAN_POINT ( 'NONE',  ( 5.896782393890504181, 10.81700609697876736, 16.95636948099257424 ) ) ;
#60980 = CARTESIAN_POINT ( 'NONE',  ( 1.227938101723756947, 41.66816631169191965, 10.28900963485394904 ) ) ;
#60981 = CARTESIAN_POINT ( 'NONE',  ( 5.958863334805807099, -19.82657410201446524, 5.311251202228508106 ) ) ;
#60982 = VERTEX_POINT ( 'NONE', #36489 ) ;
#60983 = DIRECTION ( 'NONE',  ( 0.09835009131224552170, 0.9951218349151971232, -0.007732607185420483503 ) ) ;
#60984 = CARTESIAN_POINT ( 'NONE',  ( 0.8760168074887090262, -47.56749362999718045, 7.161346975772893586 ) ) ;
#60985 = VECTOR ( 'NONE', #58509, 1000.000000000000000 ) ;
#60986 = ORIENTED_EDGE ( 'NONE', *, *, #7189, .F. ) ;
#60987 = CARTESIAN_POINT ( 'NONE',  ( 5.959547316686252039, -7.851524054666535690, 18.96456592444086908 ) ) ;
#60988 = CARTESIAN_POINT ( 'NONE',  ( -6.063463321072278589, -17.35644658106392058, 8.341115906049047624 ) ) ;
#60989 = CARTESIAN_POINT ( 'NONE',  ( 0.5809828226811553087, 18.83114015454698631, 44.03860873105701046 ) ) ;
#60990 = LINE ( 'NONE', #18098, #56998 ) ;
#60991 = CARTESIAN_POINT ( 'NONE',  ( 4.691466044806102076, -33.30232861642411990, -29.64918311951117502 ) ) ;
#60992 = CARTESIAN_POINT ( 'NONE',  ( 0.7245667037590741710, -41.24129124474318075, 24.75815201345775662 ) ) ;
#60993 = CARTESIAN_POINT ( 'NONE',  ( 0.5786265663353153954, -43.97352617418629706, 18.99608782658018313 ) ) ;
#60994 =( LENGTH_UNIT ( ) NAMED_UNIT ( * ) SI_UNIT ( .MILLI., .METRE. ) );
#60995 = CARTESIAN_POINT ( 'NONE',  ( 0.6029303876144825880, 47.67862422489724850, 6.409038528276291835 ) ) ;
#60996 = ADVANCED_FACE ( 'NONE', ( #7961 ), #29632, .T. ) ;
#60997 = DIRECTION ( 'NONE',  ( 0.000000000000000000, 0.000000000000000000, 1.000000000000000000 ) ) ;
#60998 = CARTESIAN_POINT ( 'NONE',  ( 1.000110580585049647, 19.56154407020022745, 37.06431540392340196 ) ) ;
#60999 = CARTESIAN_POINT ( 'NONE',  ( 0.1073791018717483448, -5.147744207007177053, 42.81622261970985477 ) ) ;
#61000 = ORIENTED_EDGE ( 'NONE', *, *, #47258, .F. ) ;
#61001 = CARTESIAN_POINT ( 'NONE',  ( 3.782542959838394392, 35.26067992111592275, 22.88934915844450657 ) ) ;
#61002 = CARTESIAN_POINT ( 'NONE',  ( 1.231276596079887931, -40.90292846002456173, 9.177538581350681568 ) ) ;
#61003 = CARTESIAN_POINT ( 'NONE',  ( 7.999999999999981348, 85.00000000000001421, 1.040949779275250495E-14 ) ) ;
#61004 = CARTESIAN_POINT ( 'NONE',  ( 2.299652685299201860, 29.09982397834946255, -39.46494608240623592 ) ) ;
#61005 = FACE_BOUND ( 'NONE', #9622, .T. ) ;
#61006 = PLANE ( 'NONE',  #54836 ) ;
#61007 =( BOUNDED_SURFACE ( )  B_SPLINE_SURFACE ( 3, 1, ( 
 ( #34489, #19164 ),
 ( #4701, #28529 ),
 ( #38275, #53560 ),
 ( #10677, #19462 ) ),
 .UNSPECIFIED., .F., .F., .F. ) 
 B_SPLINE_SURFACE_WITH_KNOTS ( ( 4, 4 ),
 ( 2, 2 ),
 ( 0.000000000000000000, 1.000000000000000000 ),
 ( 0.000000000000000000, 1.000000000000000000 ),
 .UNSPECIFIED. ) 
 GEOMETRIC_REPRESENTATION_ITEM ( )  RATIONAL_B_SPLINE_SURFACE ( (
 ( 1.000000000000000000, 1.000000000000000000),
 ( 0.7223157951917480446, 0.9931996967497186413),
 ( 0.7223157951917480446, 0.9931996967497186413),
 ( 1.000000000000000000, 1.000000000000000000) ) ) 
 REPRESENTATION_ITEM ( '' )  SURFACE ( )  );
#61008 = ORIENTED_EDGE ( 'NONE', *, *, #27002, .F. ) ;
#61009 = CARTESIAN_POINT ( 'NONE',  ( 0.9757892942422827787, 11.05594550521701613, -41.45966865212795938 ) ) ;
#61010 =( BOUNDED_SURFACE ( )  B_SPLINE_SURFACE ( 3, 1, ( 
 ( #40592, #39663 ),
 ( #16149, #54321 ),
 ( #30527, #59653 ),
 ( #16767, #29613 ) ),
 .UNSPECIFIED., .F., .F., .F. ) 
 B_SPLINE_SURFACE_WITH_KNOTS ( ( 4, 4 ),
 ( 2, 2 ),
 ( 0.000000000000000000, 1.000000000000000000 ),
 ( 0.000000000000000000, 1.000000000000000000 ),
 .UNSPECIFIED. ) 
 GEOMETRIC_REPRESENTATION_ITEM ( )  RATIONAL_B_SPLINE_SURFACE ( (
 ( 1.000000000000000000, 1.000000000000000000),
 ( 0.9953390228620291325, 0.8624445117761032620),
 ( 0.9953390228620291325, 0.8624445117761032620),
 ( 1.000000000000000000, 1.000000000000000000) ) ) 
 REPRESENTATION_ITEM ( '' )  SURFACE ( )  );
#61011 = AXIS2_PLACEMENT_3D ( 'NONE', #35647, #49718, #30922 ) ;
#61012 = CARTESIAN_POINT ( 'NONE',  ( 4.322998006666165516, -47.25487450103530307, -8.359821156456311186 ) ) ;
#61013 = CARTESIAN_POINT ( 'NONE',  ( 2.359973842542475886, 28.46303439710156624, -33.58558571086580713 ) ) ;
#61014 = FACE_OUTER_BOUND ( 'NONE', #2875, .T. ) ;
#61015 = VERTEX_POINT ( 'NONE', #36181 ) ;
#61016 = CARTESIAN_POINT ( 'NONE',  ( 5.838029081930955932, -4.708022006887727429, -46.99893176377076287 ) ) ;
#61017 = CARTESIAN_POINT ( 'NONE',  ( 0.8554163680231738898, -38.15570339590799165, -27.30105806512478850 ) ) ;
#61018 = VERTEX_POINT ( 'NONE', #45897 ) ;
#61019 = CLOSED_SHELL ( 'NONE', ( #37872, #780, #25310, #41274, #22863, #45562, #2842, #45238, #45368, #29482, #7071, #61856, #1059, #26957, #31880, #16439, #9764, #31725, #4847, #15381, #31242, #12485 ) ) ;
#61020 = CARTESIAN_POINT ( 'NONE',  ( 0.7044674535453004927, 17.74870190915572010, 45.79067921914718653 ) ) ;
#61021 = EDGE_CURVE ( 'NONE', #54056, #4316, #2942, .T. ) ;
#61022 = ORIENTED_EDGE ( 'NONE', *, *, #22831, .T. ) ;
#61023 = CARTESIAN_POINT ( 'NONE',  ( -6.010958268070873523, -18.84344976839986785, -0.01451635840183061917 ) ) ;
#61024 = TOROIDAL_SURFACE ( 'NONE', #35077, 6.866799999999992465, 0.02570000000000859444 ) ;
#61025 = LINE ( 'NONE', #8399, #45569 ) ;
#61026 = ORIENTED_EDGE ( 'NONE', *, *, #7412, .T. ) ;
#61027 = CARTESIAN_POINT ( 'NONE',  ( 2.281448460670573830, -42.18752512472227068, -22.83953674062058070 ) ) ;
#61028 = CARTESIAN_POINT ( 'NONE',  ( 0.1087620492084205026, 25.96440931622084847, 34.43219573047441173 ) ) ;
#61030 = ORIENTED_EDGE ( 'NONE', *, *, #34652, .F. ) ;
#61029 = EDGE_CURVE ( 'NONE', #58239, #49073, #55555, .T. ) ;
#61031 = CARTESIAN_POINT ( 'NONE',  ( 3.238018933889920792, -9.747366695765370181, 9.186747785039983683 ) ) ;
#61032 = CARTESIAN_POINT ( 'NONE',  ( 0.6845945791218023269, -30.94166671083539910, -35.25648567100138564 ) ) ;
#61033 = ORIENTED_EDGE ( 'NONE', *, *, #40269, .F. ) ;
#61035 = B_SPLINE_CURVE_WITH_KNOTS ( 'NONE', 3,
 ( #33095, #29600, #23983, #61858, #52168, #38115, #19926, #48405, #33399, #5467, #43424, #14915, #14604, #5160, #48106, #43113, #52476, #28993, #39038, #24291, #58091, #464, #9567, #24605, #28679 ),
 .UNSPECIFIED., .F., .F.,
 ( 4, 3, 3, 3, 3, 3, 3, 3, 4 ),
 ( 5.057544569639794935E-18, 0.0005656085177311393148, 0.001131215744874499406, 0.001696821861372765699, 0.002262427090022497717, 0.002828031679238745492, 0.003393635864401604429, 0.003977030878808131623, 0.004561030005651158133 ),
 .UNSPECIFIED. ) ;
#61034 = CARTESIAN_POINT ( 'NONE',  ( 0.6021447746440204973, -8.095348290905777233, -48.43559099605801777 ) ) ;
#61036 = EDGE_CURVE ( 'NONE', #55532, #45559, #40671, .T. ) ;
#61037 = ORIENTED_EDGE ( 'NONE', *, *, #28548, .T. ) ;
#61038 = CARTESIAN_POINT ( 'NONE',  ( 0.5797568665920711517, -39.01551406077552997, -26.01951135542895344 ) ) ;
#61039 = VERTEX_POINT ( 'NONE', #33335 ) ;
#61040 = ORIENTED_EDGE ( 'NONE', *, *, #15648, .F. ) ;
#61041 = CARTESIAN_POINT ( 'NONE',  ( 4.958415959904818315, -5.049385427348107136, -45.14097540626171678 ) ) ;
#61042 = CARTESIAN_POINT ( 'NONE',  ( 0.8551540677456715978, 47.61725548905997840, -5.348818140990417191 ) ) ;
#61043 = CARTESIAN_POINT ( 'NONE',  ( 5.895596859100789899, -11.92767122914705880, 16.19440774656069237 ) ) ;
#61044 = CARTESIAN_POINT ( 'NONE',  ( 4.963659409799328515, -40.34793212403981499, 19.36487359954685417 ) ) ;
#61045 = CARTESIAN_POINT ( 'NONE',  ( 2.009741617377216460, -28.51672276494278080, -33.56040226770888069 ) ) ;
#61046 = VERTEX_POINT ( 'NONE', #47121 ) ;
#61047 = CARTESIAN_POINT ( 'NONE',  ( 0.9754292589017197201, -39.39482825664529742, 14.29597752952562040 ) ) ;
#61048 = DIRECTION ( 'NONE',  ( 1.000000000000000000, 1.836909530733573776E-16, -1.925929944387235853E-32 ) ) ;
#61049 = EDGE_CURVE ( 'NONE', #53786, #40335, #42864, .T. ) ;
#61050 = CARTESIAN_POINT ( 'NONE',  ( -6.078726893082806448, -18.90026279491059924, 3.684305572565647946 ) ) ;
#61051 = ORIENTED_EDGE ( 'NONE', *, *, #52038, .T. ) ;
#61052 = VERTEX_POINT ( 'NONE', #10124 ) ;
#61053 = CARTESIAN_POINT ( 'NONE',  ( 0.1101816497532062955, -21.67974746580523870, -37.27878591512666162 ) ) ;
#61054 = CARTESIAN_POINT ( 'NONE',  ( 0.5988103622719986863, 47.61318311633114320, 6.880137819455026005 ) ) ;
#61055 = CARTESIAN_POINT ( 'NONE',  ( 5.960721111146673579, -5.306302591836717930, 19.82781442290488627 ) ) ;
#61056 = CARTESIAN_POINT ( 'NONE',  ( 0.8753041380234471980, 43.84722337925211377, 22.10337824412700414 ) ) ;
#61057 = CARTESIAN_POINT ( 'NONE',  ( 0.6041374136657475802, 41.74951251761573445, -23.90252055111279716 ) ) ;
#61058 = ORIENTED_EDGE ( 'NONE', *, *, #54278, .F. ) ;
#61059 = CARTESIAN_POINT ( 'NONE',  ( 0.5839880159502344181, 47.48028790449886571, 6.296669079378329315 ) ) ;
#61060 = CARTESIAN_POINT ( 'NONE',  ( 5.901764892641288895, -22.61189840244751181, 43.43608543684697310 ) ) ;
#61061 = CARTESIAN_POINT ( 'NONE',  ( 49.64480425791989404, 15.29488547570532297, 2.514152515238056829 ) ) ;
#61062 = DIRECTION ( 'NONE',  ( -1.000000000000000000, -0.000000000000000000, -0.000000000000000000 ) ) ;
#61063 = CARTESIAN_POINT ( 'NONE',  ( 0.7413678028165007206, -43.60517056639338307, 6.563169329369992866 ) ) ;
#61064 = FACE_OUTER_BOUND ( 'NONE', #19227, .T. ) ;
#61065 = ORIENTED_EDGE ( 'NONE', *, *, #44370, .T. ) ;
#61066 = FACE_OUTER_BOUND ( 'NONE', #35296, .T. ) ;
#61067 = CARTESIAN_POINT ( 'NONE',  ( 5.917102823773431552, 8.473612197389558176, -18.23972626932742358 ) ) ;
#61068 = CARTESIAN_POINT ( 'NONE',  ( 5.895881250540457863, 3.349849349787696440, -19.83194874292559007 ) ) ;
#61069 = CARTESIAN_POINT ( 'NONE',  ( 3.238931869106855377, -1.828840280769088000, -42.95312220797016067 ) ) ;
#61070 = CARTESIAN_POINT ( 'NONE',  ( 5.958863334805807099, -7.855954700275743718, 18.96276366205780661 ) ) ;
#61071 = EDGE_CURVE ( 'NONE', #58688, #57391, #17431, .T. ) ;
#61072 = CARTESIAN_POINT ( 'NONE',  ( 0.5837374860065636106, 6.071555045025283093, -47.50965286059331305 ) ) ;
#61073 = CARTESIAN_POINT ( 'NONE',  ( 5.959547316686252039, 19.82715097195154996, 5.308980600728524735 ) ) ;
#61074 = CARTESIAN_POINT ( 'NONE',  ( 0.3622758884714600280, 41.85013935980101962, -10.35929834645879133 ) ) ;
#61075 = EDGE_CURVE ( 'NONE', #54614, #35968, #14533, .T. ) ;
#61076 = EDGE_CURVE ( 'NONE', #41057, #36974, #36868, .T. ) ;
#61077 = CARTESIAN_POINT ( 'NONE',  ( 2.000000000000027089, 3.464101615137739731, 0.000000000000000000 ) ) ;
#61078 = ORIENTED_EDGE ( 'NONE', *, *, #42600, .T. ) ;
#61079 = DIRECTION ( 'NONE',  ( 0.000000000000000000, 0.000000000000000000, 1.000000000000000000 ) ) ;
#61080 = CARTESIAN_POINT ( 'NONE',  ( 0.9769922540276050338, 19.75190663635009614, 36.96205810442694428 ) ) ;
#61081 = CARTESIAN_POINT ( 'NONE',  ( 4.553261556744873317, -41.75933753256789771, -13.62707946203816967 ) ) ;
#61082 = CARTESIAN_POINT ( 'NONE',  ( 4.975801465491695552, 47.10002938642130488, 8.787181743660319455 ) ) ;
#61083 = EDGE_LOOP ( 'NONE', ( #40925, #37970, #26915 ) ) ;
#61084 = CARTESIAN_POINT ( 'NONE',  ( 1.500000000000001332, 0.000000000000000000, 5.453125000000000000 ) ) ;
#61085 = CARTESIAN_POINT ( 'NONE',  ( 0.9790850452238877288, -41.81844294212524460, -2.748665159565954585 ) ) ;
#61086 = ORIENTED_EDGE ( 'NONE', *, *, #23981, .F. ) ;
#61087 = CARTESIAN_POINT ( 'NONE',  ( 0.1157991065609915715, 4.317964046107984011, -43.91238495042393453 ) ) ;
#61088 = CARTESIAN_POINT ( 'NONE',  ( 9.999999999999991118, 80.00000000000001421, -2.649999999999992806 ) ) ;
#61089 = CARTESIAN_POINT ( 'NONE',  ( 4.335381028904201628, 48.97680438974857253, -1.014632658970608059 ) ) ;
#61090 = ADVANCED_FACE ( 'NONE', ( #29220 ), #2616, .T. ) ;
#61091 = ORIENTED_EDGE ( 'NONE', *, *, #36726, .F. ) ;
#61092 = CARTESIAN_POINT ( 'NONE',  ( 1.227938101723748288, -30.94118573761333479, 29.74462687941215222 ) ) ;
#61093 = ORIENTED_EDGE ( 'NONE', *, *, #41396, .T. ) ;
#61094 = ORIENTED_EDGE ( 'NONE', *, *, #56, .F. ) ;
#61095 = CARTESIAN_POINT ( 'NONE',  ( 10.00000000000002132, -80.00000000000001421, -2.649999999999992806 ) ) ;
#61096 = EDGE_LOOP ( 'NONE', ( #38395, #36855, #46547, #35104 ) ) ;
#61097 = CARTESIAN_POINT ( 'NONE',  ( 0.8557997880470599172, 28.43566216844970640, 38.55640757422448672 ) ) ;
#61098 = ORIENTED_EDGE ( 'NONE', *, *, #60442, .F. ) ;
#61099 = CARTESIAN_POINT ( 'NONE',  ( -6.015611763856276717, 16.31561949997075445, 9.427003116184231146 ) ) ;
#61100 = ADVANCED_FACE ( 'NONE', ( #15141 ), #34248, .T. ) ;
#61101 = AXIS2_PLACEMENT_3D ( 'NONE', #6576, #25722, #12572 ) ;
#61102 = CARTESIAN_POINT ( 'NONE',  ( 0.6000166863083106206, 4.195342255947409171, -48.93079383234974244 ) ) ;
#61103 = CARTESIAN_POINT ( 'NONE',  ( 1.231276596079881047, 8.892602616353681100, 40.96581977363184990 ) ) ;
#61104 = ORIENTED_EDGE ( 'NONE', *, *, #31397, .T. ) ;
#61105 = CARTESIAN_POINT ( 'NONE',  ( 0.9745511491811742477, -16.10518088436877093, -39.77127619790159230 ) ) ;
#61106 = CARTESIAN_POINT ( 'NONE',  ( 5.910764540655177868, 19.71228184310538367, -3.990887496176878102 ) ) ;
#61107 = CARTESIAN_POINT ( 'NONE',  ( 3.390910168358337362, -37.31396665576448868, 23.27584647109819116 ) ) ;
#61108 = CARTESIAN_POINT ( 'NONE',  ( 4.975801465491695552, 0.000000000000000000, 0.000000000000000000 ) ) ;
#61109 = ORIENTED_EDGE ( 'NONE', *, *, #32155, .T. ) ;
#61110 = CARTESIAN_POINT ( 'NONE',  ( 4.962356264823608143, 0.000000000000000000, 0.000000000000000000 ) ) ;
#61111 = ADVANCED_FACE ( 'NONE', ( #53324 ), #42865, .F. ) ;
#61112 = CARTESIAN_POINT ( 'NONE',  ( 5.959547316686252039, 12.49803383497728326, 16.28190225198622443 ) ) ;
#61113 = ORIENTED_EDGE ( 'NONE', *, *, #47376, .F. ) ;
#61114 = CARTESIAN_POINT ( 'NONE',  ( 3.783278058412223643, 22.99727281874625717, 36.37891728069877928 ) ) ;
#61115 = ORIENTED_EDGE ( 'NONE', *, *, #51126, .T. ) ;
#61116 = CARTESIAN_POINT ( 'NONE',  ( 0.1158403557922069033, -12.59083259422814294, 42.28961151119671769 ) ) ;
#61117 =( BOUNDED_SURFACE ( )  B_SPLINE_SURFACE ( 3, 1, ( 
 ( #46753, #18864 ),
 ( #14468, #37986 ),
 ( #14165, #33271 ),
 ( #37349, #18537 ) ),
 .UNSPECIFIED., .F., .F., .F. ) 
 B_SPLINE_SURFACE_WITH_KNOTS ( ( 4, 4 ),
 ( 2, 2 ),
 ( 0.000000000000000000, 1.000000000000000000 ),
 ( 0.000000000000000000, 1.000000000000000000 ),
 .UNSPECIFIED. ) 
 GEOMETRIC_REPRESENTATION_ITEM ( )  RATIONAL_B_SPLINE_SURFACE ( (
 ( 1.000000000000000000, 1.000000000000000000),
 ( 0.9952954269826590483, 0.8620686068821339365),
 ( 0.9952954269826590483, 0.8620686068821339365),
 ( 1.000000000000000000, 1.000000000000000000) ) ) 
 REPRESENTATION_ITEM ( '' )  SURFACE ( )  );
#61118 = CARTESIAN_POINT ( 'NONE',  ( 0.6008123274975392114, 46.74120613782822176, -15.06035191951060526 ) ) ;
#61119 = VERTEX_POINT ( 'NONE', #4165 ) ;
#61120 = DIRECTION ( 'NONE',  ( 0.000000000000000000, 0.000000000000000000, 1.000000000000000000 ) ) ;
#61121 = CARTESIAN_POINT ( 'NONE',  ( 4.958415959904820092, -44.94704195038539751, 6.554950322689975906 ) ) ;
#61122 = CARTESIAN_POINT ( 'NONE',  ( 0.6021447746440204973, 28.30907211267130563, 40.12651959998603957 ) ) ;
#61123 = CARTESIAN_POINT ( 'NONE',  ( 0.5830082357119558134, -1.293980016005006339, -46.87811483684595970 ) ) ;
#61124 = EDGE_LOOP ( 'NONE', ( #38139, #14171, #18505, #5301 ) ) ;
#61125 = CARTESIAN_POINT ( 'NONE',  ( 4.962356264823593932, 31.50371261889118557, 27.90612278853270922 ) ) ;
#61126 = CARTESIAN_POINT ( 'NONE',  ( 5.860006189529246790, -43.26650951066883266, 21.31760477694567513 ) ) ;
#61127 = CARTESIAN_POINT ( 'NONE',  ( 5.960221823109900008, -12.49086489703216607, -16.28736530777586466 ) ) ;
#61129 = B_SPLINE_CURVE_WITH_KNOTS ( 'NONE', 3,
 ( #5433, #15485, #34592, #33985 ),
 .UNSPECIFIED., .F., .F.,
 ( 4, 4 ),
 ( 8.673617379884035472E-19, 0.004042984057420973693 ),
 .UNSPECIFIED. ) ;
#61128 = CARTESIAN_POINT ( 'NONE',  ( -6.016761891674564211, 18.68153697670645030, -2.462934516563616949 ) ) ;
#61130 = CARTESIAN_POINT ( 'NONE',  ( 4.214292481396495482, -11.25702090725073035, -1.199999999999999956 ) ) ;
#61131 = CARTESIAN_POINT ( 'NONE',  ( 3.678834586032787346, -48.30243548991658287, -8.092409738192980484 ) ) ;
#61132 = CARTESIAN_POINT ( 'NONE',  ( 0.9968887458511642707, 39.89008038581167170, -15.81144734640142424 ) ) ;
#61133 = CARTESIAN_POINT ( 'NONE',  ( 0.8744876279028263033, -24.68559978112701714, -42.43785119236734715 ) ) ;
#61134 = CARTESIAN_POINT ( 'NONE',  ( 0.9772918015221174759, -12.01962968694840406, 40.14804301506249118 ) ) ;
#61135 = CARTESIAN_POINT ( 'NONE',  ( 5.960721111146673579, 19.82781442290498219, -5.306302591836375981 ) ) ;
#61136 = EDGE_CURVE ( 'NONE', #39909, #42030, #14449, .T. ) ;
#61137 = CARTESIAN_POINT ( 'NONE',  ( 5.960221823109900008, 5.317678907195162452, 19.82478916873576225 ) ) ;
#61138 = CARTESIAN_POINT ( 'NONE',  ( 0.1097557419366048670, -21.36873056345920219, 37.45792859959189514 ) ) ;
#61139 = CARTESIAN_POINT ( 'NONE',  ( 0.5848930533535030563, 46.45334699384599020, -6.431145734385029122 ) ) ;
#61140 = CARTESIAN_POINT ( 'NONE',  ( 0.9757402383260949108, 37.11731350497355919, 21.52772413548494868 ) ) ;
#61142 = EDGE_CURVE ( 'NONE', #19392, #51621, #9194, .T. ) ;
#61141 = FACE_OUTER_BOUND ( 'NONE', #21496, .T. ) ;
#61143 = CIRCLE ( 'NONE', #53841, 47.09074272231896430 ) ;
#61144 = CARTESIAN_POINT ( 'NONE',  ( 4.956445790443988031, 0.000000000000000000, 0.000000000000000000 ) ) ;
#61145 = ADVANCED_FACE ( 'NONE', ( #47727 ), #12861, .F. ) ;
#61146 = CARTESIAN_POINT ( 'NONE',  ( 0.6845945791218034371, 11.71498854670100975, -45.42208233959124897 ) ) ;
#61147 = CARTESIAN_POINT ( 'NONE',  ( 0.6017667736363749853, 46.55748817282775320, -12.11362382130087845 ) ) ;
#61148 = ADVANCED_FACE ( 'NONE', ( #2243 ), #3593, .T. ) ;
#61150 = ORIENTED_EDGE ( 'NONE', *, *, #28147, .T. ) ;
#61149 = CARTESIAN_POINT ( 'NONE',  ( 0.7048096507298635682, 24.78213711671542185, 41.23648859290934610 ) ) ;
#61151 = ORIENTED_EDGE ( 'NONE', *, *, #13578, .T. ) ;
#61152 = CARTESIAN_POINT ( 'NONE',  ( 5.896782393890504181, -18.51439742298342139, 7.857682542699045314 ) ) ;
#61153 = LINE ( 'NONE', #37383, #53502 ) ;
#61154 = EDGE_CURVE ( 'NONE', #50643, #26909, #59233, .T. ) ;
#61155 = CARTESIAN_POINT ( 'NONE',  ( 5.958863334805807099, 19.82594244347345480, 5.313608583996586532 ) ) ;
#61156 = ORIENTED_EDGE ( 'NONE', *, *, #50417, .F. ) ;
#61157 = ORIENTED_EDGE ( 'NONE', *, *, #15784, .F. ) ;
#61158 = CARTESIAN_POINT ( 'NONE',  ( 2.185380717157383579, -30.61275100921421455, 31.64931719192459880 ) ) ;
#61159 = CARTESIAN_POINT ( 'NONE',  ( 0.5980271706414734822, -39.77423938000247006, -28.81074668563666208 ) ) ;
#61160 = B_SPLINE_CURVE_WITH_KNOTS ( 'NONE', 3,
 ( #51446, #27971, #38020, #51765 ),
 .UNSPECIFIED., .F., .F.,
 ( 4, 4 ),
 ( 9.813077866773594792E-18, 0.005004741218457441423 ),
 .UNSPECIFIED. ) ;
#61161 = UNCERTAINTY_MEASURE_WITH_UNIT (LENGTH_MEASURE( 1.000000000000000082E-05 ), #39456, 'distance_accuracy_value', 'NONE');
#61162 = ORIENTED_EDGE ( 'NONE', *, *, #43575, .F. ) ;
#61163 = VERTEX_POINT ( 'NONE', #25442 ) ;
#61164 = EDGE_CURVE ( 'NONE', #21388, #22462, #45090, .T. ) ;
#61165 = CARTESIAN_POINT ( 'NONE',  ( 0.7948884756798505480, -31.28609784800016769, 37.84017344100726632 ) ) ;
#61166 = EDGE_CURVE ( 'NONE', #55841, #35106, #50262, .T. ) ;
#61167 = CARTESIAN_POINT ( 'NONE',  ( 0.5850706913938534814, -18.49682194437931670, -44.18063951072240769 ) ) ;
#61168 = CARTESIAN_POINT ( 'NONE',  ( 0.9754292589017224957, -1.982398212836277818, -41.86164789184748969 ) ) ;
#61169 = ORIENTED_EDGE ( 'NONE', *, *, #49786, .F. ) ;
#61170 = ORIENTED_EDGE ( 'NONE', *, *, #35112, .T. ) ;
#61171 = CARTESIAN_POINT ( 'NONE',  ( 0.5839879882012681822, -12.39641777360489350, -46.26394433311397592 ) ) ;
#61172 = B_SPLINE_CURVE_WITH_KNOTS ( 'NONE', 3,
 ( #2944, #31461, #12688, #45899 ),
 .UNSPECIFIED., .F., .F.,
 ( 4, 4 ),
 ( 5.421010862427522170E-19, 0.004444878191957664371 ),
 .UNSPECIFIED. ) ;
#61173 = VERTEX_POINT ( 'NONE', #20760 ) ;
#61174 = CARTESIAN_POINT ( 'NONE',  ( 1.227938101723748288, 11.92353943228006585, -41.23019537246697297 ) ) ;
#61175 = CARTESIAN_POINT ( 'NONE',  ( 4.834790513006555379, 37.58952546674482420, -28.62895241026682314 ) ) ;
#61176 = CARTESIAN_POINT ( 'NONE',  ( 2.281448460670569389, -45.98107640562105303, 13.68109378871694481 ) ) ;
#61177 = ORIENTED_EDGE ( 'NONE', *, *, #23967, .T. ) ;
#61178 =( BOUNDED_SURFACE ( )  B_SPLINE_SURFACE ( 3, 1, ( 
 ( #53707, #10520 ),
 ( #52492, #34039 ),
 ( #14621, #10838 ),
 ( #39052, #53109 ) ),
 .UNSPECIFIED., .F., .F., .F. ) 
 B_SPLINE_SURFACE_WITH_KNOTS ( ( 4, 4 ),
 ( 2, 2 ),
 ( 0.000000000000000000, 1.000000000000000000 ),
 ( 0.000000000000000000, 1.000000000000000000 ),
 .UNSPECIFIED. ) 
 GEOMETRIC_REPRESENTATION_ITEM ( )  RATIONAL_B_SPLINE_SURFACE ( (
 ( 1.000000000000000000, 1.000000000000000000),
 ( 0.9952954269826590483, 0.8620686068821339365),
 ( 0.9952954269826590483, 0.8620686068821339365),
 ( 1.000000000000000000, 1.000000000000000000) ) ) 
 REPRESENTATION_ITEM ( '' )  SURFACE ( )  );
#61179 = CARTESIAN_POINT ( 'NONE',  ( 0.6023143664670691511, -48.10676742339276046, -0.2618215695305907698 ) ) ;
#61180 = ORIENTED_EDGE ( 'NONE', *, *, #39693, .F. ) ;
#61181 = ORIENTED_EDGE ( 'NONE', *, *, #49077, .T. ) ;
#61182 = LINE ( 'NONE', #50863, #23549 ) ;
#61183 = ORIENTED_EDGE ( 'NONE', *, *, #27361, .F. ) ;
#61184 = CARTESIAN_POINT ( 'NONE',  ( 0.7764139734771252632, -8.679346378251009853, 46.09457036737849478 ) ) ;
#61185 = CARTESIAN_POINT ( 'NONE',  ( 0.6041374136657476912, 33.89363087703046773, -34.14050483116103862 ) ) ;
#61186 = CARTESIAN_POINT ( 'NONE',  ( 0.7764139734771221546, -20.54893558373679596, 42.16374885232933423 ) ) ;
#61187 = CARTESIAN_POINT ( 'NONE',  ( 0.5834584762367749367, -38.76579285815412845, 26.39032574811979970 ) ) ;
#61188 = DIRECTION ( 'NONE',  ( -1.000000000000000000, 0.000000000000000000, 0.000000000000000000 ) ) ;
#61189 = EDGE_CURVE ( 'NONE', #24422, #38048, #44904, .T. ) ;
#61190 = B_SPLINE_CURVE_WITH_KNOTS ( 'NONE', 3,
 ( #20931, #50352, #30319, #55044 ),
 .UNSPECIFIED., .F., .F.,
 ( 4, 4 ),
 ( 4.670885906470169154E-18, 0.004566006591234647236 ),
 .UNSPECIFIED. ) ;
#61191 = ORIENTED_EDGE ( 'NONE', *, *, #41614, .T. ) ;
#61192 = FACE_OUTER_BOUND ( 'NONE', #20845, .T. ) ;
#61193 = VECTOR ( 'NONE', #57362, 1000.000000000000000 ) ;
#61194 = CARTESIAN_POINT ( 'NONE',  ( -6.077587904424778920, -1.842868750311850601, 19.16767738050321412 ) ) ;
#61195 =( BOUNDED_SURFACE ( )  B_SPLINE_SURFACE ( 3, 1, ( 
 ( #36045, #3402 ),
 ( #60122, #36351 ),
 ( #31627, #36652 ),
 ( #7807, #26932 ) ),
 .UNSPECIFIED., .F., .F., .F. ) 
 B_SPLINE_SURFACE_WITH_KNOTS ( ( 4, 4 ),
 ( 2, 2 ),
 ( 0.000000000000000000, 1.000000000000000000 ),
 ( 0.000000000000000000, 1.000000000000000000 ),
 .UNSPECIFIED. ) 
 GEOMETRIC_REPRESENTATION_ITEM ( )  RATIONAL_B_SPLINE_SURFACE ( (
 ( 1.000000000000000000, 1.000000000000000000),
 ( 0.9732289882329797637, 0.9999525324661233672),
 ( 0.9732289882329797637, 0.9999525324661233672),
 ( 1.000000000000000000, 1.000000000000000000) ) ) 
 REPRESENTATION_ITEM ( '' )  SURFACE ( )  );
#61196 = AXIS2_PLACEMENT_3D ( 'NONE', #22327, #9143, #8212 ) ;
#61197 = EDGE_CURVE ( 'NONE', #34095, #30211, #6856, .T. ) ;
#61198 = CARTESIAN_POINT ( 'NONE',  ( 4.975801465491695552, 36.39623109580423943, 31.15993731089136887 ) ) ;
#61199 = VERTEX_POINT ( 'NONE', #48637 ) ;
#61200 = CARTESIAN_POINT ( 'NONE',  ( 0.9762797500689124330, -22.12212327108586152, -35.59405072711710716 ) ) ;
#61201 = CARTESIAN_POINT ( 'NONE',  ( 0.9758171775293917882, 30.34506652060244747, 30.33669560438079316 ) ) ;
#61202 = CARTESIAN_POINT ( 'NONE',  ( 0.7948884756798505480, -24.70668297336682073, -42.42968843927206279 ) ) ;
#61203 = EDGE_LOOP ( 'NONE', ( #4459, #36098, #1165, #57265 ) ) ;
#61204 = CARTESIAN_POINT ( 'NONE',  ( 5.959547316686252039, 18.96456592444089395, 7.851524054666477959 ) ) ;
#61205 = CARTESIAN_POINT ( 'NONE',  ( 4.960156602257181468, 38.31207700265951388, 26.21519897043440039 ) ) ;
#61206 = DIRECTION ( 'NONE',  ( -0.1011922191286467321, 0.1714634860903305191, -0.9799797996517943810 ) ) ;
#61207 = CARTESIAN_POINT ( 'NONE',  ( 0.5806925824938499181, -29.85799195566266917, -36.16244846134105018 ) ) ;
#61208 = CARTESIAN_POINT ( 'NONE',  ( 1.227938101723756947, -22.18841447410693846, -36.73927144310534487 ) ) ;
#61209 = CARTESIAN_POINT ( 'NONE',  ( 0.9730545539215883499, 42.90536227157002003, 0.5054011016614263774 ) ) ;
#61210 = CARTESIAN_POINT ( 'NONE',  ( 2.281351352603276261, 45.98107981851866555, 13.68106635380579661 ) ) ;
#61211 = CARTESIAN_POINT ( 'NONE',  ( 4.956445790444004018, -40.78973928653763181, -23.53157918788973291 ) ) ;
#61212 = CARTESIAN_POINT ( 'NONE',  ( 0.2940135542859013684, -22.17757310257280778, 38.13654153133788327 ) ) ;
#61213 = CARTESIAN_POINT ( 'NONE',  ( 5.958863334805807099, 10.26176968287920310, 17.77634700750932595 ) ) ;
#61214 = VERTEX_POINT ( 'NONE', #11359 ) ;
#61215 = DIRECTION ( 'NONE',  ( 0.000000000000000000, 0.000000000000000000, 1.000000000000000000 ) ) ;
#61216 = CARTESIAN_POINT ( 'NONE',  ( 0.5987334308729317378, 32.56457219905072975, -36.75746922820641771 ) ) ;
#61217 = CARTESIAN_POINT ( 'NONE',  ( -6.016104459813371719, -11.46679299034590827, 14.95258000663128328 ) ) ;
#61218 = CARTESIAN_POINT ( 'NONE',  ( 0.8760168074886965917, -37.61398439004513961, -29.98565522133333516 ) ) ;
#61219 = B_SPLINE_CURVE_WITH_KNOTS ( 'NONE', 3,
 ( #55487, #11139, #45825, #30223, #2562, #59889, #17003, #2869, #41434, #60491, #17607, #315, #19461, #57323, #4089, #38580 ),
 .UNSPECIFIED., .F., .F.,
 ( 4, 3, 3, 3, 3, 4 ),
 ( 1.250973872328959318E-17, 0.0002724568934985580949, 0.0004086836638483871400, 0.0005449104342063620671, 0.0008173270854453674322, 0.001089761613562689226 ),
 .UNSPECIFIED. ) ;
#61220 = CARTESIAN_POINT ( 'NONE',  ( 4.060580049360325461, -24.72948427782955250, -36.33070742102043482 ) ) ;
#61221 = CARTESIAN_POINT ( 'NONE',  ( 0.1081432562775997558, 42.69830087850304068, 6.048481838666182497 ) ) ;
#61222 = CONTEXT_DEPENDENT_SHAPE_REPRESENTATION ( #24844, #22295 ) ;
#61224 = ADVANCED_FACE ( 'NONE', ( #5695 ), #36454, .F. ) ;
#61223 = CARTESIAN_POINT ( 'NONE',  ( 0.8751705887134423323, -23.27176129838396790, -42.09020928323367627 ) ) ;
#61225 = CARTESIAN_POINT ( 'NONE',  ( 5.910764540655177868, -4.677486889029990991, 19.56073502893272220 ) ) ;
#61226 = EDGE_CURVE ( 'NONE', #28131, #39143, #19643, .T. ) ;
#61227 = CARTESIAN_POINT ( 'NONE',  ( -6.079354080745853928, 16.77867255551505110, -9.448232772480160691 ) ) ;
#61228 = EDGE_CURVE ( 'NONE', #9105, #17449, #27000, .T. ) ;
#61230 = ORIENTED_EDGE ( 'NONE', *, *, #1369, .F. ) ;
#61229 = CARTESIAN_POINT ( 'NONE',  ( 0.09136607875274982415, 0.000000000000000000, 43.12527911185304674 ) ) ;
#61231 = ORIENTED_EDGE ( 'NONE', *, *, #3725, .F. ) ;
#61232 = CARTESIAN_POINT ( 'NONE',  ( 0.1084644655670282398, -43.12277244437005663, 0.3976617192056919881 ) ) ;
#61233 = CARTESIAN_POINT ( 'NONE',  ( 0.5817216825391123836, -7.350843310970423872, 46.31630441674961673 ) ) ;
#61234 = EDGE_CURVE ( 'NONE', #1809, #29343, #23310, .T. ) ;
#61235 = CARTESIAN_POINT ( 'NONE',  ( -1.500000000000001332, 0.000000000000000000, 0.000000000000000000 ) ) ;
#61236 = EDGE_LOOP ( 'NONE', ( #10127, #16133, #50085, #45040 ) ) ;
#61237 = CARTESIAN_POINT ( 'NONE',  ( 0.6029443199889047422, 10.92740274660737221, -47.87618939585563993 ) ) ;
#61238 = CARTESIAN_POINT ( 'NONE',  ( 0.5830082357119567016, -46.00988774283680982, 9.073161787926713018 ) ) ;
#61239 = DIRECTION ( 'NONE',  ( -0.1011922191286467460, 0.9947837607124679904, 0.01286095682984216872 ) ) ;
#61240 = CIRCLE ( 'NONE', #14230, 42.92674063221959813 ) ;
#61241 = ORIENTED_EDGE ( 'NONE', *, *, #41401, .T. ) ;
#61242 = ORIENTED_EDGE ( 'NONE', *, *, #6944, .T. ) ;
#61243 = CARTESIAN_POINT ( 'NONE',  ( 0.9754402186311947887, 41.49454543482930546, 10.92425836141432960 ) ) ;
#61244 = CARTESIAN_POINT ( 'NONE',  ( 1.112077966505211624, -40.45272749787142175, 17.51020168677428046 ) ) ;
#61245 = CARTESIAN_POINT ( 'NONE',  ( 0.5549461598389369144, 37.43508315588892543, 23.32021107491279110 ) ) ;
#61246 = CARTESIAN_POINT ( 'NONE',  ( 0.5824936645240067490, 46.89462130976617971, 0.3642406538733899413 ) ) ;
#61247 = CARTESIAN_POINT ( 'NONE',  ( 0.8760168074887076939, -34.63873394077464951, -33.37827814204112542 ) ) ;
#61248 = CARTESIAN_POINT ( 'NONE',  ( 0.5998501479064708430, -23.59887241503325228, -41.92175333043611829 ) ) ;
#61249 = B_SPLINE_CURVE_WITH_KNOTS ( 'NONE', 3,
 ( #2537, #59861, #53598, #48925, #5974, #11333 ),
 .UNSPECIFIED., .F., .F.,
 ( 4, 2, 4 ),
 ( 8.471125239557413953E-17, 0.0002293366620881436295, 0.0004586733241762025828 ),
 .UNSPECIFIED. ) ;
#61250 = CARTESIAN_POINT ( 'NONE',  ( 5.838029081930957709, -10.96929503790485683, -45.94278642533902968 ) ) ;
#61251 = ORIENTED_EDGE ( 'NONE', *, *, #38166, .T. ) ;
#61252 = CARTESIAN_POINT ( 'NONE',  ( 0.9972139404380295780, 15.81078898082040674, -39.89035676513719153 ) ) ;
#61253 = ORIENTED_EDGE ( 'NONE', *, *, #23071, .F. ) ;
#61254 = CARTESIAN_POINT ( 'NONE',  ( 0.1147471544378676628, 41.77752542102519584, -14.19825898372188178 ) ) ;
#61255 = CARTESIAN_POINT ( 'NONE',  ( 4.291220156522060236, 20.72764654176005195, -42.30548033228744487 ) ) ;
#61256 = CARTESIAN_POINT ( 'NONE',  ( 2.009741617377216460, 39.06454069786799721, -20.33385693093319446 ) ) ;
#61257 = FACE_OUTER_BOUND ( 'NONE', #13835, .T. ) ;
#61258 = ORIENTED_EDGE ( 'NONE', *, *, #45187, .F. ) ;
#61259 = ORIENTED_EDGE ( 'NONE', *, *, #30179, .F. ) ;
#61260 = CARTESIAN_POINT ( 'NONE',  ( 0.9757954354143123510, 0.03224588977124673295, 42.90846090505963417 ) ) ;
#61261 = CARTESIAN_POINT ( 'NONE',  ( 0.6000166863083090663, -47.36892948402865500, -12.96179004788981182 ) ) ;
#61262 = CARTESIAN_POINT ( 'NONE',  ( 4.962356264823596597, -3.779019546647577776, 41.91604238389407300 ) ) ;
#61263 = EDGE_CURVE ( 'NONE', #39947, #4978, #40527, .T. ) ;
#61264 = EDGE_LOOP ( 'NONE', ( #25438, #56698, #31474, #48823 ) ) ;
#61265 = CARTESIAN_POINT ( 'NONE',  ( 4.975610109902397937, -40.67634447773618689, 27.16402781375239073 ) ) ;
#61266 = VERTEX_POINT ( 'NONE', #37044 ) ;
#61267 = CARTESIAN_POINT ( 'NONE',  ( 1.227938101723748288, -4.762198645644156514, -42.65467462194923343 ) ) ;
#61268 = CARTESIAN_POINT ( 'NONE',  ( 0.5806925824938499181, 27.37593026015182218, 38.07598724570208049 ) ) ;
#61269 =( BOUNDED_SURFACE ( )  B_SPLINE_SURFACE ( 3, 1, ( 
 ( #29505, #23575 ),
 ( #18900, #42700 ),
 ( #5668, #43956 ),
 ( #59548, #1595 ) ),
 .UNSPECIFIED., .F., .F., .F. ) 
 B_SPLINE_SURFACE_WITH_KNOTS ( ( 4, 4 ),
 ( 2, 2 ),
 ( 0.000000000000000000, 1.000000000000000000 ),
 ( 0.000000000000000000, 1.000000000000000000 ),
 .UNSPECIFIED. ) 
 GEOMETRIC_REPRESENTATION_ITEM ( )  RATIONAL_B_SPLINE_SURFACE ( (
 ( 1.000000000000000000, 1.000000000000000000),
 ( 0.9952954269826590483, 0.8620686068821339365),
 ( 0.9952954269826590483, 0.8620686068821339365),
 ( 1.000000000000000000, 1.000000000000000000) ) ) 
 REPRESENTATION_ITEM ( '' )  SURFACE ( )  );
#61270 = CARTESIAN_POINT ( 'NONE',  ( 0.1139756605157203756, 36.76166588342440633, -24.40358869450336599 ) ) ;
#61271 = EDGE_LOOP ( 'NONE', ( #11741, #41203, #2136, #27126 ) ) ;
#61272 = CARTESIAN_POINT ( 'NONE',  ( 0.5827357941260202789, -47.53228940613939812, -5.891356987508117982 ) ) ;
#61273 = CARTESIAN_POINT ( 'NONE',  ( 0.8753041380234530822, -49.09527960836077654, 0.8898584437169362316 ) ) ;
#61274 = CARTESIAN_POINT ( 'NONE',  ( 0.5834584762367738264, -41.93739078247706686, 20.98788325131905452 ) ) ;
#61275 = STYLED_ITEM ( 'NONE', ( #5895 ), #31244 ) ;
#61276 = VERTEX_POINT ( 'NONE', #46742 ) ;
#61277 = CARTESIAN_POINT ( 'NONE',  ( 0.6031356219577718170, -29.35521383643431292, -38.11305734842053283 ) ) ;
#61278 = CIRCLE ( 'NONE', #7252, 75.00000000000001421 ) ;
#61279 = CARTESIAN_POINT ( 'NONE',  ( -5.440000000000003944, 15.43999999999999950, 0.000000000000000000 ) ) ;
#61280 = CARTESIAN_POINT ( 'NONE',  ( 5.901463166500145796, 10.81005692193063261, 16.96055835417148927 ) ) ;
#61281 = CARTESIAN_POINT ( 'NONE',  ( 0.6031356219577718170, 47.68448279784254851, -6.365832241666079305 ) ) ;
#61282 = CARTESIAN_POINT ( 'NONE',  ( 0.2940133293163017525, -38.82777377762746340, 20.94384236598979143 ) ) ;
#61283 = ORIENTED_EDGE ( 'NONE', *, *, #40269, .T. ) ;
#61284 = DIRECTION ( 'NONE',  ( 0.1024043820194936449, -0.5087173657443522234, -0.8548216096550979026 ) ) ;
#61285 = CARTESIAN_POINT ( 'NONE',  ( -5.331200000000000827, 15.38218000000000174, 0.000000000000000000 ) ) ;
#61286 = ORIENTED_EDGE ( 'NONE', *, *, #16211, .T. ) ;
#61288 = CARTESIAN_POINT ( 'NONE',  ( 5.896782393890504181, 10.82771479451271368, 16.94953330350728748 ) ) ;
#61287 =( BOUNDED_SURFACE ( )  B_SPLINE_SURFACE ( 3, 1, ( 
 ( #27454, #61261 ),
 ( #8645, #22760 ),
 ( #14001, #41894 ),
 ( #33104, #9270 ) ),
 .UNSPECIFIED., .F., .F., .F. ) 
 B_SPLINE_SURFACE_WITH_KNOTS ( ( 4, 4 ),
 ( 2, 2 ),
 ( 0.000000000000000000, 1.000000000000000000 ),
 ( 0.000000000000000000, 1.000000000000000000 ),
 .UNSPECIFIED. ) 
 GEOMETRIC_REPRESENTATION_ITEM ( )  RATIONAL_B_SPLINE_SURFACE ( (
 ( 1.000000000000000000, 1.000000000000000000),
 ( 0.9953485035131437453, 0.8621029689291523912),
 ( 0.9953485035131437453, 0.8621029689291523912),
 ( 1.000000000000000000, 1.000000000000000000) ) ) 
 REPRESENTATION_ITEM ( '' )  SURFACE ( )  );
#61289 = CARTESIAN_POINT ( 'NONE',  ( 0.9788927965476030835, -26.94903577592939925, 32.09495417319448762 ) ) ;
#61290 = ADVANCED_FACE ( 'NONE', ( #8487 ), #36732, .F. ) ;
#61291 = FACE_OUTER_BOUND ( 'NONE', #40359, .T. ) ;
#61292 = CARTESIAN_POINT ( 'NONE',  ( 5.894904586330512508, -17.30455939762474671, 10.25093342655779338 ) ) ;
#61293 = CARTESIAN_POINT ( 'NONE',  ( 0.8751705887134423323, 37.60752970653787486, 29.98056538504974000 ) ) ;
#61294 = CYLINDRICAL_SURFACE ( 'NONE', #29062, 15.14599999999999369 ) ;
#61295 = CARTESIAN_POINT ( 'NONE',  ( 0.5809828226811553087, -47.89273459658654275, 0.5448590168530708100 ) ) ;
#61296 = CARTESIAN_POINT ( 'NONE',  ( 0.000000000000000000, 0.000000000000000000, 0.000000000000000000 ) ) ;
#61298 = EDGE_CURVE ( 'NONE', #49156, #52762, #60190, .T. ) ;
#61297 = CARTESIAN_POINT ( 'NONE',  ( 0.6025881611877910160, 47.66695236827166582, 6.495537368246036003 ) ) ;
#61299 = AXIS2_PLACEMENT_3D ( 'NONE', #12895, #55769, #17580 ) ;
#61300 = CARTESIAN_POINT ( 'NONE',  ( -6.078457390727109555, 12.00936083188108583, -15.05223450013945019 ) ) ;
#61301 = CARTESIAN_POINT ( 'NONE',  ( 1.114300000000000068, 0.000000000000000000, -6.866799999999992465 ) ) ;
#61302 = EDGE_CURVE ( 'NONE', #593, #29811, #51695, .T. ) ;
#61303 = CARTESIAN_POINT ( 'NONE',  ( -6.016761891674565099, -9.424569481870369358, 16.31696541414269319 ) ) ;
#61304 = ORIENTED_EDGE ( 'NONE', *, *, #47827, .T. ) ;
#61305 = CARTESIAN_POINT ( 'NONE',  ( 0.8551540677456715978, -44.61036085020937492, -17.49081417858833731 ) ) ;
#61306 = ADVANCED_FACE ( 'NONE', ( #7883 ), #7620, .T. ) ;
#61307 = CARTESIAN_POINT ( 'NONE',  ( 0.8554163680231708922, 46.61139063278411498, -5.346376005279187993 ) ) ;
#61308 = CARTESIAN_POINT ( 'NONE',  ( 1.231276596079881047, -21.83837404314779462, -35.78214904347746739 ) ) ;
#61309 = CARTESIAN_POINT ( 'NONE',  ( 4.962356264823603702, 0.9708976703223142213, -42.07484944210863631 ) ) ;
#61310 = CARTESIAN_POINT ( 'NONE',  ( 3.559346040607745287, 32.11337397044390940, -30.03600329232243027 ) ) ;
#61311 = B_SPLINE_CURVE_WITH_KNOTS ( 'NONE', 3,
 ( #18466, #37594, #53198, #53495 ),
 .UNSPECIFIED., .F., .F.,
 ( 4, 4 ),
 ( 0.000000000000000000, 0.002405070305343063371 ),
 .UNSPECIFIED. ) ;
#61312 = ORIENTED_EDGE ( 'NONE', *, *, #37934, .F. ) ;
#61313 = CARTESIAN_POINT ( 'NONE',  ( 3.238741278300273141, -12.88350628398768905, 41.01623499585991794 ) ) ;
#61314 = EDGE_CURVE ( 'NONE', #33419, #32395, #32690, .T. ) ;
#61315 = DIRECTION ( 'NONE',  ( -1.000000000000000000, -0.000000000000000000, -0.000000000000000000 ) ) ;
#61316 = CARTESIAN_POINT ( 'NONE',  ( -19.55483905134862965, -7.879146627487763510, -1.388794482494389637 ) ) ;
#61317 = VERTEX_POINT ( 'NONE', #26376 ) ;
#61318 = EDGE_CURVE ( 'NONE', #33684, #4545, #9093, .T. ) ;
#61319 = CARTESIAN_POINT ( 'NONE',  ( -6.015611763856276717, -4.870987357968047604, -18.20278301740941629 ) ) ;
#61320 = CIRCLE ( 'NONE', #7296, 12.49999999999999822 ) ;
#61321 = CARTESIAN_POINT ( 'NONE',  ( 3.783198216974389627, 42.86118135813612184, -3.901161703631621958 ) ) ;
#61322 = ORIENTED_EDGE ( 'NONE', *, *, #31604, .T. ) ;
#61323 = ORIENTED_EDGE ( 'NONE', *, *, #59250, .F. ) ;
#61324 = CARTESIAN_POINT ( 'NONE',  ( 2.648799415243696664, -29.47778256948665998, -39.18644916390953625 ) ) ;
#61325 = CARTESIAN_POINT ( 'NONE',  ( 3.238741278300274029, -42.95313747363663026, -1.828728677531676228 ) ) ;
#61326 = ORIENTED_EDGE ( 'NONE', *, *, #3237, .T. ) ;
#61327 = CARTESIAN_POINT ( 'NONE',  ( 4.962356264823602814, -29.56943756613081931, -29.94802096775409339 ) ) ;
#61328 = CARTESIAN_POINT ( 'NONE',  ( 0.5809828226811617480, -29.58751527316205809, 37.66417181417541826 ) ) ;
#61329 = ORIENTED_EDGE ( 'NONE', *, *, #27858, .T. ) ;
#61330 = CARTESIAN_POINT ( 'NONE',  ( 0.5830081025819929819, -8.069435828662605559, -46.19649596873491504 ) ) ;
#61331 = CARTESIAN_POINT ( 'NONE',  ( 4.967162193818130511, 7.970725651240403664, -42.34252806656584056 ) ) ;
#61332 = VECTOR ( 'NONE', #45250, 1000.000000000000000 ) ;
#61333 = EDGE_LOOP ( 'NONE', ( #60949, #51090, #56568, #36497 ) ) ;
#61334 = ORIENTED_EDGE ( 'NONE', *, *, #35820, .F. ) ;
#61335 = CARTESIAN_POINT ( 'NONE',  ( 5.960721111146673579, 12.50019045452738276, -16.28018152803680252 ) ) ;
#61336 = ADVANCED_FACE ( 'NONE', ( #22304 ), #57996, .F. ) ;
#61337 = ORIENTED_EDGE ( 'NONE', *, *, #23064, .T. ) ;
#61338 = ORIENTED_EDGE ( 'NONE', *, *, #49706, .T. ) ;
#61339 = DIRECTION ( 'NONE',  ( -1.000000000000000000, -0.000000000000000000, -0.000000000000000000 ) ) ;
#61340 = CARTESIAN_POINT ( 'NONE',  ( 5.959547316686252039, -18.96183906913549322, 7.858107265727412027 ) ) ;
#61341 = CARTESIAN_POINT ( 'NONE',  ( 0.9758171775293921213, 34.04519363167634793, 26.11633498242636264 ) ) ;
#61342 = CARTESIAN_POINT ( 'NONE',  ( 3.221118495291108275, -28.87617019281731245, -33.18023831525626832 ) ) ;
#61343 = EDGE_LOOP ( 'NONE', ( #11467, #10610, #60462, #44291 ) ) ;
#61344 = DIRECTION ( 'NONE',  ( 1.000000000000000000, 0.000000000000000000, 0.000000000000000000 ) ) ;
#61345 = CARTESIAN_POINT ( 'NONE',  ( -6.077587904424778920, -18.89978312007036720, 3.687033958106935128 ) ) ;
#61346 = ORIENTED_EDGE ( 'NONE', *, *, #27598, .T. ) ;
#61347 = B_SPLINE_CURVE_WITH_KNOTS ( 'NONE', 3,
 ( #4376, #23514, #61703, #61097 ),
 .UNSPECIFIED., .F., .F.,
 ( 4, 4 ),
 ( 0.000000000000000000, 0.004446090762761357312 ),
 .UNSPECIFIED. ) ;
#61348 = ORIENTED_EDGE ( 'NONE', *, *, #55727, .F. ) ;
#61349 = CARTESIAN_POINT ( 'NONE',  ( 0.8744876279028263033, -49.08725279547490317, -0.8897546699139439186 ) ) ;
#61350 = CARTESIAN_POINT ( 'NONE',  ( 2.648799415243696664, 15.62808678998912448, 46.47881632070856739 ) ) ;
#61351 = LINE ( 'NONE', #23779, #8947 ) ;
#61352 = CARTESIAN_POINT ( 'NONE',  ( -15.25000000000000711, -2.688986455804108555, -9.952330921218299798E-16 ) ) ;
#61353 = CARTESIAN_POINT ( 'NONE',  ( -2.601141883200665639, -9.652501068366241554, 11.38528219213635317 ) ) ;
#61354 = B_SPLINE_CURVE_WITH_KNOTS ( 'NONE', 3,
 ( #588, #16251, #34140, #25642, #6500, #5583, #20339, #44479, #20641, #48228, #24723, #19723, #35376, #1823, #11244, #39778, #20952, #5281, #34750 ),
 .UNSPECIFIED., .F., .F.,
 ( 4, 3, 3, 3, 3, 3, 4 ),
 ( 0.000000000000000000, 0.0002612768053151720343, 0.0003919133833142896244, 0.0005225499612322636808, 0.0006531865391693353080, 0.0008112755173415234352, 0.0009693688056799755004 ),
 .UNSPECIFIED. ) ;
#61355 = ORIENTED_EDGE ( 'NONE', *, *, #53770, .F. ) ;
#61356 = CARTESIAN_POINT ( 'NONE',  ( 4.975610109902397937, -46.59897809419055648, 14.86555238512586463 ) ) ;
#61357 = CARTESIAN_POINT ( 'NONE',  ( 50.32685901376226667, 15.27178771460631168, 2.649999999999992806 ) ) ;
#61358 = CARTESIAN_POINT ( 'NONE',  ( 4.549368137175248350, 35.80950303116068056, 23.67244292351653101 ) ) ;
#61359 = B_SPLINE_CURVE_WITH_KNOTS ( 'NONE', 3,
 ( #2289, #21418, #17342, #8230 ),
 .UNSPECIFIED., .F., .F.,
 ( 4, 4 ),
 ( 0.000000000000000000, 0.005004741218457423209 ),
 .UNSPECIFIED. ) ;
#61360 = VECTOR ( 'NONE', #31169, 1000.000000000000000 ) ;
#61361 = CARTESIAN_POINT ( 'NONE',  ( 1.112077966505211402, -41.24073227881319781, -15.56381464281200877 ) ) ;
#61362 =( NAMED_UNIT ( * ) PLANE_ANGLE_UNIT ( ) SI_UNIT ( $, .RADIAN. ) );
#61363 = CARTESIAN_POINT ( 'NONE',  ( 0.8551540677456739292, -44.61036085020961650, 17.49081417858772269 ) ) ;
#61364 =( BOUNDED_SURFACE ( )  B_SPLINE_SURFACE ( 3, 1, ( 
 ( #27856, #31948 ),
 ( #36978, #31633 ),
 ( #7812, #56039 ),
 ( #51032, #13158 ) ),
 .UNSPECIFIED., .F., .F., .F. ) 
 B_SPLINE_SURFACE_WITH_KNOTS ( ( 4, 4 ),
 ( 2, 2 ),
 ( 0.000000000000000000, 1.000000000000000000 ),
 ( 0.000000000000000000, 1.000000000000000000 ),
 .UNSPECIFIED. ) 
 GEOMETRIC_REPRESENTATION_ITEM ( )  RATIONAL_B_SPLINE_SURFACE ( (
 ( 1.000000000000000000, 1.000000000000000000),
 ( 0.9729067724841187204, 0.9999501103223794596),
 ( 0.9729067724841187204, 0.9999501103223794596),
 ( 1.000000000000000000, 1.000000000000000000) ) ) 
 REPRESENTATION_ITEM ( '' )  SURFACE ( )  );
#61365 = ORIENTED_EDGE ( 'NONE', *, *, #21746, .T. ) ;
#61366 = CARTESIAN_POINT ( 'NONE',  ( 0.1064266418746776799, 34.55203617814591155, -25.80493189480195326 ) ) ;
#61367 = CARTESIAN_POINT ( 'NONE',  ( -6.063463321072276813, -18.27076090991278434, 6.082741836727326934 ) ) ;
#61368 = ADVANCED_FACE ( 'NONE', ( #18528 ), #14862, .F. ) ;
#61369 = CARTESIAN_POINT ( 'NONE',  ( 4.962356264823603702, 12.05238263218972072, -40.32338863178092225 ) ) ;
#61370 = CARTESIAN_POINT ( 'NONE',  ( -0.5999999999999992006, -11.64055411052240352, -1.199999999999999956 ) ) ;
#61371 = CARTESIAN_POINT ( 'NONE',  ( 0.9787284016396619046, 29.26888682565846977, 29.99447053901143079 ) ) ;
#61372 = EDGE_CURVE ( 'NONE', #61502, #40551, #33260, .T. ) ;
#61373 = CARTESIAN_POINT ( 'NONE',  ( 3.680882792899938583, -43.58303137875421385, 20.05474345988731955 ) ) ;
#61374 = CARTESIAN_POINT ( 'NONE',  ( 0.5997462898726536595, -49.10477184366966696, 0.5225058138009974762 ) ) ;
#61375 = VECTOR ( 'NONE', #18001, 1000.000000000000227 ) ;
#61376 = CARTESIAN_POINT ( 'NONE',  ( 2.281448460670572054, -1.314143534315570072, -47.95523685111405143 ) ) ;
#61377 = FACE_OUTER_BOUND ( 'NONE', #9274, .T. ) ;
#61378 = VERTEX_POINT ( 'NONE', #51718 ) ;
#61379 = CARTESIAN_POINT ( 'NONE',  ( -6.072942160501519915, 19.25627044167811874, -0.01452466776898916206 ) ) ;
#61380 = CARTESIAN_POINT ( 'NONE',  ( 4.975610109902397937, -48.11736577406863802, 8.784561349450592971 ) ) ;
#61381 = CARTESIAN_POINT ( 'NONE',  ( 0.9762797500689124330, 38.38274741215467145, 16.82526333465357382 ) ) ;
#61382 = CARTESIAN_POINT ( 'NONE',  ( -6.016104459813374383, 16.32137543786095790, -9.416989654584133618 ) ) ;
#61383 = VERTEX_POINT ( 'NONE', #23226 ) ;
#61384 = EDGE_CURVE ( 'NONE', #9740, #1744, #27079, .T. ) ;
#61385 = CARTESIAN_POINT ( 'NONE',  ( 0.7762783648524379521, 46.03397615175201452, -13.25585403815072105 ) ) ;
#61386 = CARTESIAN_POINT ( 'NONE',  ( 0.8560838555295223751, 27.08392101972057731, -38.29926965725677235 ) ) ;
#61387 = DIRECTION ( 'NONE',  ( 0.000000000000000000, 0.000000000000000000, 1.000000000000000000 ) ) ;
#61388 = ORIENTED_EDGE ( 'NONE', *, *, #59210, .T. ) ;
#61389 = CARTESIAN_POINT ( 'NONE',  ( 5.860006189529246790, 45.67886430272052678, -15.48781697582000483 ) ) ;
#61390 = CARTESIAN_POINT ( 'NONE',  ( 0.7048096507298635682, -47.80151517212783574, -5.442192462019296073 ) ) ;
#61391 = CARTESIAN_POINT ( 'NONE',  ( 4.956653778116988818, -45.71126949320240840, -14.93973939759935021 ) ) ;
#61392 = ORIENTED_EDGE ( 'NONE', *, *, #50777, .T. ) ;
#61393 = LINE ( 'NONE', #22597, #17843 ) ;
#61394 = VERTEX_POINT ( 'NONE', #4698 ) ;
#61395 = ORIENTED_EDGE ( 'NONE', *, *, #50707, .F. ) ;
#61396 = CARTESIAN_POINT ( 'NONE',  ( 5.895596859100789899, 8.469463536103054579, -18.24270732712412624 ) ) ;
#61397 = LINE ( 'NONE', #42041, #30475 ) ;
#61398 = EDGE_LOOP ( 'NONE', ( #43399, #46668, #12455, #34845 ) ) ;
#61399 = CARTESIAN_POINT ( 'NONE',  ( -14.84250595937556483, -4.999999999999993783, 6.123233995736803753E-16 ) ) ;
#61400 = VECTOR ( 'NONE', #44551, 1000.000000000000114 ) ;
#61401 = ORIENTED_EDGE ( 'NONE', *, *, #30182, .F. ) ;
#61402 = CARTESIAN_POINT ( 'NONE',  ( 5.960721111146673579, 16.28018152803692686, -12.50019045452721222 ) ) ;
#61403 = CARTESIAN_POINT ( 'NONE',  ( 0.8551540677456739292, -37.45266983663475457, -29.88829867897852921 ) ) ;
#61404 = ORIENTED_EDGE ( 'NONE', *, *, #2763, .F. ) ;
#61405 = CARTESIAN_POINT ( 'NONE',  ( 0.5997462898726536595, 37.05192695178169515, -32.22896739432000146 ) ) ;
#61406 = CARTESIAN_POINT ( 'NONE',  ( 0.6039202388192953519, 37.50551550546074253, 31.70015803617760852 ) ) ;
#61407 = CARTESIAN_POINT ( 'NONE',  ( 5.860006189529234355, -9.393028332205062725, 47.30964106197854591 ) ) ;
#61408 = CARTESIAN_POINT ( 'NONE',  ( 0.7948878604505662526, 27.37440007400915576, -40.75954940730458276 ) ) ;
#61409 = ORIENTED_EDGE ( 'NONE', *, *, #16204, .F. ) ;
#61410 = CARTESIAN_POINT ( 'NONE',  ( 0.5836750258453350382, -33.73891062492380399, -33.99574025613945594 ) ) ;
#61411 = CARTESIAN_POINT ( 'NONE',  ( 0.1158516988532803382, -31.73079332305263378, -30.66103249928995922 ) ) ;
#61412 = VECTOR ( 'NONE', #27941, 1000.000000000000114 ) ;
#61413 = VERTEX_POINT ( 'NONE', #24451 ) ;
#61414 = CARTESIAN_POINT ( 'NONE',  ( 0.5837157313716018203, 43.21027797204915544, -18.22385637455116481 ) ) ;
#61415 = EDGE_CURVE ( 'NONE', #57030, #34351, #15888, .T. ) ;
#61416 = ORIENTED_EDGE ( 'NONE', *, *, #24626, .T. ) ;
#61417 = CARTESIAN_POINT ( 'NONE',  ( 2.526552050251864578, 12.29062829844035498, -41.18423939305552040 ) ) ;
#61418 = CARTESIAN_POINT ( 'NONE',  ( 0.6026112563231247332, 46.66028695286041739, -15.30877579628533702 ) ) ;
#61419 = ORIENTED_EDGE ( 'NONE', *, *, #12175, .F. ) ;
#61420 = CARTESIAN_POINT ( 'NONE',  ( 0.9784957157296378938, -34.68241884430302235, -23.52579180603076736 ) ) ;
#61421 = FACE_OUTER_BOUND ( 'NONE', #60127, .T. ) ;
#61422 = EDGE_CURVE ( 'NONE', #42948, #59492, #28224, .T. ) ;
#61423 = DIRECTION ( 'NONE',  ( 0.000000000000000000, 0.000000000000000000, 1.000000000000000000 ) ) ;
#61424 = ORIENTED_EDGE ( 'NONE', *, *, #52111, .T. ) ;
#61425 = CARTESIAN_POINT ( 'NONE',  ( 0.6064782688330875304, 45.03780212049427689, 13.07405165103655165 ) ) ;
#61426 = CARTESIAN_POINT ( 'NONE',  ( 0.6846871229502899947, 38.52803883689301756, 28.47437962186140226 ) ) ;
#61427 = FACE_OUTER_BOUND ( 'NONE', #29045, .T. ) ;
#61428 = CARTESIAN_POINT ( 'NONE',  ( 3.680882792899937250, -20.05474345988779561, -43.58303137875400068 ) ) ;
#61429 = DIRECTION ( 'NONE',  ( 0.9914448613738107152, -0.1305261922200498526, 0.000000000000000000 ) ) ;
#61430 = CARTESIAN_POINT ( 'NONE',  ( 3.782625744892853525, -41.50499360117703418, -6.676347074655189395 ) ) ;
#61431 = CARTESIAN_POINT ( 'NONE',  ( 0.5839879882012696255, -46.26394433311389065, 12.39641777360504449 ) ) ;
#61432 = EDGE_CURVE ( 'NONE', #61929, #24638, #38309, .T. ) ;
#61433 = CARTESIAN_POINT ( 'NONE',  ( 0.000000000000000000, 0.000000000000000000, -1.199999999999999956 ) ) ;
#61434 = CARTESIAN_POINT ( 'NONE',  ( 0.8744876279028306332, 21.91587810745098963, -43.93226988397984911 ) ) ;
#61435 = EDGE_CURVE ( 'NONE', #57834, #52026, #60679, .T. ) ;
#61436 = CARTESIAN_POINT ( 'NONE',  ( 0.1073791018717483448, -37.10214135362904386, 21.98088480513601795 ) ) ;
#61437 = CARTESIAN_POINT ( 'NONE',  ( 0.8753041380234524160, -13.11588273819849526, 47.31925557181565267 ) ) ;
#61438 = DIRECTION ( 'NONE',  ( 0.000000000000000000, 1.000000000000000000, -1.287488025362403787E-15 ) ) ;
#61439 = CARTESIAN_POINT ( 'NONE',  ( 7.999999999999996447, 1.469527624586858429E-15, -1.540743955509788245E-31 ) ) ;
#61440 = CARTESIAN_POINT ( 'NONE',  ( 4.962356264823598373, -24.61258717641114657, 34.13877780978559429 ) ) ;
#61441 = CARTESIAN_POINT ( 'NONE',  ( 4.226256110419179812, -20.68992697050140350, 38.76537336260938815 ) ) ;
#61442 = ADVANCED_FACE ( 'NONE', ( #59190 ), #4025, .F. ) ;
#61443 = B_SPLINE_CURVE_WITH_KNOTS ( 'NONE', 3,
 ( #50624, #7714, #55627, #60632, #22445, #17751 ),
 .UNSPECIFIED., .F., .F.,
 ( 4, 2, 4 ),
 ( 8.542799345870747147E-17, 0.0002293366620881467195, 0.0004586733241762080038 ),
 .UNSPECIFIED. ) ;
#61444 = CARTESIAN_POINT ( 'NONE',  ( 0.5786265663353153954, 34.37803667029811550, 33.35675271369551353 ) ) ;
#61445 = VECTOR ( 'NONE', #8184, 1000.000000000000114 ) ;
#61446 = CARTESIAN_POINT ( 'NONE',  ( 0.5797568599927148680, -13.29195561999140018, -44.97276091666135756 ) ) ;
#61447 = CARTESIAN_POINT ( 'NONE',  ( 0.9730545539215883499, 34.34678117142556175, 25.71816799638790840 ) ) ;
#61449 = ORIENTED_EDGE ( 'NONE', *, *, #16443, .T. ) ;
#61448 = CARTESIAN_POINT ( 'NONE',  ( 0.9757892942422831117, 39.66188497122492151, 16.37293303864320038 ) ) ;
#61450 = CARTESIAN_POINT ( 'NONE',  ( 4.553261556744875094, 0.000000000000000000, 0.000000000000000000 ) ) ;
#61451 = FACE_OUTER_BOUND ( 'NONE', #7746, .T. ) ;
#61452 = DIRECTION ( 'NONE',  ( 0.000000000000000000, 1.000000000000000000, 0.000000000000000000 ) ) ;
#61453 = EDGE_LOOP ( 'NONE', ( #11326, #43505, #49705, #61638 ) ) ;
#61454 = EDGE_CURVE ( 'NONE', #41141, #12584, #32299, .T. ) ;
#61455 = ORIENTED_EDGE ( 'NONE', *, *, #30779, .T. ) ;
#61456 = CARTESIAN_POINT ( 'NONE',  ( 0.5827359174754810356, -34.12345922495634909, 33.60976280407636807 ) ) ;
#61457 = AXIS2_PLACEMENT_3D ( 'NONE', #33166, #52552, #9648 ) ;
#61458 = CARTESIAN_POINT ( 'NONE',  ( 0.3676999524040323597, 43.13409918076290950, 9.241215893319909114 ) ) ;
#61459 = EDGE_LOOP ( 'NONE', ( #17151, #20896, #35426, #36347 ) ) ;
#61460 = EDGE_LOOP ( 'NONE', ( #45838, #13352, #3692, #16537 ) ) ;
#61461 = CARTESIAN_POINT ( 'NONE',  ( 0.9756950546413923897, -11.19893879603418974, -41.42124338356090618 ) ) ;
#61462 = ORIENTED_EDGE ( 'NONE', *, *, #4409, .F. ) ;
#61463 = CARTESIAN_POINT ( 'NONE',  ( 4.962356264823608143, 17.31942680647409460, 38.35717733303029320 ) ) ;
#61464 = DIRECTION ( 'NONE',  ( 0.09722883295013594329, 0.5755877901554883325, 0.8119391909909733362 ) ) ;
#61465 = B_SPLINE_CURVE_WITH_KNOTS ( 'NONE', 3,
 ( #54503, #11631, #34206, #34827, #54193, #5954 ),
 .UNSPECIFIED., .F., .F.,
 ( 4, 2, 4 ),
 ( 0.000000000000000000, 0.0002291966416970797290, 0.0004583932833941594580 ),
 .UNSPECIFIED. ) ;
#61466 = VERTEX_POINT ( 'NONE', #20083 ) ;
#61467 = VERTEX_POINT ( 'NONE', #49807 ) ;
#61468 = DIRECTION ( 'NONE',  ( 0.000000000000000000, 0.000000000000000000, -1.000000000000000000 ) ) ;
#61469 = EDGE_LOOP ( 'NONE', ( #11297, #7941, #57686, #31246, #19756, #40816 ) ) ;
#61470 = CARTESIAN_POINT ( 'NONE',  ( 4.834790513006553603, 24.09885983197524340, 40.64276437108075868 ) ) ;
#61471 = CARTESIAN_POINT ( 'NONE',  ( 4.322998006666165516, -27.50295597456424446, -39.32552843303840717 ) ) ;
#61472 = CARTESIAN_POINT ( 'NONE',  ( 0.8557997880470697982, -46.03118133706034598, 13.27832040216623355 ) ) ;
#61473 = VERTEX_POINT ( 'NONE', #53258 ) ;
#61474 = B_SPLINE_CURVE_WITH_KNOTS ( 'NONE', 3,
 ( #60227, #6978, #59000, #36154 ),
 .UNSPECIFIED., .F., .F.,
 ( 4, 4 ),
 ( 0.000000000000000000, 0.004446090762761366853 ),
 .UNSPECIFIED. ) ;
#61475 = AXIS2_PLACEMENT_3D ( 'NONE', #26410, #6971, #26106 ) ;
#61476 =( BOUNDED_SURFACE ( )  B_SPLINE_SURFACE ( 3, 1, ( 
 ( #36633, #45728 ),
 ( #7790, #46343 ),
 ( #56019, #31925 ),
 ( #8719, #42269 ) ),
 .UNSPECIFIED., .F., .F., .F. ) 
 B_SPLINE_SURFACE_WITH_KNOTS ( ( 4, 4 ),
 ( 2, 2 ),
 ( 0.000000000000000000, 1.000000000000000000 ),
 ( 0.000000000000000000, 1.000000000000000000 ),
 .UNSPECIFIED. ) 
 GEOMETRIC_REPRESENTATION_ITEM ( )  RATIONAL_B_SPLINE_SURFACE ( (
 ( 1.000000000000000000, 1.000000000000000000),
 ( 0.7211978278499968642, 0.9934217856018975334),
 ( 0.7211978278499968642, 0.9934217856018975334),
 ( 1.000000000000000000, 1.000000000000000000) ) ) 
 REPRESENTATION_ITEM ( '' )  SURFACE ( )  );
#61477 = CARTESIAN_POINT ( 'NONE',  ( 0.9787284016396609054, -39.52800361071009405, 13.92382596417090390 ) ) ;
#61478 = EDGE_LOOP ( 'NONE', ( #39344, #4554, #61462, #29575 ) ) ;
#61479 = VERTEX_POINT ( 'NONE', #25072 ) ;
#61480 = EDGE_CURVE ( 'NONE', #19687, #39282, #39200, .T. ) ;
#61481 = CARTESIAN_POINT ( 'NONE',  ( -6.016761891674564211, 14.94721834528430371, -11.47373234755488092 ) ) ;
#61482 = ORIENTED_EDGE ( 'NONE', *, *, #39328, .T. ) ;
#61483 = CARTESIAN_POINT ( 'NONE',  ( 5.880360259849739535, -45.41096578730658706, 15.46489389606675147 ) ) ;
#61484 = CARTESIAN_POINT ( 'NONE',  ( -6.078726893082806448, -14.66462719274100479, -12.47969352855434444 ) ) ;
#61485 = CARTESIAN_POINT ( 'NONE',  ( 0.9757954354143116849, 5.207268878499845415E-15, 42.90846090505964128 ) ) ;
#61486 = FACE_OUTER_BOUND ( 'NONE', #61236, .T. ) ;
#61487 = LINE ( 'NONE', #7963, #4349 ) ;
#61488 = ADVANCED_FACE ( 'NONE', ( #10673 ), #21257, .F. ) ;
#61489 = ORIENTED_EDGE ( 'NONE', *, *, #25114, .T. ) ;
#61490 = CARTESIAN_POINT ( 'NONE',  ( 1.157644175074337811, 32.37803412471593134, 26.62076598631064783 ) ) ;
#61491 = EDGE_CURVE ( 'NONE', #54789, #46497, #46507, .T. ) ;
#61492 = DIRECTION ( 'NONE',  ( -1.000000000000000000, -0.000000000000000000, -0.000000000000000000 ) ) ;
#61493 = B_SPLINE_CURVE_WITH_KNOTS ( 'NONE', 3,
 ( #11317, #35449, #11634, #30719 ),
 .UNSPECIFIED., .F., .F.,
 ( 4, 4 ),
 ( 0.000000000000000000, 0.004447772540403806783 ),
 .UNSPECIFIED. ) ;
#61494 = MECHANICAL_DESIGN_GEOMETRIC_PRESENTATION_REPRESENTATION (  '', ( #48506 ), #36545 ) ;
#61495 = VERTEX_POINT ( 'NONE', #5622 ) ;
#61496 = LINE ( 'NONE', #37748, #55517 ) ;
#61497 = EDGE_CURVE ( 'NONE', #46812, #2175, #21087, .T. ) ;
#61498 = CARTESIAN_POINT ( 'NONE',  ( -6.077587904424778920, 12.01079512011154193, -15.05114022181160927 ) ) ;
#61499 = CARTESIAN_POINT ( 'NONE',  ( 3.894904216938897878, -4.810386045490164797, 43.69192738446720625 ) ) ;
#61501 = ORIENTED_EDGE ( 'NONE', *, *, #61497, .T. ) ;
#61500 = AXIS2_PLACEMENT_3D ( 'NONE', #58070, #15191, #53372 ) ;
#61502 = VERTEX_POINT ( 'NONE', #29456 ) ;
#61503 = DIRECTION ( 'NONE',  ( 1.000000000000000000, 0.000000000000000000, 0.000000000000000000 ) ) ;
#61504 = CARTESIAN_POINT ( 'NONE',  ( 0.1087620492084205026, -42.80136086877936918, 5.269740196867194193 ) ) ;
#61505 = DIRECTION ( 'NONE',  ( 0.1011922191286467876, 0.1083236746283898905, 0.9889520293233755588 ) ) ;
#61506 = AXIS2_PLACEMENT_3D ( 'NONE', #14066, #42569, #19076 ) ;
#61507 = LINE ( 'NONE', #37757, #57782 ) ;
#61508 = CARTESIAN_POINT ( 'NONE',  ( 0.8560838555295158248, -24.46533024579895610, -40.02274915652004239 ) ) ;
#61509 = CARTESIAN_POINT ( 'NONE',  ( 0.1135584504625008206, -17.46491369724040865, -40.52072113972302958 ) ) ;
#61510 = CARTESIAN_POINT ( 'NONE',  ( 3.238741278300274029, -32.96375560769479307, -27.59904135366523548 ) ) ;
#61511 = CARTESIAN_POINT ( 'NONE',  ( 0.7057020205115021039, 47.59410670607645955, -5.417413437617099703 ) ) ;
#61512 = CARTESIAN_POINT ( 'NONE',  ( -6.078726893082806448, -17.34758611459996303, -8.357948149232475643 ) ) ;
#61513 = CARTESIAN_POINT ( 'NONE',  ( 5.917102823773431552, -17.30871814525818664, 10.24197218409383581 ) ) ;
#61514 = ADVANCED_FACE ( 'NONE', ( #44831 ), #6027, .F. ) ;
#61515 = CARTESIAN_POINT ( 'NONE',  ( 0.9787464366903563251, -1.223426366651767072, -41.89077727633904402 ) ) ;
#61516 = DIRECTION ( 'NONE',  ( 0.000000000000000000, -0.7071067811865553443, 0.7071067811865395791 ) ) ;
#61517 = ORIENTED_EDGE ( 'NONE', *, *, #59660, .F. ) ;
#61518 = EDGE_CURVE ( 'NONE', #4313, #17449, #18103, .T. ) ;
#61519 = CARTESIAN_POINT ( 'NONE',  ( 0.6001305935487422083, -6.798494447612560165, 47.62765676940932025 ) ) ;
#61520 = CARTESIAN_POINT ( 'NONE',  ( 0.1081432562775997835, -33.95357233988211476, -26.58728936586504688 ) ) ;
#61521 = CARTESIAN_POINT ( 'NONE',  ( 0.1152339509894530906, -35.49488302199451795, -26.21175251123374750 ) ) ;
#61522 = CARTESIAN_POINT ( 'NONE',  ( 0.6021448801613057400, -39.19856320471260602, -29.58063186128886457 ) ) ;
#61523 = CARTESIAN_POINT ( 'NONE',  ( 3.680974057930773924, 44.99871514631792024, -16.63696281867813909 ) ) ;
#61524 = CARTESIAN_POINT ( 'NONE',  ( 0.5786265663353196143, 0.7221568112313164756, -47.89572889566445468 ) ) ;
#61525 = CARTESIAN_POINT ( 'NONE',  ( 0.5837800005270550319, -25.23388577838564828, 39.52829704357589691 ) ) ;
#61526 = ADVANCED_FACE ( 'NONE', ( #41660 ), #38469, .F. ) ;
#61527 = DIRECTION ( 'NONE',  ( 0.000000000000000000, 0.000000000000000000, 1.000000000000000000 ) ) ;
#61528 = CARTESIAN_POINT ( 'NONE',  ( 1.092182651088183576, -37.05014944566807600, 19.59713271108671506 ) ) ;
#61530 = ORIENTED_EDGE ( 'NONE', *, *, #28006, .T. ) ;
#61529 = CARTESIAN_POINT ( 'NONE',  ( 0.3676999524040366896, -35.84016207189403502, -25.71834687500748373 ) ) ;
#61531 = VERTEX_POINT ( 'NONE', #36973 ) ;
#61532 = CARTESIAN_POINT ( 'NONE',  ( 1.227938101723756947, -42.91134962331487657, 0.8460948827223682134 ) ) ;
#61533 = CARTESIAN_POINT ( 'NONE',  ( 4.291220156522059348, -16.00047830133278381, 44.30997282141206028 ) ) ;
#61534 = LINE ( 'NONE', #54285, #45788 ) ;
#61535 = EDGE_CURVE ( 'NONE', #38633, #20738, #51029, .T. ) ;
#61536 = ORIENTED_EDGE ( 'NONE', *, *, #6981, .F. ) ;
#61537 = CARTESIAN_POINT ( 'NONE',  ( 0.6028777368367060907, 11.01229867075015001, -47.85675613011466112 ) ) ;
#61538 = DIRECTION ( 'NONE',  ( -1.000000000000000000, -1.836909530733554547E-16, -1.836909530733573529E-16 ) ) ;
#61539 = CARTESIAN_POINT ( 'NONE',  ( 0.6017666602106489515, -44.57804174182710000, -18.08695057064577583 ) ) ;
#61540 = B_SPLINE_CURVE_WITH_KNOTS ( 'NONE', 3,
 ( #40915, #60581, #36200, #55893 ),
 .UNSPECIFIED., .F., .F.,
 ( 4, 4 ),
 ( 1.734723475976807094E-18, 0.004042984057420974560 ),
 .UNSPECIFIED. ) ;
#61541 =( BOUNDED_SURFACE ( )  B_SPLINE_SURFACE ( 3, 1, ( 
 ( #46919, #22167 ),
 ( #27786, #46295 ),
 ( #3955, #23095 ),
 ( #3339, #22468 ) ),
 .UNSPECIFIED., .F., .F., .F. ) 
 B_SPLINE_SURFACE_WITH_KNOTS ( ( 4, 4 ),
 ( 2, 2 ),
 ( 0.000000000000000000, 1.000000000000000000 ),
 ( 0.000000000000000000, 1.000000000000000000 ),
 .UNSPECIFIED. ) 
 GEOMETRIC_REPRESENTATION_ITEM ( )  RATIONAL_B_SPLINE_SURFACE ( (
 ( 1.000000000000000000, 1.000000000000000000),
 ( 0.9953040768229013402, 0.8617119497784988535),
 ( 0.9953040768229013402, 0.8617119497784988535),
 ( 1.000000000000000000, 1.000000000000000000) ) ) 
 REPRESENTATION_ITEM ( '' )  SURFACE ( )  );
#61543 = EDGE_CURVE ( 'NONE', #11235, #38956, #20704, .T. ) ;
#61542 = EDGE_LOOP ( 'NONE', ( #9129, #3976, #32146, #52843 ) ) ;
#61544 = ORIENTED_EDGE ( 'NONE', *, *, #34344, .T. ) ;
#61545 = B_SPLINE_CURVE_WITH_KNOTS ( 'NONE', 3,
 ( #16141, #15833, #39654, #6377 ),
 .UNSPECIFIED., .F., .F.,
 ( 4, 4 ),
 ( 5.421010862427522170E-19, 0.004446298630425054611 ),
 .UNSPECIFIED. ) ;
#61546 = AXIS2_PLACEMENT_3D ( 'NONE', #3848, #32698, #18914 ) ;
#61547 = CARTESIAN_POINT ( 'NONE',  ( 0.9790320750461904975, 24.92853536925881031, -33.68835491510091629 ) ) ;
#61548 = CARTESIAN_POINT ( 'NONE',  ( 0.5997462898726536595, -7.321308210775074876, -48.55872811583048332 ) ) ;
#61549 = CARTESIAN_POINT ( 'NONE',  ( 0.5835226383429297226, 46.89572792844976590, -0.1821444667875269929 ) ) ;
#61551 = CARTESIAN_POINT ( 'NONE',  ( 0.5980894510889457338, -34.51330645350379456, -33.52121017007815595 ) ) ;
#61550 = VECTOR ( 'NONE', #44764, 1000.000000000000114 ) ;
#61552 = FACE_OUTER_BOUND ( 'NONE', #23056, .T. ) ;
#61553 =( BOUNDED_SURFACE ( )  B_SPLINE_SURFACE ( 3, 1, ( 
 ( #44478, #30963 ),
 ( #49445, #2439 ),
 ( #49141, #35688 ),
 ( #45092, #58829 ) ),
 .UNSPECIFIED., .F., .F., .F. ) 
 B_SPLINE_SURFACE_WITH_KNOTS ( ( 4, 4 ),
 ( 2, 2 ),
 ( 0.000000000000000000, 1.000000000000000000 ),
 ( 0.000000000000000000, 1.000000000000000000 ),
 .UNSPECIFIED. ) 
 GEOMETRIC_REPRESENTATION_ITEM ( )  RATIONAL_B_SPLINE_SURFACE ( (
 ( 1.000000000000000000, 1.000000000000000000),
 ( 0.7282232189291694135, 0.9929344683865672927),
 ( 0.7282232189291694135, 0.9929344683865672927),
 ( 1.000000000000000000, 1.000000000000000000) ) ) 
 REPRESENTATION_ITEM ( '' )  SURFACE ( )  );
#61554 = CARTESIAN_POINT ( 'NONE',  ( -2.569797478183783568, 6.011723966603960356, 13.34095667500607085 ) ) ;
#61555 = ORIENTED_EDGE ( 'NONE', *, *, #38218, .T. ) ;
#61556 = CARTESIAN_POINT ( 'NONE',  ( -6.010958268070873523, -9.434296419346321017, 16.31164801516939278 ) ) ;
#61557 = CARTESIAN_POINT ( 'NONE',  ( 2.648799415243696664, -48.43667485455532784, -7.642381325456497621 ) ) ;
#61558 = EDGE_LOOP ( 'NONE', ( #39262, #29581, #20199, #46726 ) ) ;
#61559 = CARTESIAN_POINT ( 'NONE',  ( 0.1152339509894530906, 41.80536608004668153, -14.11573793212829386 ) ) ;
#61560 = DIRECTION ( 'NONE',  ( -1.000000000000000000, -0.000000000000000000, -0.000000000000000000 ) ) ;
#61561 = CARTESIAN_POINT ( 'NONE',  ( 0.9762797500689124330, 4.697980241569248427, -41.64437257103928403 ) ) ;
#61562 = CARTESIAN_POINT ( 'NONE',  ( 0.7242486021783822725, 23.43459903703420366, -43.14894008370782075 ) ) ;
#61563 = EDGE_CURVE ( 'NONE', #39811, #46967, #46359, .T. ) ;
#61564 = VERTEX_POINT ( 'NONE', #22236 ) ;
#61565 = VERTEX_POINT ( 'NONE', #41359 ) ;
#61566 = CARTESIAN_POINT ( 'NONE',  ( 0.1139756605157203340, -44.12252424054494782, 0.3975856354873956722 ) ) ;
#61567 = DIRECTION ( 'NONE',  ( -0.07500201931887529039, -0.5478996815936019171, -0.8331750332359465494 ) ) ;
#61568 = EDGE_CURVE ( 'NONE', #50920, #31073, #7046, .T. ) ;
#61569 = CARTESIAN_POINT ( 'NONE',  ( -6.079354080745853928, -6.651439635596356759, -18.07073064439232368 ) ) ;
#61570 = VERTEX_POINT ( 'NONE', #27541 ) ;
#61571 = CARTESIAN_POINT ( 'NONE',  ( 0.6001305935487422083, -34.38748867424735778, 33.64689939321883116 ) ) ;
#61573 = ORIENTED_EDGE ( 'NONE', *, *, #5446, .T. ) ;
#61572 = EDGE_CURVE ( 'NONE', #9990, #4178, #55684, .T. ) ;
#61574 = CARTESIAN_POINT ( 'NONE',  ( 4.553261556744875094, 43.53643125131386427, 5.841123155974254466 ) ) ;
#61575 = CARTESIAN_POINT ( 'NONE',  ( 3.238018933889920792, -0.7223087070294264000, 13.37481822304147983 ) ) ;
#61576 = ADVANCED_FACE ( 'NONE', ( #2171 ), #11934, .F. ) ;
#61577 = ORIENTED_EDGE ( 'NONE', *, *, #46331, .T. ) ;
#61578 = CARTESIAN_POINT ( 'NONE',  ( 4.956445790443988031, 0.000000000000000000, 0.000000000000000000 ) ) ;
#61579 = ADVANCED_FACE ( 'NONE', ( #50420 ), #51233, .F. ) ;
#61580 = CARTESIAN_POINT ( 'NONE',  ( 0.9730545539215892381, 26.52009130076819687, -33.73144377768529978 ) ) ;
#61581 = CARTESIAN_POINT ( 'NONE',  ( -6.000000000000001776, 4.730042041638951881E-15, 0.000000000000000000 ) ) ;
#61582 = CARTESIAN_POINT ( 'NONE',  ( 0.3676999524040366896, -43.63756228305280160, 6.458617600967457406 ) ) ;
#61583 = DIRECTION ( 'NONE',  ( 0.000000000000000000, 0.000000000000000000, 1.000000000000000000 ) ) ;
#61584 = EDGE_CURVE ( 'NONE', #4220, #59114, #60865, .T. ) ;
#61585 = CARTESIAN_POINT ( 'NONE',  ( 0.6031357023905875581, 47.70157053127529423, -6.236038527293559675 ) ) ;
#61586 = B_SPLINE_CURVE_WITH_KNOTS ( 'NONE', 3,
 ( #45993, #26856, #22772, #22163 ),
 .UNSPECIFIED., .F., .F.,
 ( 4, 4 ),
 ( 2.012794395885733147E-17, 0.004444306975806116763 ),
 .UNSPECIFIED. ) ;
#61587 = CARTESIAN_POINT ( 'NONE',  ( 0.1101816497532063371, 16.37745527993589434, -39.89358705406968397 ) ) ;
#61588 = VERTEX_POINT ( 'NONE', #17229 ) ;
#61589 = CARTESIAN_POINT ( 'NONE',  ( 0.8760168074886960365, -37.61398439004513961, -29.98565522133333161 ) ) ;
#61590 = DIRECTION ( 'NONE',  ( 0.000000000000000000, 0.000000000000000000, 1.000000000000000000 ) ) ;
#61591 = VERTEX_POINT ( 'NONE', #50716 ) ;
#61592 = AXIS2_PLACEMENT_3D ( 'NONE', #23905, #33015, #43036 ) ;
#61593 = DIRECTION ( 'NONE',  ( -1.000000000000000000, -0.000000000000000000, -0.000000000000000000 ) ) ;
#61594 = CARTESIAN_POINT ( 'NONE',  ( 0.5827359174754840332, 0.3632382226757386867, -47.89462060834301127 ) ) ;
#61595 = CARTESIAN_POINT ( 'NONE',  ( 3.238018933889920792, -13.06836926121498443, -2.936872012904941265 ) ) ;
#61596 = CIRCLE ( 'NONE', #40631, 43.92652462719577500 ) ;
#61597 = CARTESIAN_POINT ( 'NONE',  ( 0.9730545539215883499, 41.57420493492400482, -10.61654491617520080 ) ) ;
#61598 = CARTESIAN_POINT ( 'NONE',  ( 0.5806925824938499181, -7.260877859416734026, -46.33035738103254175 ) ) ;
#61599 = CARTESIAN_POINT ( 'NONE',  ( 0.5809828226811617480, 47.41188724015879785, 6.791453954330491705 ) ) ;
#61600 = CARTESIAN_POINT ( 'NONE',  ( 0.5807400328401637335, -44.04145271122577299, 18.83234461715167640 ) ) ;
#61601 = DIRECTION ( 'NONE',  ( -1.091178482119751852E-16, 0.4283517167067198983, -0.9036120886721283885 ) ) ;
#61602 = CARTESIAN_POINT ( 'NONE',  ( 4.553261556744875094, 0.000000000000000000, 0.000000000000000000 ) ) ;
#61603 = CARTESIAN_POINT ( 'NONE',  ( 4.553261556744875094, 12.71466023209559104, -42.04612920360213479 ) ) ;
#61604 = VECTOR ( 'NONE', #29945, 1000.000000000000000 ) ;
#61605 = CARTESIAN_POINT ( 'NONE',  ( 0.5835871038041874348, 32.50343185804469215, 33.80475366499425860 ) ) ;
#61606 = CARTESIAN_POINT ( 'NONE',  ( 0.5980894510889457338, 23.44630161211586383, -42.01322166096895216 ) ) ;
#61607 = ORIENTED_EDGE ( 'NONE', *, *, #36173, .F. ) ;
#61608 = LINE ( 'NONE', #38463, #4477 ) ;
#61609 = CARTESIAN_POINT ( 'NONE',  ( 0.8751705887134553219, -28.56654290188682666, 38.69254731947783199 ) ) ;
#61610 = CARTESIAN_POINT ( 'NONE',  ( 0.9722240750034575330, 30.74950257331021319, 29.92651530838598717 ) ) ;
#61611 = CYLINDRICAL_SURFACE ( 'NONE', #43728, 12.50000000000000000 ) ;
#61612 = CARTESIAN_POINT ( 'NONE',  ( 4.060580049360325461, 31.91818944962045279, -30.21087348319056431 ) ) ;
#61613 = EDGE_CURVE ( 'NONE', #51265, #31834, #51887, .T. ) ;
#61614 = ORIENTED_EDGE ( 'NONE', *, *, #48521, .T. ) ;
#61615 = CARTESIAN_POINT ( 'NONE',  ( 5.974727161628369032, 18.95664195401506191, 7.868887636447684741 ) ) ;
#61616 = CARTESIAN_POINT ( 'NONE',  ( 0.5997462898726536595, -45.71211507932765983, -17.94308126043611296 ) ) ;
#61617 = EDGE_LOOP ( 'NONE', ( #24578, #22296, #27844, #12898 ) ) ;
#61618 = CARTESIAN_POINT ( 'NONE',  ( 4.975801465491694664, -15.94009207553080643, 45.18341283946430309 ) ) ;
#61619 = CARTESIAN_POINT ( 'NONE',  ( 4.549368137175248350, 23.67244292351640667, -35.80950303116076583 ) ) ;
#61620 = VERTEX_POINT ( 'NONE', #46063 ) ;
#61621 = CARTESIAN_POINT ( 'NONE',  ( 1.227938101723748288, 41.23019537246709376, 11.92353943227963597 ) ) ;
#61622 = AXIS2_PLACEMENT_3D ( 'NONE', #61110, #36735, #46744 ) ;
#61623 = VERTEX_POINT ( 'NONE', #33494 ) ;
#61624 = CARTESIAN_POINT ( 'NONE',  ( -6.016761891674564211, 17.40752468084793136, -7.214149619366169830 ) ) ;
#61625 = CARTESIAN_POINT ( 'NONE',  ( 0.8744876279028306332, 17.78802839418675674, 45.75954650373076049 ) ) ;
#61626 = VECTOR ( 'NONE', #45823, 1000.000000000000114 ) ;
#61627 = ORIENTED_EDGE ( 'NONE', *, *, #49081, .F. ) ;
#61628 = CARTESIAN_POINT ( 'NONE',  ( 4.962356264823608143, 27.50309822711080443, -31.85616401533997077 ) ) ;
#61629 = CARTESIAN_POINT ( 'NONE',  ( 0.1084644655670282398, 26.56696682929009867, 33.96951444491432426 ) ) ;
#61630 = CARTESIAN_POINT ( 'NONE',  ( 5.571549742892842438, -9.254395351074542475, 0.000000000000000000 ) ) ;
#61631 = CARTESIAN_POINT ( 'NONE',  ( 0.5836750258453364815, -38.10871351907207583, 29.01293504009526103 ) ) ;
#61632 = ORIENTED_EDGE ( 'NONE', *, *, #46158, .T. ) ;
#61633 = B_SPLINE_CURVE_WITH_KNOTS ( 'NONE', 3,
 ( #47584, #10836, #24078, #4017, #18776, #43206 ),
 .UNSPECIFIED., .F., .F.,
 ( 4, 2, 4 ),
 ( 1.910758783386232924E-17, 0.0002293755540694310746, 0.0004587511081388430129 ),
 .UNSPECIFIED. ) ;
#61634 = CARTESIAN_POINT ( 'NONE',  ( 2.301430502907646503, 33.04218380901171770, 34.86297247504486307 ) ) ;
#61635 = ADVANCED_FACE ( 'NONE', ( #61647 ), #14081, .F. ) ;
#61636 = ORIENTED_EDGE ( 'NONE', *, *, #50571, .F. ) ;
#61637 = DIRECTION ( 'NONE',  ( -0.1024043820194934645, -0.6159418278945602010, 0.7811075516170060684 ) ) ;
#61639 = ADVANCED_FACE ( 'NONE', ( #19387 ), #44731, .T. ) ;
#61638 = ORIENTED_EDGE ( 'NONE', *, *, #57142, .T. ) ;
#61640 = ORIENTED_EDGE ( 'NONE', *, *, #50248, .T. ) ;
#61641 = CARTESIAN_POINT ( 'NONE',  ( 0.2279481005628816725, 25.86035487905268226, -35.74556661464986007 ) ) ;
#61643 = VECTOR ( 'NONE', #6968, 1000.000000000000114 ) ;
#61642 = CARTESIAN_POINT ( 'NONE',  ( 0.9789889208857702751, -37.36078624453494257, 18.98701001296773327 ) ) ;
#61644 = EDGE_CURVE ( 'NONE', #2228, #34059, #61633, .T. ) ;
#61646 = CARTESIAN_POINT ( 'NONE',  ( 0.9730545539215883499, 34.34678117142556175, 25.71816799638790840 ) ) ;
#61645 = B_SPLINE_CURVE_WITH_KNOTS ( 'NONE', 3,
 ( #57119, #23630, #32734, #43066 ),
 .UNSPECIFIED., .F., .F.,
 ( 4, 4 ),
 ( 7.152448122690996019E-18, 0.005014147105413700387 ),
 .UNSPECIFIED. ) ;
#61647 = FACE_OUTER_BOUND ( 'NONE', #53558, .T. ) ;
#61648 = VERTEX_POINT ( 'NONE', #28457 ) ;
#61649 = LINE ( 'NONE', #37585, #7852 ) ;
#61650 = EDGE_CURVE ( 'NONE', #41374, #57370, #7845, .T. ) ;
#61651 = DIRECTION ( 'NONE',  ( 0.000000000000000000, 0.000000000000000000, -1.000000000000000000 ) ) ;
#61652 = CARTESIAN_POINT ( 'NONE',  ( 14.84250595937556483, 5.000000000000012434, -2.300655493813809945E-30 ) ) ;
#61653 = ORIENTED_EDGE ( 'NONE', *, *, #48591, .T. ) ;
#61654 = VERTEX_POINT ( 'NONE', #52570 ) ;
#61655 = CARTESIAN_POINT ( 'NONE',  ( 0.7242486021783834937, -49.09521972001481060, -0.8190622793412020153 ) ) ;
#61656 =( BOUNDED_SURFACE ( )  B_SPLINE_SURFACE ( 3, 1, ( 
 ( #50027, #2395 ),
 ( #45350, #1464 ),
 ( #30917, #54388 ),
 ( #49401, #2077 ) ),
 .UNSPECIFIED., .F., .F., .F. ) 
 B_SPLINE_SURFACE_WITH_KNOTS ( ( 4, 4 ),
 ( 2, 2 ),
 ( 0.000000000000000000, 1.000000000000000000 ),
 ( 0.000000000000000000, 1.000000000000000000 ),
 .UNSPECIFIED. ) 
 GEOMETRIC_REPRESENTATION_ITEM ( )  RATIONAL_B_SPLINE_SURFACE ( (
 ( 1.000000000000000000, 1.000000000000000000),
 ( 0.7269869731126817891, 0.9931720237060910339),
 ( 0.7269869731126817891, 0.9931720237060910339),
 ( 1.000000000000000000, 1.000000000000000000) ) ) 
 REPRESENTATION_ITEM ( '' )  SURFACE ( )  );
#61657 = DIRECTION ( 'NONE',  ( 0.000000000000000000, -1.000000000000000000, 0.000000000000000000 ) ) ;
#61658 = LINE ( 'NONE', #32263, #12950 ) ;
#61659 = FACE_OUTER_BOUND ( 'NONE', #14272, .T. ) ;
#61660 = CARTESIAN_POINT ( 'NONE',  ( 0.3676999524040323597, -38.02468164711575582, -22.36233818182566324 ) ) ;
#61661 = ORIENTED_EDGE ( 'NONE', *, *, #49945, .F. ) ;
#61662 = ADVANCED_FACE ( 'NONE', ( #46667 ), #12487, .F. ) ;
#61663 = ORIENTED_EDGE ( 'NONE', *, *, #47676, .T. ) ;
#61664 = EDGE_CURVE ( 'NONE', #24375, #5770, #19081, .T. ) ;
#61665 = DIRECTION ( 'NONE',  ( -0.07439287786467650709, -0.9161872986448725831, 0.3937848822959336137 ) ) ;
#61666 = CARTESIAN_POINT ( 'NONE',  ( 1.834102595619085507, 42.96742150962945317, -9.695278937272329145 ) ) ;
#61667 = CARTESIAN_POINT ( 'NONE',  ( 0.5837157313716025975, -41.81444688234194018, -21.23179444855826858 ) ) ;
#61668 = CARTESIAN_POINT ( 'NONE',  ( 0.1129192098497455998, -32.03190746135001632, 30.34647742609778831 ) ) ;
#61669 = LINE ( 'NONE', #28478, #17823 ) ;
#61670 = ORIENTED_EDGE ( 'NONE', *, *, #12262, .T. ) ;
#61671 = CARTESIAN_POINT ( 'NONE',  ( 2.624215991343620935, 1.411420423865478613, 47.98682984381861871 ) ) ;
#61672 = VECTOR ( 'NONE', #25943, 1000.000000000000114 ) ;
#61673 = CARTESIAN_POINT ( 'NONE',  ( 5.860006189529234355, 47.30964106197858854, 9.393028332204897524 ) ) ;
#61674 = CARTESIAN_POINT ( 'NONE',  ( 0.5850706913938534814, -41.38834827854224585, 24.10530971368273612 ) ) ;
#61675 = CONICAL_SURFACE ( 'NONE', #19726, 43.92652462719577500, 1.486293639869522343 ) ;
#61676 = CARTESIAN_POINT ( 'NONE',  ( 5.894904586330512508, 19.71013252676728200, 4.005007845050151616 ) ) ;
#61677 = DIRECTION ( 'NONE',  ( -0.9848077530122079093, -0.1736481776669314414, 2.220446049250313081E-16 ) ) ;
#61678 = CARTESIAN_POINT ( 'NONE',  ( 0.8551540677456715978, -11.51835730326512142, 46.51172240253117707 ) ) ;
#61679 = B_SPLINE_CURVE_WITH_KNOTS ( 'NONE', 3,
 ( #12081, #54319, #1394, #49033 ),
 .UNSPECIFIED., .F., .F.,
 ( 4, 4 ),
 ( 4.336808689942017120E-17, 0.005004741218457454434 ),
 .UNSPECIFIED. ) ;
#61680 = ADVANCED_FACE ( 'NONE', ( #23157 ), #10460, .F. ) ;
#61681 = CARTESIAN_POINT ( 'NONE',  ( 5.880360259849752858, -36.09847387447880607, 31.59460303415922411 ) ) ;
#61682 = EDGE_LOOP ( 'NONE', ( #2176, #53792, #59003, #42099 ) ) ;
#61683 = CARTESIAN_POINT ( 'NONE',  ( 0.9972139404380295780, -39.89035676513721285, -15.81078898082028594 ) ) ;
#61684 = CARTESIAN_POINT ( 'NONE',  ( 3.050102900204245682, 23.66345782521629459, -37.08727562024838420 ) ) ;
#61685 = CARTESIAN_POINT ( 'NONE',  ( 0.6001305935487315502, 12.95698906763746017, 46.33281397023068138 ) ) ;
#61686 = LINE ( 'NONE', #8456, #16737 ) ;
#61687 = ORIENTED_EDGE ( 'NONE', *, *, #31973, .T. ) ;
#61688 = CARTESIAN_POINT ( 'NONE',  ( 5.895596859100789899, 19.71057157537860149, -4.002693016503341639 ) ) ;
#61689 = CARTESIAN_POINT ( 'NONE',  ( 3.661921753702024329, 26.36408909118086541, -38.95594858588754761 ) ) ;
#61690 = ORIENTED_EDGE ( 'NONE', *, *, #47460, .T. ) ;
#61691 = CARTESIAN_POINT ( 'NONE',  ( 0.3622758884714600280, -20.83792692158946025, -37.74294673546579304 ) ) ;
#61692 = DIRECTION ( 'NONE',  ( -1.000000000000000000, -0.000000000000000000, -0.000000000000000000 ) ) ;
#61693 = CARTESIAN_POINT ( 'NONE',  ( 2.648799415243696664, 49.00436887187491664, -1.757638972831356616 ) ) ;
#61694 = ORIENTED_EDGE ( 'NONE', *, *, #56, .T. ) ;
#61695 = CARTESIAN_POINT ( 'NONE',  ( 0.1310142868023685681, -17.08943085418612995, 39.59283406808302885 ) ) ;
#61696 = B_SPLINE_CURVE_WITH_KNOTS ( 'NONE', 3,
 ( #14561, #44311, #43379, #57733, #33976, #53050, #19874, #9844, #1339, #20180, #43693, #39293, #39605, #5422, #58659, #53962 ),
 .UNSPECIFIED., .F., .F.,
 ( 4, 3, 3, 3, 3, 4 ),
 ( 1.868480190406682863E-17, 0.0002618515315864450668, 0.0003927756766342005933, 0.0005236998216950575647, 0.0007855159896329933682, 0.001047349442285928738 ),
 .UNSPECIFIED. ) ;
#61697 = ORIENTED_EDGE ( 'NONE', *, *, #42768, .T. ) ;
#61698 = CARTESIAN_POINT ( 'NONE',  ( 2.643462169533613793, -43.83256147628748067, 19.65219740572111817 ) ) ;
#61699 = ORIENTED_EDGE ( 'NONE', *, *, #13701, .F. ) ;
#61700 = CARTESIAN_POINT ( 'NONE',  ( 1.091591847532194626, -6.200834385736088805, -41.45248658255029994 ) ) ;
#61701 = CARTESIAN_POINT ( 'NONE',  ( 0.6000166863083090663, -48.63754814943186489, 6.797969676318824206 ) ) ;
#61702 = ORIENTED_EDGE ( 'NONE', *, *, #59781, .T. ) ;
#61703 = CARTESIAN_POINT ( 'NONE',  ( 2.281351352603289584, 28.15073776031364972, 38.84542754822333421 ) ) ;
#61704 = ORIENTED_EDGE ( 'NONE', *, *, #20971, .F. ) ;
#61705 = CARTESIAN_POINT ( 'NONE',  ( 2.526464513654346877, -12.29060355381822056, -41.18424249084328181 ) ) ;
#61706 = CARTESIAN_POINT ( 'NONE',  ( 4.967162193818130511, 14.26841313271282097, 40.65506779172170582 ) ) ;
#61707 = CARTESIAN_POINT ( 'NONE',  ( 5.960721111146673579, -18.96073515164554379, 7.860635756377555516 ) ) ;
#61708 = EDGE_CURVE ( 'NONE', #21985, #868, #26481, .T. ) ;
#61709 = EDGE_LOOP ( 'NONE', ( #16696, #2937, #1779, #54805 ) ) ;
#61710 = CARTESIAN_POINT ( 'NONE',  ( 5.896278296736517710, -19.93412839397019098, -2.675351339001139195 ) ) ;
#61711 =( GEOMETRIC_REPRESENTATION_CONTEXT ( 3 ) GLOBAL_UNCERTAINTY_ASSIGNED_CONTEXT ( ( #55535 ) ) GLOBAL_UNIT_ASSIGNED_CONTEXT ( ( #45164, #36067, #59211 ) ) REPRESENTATION_CONTEXT ( 'NONE', 'WORKASPACE' ) );
#61712 = AXIS2_PLACEMENT_3D ( 'NONE', #16300, #58567, #25383 ) ;
#61713 = CARTESIAN_POINT ( 'NONE',  ( 5.895881250540457863, -9.669871309367247036, 17.63579514704616358 ) ) ;
#61714 = CARTESIAN_POINT ( 'NONE',  ( 5.895596859100789899, 17.94951300836817865, -9.074313526372616678 ) ) ;
#61715 = VECTOR ( 'NONE', #3320, 1000.000000000000000 ) ;
#61716 = CARTESIAN_POINT ( 'NONE',  ( 0.5837799406558213944, 16.93978989757854592, 43.72970463887332926 ) ) ;
#61717 = ORIENTED_EDGE ( 'NONE', *, *, #6262, .F. ) ;
#61718 = EDGE_CURVE ( 'NONE', #1357, #47400, #9693, .T. ) ;
#61719 = CARTESIAN_POINT ( 'NONE',  ( 0.6001305935487422083, -24.50730504006429200, -41.40054608060284380 ) ) ;
#61720 = CARTESIAN_POINT ( 'NONE',  ( 0.1155031312995260795, -31.57910769448971067, -30.81722878118065623 ) ) ;
#61721 = ORIENTED_EDGE ( 'NONE', *, *, #52746, .T. ) ;
#61722 = CARTESIAN_POINT ( 'NONE',  ( 0.5800708119828332787, 47.56394195701287231, 5.628966929617906345 ) ) ;
#61723 =( BOUNDED_SURFACE ( )  B_SPLINE_SURFACE ( 3, 1, ( 
 ( #55355, #27795 ),
 ( #32195, #2428 ),
 ( #26871, #41603 ),
 ( #21869, #41920 ) ),
 .UNSPECIFIED., .F., .F., .F. ) 
 B_SPLINE_SURFACE_WITH_KNOTS ( ( 4, 4 ),
 ( 2, 2 ),
 ( 0.000000000000000000, 1.000000000000000000 ),
 ( 0.000000000000000000, 1.000000000000000000 ),
 .UNSPECIFIED. ) 
 GEOMETRIC_REPRESENTATION_ITEM ( )  RATIONAL_B_SPLINE_SURFACE ( (
 ( 1.000000000000000000, 1.000000000000000000),
 ( 0.9953485035131437453, 0.8621029689291515030),
 ( 0.9953485035131437453, 0.8621029689291515030),
 ( 1.000000000000000000, 1.000000000000000000) ) ) 
 REPRESENTATION_ITEM ( '' )  SURFACE ( )  );
#61724 = ORIENTED_EDGE ( 'NONE', *, *, #14585, .F. ) ;
#61725 = CARTESIAN_POINT ( 'NONE',  ( 4.962356264823608143, 0.000000000000000000, 0.000000000000000000 ) ) ;
#61726 = CARTESIAN_POINT ( 'NONE',  ( 0.5835871038041865466, 11.00424250131069748, -45.58663290783655242 ) ) ;
#61727 = VERTEX_POINT ( 'NONE', #2017 ) ;
#61728 = CARTESIAN_POINT ( 'NONE',  ( 0.9769922540276045897, -34.29921094923819425, -24.08102330354307341 ) ) ;
#61729 = DIRECTION ( 'NONE',  ( 0.000000000000000000, 0.000000000000000000, 1.000000000000000000 ) ) ;
#61730 = CARTESIAN_POINT ( 'NONE',  ( 4.962356264823603702, 0.9708976703223142213, -42.07484944210863631 ) ) ;
#61731 = CARTESIAN_POINT ( 'NONE',  ( -2.601141883200665639, -5.629531953699136615, -13.82402971103827660 ) ) ;
#61732 = EDGE_CURVE ( 'NONE', #60778, #36963, #8618, .T. ) ;
#61733 = ORIENTED_EDGE ( 'NONE', *, *, #33627, .F. ) ;
#61734 = CARTESIAN_POINT ( 'NONE',  ( 2.281351352603289584, 4.956540261593756824, 47.71649595778612962 ) ) ;
#61735 = CARTESIAN_POINT ( 'NONE',  ( 0.9787464366903561030, -41.82650318302786729, 2.622522520517909683 ) ) ;
#61736 = CARTESIAN_POINT ( 'NONE',  ( 0.5804410086790514622, 37.14246315962216016, 28.63489623329386191 ) ) ;
#61737 = ADVANCED_FACE ( 'NONE', ( #20537 ), #28026, .F. ) ;
#61738 = CARTESIAN_POINT ( 'NONE',  ( 0.5827357941260210561, -44.38787053017136230, -17.99287562175633681 ) ) ;
#61739 = CARTESIAN_POINT ( 'NONE',  ( 1.827326673878743701, -6.839036141888885645, 42.50320212329568648 ) ) ;
#61740 = DIRECTION ( 'NONE',  ( 0.09722883295013594329, 0.8999532196066740708, 0.4250067723727894986 ) ) ;
#61741 = CARTESIAN_POINT ( 'NONE',  ( 0.5839879327111935359, -46.24044206955225889, 12.48412918464419974 ) ) ;
#61742 = VECTOR ( 'NONE', #49603, 1000.000000000000000 ) ;
#61743 = FACE_OUTER_BOUND ( 'NONE', #40185, .T. ) ;
#61744 = CARTESIAN_POINT ( 'NONE',  ( 0.5835226383429281682, 40.25633451856137413, -24.05556080567755473 ) ) ;
#61745 = LINE ( 'NONE', #37369, #59394 ) ;
#61746 = CARTESIAN_POINT ( 'NONE',  ( -6.010958268070873523, -16.31164801516948870, 9.434296419346148710 ) ) ;
#61747 = CARTESIAN_POINT ( 'NONE',  ( 5.880360259849752858, 15.46489389606756149, -45.41096578730631705 ) ) ;
#61748 = DIRECTION ( 'NONE',  ( -1.000000000000000000, -0.000000000000000000, -0.000000000000000000 ) ) ;
#61749 = CARTESIAN_POINT ( 'NONE',  ( 0.9754402186311941225, 37.25324696807229685, 21.29160191075010644 ) ) ;
#61750 = CARTESIAN_POINT ( 'NONE',  ( 0.1119899015040011075, -31.30369570375773947, -31.09726585214597705 ) ) ;
#61751 = CARTESIAN_POINT ( 'NONE',  ( 0.9730545539215883499, -37.40983423658458662, -21.01499094264588763 ) ) ;
#61752 = ADVANCED_FACE ( 'NONE', ( #17081 ), #49233, .F. ) ;
#61753 = CARTESIAN_POINT ( 'NONE',  ( 2.282803330402960906, 15.64995782534825075, 44.28967969540766347 ) ) ;
#61755 = VERTEX_POINT ( 'NONE', #59971 ) ;
#61754 = CARTESIAN_POINT ( 'NONE',  ( 3.238018933889920792, -10.11627964985467010, 8.778859744499238005 ) ) ;
#61756 = CIRCLE ( 'NONE', #27809, 48.91267123290010943 ) ;
#61757 = CARTESIAN_POINT ( 'NONE',  ( -6.078457390727109555, 13.83560117034712889, -13.39293288613801280 ) ) ;
#61758 = CARTESIAN_POINT ( 'NONE',  ( 0.6253024248130490959, 5.398505417741914947, -48.80881443624968341 ) ) ;
#61759 = VECTOR ( 'NONE', #45140, 999.9999999999998863 ) ;
#61760 = CARTESIAN_POINT ( 'NONE',  ( 0.8554163680231738898, 3.785871848716432453, 46.76401017296225149 ) ) ;
#61761 = ORIENTED_EDGE ( 'NONE', *, *, #28444, .T. ) ;
#61762 = CARTESIAN_POINT ( 'NONE',  ( 0.5839880159502345292, -33.89965136132169476, 33.83547574026613347 ) ) ;
#61763 = CARTESIAN_POINT ( 'NONE',  ( 0.5786265663353153954, 37.55861529268594268, -29.72999788434255564 ) ) ;
#61764 = ORIENTED_EDGE ( 'NONE', *, *, #41078, .T. ) ;
#61765 = VERTEX_POINT ( 'NONE', #16150 ) ;
#61766 = CARTESIAN_POINT ( 'NONE',  ( 0.9756008150404589241, -11.24277293639960362, -41.40938772927945877 ) ) ;
#61767 = VERTEX_POINT ( 'NONE', #35264 ) ;
#61768 = B_SPLINE_CURVE_WITH_KNOTS ( 'NONE', 3,
 ( #50132, #45154, #6560, #44845 ),
 .UNSPECIFIED., .F., .F.,
 ( 4, 4 ),
 ( 2.030441771438897580E-17, 0.004444306975806115029 ),
 .UNSPECIFIED. ) ;
#61769 = CARTESIAN_POINT ( 'NONE',  ( -0.2999999999999999889, -13.49666625504239015, -1.199999999999999956 ) ) ;
#61770 = CARTESIAN_POINT ( 'NONE',  ( 0.9730545539215883499, -41.57420493492393376, 10.61654491617549034 ) ) ;
#61771 = EDGE_LOOP ( 'NONE', ( #3404, #32839, #60591, #56385 ) ) ;
#61772 = ORIENTED_EDGE ( 'NONE', *, *, #41027, .T. ) ;
#61773 = CARTESIAN_POINT ( 'NONE',  ( 4.549368137175248350, 0.000000000000000000, 0.000000000000000000 ) ) ;
#61774 = ORIENTED_EDGE ( 'NONE', *, *, #35461, .T. ) ;
#61775 = CARTESIAN_POINT ( 'NONE',  ( 0.1129192098497455998, -23.28677643606931014, 37.47903188453085477 ) ) ;
#61776 = DIRECTION ( 'NONE',  ( 0.000000000000000000, 0.000000000000000000, 1.000000000000000000 ) ) ;
#61777 = B_SPLINE_CURVE_WITH_KNOTS ( 'NONE', 3,
 ( #47239, #42550, #18733, #14047, #50677, #7767 ),
 .UNSPECIFIED., .F., .F.,
 ( 4, 2, 4 ),
 ( 6.256513556477135401E-18, 0.0002445244328975379445, 0.0004890488657950697090 ),
 .UNSPECIFIED. ) ;
#61778 = AXIS2_PLACEMENT_3D ( 'NONE', #27715, #46843, #13629 ) ;
#61779 = CARTESIAN_POINT ( 'NONE',  ( 5.880360259849739535, -45.44137230084871248, -15.37531919565220129 ) ) ;
#61780 = VERTEX_POINT ( 'NONE', #30528 ) ;
#61781 = CARTESIAN_POINT ( 'NONE',  ( 0.8551540677456834771, 24.74404575822774888, 41.03346287276437465 ) ) ;
#61782 = CARTESIAN_POINT ( 'NONE',  ( 0.9775691876210993447, -39.71209476610986400, 13.38966908767717534 ) ) ;
#61783 = EDGE_LOOP ( 'NONE', ( #45195, #16016, #10827, #39494 ) ) ;
#61784 = EDGE_CURVE ( 'NONE', #55636, #46169, #39728, .T. ) ;
#61785 = ORIENTED_EDGE ( 'NONE', *, *, #52731, .F. ) ;
#61786 = FACE_OUTER_BOUND ( 'NONE', #27250, .T. ) ;
#61787 = ORIENTED_EDGE ( 'NONE', *, *, #22492, .F. ) ;
#61788 = CARTESIAN_POINT ( 'NONE',  ( 0.2230388203127586233, 41.44703429209685908, -11.89247826311231471 ) ) ;
#61789 = CARTESIAN_POINT ( 'NONE',  ( 0.5980894510889457338, 5.583794302585253888, -47.78766676462070251 ) ) ;
#61790 = CARTESIAN_POINT ( 'NONE',  ( 4.962356264823608143, 0.000000000000000000, 0.000000000000000000 ) ) ;
#61791 = CARTESIAN_POINT ( 'NONE',  ( 0.7764139734771250412, -0.6759653311300753975, -46.89971792855448740 ) ) ;
#61792 = ADVANCED_FACE ( 'NONE', ( #6089 ), #15843, .T. ) ;
#61793 = EDGE_LOOP ( 'NONE', ( #2072, #44190, #53263, #49690 ) ) ;
#61794 = CARTESIAN_POINT ( 'NONE',  ( 4.962356264823608143, -38.91448554252697534, 16.02805081171152324 ) ) ;
#61795 = CARTESIAN_POINT ( 'NONE',  ( 0.8744876279028263033, -47.70753782033983725, 11.59055156152357213 ) ) ;
#61796 = EDGE_CURVE ( 'NONE', #56932, #53499, #55651, .T. ) ;
#61797 = B_SPLINE_CURVE_WITH_KNOTS ( 'NONE', 3,
 ( #59225, #16333, #35458, #26046 ),
 .UNSPECIFIED., .F., .F.,
 ( 4, 4 ),
 ( 0.000000000000000000, 0.004444103432399266161 ),
 .UNSPECIFIED. ) ;
#61798 = CARTESIAN_POINT ( 'NONE',  ( 0.5824936645240084143, 37.02860808157328165, -28.77708050830649356 ) ) ;
#61799 = ORIENTED_EDGE ( 'NONE', *, *, #18176, .F. ) ;
#61800 = CARTESIAN_POINT ( 'NONE',  ( 1.231276596079881047, -7.805643096902013411, 41.18675402191647805 ) ) ;
#61801 = CARTESIAN_POINT ( 'NONE',  ( 0.7044674535453004927, -24.73445998053471229, 42.42651543884123555 ) ) ;
#61802 = CARTESIAN_POINT ( 'NONE',  ( 0.5988103622719987973, 6.880137819454861692, -47.61318311633117872 ) ) ;
#61803 = AXIS2_PLACEMENT_3D ( 'NONE', #4080, #52014, #30830 ) ;
#61804 = AXIS2_PLACEMENT_3D ( 'NONE', #5504, #6414, #825 ) ;
#61805 = ORIENTED_EDGE ( 'NONE', *, *, #49580, .T. ) ;
#61806 = ORIENTED_EDGE ( 'NONE', *, *, #42345, .T. ) ;
#61807 = CARTESIAN_POINT ( 'NONE',  ( 0.5807400328401637335, -44.04145271122550298, -18.83234461715230168 ) ) ;
#61808 = CARTESIAN_POINT ( 'NONE',  ( -6.015611763856276717, 14.95313250337445332, -11.46610900684707701 ) ) ;
#61809 = DIRECTION ( 'NONE',  ( 0.000000000000000000, 0.000000000000000000, 1.000000000000000000 ) ) ;
#61810 = EDGE_CURVE ( 'NONE', #10199, #37874, #29475, .T. ) ;
#61811 = CARTESIAN_POINT ( 'NONE',  ( -6.016761891674565099, 9.418621820384494470, 16.32039929810260048 ) ) ;
#61812 = FACE_OUTER_BOUND ( 'NONE', #48854, .T. ) ;
#61813 = CARTESIAN_POINT ( 'NONE',  ( 2.643462169533613793, 11.09243630552533055, -46.73820883660196301 ) ) ;
#61814 = FACE_OUTER_BOUND ( 'NONE', #48745, .T. ) ;
#61815 = CARTESIAN_POINT ( 'NONE',  ( 0.2885700199627510010, -17.24062365614568293, -39.51953436244168216 ) ) ;
#61816 = CARTESIAN_POINT ( 'NONE',  ( 0.6000166863083106206, 23.17738933882476005, 43.29702189695021275 ) ) ;
#61817 = CARTESIAN_POINT ( 'NONE',  ( 4.549368137175248350, 0.000000000000000000, 0.000000000000000000 ) ) ;
#61818 = CARTESIAN_POINT ( 'NONE',  ( 0.9787284016396602393, 41.90824429648411353, -0.1872402601951978218 ) ) ;
#61819 = CARTESIAN_POINT ( 'NONE',  ( 0.1368894036331267383, 40.02613545401979422, 18.56797798737903804 ) ) ;
#61820 = ORIENTED_EDGE ( 'NONE', *, *, #24201, .F. ) ;
#61821 = FACE_OUTER_BOUND ( 'NONE', #18942, .T. ) ;
#61822 = CARTESIAN_POINT ( 'NONE',  ( 3.240649175237396484, 18.70948899608092120, 39.81482059363294468 ) ) ;
#61823 = CARTESIAN_POINT ( 'NONE',  ( 0.1139756605157204172, -35.59819211292886365, -26.07151583598530209 ) ) ;
#61824 = DIRECTION ( 'NONE',  ( -1.000000000000000000, -0.000000000000000000, -0.000000000000000000 ) ) ;
#61825 = CARTESIAN_POINT ( 'NONE',  ( 4.975610109902397937, 25.84633036597824329, 41.52609557555928177 ) ) ;
#61826 = CARTESIAN_POINT ( 'NONE',  ( 1.154321485836935057, -39.32643515542047652, 17.18284940416437223 ) ) ;
#61827 = CARTESIAN_POINT ( 'NONE',  ( 4.553261556744875094, 0.000000000000000000, 0.000000000000000000 ) ) ;
#61828 = CARTESIAN_POINT ( 'NONE',  ( 4.958415959904820092, -35.33199410137683572, -28.54565022280822006 ) ) ;
#61829 = CARTESIAN_POINT ( 'NONE',  ( 0.5834872094924179464, 12.17696997821523119, 46.32218741137602080 ) ) ;
#61830 = PRESENTATION_LAYER_ASSIGNMENT (  '', '', ( #15859 ) ) ;
#61831 = DIRECTION ( 'NONE',  ( -1.000000000000000000, -1.836909530733573776E-16, 1.925929944387235579E-32 ) ) ;
#61833 = ORIENTED_EDGE ( 'NONE', *, *, #24347, .T. ) ;
#61832 = CARTESIAN_POINT ( 'NONE',  ( 4.963659409799330291, 3.403493583737315475, 44.62477100936217056 ) ) ;
#61834 = EDGE_LOOP ( 'NONE', ( #29216, #40610, #54856, #317 ) ) ;
#61835 = CARTESIAN_POINT ( 'NONE',  ( 5.895596859100789899, 10.81936814621369969, 16.95492424427734690 ) ) ;
#61836 = CARTESIAN_POINT ( 'NONE',  ( 0.2285344041767109480, 14.52189545027388284, -41.66072158312635310 ) ) ;
#61837 = CARTESIAN_POINT ( 'NONE',  ( 4.975610109902397937, -48.11736577406863802, 8.784561349450592971 ) ) ;
#61838 = EDGE_CURVE ( 'NONE', #44257, #13798, #16860, .T. ) ;
#61839 = ORIENTED_EDGE ( 'NONE', *, *, #29802, .F. ) ;
#61840 = DIRECTION ( 'NONE',  ( -1.000000000000000000, -0.000000000000000000, -0.000000000000000000 ) ) ;
#61841 = CARTESIAN_POINT ( 'NONE',  ( -2.708315649062916552, -4.041664582652708226, -14.06540004355481166 ) ) ;
#61842 = CARTESIAN_POINT ( 'NONE',  ( 3.240649175237395596, -43.35902152968361634, -7.433718409119623338 ) ) ;
#61843 = EDGE_CURVE ( 'NONE', #16220, #26981, #31791, .T. ) ;
#61844 = ORIENTED_EDGE ( 'NONE', *, *, #59634, .T. ) ;
#61845 = ORIENTED_EDGE ( 'NONE', *, *, #7352, .F. ) ;
#61846 = CARTESIAN_POINT ( 'NONE',  ( 0.9730545539215892381, 29.98130006528861813, 30.69604515769660935 ) ) ;
#61847 = EDGE_CURVE ( 'NONE', #44407, #45339, #3873, .T. ) ;
#61848 = AXIS2_PLACEMENT_3D ( 'NONE', #7288, #59616, #27044 ) ;
#61849 = AXIS2_PLACEMENT_3D ( 'NONE', #26225, #55033, #51260 ) ;
#61850 = LINE ( 'NONE', #454, #25525 ) ;
#61851 = CARTESIAN_POINT ( 'NONE',  ( 0.5806925824938499181, 17.36345040154836994, -43.56297685531297503 ) ) ;
#61852 = CARTESIAN_POINT ( 'NONE',  ( 0.5987334308729321819, -47.65150826912793036, -11.86999015361692678 ) ) ;
#61853 = CARTESIAN_POINT ( 'NONE',  ( 4.956445790443998689, -11.44166143952028314, 45.67960632101629415 ) ) ;
#61854 = CARTESIAN_POINT ( 'NONE',  ( 5.959547316686252039, 2.675599016784261597, 20.35048796920737857 ) ) ;
#61855 = ORIENTED_EDGE ( 'NONE', *, *, #30691, .F. ) ;
#61856 = ADVANCED_FACE ( 'NONE', ( #23015 ), #55886, .F. ) ;
#61857 = DIRECTION ( 'NONE',  ( -1.000000000000000000, -1.836909530733573776E-16, 1.361838123766442686E-32 ) ) ;
#61858 = CARTESIAN_POINT ( 'NONE',  ( 4.060580049360325461, 43.94558816817623637, 0.5029661144227123293 ) ) ;
#61859 = CIRCLE ( 'NONE', #28841, 47.09074272231896430 ) ;
#61860 = ORIENTED_EDGE ( 'NONE', *, *, #44068, .F. ) ;
#61861 = CARTESIAN_POINT ( 'NONE',  ( 0.1140933569871964287, 41.99434624594081811, -13.54344245234356059 ) ) ;
#61862 = ADVANCED_FACE ( 'NONE', ( #31471 ), #25273, .F. ) ;
#61863 = FACE_OUTER_BOUND ( 'NONE', #23998, .T. ) ;
#61864 = CARTESIAN_POINT ( 'NONE',  ( -6.015611763856276717, 9.427003116184170750, 16.31561949997079353 ) ) ;
#61865 = CYLINDRICAL_SURFACE ( 'NONE', #9383, 2.099999999999996092 ) ;
#61866 = ORIENTED_EDGE ( 'NONE', *, *, #38672, .T. ) ;
#61867 = ORIENTED_EDGE ( 'NONE', *, *, #6193, .F. ) ;
#61868 = CARTESIAN_POINT ( 'NONE',  ( 0.1155031312995260795, -44.12383981002575695, -0.1685020800892448045 ) ) ;
#61869 = CARTESIAN_POINT ( 'NONE',  ( 4.960386119450146403, 17.98972314615754087, -39.88491351121305684 ) ) ;
#61870 = ADVANCED_FACE ( 'NONE', ( #41205 ), #7663, .F. ) ;
#61871 = CARTESIAN_POINT ( 'NONE',  ( 2.282803330402976005, 18.10201666796580255, -43.34528694113895853 ) ) ;
#61872 = AXIS2_PLACEMENT_3D ( 'NONE', #29643, #58744, #45010 ) ;
#61873 = EDGE_LOOP ( 'NONE', ( #6858, #3156, #36185, #20775 ) ) ;
#61874 = CYLINDRICAL_SURFACE ( 'NONE', #57520, 2.099999999999996092 ) ;
#61875 = ORIENTED_EDGE ( 'NONE', *, *, #36439, .T. ) ;
#61876 = CARTESIAN_POINT ( 'NONE',  ( 3.050102900204245682, 43.49164654874852687, 6.625853126714405406 ) ) ;
#61877 = CARTESIAN_POINT ( 'NONE',  ( 0.6026112563231247332, -25.60570374804708749, 41.90332839371419738 ) ) ;
#61878 = VERTEX_POINT ( 'NONE', #13010 ) ;
#61879 = CARTESIAN_POINT ( 'NONE',  ( 0.5839254288179551722, -47.47429404163003142, -6.341681103465038660 ) ) ;
#61880 = CARTESIAN_POINT ( 'NONE',  ( -2.708315649062916552, 14.47261168455369607, -2.171184472130541998 ) ) ;
#61881 = DIRECTION ( 'NONE',  ( 0.000000000000000000, 0.000000000000000000, 1.000000000000000000 ) ) ;
#61882 = ADVANCED_FACE ( 'NONE', ( #60265 ), #31682, .F. ) ;
#61883 = B_SPLINE_CURVE_WITH_KNOTS ( 'NONE', 3,
 ( #55161, #36094, #11653, #12591 ),
 .UNSPECIFIED., .F., .F.,
 ( 4, 4 ),
 ( 2.194270917860438266E-17, 0.004559932413162189405 ),
 .UNSPECIFIED. ) ;
#61884 = VERTEX_POINT ( 'NONE', #51183 ) ;
#61885 = DIRECTION ( 'NONE',  ( 0.000000000000000000, 0.000000000000000000, 1.000000000000000000 ) ) ;
#61886 = DIRECTION ( 'NONE',  ( -1.000000000000000000, 0.000000000000000000, 0.000000000000000000 ) ) ;
#61887 = CARTESIAN_POINT ( 'NONE',  ( 5.901463166500146684, -19.40182753204446442, -5.299713082558163535 ) ) ;
#61888 = CARTESIAN_POINT ( 'NONE',  ( 0.5809828226811548646, -47.41188724015884048, 6.791453954330148868 ) ) ;
#61889 = CARTESIAN_POINT ( 'NONE',  ( 4.975801465491694664, 9.906103548668228953, -46.87746200127445206 ) ) ;
#61890 = ORIENTED_EDGE ( 'NONE', *, *, #1260, .T. ) ;
#61891 = CARTESIAN_POINT ( 'NONE',  ( 0.6039202388192952409, -14.13938383033910817, 47.02809306943389345 ) ) ;
#61892 = CARTESIAN_POINT ( 'NONE',  ( 4.226256110419178924, -15.56285703882488214, 41.09287931961308971 ) ) ;
#61893 = ORIENTED_EDGE ( 'NONE', *, *, #25917, .F. ) ;
#61894 = AXIS2_PLACEMENT_3D ( 'NONE', #13864, #36749, #9439 ) ;
#61895 = CARTESIAN_POINT ( 'NONE',  ( -1.399999999999998579, 0.000000000000000000, 0.000000000000000000 ) ) ;
#61896 = CARTESIAN_POINT ( 'NONE',  ( -6.015611763856276717, -11.47596948473821321, 14.94556629257421498 ) ) ;
#61897 = CARTESIAN_POINT ( 'NONE',  ( 2.299746137290199943, 40.37734675500032466, -27.81997855341737491 ) ) ;
#61898 = CARTESIAN_POINT ( 'NONE',  ( 2.526464513654346877, 34.82216969498465176, 25.19161096467240313 ) ) ;
#61899 = CARTESIAN_POINT ( 'NONE',  ( 0.8760168074887090262, -24.81951362746049483, -41.20610493656901241 ) ) ;
#61900 = CARTESIAN_POINT ( 'NONE',  ( -6.078726893082806448, -4.281536037413855134, -18.77398440473003305 ) ) ;
#61901 = CARTESIAN_POINT ( 'NONE',  ( 3.238741278300274029, -24.69738534405286501, -35.19027457370170708 ) ) ;
#61902 = DIRECTION ( 'NONE',  ( 6.323743061725745322E-22, 0.000000000000000000, -1.000000000000000222 ) ) ;
#61903 = CARTESIAN_POINT ( 'NONE',  ( 0.5837800005270561421, 10.87146978434382838, 45.61848751734192575 ) ) ;
#61904 =( BOUNDED_SURFACE ( )  B_SPLINE_SURFACE ( 3, 1, ( 
 ( #61335, #22836 ),
 ( #51325, #56334 ),
 ( #61946, #14074 ),
 ( #19084, #33176 ) ),
 .UNSPECIFIED., .F., .F., .F. ) 
 B_SPLINE_SURFACE_WITH_KNOTS ( ( 4, 4 ),
 ( 2, 2 ),
 ( 0.000000000000000000, 1.000000000000000000 ),
 ( 0.000000000000000000, 1.000000000000000000 ),
 .UNSPECIFIED. ) 
 GEOMETRIC_REPRESENTATION_ITEM ( )  RATIONAL_B_SPLINE_SURFACE ( (
 ( 1.000000000000000000, 1.000000000000000000),
 ( 0.9953390228620291325, 0.8624445117760984880),
 ( 0.9953390228620291325, 0.8624445117760984880),
 ( 1.000000000000000000, 1.000000000000000000) ) ) 
 REPRESENTATION_ITEM ( '' )  SURFACE ( )  );
#61905 = DIRECTION ( 'NONE',  ( 1.000000000000000000, 0.000000000000000000, 0.000000000000000000 ) ) ;
#61906 = CIRCLE ( 'NONE', #56914, 43.92652462719577500 ) ;
#61907 = CARTESIAN_POINT ( 'NONE',  ( 0.1310142868023678742, -25.74368468368911778, -34.59629828998408385 ) ) ;
#61908 = DIRECTION ( 'NONE',  ( -1.000000000000000000, -1.836970198721027715E-16, 2.218671295934095703E-31 ) ) ;
#61909 = ORIENTED_EDGE ( 'NONE', *, *, #38632, .T. ) ;
#61910 = AXIS2_PLACEMENT_3D ( 'NONE', #40439, #6549, #41069 ) ;
#61911 = DIRECTION ( 'NONE',  ( 0.000000000000000000, 1.000000000000000000, 0.000000000000000000 ) ) ;
#61912 = CARTESIAN_POINT ( 'NONE',  ( 48.50368771458344952, 15.40123845184989726, -1.751266045669078286 ) ) ;
#61913 = EDGE_CURVE ( 'NONE', #48862, #41443, #52660, .T. ) ;
#61914 = CARTESIAN_POINT ( 'NONE',  ( -6.057079549204054558, 3.081801865089040415, -19.00878029659116208 ) ) ;
#61915 = CARTESIAN_POINT ( 'NONE',  ( 4.962356264823608143, 0.000000000000000000, 0.000000000000000000 ) ) ;
#61916 = DIRECTION ( 'NONE',  ( 1.000000000000000000, 0.000000000000000000, 0.000000000000000000 ) ) ;
#61917 = EDGE_CURVE ( 'NONE', #47787, #45831, #10865, .T. ) ;
#61918 =( BOUNDED_SURFACE ( )  B_SPLINE_SURFACE ( 3, 1, ( 
 ( #6305, #39895 ),
 ( #44585, #30139 ),
 ( #39577, #58630 ),
 ( #58954, #15758 ) ),
 .UNSPECIFIED., .F., .F., .F. ) 
 B_SPLINE_SURFACE_WITH_KNOTS ( ( 4, 4 ),
 ( 2, 2 ),
 ( 0.000000000000000000, 1.000000000000000000 ),
 ( 0.000000000000000000, 1.000000000000000000 ),
 .UNSPECIFIED. ) 
 GEOMETRIC_REPRESENTATION_ITEM ( )  RATIONAL_B_SPLINE_SURFACE ( (
 ( 1.000000000000000000, 1.000000000000000000),
 ( 0.7282232189291694135, 0.9929344683865672927),
 ( 0.7282232189291694135, 0.9929344683865672927),
 ( 1.000000000000000000, 1.000000000000000000) ) ) 
 REPRESENTATION_ITEM ( '' )  SURFACE ( )  );
#61919 = VERTEX_POINT ( 'NONE', #55567 ) ;
#61920 = CARTESIAN_POINT ( 'NONE',  ( 5.965394784446460541, 18.95742317323934145, 7.868087674481023086 ) ) ;
#61921 = ADVANCED_FACE ( 'NONE', ( #6914 ), #33685, .F. ) ;
#61922 = ADVANCED_FACE ( 'NONE', ( #1596, #7537 ), #25419, .T. ) ;
#61923 = CARTESIAN_POINT ( 'NONE',  ( -6.078075953587585900, -11.01234782890449182, 15.79630873154732917 ) ) ;
#61924 = EDGE_CURVE ( 'NONE', #55528, #30663, #38493, .T. ) ;
#61925 = CARTESIAN_POINT ( 'NONE',  ( 4.975801465491694664, 9.906103548668228953, -46.87746200127445206 ) ) ;
#61926 = ORIENTED_EDGE ( 'NONE', *, *, #50368, .T. ) ;
#61927 = CARTESIAN_POINT ( 'NONE',  ( 5.974727161628369032, -12.48248968439917661, -16.29297756969643984 ) ) ;
#61928 = CARTESIAN_POINT ( 'NONE',  ( 0.5819845901640491315, 47.54333976522124772, -5.801229454883471526 ) ) ;
#61929 = VERTEX_POINT ( 'NONE', #50466 ) ;
#61930 = CIRCLE ( 'NONE', #31969, 75.00000000000001421 ) ;
#61931 = EDGE_CURVE ( 'NONE', #18314, #13524, #56676, .T. ) ;
#61932 = CARTESIAN_POINT ( 'NONE',  ( 0.8753041380234530822, 23.49739456791611047, 43.11624724384818563 ) ) ;
#61933 = EDGE_LOOP ( 'NONE', ( #42585, #29198, #33092, #9959 ) ) ;
#61934 = EDGE_CURVE ( 'NONE', #27020, #32624, #3634, .T. ) ;
#61935 = CARTESIAN_POINT ( 'NONE',  ( -6.016761891674564211, -13.32657647165345693, -13.32172022638605569 ) ) ;
#61937 = CARTESIAN_POINT ( 'NONE',  ( 4.975610109902397937, -16.35148546628954236, 46.09857188876348744 ) ) ;
#61936 = VECTOR ( 'NONE', #17135, 999.9999999999998863 ) ;
#61938 = EDGE_LOOP ( 'NONE', ( #17820, #27254, #1327, #2156 ) ) ;
#61939 = CARTESIAN_POINT ( 'NONE',  ( -6.015611763856276717, -16.32183393015603556, 9.416239407363246272 ) ) ;
#61940 = CARTESIAN_POINT ( 'NONE',  ( 2.301529144917016989, -40.93948199333351567, 25.12312032040438226 ) ) ;
#61941 = CARTESIAN_POINT ( 'NONE',  ( 4.549368137175248350, -38.40568845698262379, -19.17571786012310753 ) ) ;
#61942 = CARTESIAN_POINT ( 'NONE',  ( 4.956653778116971054, 42.88673967249130925, 21.75875759808722876 ) ) ;
#61943 = ORIENTED_EDGE ( 'NONE', *, *, #23429, .F. ) ;
#61944 = DIRECTION ( 'NONE',  ( 0.9990097760809873995, 5.448601141172495260E-18, 0.04449120468829072944 ) ) ;
#61945 = ORIENTED_EDGE ( 'NONE', *, *, #42616, .T. ) ;
#61946 = CARTESIAN_POINT ( 'NONE',  ( 5.959828726073459926, 12.49879082830568144, -16.28130559351252060 ) ) ;
#61947 = ORIENTED_EDGE ( 'NONE', *, *, #21148, .F. ) ;
#61948 = VERTEX_POINT ( 'NONE', #54525 ) ;
#61949 = CARTESIAN_POINT ( 'NONE',  ( 0.6021448801613057400, -42.65943078590919413, -24.32517427787867703 ) ) ;
#61950 = CARTESIAN_POINT ( 'NONE',  ( 0.9780303403264775097, -37.25713683229096063, 19.18972038501425814 ) ) ;
#61951 = AXIS2_PLACEMENT_3D ( 'NONE', #15700, #19784, #38588 ) ;
#61952 = CARTESIAN_POINT ( 'NONE',  ( 0.9740398440564311811, 34.29238484271531462, 25.79088785828992769 ) ) ;
#61953 = VERTEX_POINT ( 'NONE', #54846 ) ;
#61954 = DIRECTION ( 'NONE',  ( -0.07906939808003034253, -0.1737655548591644228, -0.9816076416938430693 ) ) ;
#61955 = CARTESIAN_POINT ( 'NONE',  ( 4.291220156522060236, -21.76365521422027882, -41.78196152674308905 ) ) ;
#61956 = CARTESIAN_POINT ( 'NONE',  ( 0.1129192098497455998, -27.88830454350494392, 34.19348267541455044 ) ) ;
#61958 = ORIENTED_EDGE ( 'NONE', *, *, #36670, .F. ) ;
#61957 = EDGE_CURVE ( 'NONE', #30850, #56380, #45800, .T. ) ;
#61959 = ORIENTED_EDGE ( 'NONE', *, *, #11790, .F. ) ;
#61960 = FILL_AREA_STYLE_COLOUR ( '', #459 ) ;
#61962 = EDGE_CURVE ( 'NONE', #50661, #31157, #31046, .T. ) ;
#61961 = DIRECTION ( 'NONE',  ( -1.836909530733573776E-16, 1.000000000000000000, 0.000000000000000000 ) ) ;
#61963 = FACE_OUTER_BOUND ( 'NONE', #16906, .T. ) ;
#61964 = CARTESIAN_POINT ( 'NONE',  ( 0.1103878639767399555, -34.18336104662756725, 26.29099398937389864 ) ) ;
#61965 = CARTESIAN_POINT ( 'NONE',  ( 0.9772918015221170318, 38.74329897262556699, 15.97791101703945138 ) ) ;
#61966 = ORIENTED_EDGE ( 'NONE', *, *, #10650, .T. ) ;
#61967 = EDGE_LOOP ( 'NONE', ( #40259, #27142, #18518, #7857, #38882, #55800, #9705, #38762, #39476, #58088, #20620, #26425, #61761, #20996, #575, #41043, #42244, #28354, #53320, #36175, #60307, #18395, #23613, #11346, #24064, #23231, #43220, #1753, #3621, #20898, #6616, #21061, #136, #33313, #21228, #28659, #55640, #57438, #18453, #11485, #23743, #10822, #54724, #29693, #56027, #48969, #33307, #54145, #5633, #24206, #32010, #42514, #17242, #20427, #47196, #10266, #40939, #42544, #24686, #3290, #19303, #26507, #27877, #5371, #24009, #38644, #12371, #33935, #53142, #61530, #35419, #13596, #6286, #15120, #33210, #16049, #42123, #4790, #26535, #28772, #18542, #23829, #38428, #33995, #41801, #22837, #47890, #13341, #60168, #8005, #32934, #18303, #22015, #29217, #18824, #43336, #22203, #28823, #55126, #30212, #57708, #14934, #55956, #45427, #36627, #59555, #30526, #1924, #24490, #18835, #61078, #25982, #49409, #21618, #7928, #17473, #1214, #19308, #5574, #23470, #34188, #12907, #42891, #16721, #51015, #17338, #45891, #56455, #54286, #13608, #1767, #15610, #24363, #12050, #6882, #27970, #44137, #40213, #43580, #49647, #37751, #26984, #18218, #14820, #59223, #3676, #46808, #29919 ) ) ;
#61968 = PRODUCT_DEFINITION ( 'UNKNOWN', '', #50889, #6591 ) ;
#61969 = CARTESIAN_POINT ( 'NONE',  ( 5.901764892641307547, -46.48816889762547078, 15.38965951493164575 ) ) ;
#61970 = CARTESIAN_POINT ( 'NONE',  ( 0.9789233960466718898, -41.09488416218491125, 8.218711731709811730 ) ) ;
#61971 = CARTESIAN_POINT ( 'NONE',  ( 1.296416391601052265, -38.93352552143989698, -20.65158503717203686 ) ) ;
#61972 = CARTESIAN_POINT ( 'NONE',  ( 3.376099380956838925, 13.39763462305342756, 0.4601848967830198811 ) ) ;
#61973 = CARTESIAN_POINT ( 'NONE',  ( 0.7056313189692619003, -35.34445970792710767, -30.83046888894615734 ) ) ;
#61974 = NEXT_ASSEMBLY_USAGE_OCCURRENCE ( 'NAUO1', ' ', ' ', #2291, #43635, $ ) ;
#61975 = NEXT_ASSEMBLY_USAGE_OCCURRENCE ( 'NAUO2', ' ', ' ', #2291, #16454, $ ) ;
#61976 = NEXT_ASSEMBLY_USAGE_OCCURRENCE ( 'NAUO3', ' ', ' ', #2291, #744, $ ) ;
#61977 = NEXT_ASSEMBLY_USAGE_OCCURRENCE ( 'NAUO4', ' ', ' ', #2291, #36005, $ ) ;
#61978 = NEXT_ASSEMBLY_USAGE_OCCURRENCE ( 'NAUO5', ' ', ' ', #2291, #61968, $ ) ;
#61979 = NEXT_ASSEMBLY_USAGE_OCCURRENCE ( 'NAUO6', ' ', ' ', #2291, #40600, $ ) ;
#61980 = NEXT_ASSEMBLY_USAGE_OCCURRENCE ( 'NAUO7', ' ', ' ', #2291, #51660, $ ) ;
#61981 = NEXT_ASSEMBLY_USAGE_OCCURRENCE ( 'NAUO8', ' ', ' ', #2291, #40600, $ ) ;
#61982 = NEXT_ASSEMBLY_USAGE_OCCURRENCE ( 'NAUO9', ' ', ' ', #2291, #40600, $ ) ;
#61983 = NEXT_ASSEMBLY_USAGE_OCCURRENCE ( 'NAUO10', ' ', ' ', #2291, #22195, $ ) ;
#61984 = NEXT_ASSEMBLY_USAGE_OCCURRENCE ( 'NAUO11', ' ', ' ', #2291, #26005, $ ) ;
#61985 = NEXT_ASSEMBLY_USAGE_OCCURRENCE ( 'NAUO12', ' ', ' ', #2291, #26005, $ ) ;
#61986 = NEXT_ASSEMBLY_USAGE_OCCURRENCE ( 'NAUO13', ' ', ' ', #2291, #3771, $ ) ;
#61987 = NEXT_ASSEMBLY_USAGE_OCCURRENCE ( 'NAUO14', ' ', ' ', #2291, #12658, $ ) ;
#61988 = NEXT_ASSEMBLY_USAGE_OCCURRENCE ( 'NAUO15', ' ', ' ', #2291, #12658, $ ) ;
#61989 = NEXT_ASSEMBLY_USAGE_OCCURRENCE ( 'NAUO16', ' ', ' ', #2291, #12658, $ ) ;
#61990 = NEXT_ASSEMBLY_USAGE_OCCURRENCE ( 'NAUO17', ' ', ' ', #2291, #12658, $ ) ;
#61991 = NEXT_ASSEMBLY_USAGE_OCCURRENCE ( 'NAUO18', ' ', ' ', #2291, #12658, $ ) ;
#61992 = NEXT_ASSEMBLY_USAGE_OCCURRENCE ( 'NAUO19', ' ', ' ', #2291, #12658, $ ) ;
#61993 = NEXT_ASSEMBLY_USAGE_OCCURRENCE ( 'NAUO20', ' ', ' ', #2291, #12658, $ ) ;
#61994 = NEXT_ASSEMBLY_USAGE_OCCURRENCE ( 'NAUO21', ' ', ' ', #2291, #12658, $ ) ;
#61995 = NEXT_ASSEMBLY_USAGE_OCCURRENCE ( 'NAUO22', ' ', ' ', #2291, #8814, $ ) ;
#61996 = NEXT_ASSEMBLY_USAGE_OCCURRENCE ( 'NAUO23', ' ', ' ', #2291, #8814, $ ) ;
#61997 = NEXT_ASSEMBLY_USAGE_OCCURRENCE ( 'NAUO24', ' ', ' ', #2291, #8814, $ ) ;
#61998 = NEXT_ASSEMBLY_USAGE_OCCURRENCE ( 'NAUO25', ' ', ' ', #2291, #8814, $ ) ;
#61999 = NEXT_ASSEMBLY_USAGE_OCCURRENCE ( 'NAUO26', ' ', ' ', #2291, #8814, $ ) ;
#62000 = NEXT_ASSEMBLY_USAGE_OCCURRENCE ( 'NAUO27', ' ', ' ', #2291, #8814, $ ) ;
#62001 = NEXT_ASSEMBLY_USAGE_OCCURRENCE ( 'NAUO28', ' ', ' ', #2291, #8814, $ ) ;
#62002 = NEXT_ASSEMBLY_USAGE_OCCURRENCE ( 'NAUO29', ' ', ' ', #2291, #8814, $ ) ;
ENDSEC;
END-ISO-10303-21;
